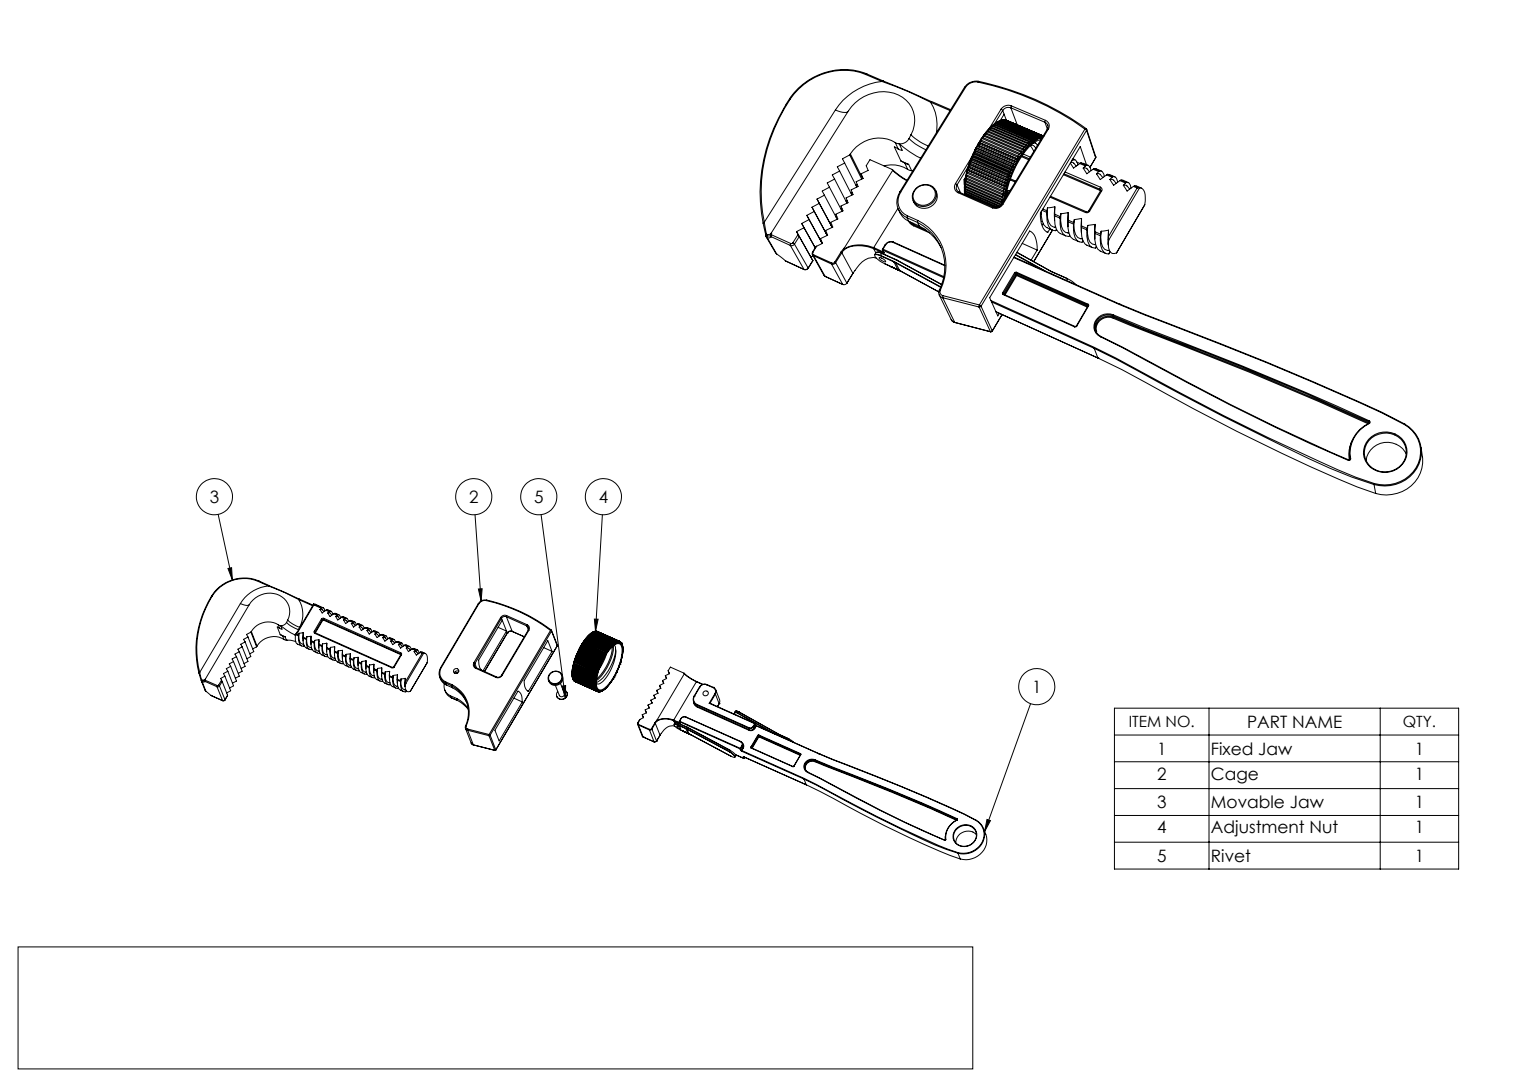
ISO-10303-21;
HEADER;
FILE_DESCRIPTION (('STEP AP214'),
    '1' );
FILE_NAME ('MAS-685',
    '2026-10-07T05:30:18',
    ( '' ),
    ( '' ),
    'SwSTEP 2.0',
    'SolidWorks 2021',
    '' );
FILE_SCHEMA (( 'AUTOMOTIVE_DESIGN' ));
ENDSEC;

DATA;
#1 = CARTESIAN_POINT ( 'NONE',  ( 7.084665262690076126, 22.02201867748817321, -10.88017736071110164 ) ) ;
#2 = CARTESIAN_POINT ( 'NONE',  ( 14.03351048042397231, -0.03417435944610275333, -2.474486531753715024 ) ) ;
#3 = CARTESIAN_POINT ( 'NONE',  ( 10.00000000000000000, 59.75893115100078745, -9.846743663894594434 ) ) ;
#4 = CARTESIAN_POINT ( 'NONE',  ( 14.71525861348289865, 0.5000000000000004441, -2.908807992686582633 ) ) ;
#5 = CARTESIAN_POINT ( 'NONE',  ( 14.92337183194729988, 29.34226448433411960, -8.527530157486177487 ) ) ;
#6 = CARTESIAN_POINT ( 'NONE',  ( -1.099225684535947600, 54.54030133659708923, 6.408140936763237150 ) ) ;
#7 = B_SPLINE_CURVE_WITH_KNOTS ( 'NONE', 3,
 ( #85792, #56757, #94261, #25787, #71286, #3780 ),
 .UNSPECIFIED., .F., .F.,
 ( 4, 2, 4 ),
 ( 0.0002800003243993068715, 0.0006862055569927260918, 0.001092410789586145421 ),
 .UNSPECIFIED. ) ;
#8 = CARTESIAN_POINT ( 'NONE',  ( 7.082119434687054849, -1.529584498419354954, 12.26659068614894288 ) ) ;
#9 = CARTESIAN_POINT ( 'NONE',  ( 4.559911319644449179, 47.23035201082150536, -9.422509992056141925 ) ) ;
#10 = CARTESIAN_POINT ( 'NONE',  ( 10.00000000000000000, 49.75893115100078745, -9.846743663894594434 ) ) ;
#11 = CARTESIAN_POINT ( 'NONE',  ( 6.204703633549690345, 40.76208216824731778, -14.16423886937410259 ) ) ;
#12 = ORIENTED_EDGE ( 'NONE', *, *, #89075, .F. ) ;
#13 = CARTESIAN_POINT ( 'NONE',  ( 17.08211943468705840, 5.137082168247300906, -12.26659068614894466 ) ) ;
#14 = CARTESIAN_POINT ( 'NONE',  ( 0.5774900079438590739, 67.64701867748817676, -5.440088680355550821 ) ) ;
#15 = CARTESIAN_POINT ( 'NONE',  ( 1.915564264621432589, 3.914659629196372862E-16, -14.37291249357990530 ) ) ;
#16 = CARTESIAN_POINT ( 'NONE',  ( 24.16423886937410614, 59.51208216824728936, -3.795296366450302550 ) ) ;
#17 = CARTESIAN_POINT ( 'NONE',  ( 13.43411237798106583, 7.665301336597086568, -12.81628187352647252 ) ) ;
#18 = CARTESIAN_POINT ( 'NONE',  ( 18.95386800104995473, 43.23810908735726599, -6.499999999999990230 ) ) ;
#19 = CARTESIAN_POINT ( 'NONE',  ( 0.5774900079438607392, 58.48035201082151247, 5.440088680355550821 ) ) ;
#20 = DIRECTION ( 'NONE',  ( -0.000000000000000000, 1.000000000000000000, -0.000000000000000000 ) ) ;
#21 = CARTESIAN_POINT ( 'NONE',  ( -46.94000000000001194, 100.5254250115999923, -8.865097534344174690 ) ) ;
#22 = CARTESIAN_POINT ( 'NONE',  ( 0.6178305044545818747, 33.49863466993042493, -9.382169495545419124 ) ) ;
#23 = CARTESIAN_POINT ( 'NONE',  ( -2.266590686148945544, 67.22041550158063217, 7.082119434687048631 ) ) ;
#24 = CARTESIAN_POINT ( 'NONE',  ( -10.88017736071110342, 33.06368534415485527, 3.903127820947815962E-15 ) ) ;
#25 = CARTESIAN_POINT ( 'NONE',  ( 20.88017736071110875, 15.77201867748817143, -2.915334737309920765 ) ) ;
#26 = CARTESIAN_POINT ( 'NONE',  ( 19.42250999205614193, 30.14701867748817321, 5.440088680355555262 ) ) ;
#27 = CARTESIAN_POINT ( 'NONE',  ( 7.361572987183169658, 49.96726448433410894, -9.846743663894592657 ) ) ;
#28 = CARTESIAN_POINT ( 'NONE',  ( 19.84674366389459266, 58.71726448433411605, -2.638427012816827677 ) ) ;
#29 = CARTESIAN_POINT ( 'NONE',  ( -2.816281873526473856, 49.12363466993042493, 9.499525473075851096E-16 ) ) ;
#31 = ORIENTED_EDGE ( 'NONE', *, *, #54443, .T. ) ;
#30 = AXIS2_PLACEMENT_3D ( 'NONE', #64343, #43811, #52312 ) ;
#32 = EDGE_CURVE ( 'NONE', #89546, #61124, #1756, .T. ) ;
#33 = VECTOR ( 'NONE', #15415, 1000.000000000000114 ) ;
#34 = CARTESIAN_POINT ( 'NONE',  ( 20.88017736071110875, 20.77201867748816611, -2.915334737309920765 ) ) ;
#35 = CARTESIAN_POINT ( 'NONE',  ( 6.565887622018943937, 23.08196800326375708, -12.81628187352647608 ) ) ;
#36 = CARTESIAN_POINT ( 'NONE',  ( 0.000000000000000000, 0.000000000000000000, 0.000000000000000000 ) ) ;
#37 = CARTESIAN_POINT ( 'NONE',  ( 10.00000000000000000, 54.75893115100078745, -9.846743663894594434 ) ) ;
#38 = CARTESIAN_POINT ( 'NONE',  ( 12.91533473730992121, 29.52201867748817321, 10.88017736071110164 ) ) ;
#39 = CARTESIAN_POINT ( 'NONE',  ( 3.591859063236763294, 18.29030133659708568, -11.09922568453595026 ) ) ;
#41 = DIRECTION ( 'NONE',  ( 1.000000000000000000, -5.818595309480553908E-17, 0.000000000000000000 ) ) ;
#40 = CARTESIAN_POINT ( 'NONE',  ( -0.8801773607111008646, 43.27201867748817676, 2.915334737309923430 ) ) ;
#42 = DIRECTION ( 'NONE',  ( -1.000000000000000000, 0.000000000000000000, 0.000000000000000000 ) ) ;
#43 = CARTESIAN_POINT ( 'NONE',  ( 21.09922568453594849, 56.20696800326375353, 6.408140936763242479 ) ) ;
#44 = ORIENTED_EDGE ( 'NONE', *, *, #85385, .F. ) ;
#45 = CARTESIAN_POINT ( 'NONE',  ( 12.63842701281683034, 62.46726448433410894, 9.846743663894596210 ) ) ;
#46 = CARTESIAN_POINT ( 'NONE',  ( -0.8801773607110991993, 42.85535201082150536, -2.915334737309923874 ) ) ;
#48 = CARTESIAN_POINT ( 'NONE',  ( -4.164238869374099039, 6.803748834913967869, 8.674139862899312516E-16 ) ) ;
#47 = CARTESIAN_POINT ( 'NONE',  ( 13.43411237798106583, 32.66530133659708213, -12.81628187352647252 ) ) ;
#49 = CARTESIAN_POINT ( 'NONE',  ( 10.00000000000000000, 9.758931151000785675, -9.846743663894594434 ) ) ;
#50 = CARTESIAN_POINT ( 'NONE',  ( 2.035157376598824452, 58.68868534415482685, 7.964842623401179544 ) ) ;
#51 = CARTESIAN_POINT ( 'NONE',  ( -4.164238869374099039, 46.80374883491397497, 8.674139862899312516E-16 ) ) ;
#52 = LINE ( 'NONE', #39009, #8257 ) ;
#53 = CARTESIAN_POINT ( 'NONE',  ( 0.1532563361054083140, 11.00893115100078568, 1.131784320476157264E-15 ) ) ;
#54 = CARTESIAN_POINT ( 'NONE',  ( 0.1532563361054082862, 6.217264484334118713, 2.638427012816831674 ) ) ;
#55 = CARTESIAN_POINT ( 'NONE',  ( 5.361923921558577000, 0.000000000000000000, -0.9937738586171993571 ) ) ;
#56 = CARTESIAN_POINT ( 'NONE',  ( 2.917880565312950480, 45.97041550158063927, -12.26659068614894821 ) ) ;
#57 = CARTESIAN_POINT ( 'NONE',  ( -14.09394518620607606, 3.895088541583166744E-16, -3.407449058785548157 ) ) ;
#58 = CARTESIAN_POINT ( 'NONE',  ( 0.5774900079438590739, 12.64701867748817143, -5.440088680355550821 ) ) ;
#59 = CARTESIAN_POINT ( 'NONE',  ( -14.35840480524194440, 15.00000000000000000, -4.340070442839038201 ) ) ;
#60 = ORIENTED_EDGE ( 'NONE', *, *, #26638, .T. ) ;
#61 = ORIENTED_EDGE ( 'NONE', *, *, #8376, .F. ) ;
#62 = CARTESIAN_POINT ( 'NONE',  ( 15.44008868035555793, 11.39701867748817143, -9.422509992056140149 ) ) ;
#64 = EDGE_CURVE ( 'NONE', #6847, #38896, #39743, .T. ) ;
#63 = CARTESIAN_POINT ( 'NONE',  ( 22.26659068614895176, 59.72041550158063927, -7.082119434687042414 ) ) ;
#65 = CARTESIAN_POINT ( 'NONE',  ( 17.20831665107776587, 42.88393115100077324, 7.208316651077764980 ) ) ;
#66 = CARTESIAN_POINT ( 'NONE',  ( -2.816281873526473856, 34.33196800326376064, 3.434112377981055619 ) ) ;
#67 = LINE ( 'NONE', #92990, #97116 ) ;
#69 = CARTESIAN_POINT ( 'NONE',  ( -2.266590686148945544, 11.38708216824730179, -7.082119434687050408 ) ) ;
#68 = FACE_OUTER_BOUND ( 'NONE', #36092, .T. ) ;
#70 = CARTESIAN_POINT ( 'NONE',  ( 12.91533473730992121, 29.52201867748817321, 10.88017736071110164 ) ) ;
#71 = CARTESIAN_POINT ( 'NONE',  ( -0.8801773607111009756, 8.063685344154837509, 1.068504757029289695E-15 ) ) ;
#72 = CARTESIAN_POINT ( 'NONE',  ( 19.84674366389459266, 48.71726448433413026, -2.638427012816827677 ) ) ;
#73 = ADVANCED_FACE ( 'NONE', ( #77721, #92241 ), #62222, .F. ) ;
#74 = SURFACE_SIDE_STYLE ('',( #68542 ) ) ;
#75 = CARTESIAN_POINT ( 'NONE',  ( 17.20831665107776587, 17.88393115100078745, 7.208316651077764980 ) ) ;
#76 = CARTESIAN_POINT ( 'NONE',  ( 1.274849032794231007, 33.57228050351031357, 6.499999999999895195 ) ) ;
#77 = CARTESIAN_POINT ( 'NONE',  ( 8.527530157486175710, 13.92559781766745886, -4.923371831947298993 ) ) ;
#78 = EDGE_LOOP ( 'NONE', ( #8782, #50817, #67592, #16515 ) ) ;
#79 = CARTESIAN_POINT ( 'NONE',  ( -6.715867195167276371, 15.00000000000000000, -12.85095824508335838 ) ) ;
#80 = ORIENTED_EDGE ( 'NONE', *, *, #34109, .F. ) ;
#81 = CARTESIAN_POINT ( 'NONE',  ( 12.63842701281683922, 59.55059781766744464, -9.846743663894590881 ) ) ;
#83 = CARTESIAN_POINT ( 'NONE',  ( 2.035157376598824452, 33.68868534415484106, 7.964842623401179544 ) ) ;
#82 = CARTESIAN_POINT ( 'NONE',  ( 20.88017736071110519, 30.56368534415484106, 2.639326808657452039E-16 ) ) ;
#85 = CARTESIAN_POINT ( 'NONE',  ( 16.40814093676323893, 25.79030133659708923, 11.09922568453595026 ) ) ;
#84 = CARTESIAN_POINT ( 'NONE',  ( 2.791683348922240793, 56.63393115100078035, 7.208316651077764092 ) ) ;
#86 = CARTESIAN_POINT ( 'NONE',  ( -2.266590686148945544, 21.38708216824730357, -7.082119434687050408 ) ) ;
#87 = CARTESIAN_POINT ( 'NONE',  ( -6.000000000000014211, 80.32179676972448590, -4.250000000000000000 ) ) ;
#88 =( GEOMETRIC_REPRESENTATION_CONTEXT ( 3 ) GLOBAL_UNCERTAINTY_ASSIGNED_CONTEXT ( ( #83266 ) ) GLOBAL_UNIT_ASSIGNED_CONTEXT ( ( #85236, #77227, #46251 ) ) REPRESENTATION_CONTEXT ( 'NONE', 'WORKASPACE' ) );
#89 = CARTESIAN_POINT ( 'NONE',  ( 19.38216949554541202, 40.99863466993042493, 9.382169495545424454 ) ) ;
#90 = EDGE_LOOP ( 'NONE', ( #14273, #19404, #8393, #55652 ) ) ;
#91 = CARTESIAN_POINT ( 'NONE',  ( 0.1532563361054083140, 51.00893115100078745, 1.131784320476157264E-15 ) ) ;
#92 = CARTESIAN_POINT ( 'NONE',  ( -0.8801773607110991993, 2.855352010821504471, -2.915334737309923874 ) ) ;
#93 = ORIENTED_EDGE ( 'NONE', *, *, #11884, .T. ) ;
#94 = CARTESIAN_POINT ( 'NONE',  ( 17.96484262340118221, 11.18868534415484106, -7.964842623401177768 ) ) ;
#95 = ORIENTED_EDGE ( 'NONE', *, *, #4795, .T. ) ;
#96 = CARTESIAN_POINT ( 'NONE',  ( 20.88017736071110164, 60.35535201082151957, 2.915334737309930979 ) ) ;
#97 = CARTESIAN_POINT ( 'NONE',  ( 15.44008868035555793, 61.39701867748817676, -9.422509992056140149 ) ) ;
#98 = CARTESIAN_POINT ( 'NONE',  ( 10.00000000000000178, 59.31368534415484106, 10.88017736071110342 ) ) ;
#99 = DIRECTION ( 'NONE',  ( -0.000000000000000000, -0.000000000000000000, -1.000000000000000000 ) ) ;
#100 = CARTESIAN_POINT ( 'NONE',  ( 0.5774900079438590739, 52.64701867748817676, -5.440088680355550821 ) ) ;
#101 = CIRCLE ( 'NONE', #95854, 15.00000000000000000 ) ;
#102 = DIRECTION ( 'NONE',  ( 0.000000000000000000, 0.000000000000000000, 1.000000000000000000 ) ) ;
#103 = CARTESIAN_POINT ( 'NONE',  ( -46.78604402846880106, 100.7423487049318140, 9.213902555517821114 ) ) ;
#105 = VERTEX_POINT ( 'NONE', #92727 ) ;
#104 = CARTESIAN_POINT ( 'NONE',  ( 11.15633734009358058, -69.21829398631774666, 4.000000000000000888 ) ) ;
#106 = CARTESIAN_POINT ( 'NONE',  ( 7.361572987183170547, 42.05059781766745886, 9.846743663894590881 ) ) ;
#107 = VERTEX_POINT ( 'NONE', #70238 ) ;
#108 = CARTESIAN_POINT ( 'NONE',  ( 1.472469842513823179, 65.59226448433412315, -4.923371831947296329 ) ) ;
#109 = FILL_AREA_STYLE_COLOUR ( '', #46180 ) ;
#110 = CARTESIAN_POINT ( 'NONE',  ( -4.164238869374098151, 16.59541550158063927, -3.795296366450310543 ) ) ;
#111 = DIRECTION ( 'NONE',  ( 1.000000000000000000, -0.000000000000000000, -0.000000000000000000 ) ) ;
#113 = CARTESIAN_POINT ( 'NONE',  ( 10.00000000000000178, 64.31368534415483396, 10.88017736071110342 ) ) ;
#112 = DIRECTION ( 'NONE',  ( 0.000000000000000000, 1.000000000000000000, 0.000000000000000000 ) ) ;
#114 = CARTESIAN_POINT ( 'NONE',  ( 7.084665262690076126, 12.02201867748817321, -10.88017736071110164 ) ) ;
#115 = CARTESIAN_POINT ( 'NONE',  ( 0.6081133539230425544, 48.33703382326399378, 6.499999999999948486 ) ) ;
#116 = CARTESIAN_POINT ( 'NONE',  ( 6.565887622018943937, 45.16530133659708923, 12.81628187352647430 ) ) ;
#117 = CARTESIAN_POINT ( 'NONE',  ( -10.32896413005679648, 5.104976035794177136, 5.963430220938290560 ) ) ;
#118 = CARTESIAN_POINT ( 'NONE',  ( 5.076628168052703671, 46.84226448433412315, 8.527530157486179263 ) ) ;
#119 = CARTESIAN_POINT ( 'NONE',  ( 12.63842701281683034, 2.467264484334118269, 9.846743663894596210 ) ) ;
#120 = CARTESIAN_POINT ( 'NONE',  ( 16.40814093676324603, 17.45696800326375353, -11.09922568453594671 ) ) ;
#121 = CARTESIAN_POINT ( 'NONE',  ( 14.92337183194729988, 19.34226448433411960, -8.527530157486177487 ) ) ;
#122 = CARTESIAN_POINT ( 'NONE',  ( 0.6178305044545818747, 13.49863466993041783, -9.382169495545419124 ) ) ;
#123 = FILL_AREA_STYLE ('',( #74603 ) ) ;
#124 = STYLED_ITEM ( 'NONE', ( #39195 ), #78361 ) ;
#125 = CARTESIAN_POINT ( 'NONE',  ( 12.63842701281683034, 12.46726448433411782, 9.846743663894596210 ) ) ;
#126 = EDGE_LOOP ( 'NONE', ( #78693, #55595, #4509, #60539 ) ) ;
#127 = ORIENTED_EDGE ( 'NONE', *, *, #93931, .T. ) ;
#128 = CARTESIAN_POINT ( 'NONE',  ( -0.8801773607110991993, 22.85535201082150181, -2.915334737309923874 ) ) ;
#129 = CARTESIAN_POINT ( 'NONE',  ( 24.16423886937410614, 19.30374883491397142, 8.672049930838204340E-16 ) ) ;
#130 = CARTESIAN_POINT ( 'NONE',  ( 0.1532563361054082862, 46.21726448433411605, 2.638427012816831674 ) ) ;
#131 = CARTESIAN_POINT ( 'NONE',  ( 1.472469842513823179, 5.592264484334118713, -4.923371831947296329 ) ) ;
#133 = CARTESIAN_POINT ( 'NONE',  ( -5.812563760649267941, -35.09659463721938977, -3.750000000000000000 ) ) ;
#132 = CARTESIAN_POINT ( 'NONE',  ( -2.816281873526473856, 44.33196800326375353, 3.434112377981055619 ) ) ;
#134 = CARTESIAN_POINT ( 'NONE',  ( -0.8801773607111008646, 18.27201867748817321, 2.915334737309923430 ) ) ;
#135 = DIRECTION ( 'NONE',  ( 0.000000000000000000, 0.000000000000000000, -1.000000000000000000 ) ) ;
#136 = CARTESIAN_POINT ( 'NONE',  ( 6.565887622018943937, 13.08196800326374998, -12.81628187352647608 ) ) ;
#137 = CARTESIAN_POINT ( 'NONE',  ( 3.591859063236761518, 4.956968003263753531, 11.09922568453594849 ) ) ;
#138 = CARTESIAN_POINT ( 'NONE',  ( 19.84674366389459266, 33.30059781766744464, 2.638427012816836559 ) ) ;
#139 = CARTESIAN_POINT ( 'NONE',  ( -10.88017736071110342, -6.936314655845155386, 3.903127820947815962E-15 ) ) ;
#140 = CARTESIAN_POINT ( 'NONE',  ( 19.38216949554541202, 30.99863466993042138, 9.382169495545424454 ) ) ;
#141 = CARTESIAN_POINT ( 'NONE',  ( 13.59972906620400401, 0.04962881387626714991, -5.718800721548577215 ) ) ;
#143 = CARTESIAN_POINT ( 'NONE',  ( 11.29222593019770393, 14.76930270348882068, 9.783848334571327854 ) ) ;
#142 = CARTESIAN_POINT ( 'NONE',  ( 2.035157376598822676, 42.43868534415483396, -7.964842623401177768 ) ) ;
#144 = ADVANCED_FACE ( 'NONE', ( #16249 ), #24174, .T. ) ;
#145 = CARTESIAN_POINT ( 'NONE',  ( 1.460619146402132233E-15, 35.00000000000000000, 11.92686044187656513 ) ) ;
#146 = CARTESIAN_POINT ( 'NONE',  ( 2.035157376598824452, 68.68868534415484817, 7.964842623401179544 ) ) ;
#147 = CARTESIAN_POINT ( 'NONE',  ( 2.035157376598822676, 42.43868534415483396, -7.964842623401177768 ) ) ;
#148 = CIRCLE ( 'NONE', #91104, 1.249999999999987121 ) ;
#149 = CARTESIAN_POINT ( 'NONE',  ( 2.035157376598824452, 48.68868534415483396, 7.964842623401179544 ) ) ;
#150 = CARTESIAN_POINT ( 'NONE',  ( 5.076628168052703671, 61.84226448433412315, 8.527530157486179263 ) ) ;
#151 = CARTESIAN_POINT ( 'NONE',  ( 19.42250999205614548, 65.98035201082151957, -5.440088680355545492 ) ) ;
#152 = CARTESIAN_POINT ( 'NONE',  ( 1.472469842513823179, 50.59226448433411605, -4.923371831947296329 ) ) ;
#153 = CARTESIAN_POINT ( 'NONE',  ( 15.44008868035555793, 6.397018677488170546, -9.422509992056140149 ) ) ;
#154 = AXIS2_PLACEMENT_3D ( 'NONE', #61355, #15392, #78324 ) ;
#155 = CARTESIAN_POINT ( 'NONE',  ( 3.591859063236763294, 8.290301336597087456, -11.09922568453595026 ) ) ;
#156 = VERTEX_POINT ( 'NONE', #67375 ) ;
#157 = CARTESIAN_POINT ( 'NONE',  ( -0.8801773607111009756, 38.06368534415484106, 1.068504757029289695E-15 ) ) ;
#159 = CARTESIAN_POINT ( 'NONE',  ( 0.9413316022086131163, 23.45508385108959004, 6.499999999999978684 ) ) ;
#158 = CARTESIAN_POINT ( 'NONE',  ( 19.84674366389459266, 63.71726448433412315, -2.638427012816827677 ) ) ;
#160 = CARTESIAN_POINT ( 'NONE',  ( 20.88017736071110164, 20.35535201082150891, 2.915334737309930979 ) ) ;
#161 = CARTESIAN_POINT ( 'NONE',  ( 4.559911319644449179, 23.89701867748817321, 9.422509992056141925 ) ) ;
#162 = CARTESIAN_POINT ( 'NONE',  ( 20.36894250292379738, 39.92874883491396787, -10.36894250292379027 ) ) ;
#163 = CARTESIAN_POINT ( 'NONE',  ( 18.52753015748618282, 23.92559781766745530, -4.923371831947291888 ) ) ;
#164 = CARTESIAN_POINT ( 'NONE',  ( 0.5774900079438590739, 42.64701867748816966, -5.440088680355550821 ) ) ;
#165 = CARTESIAN_POINT ( 'NONE',  ( 24.16423886937410614, 4.512082168247300906, -3.795296366450302550 ) ) ;
#166 = DIRECTION ( 'NONE',  ( 0.000000000000000000, 1.000000000000000000, 0.000000000000000000 ) ) ;
#167 = CARTESIAN_POINT ( 'NONE',  ( 7.361572987183170547, 57.05059781766744464, 9.846743663894590881 ) ) ;
#168 = EDGE_LOOP ( 'NONE', ( #11039, #37677, #32498, #88509 ) ) ;
#169 = ORIENTED_EDGE ( 'NONE', *, *, #60294, .T. ) ;
#170 = CARTESIAN_POINT ( 'NONE',  ( -2.266590686148945544, 32.22041550158063927, 7.082119434687048631 ) ) ;
#172 = ADVANCED_FACE ( 'NONE', ( #58883 ), #90560, .T. ) ;
#171 = CARTESIAN_POINT ( 'NONE',  ( 13.79529636645030344, 23.26208216824730002, 14.16423886937410614 ) ) ;
#173 = CARTESIAN_POINT ( 'NONE',  ( 0.1532563361054100626, 0.8005978176674514168, -2.638427012816831230 ) ) ;
#174 = CARTESIAN_POINT ( 'NONE',  ( 17.20831665107776587, 47.88393115100078745, 7.208316651077764980 ) ) ;
#175 = CARTESIAN_POINT ( 'NONE',  ( -11.62817260212919024, -77.84151128241038009, 3.750000000000000000 ) ) ;
#177 = CARTESIAN_POINT ( 'NONE',  ( 16.40814093676324603, 22.45696800326375353, -11.09922568453594671 ) ) ;
#176 = CARTESIAN_POINT ( 'NONE',  ( 4.559911319644449179, 52.23035201082151247, -9.422509992056141925 ) ) ;
#178 = CARTESIAN_POINT ( 'NONE',  ( 6.204703633549690345, 30.76208216824730357, -14.16423886937410259 ) ) ;
#179 = CARTESIAN_POINT ( 'NONE',  ( 0.5774900079438590739, 7.647018677488171434, -5.440088680355550821 ) ) ;
#180 = CARTESIAN_POINT ( 'NONE',  ( 20.88017736071110519, 25.56368534415483751, 2.639326808657452039E-16 ) ) ;
#181 = LINE ( 'NONE', #61621, #10834 ) ;
#182 = CARTESIAN_POINT ( 'NONE',  ( -0.8801773607110991993, 62.85535201082150536, -2.915334737309923874 ) ) ;
#183 = CARTESIAN_POINT ( 'NONE',  ( -1.099225684535947600, 44.54030133659708923, 6.408140936763237150 ) ) ;
#184 = CARTESIAN_POINT ( 'NONE',  ( -8.527530157486182816, -29.40773551566588040, -4.923371831947288335 ) ) ;
#185 = ORIENTED_EDGE ( 'NONE', *, *, #34928, .T. ) ;
#186 = CARTESIAN_POINT ( 'NONE',  ( 0.2074183518478781019, 14.95123636042159454, -14.75075219811622773 ) ) ;
#187 = CARTESIAN_POINT ( 'NONE',  ( 0.7375392941517235901, 0.5000000000000004441, 14.98185688723471110 ) ) ;
#188 = DIRECTION ( 'NONE',  ( 0.000000000000000000, 0.000000000000000000, -1.000000000000000000 ) ) ;
#189 = VERTEX_POINT ( 'NONE', #73386 ) ;
#190 = CARTESIAN_POINT ( 'NONE',  ( -0.8653096853335169314, -2.832054659144752395E-15, 14.59999144042650521 ) ) ;
#192 = CARTESIAN_POINT ( 'NONE',  ( 17.08211943468705840, 60.13708216824729647, -12.26659068614894466 ) ) ;
#191 = CARTESIAN_POINT ( 'NONE',  ( -0.3689425029237881626, 62.42874883491396787, 10.36894250292379027 ) ) ;
#194 = CARTESIAN_POINT ( 'NONE',  ( 2.791683348922237240, 60.38393115100078745, -7.208316651077763204 ) ) ;
#193 = CARTESIAN_POINT ( 'NONE',  ( 19.84674366389459621, 18.50893115100078745, 7.409399052514197653E-17 ) ) ;
#195 = DIRECTION ( 'NONE',  ( -1.483861936729427615E-16, 1.000000000000000000, -0.000000000000000000 ) ) ;
#196 = DIRECTION ( 'NONE',  ( 0.000000000000000000, 0.000000000000000000, 1.000000000000000000 ) ) ;
#197 = CARTESIAN_POINT ( 'NONE',  ( 21.09922568453595559, 2.040301336597086568, -6.408140936763230044 ) ) ;
#198 = CARTESIAN_POINT ( 'NONE',  ( 12.81628187352647608, 21.41530133659708923, 3.434112377981052511 ) ) ;
#199 = ORIENTED_EDGE ( 'NONE', *, *, #97123, .F. ) ;
#200 = CARTESIAN_POINT ( 'NONE',  ( 24.16423886937409904, 34.09541550158064638, 3.795296366450317205 ) ) ;
#201 = ORIENTED_EDGE ( 'NONE', *, *, #76299, .T. ) ;
#202 = CARTESIAN_POINT ( 'NONE',  ( 22.26659068614895176, 49.72041550158063927, -7.082119434687042414 ) ) ;
#203 = ORIENTED_EDGE ( 'NONE', *, *, #30154, .T. ) ;
#204 = CARTESIAN_POINT ( 'NONE',  ( 13.43411237798106583, 52.66530133659708213, -12.81628187352647252 ) ) ;
#205 = EDGE_CURVE ( 'NONE', #59600, #64703, #44234, .T. ) ;
#206 = CARTESIAN_POINT ( 'NONE',  ( -0.8801773607111008646, 28.27201867748817321, 2.915334737309923430 ) ) ;
#207 = CARTESIAN_POINT ( 'NONE',  ( 1.472469842513823179, 50.59226448433411605, -4.923371831947296329 ) ) ;
#208 = CARTESIAN_POINT ( 'NONE',  ( 19.42250999205614548, 25.98035201082150891, -5.440088680355545492 ) ) ;
#209 = CARTESIAN_POINT ( 'NONE',  ( 22.81628187352647785, 61.41530133659709634, 3.434112377981063169 ) ) ;
#210 = CARTESIAN_POINT ( 'NONE',  ( -6.874984555098656358, -78.81798443069058635, 2.499999999999998224 ) ) ;
#211 = CARTESIAN_POINT ( 'NONE',  ( 0.1532563361054083140, 51.00893115100078745, 1.131784320476157264E-15 ) ) ;
#212 = CARTESIAN_POINT ( 'NONE',  ( 7.361572987183169658, 54.96726448433413026, -9.846743663894592657 ) ) ;
#213 = EDGE_CURVE ( 'NONE', #70990, #82368, #80902, .T. ) ;
#216 = ORIENTED_EDGE ( 'NONE', *, *, #69949, .F. ) ;
#215 = VECTOR ( 'NONE', #1501, 1000.000000000000000 ) ;
#214 = CARTESIAN_POINT ( 'NONE',  ( -46.30928139467842897, 104.0823827281712255, -5.529860068218142466 ) ) ;
#217 = CARTESIAN_POINT ( 'NONE',  ( 0.7375392941518293943, 15.00000000000000000, -14.98185688723470932 ) ) ;
#218 = CARTESIAN_POINT ( 'NONE',  ( 18.52753015748617571, 3.092264484334118269, 4.923371831947298993 ) ) ;
#219 = CARTESIAN_POINT ( 'NONE',  ( -9.010802615327746068, 0.2301505768537817076, -11.91753657575794811 ) ) ;
#220 = ORIENTED_EDGE ( 'NONE', *, *, #48530, .T. ) ;
#221 = CARTESIAN_POINT ( 'NONE',  ( 0.9408516040111366552, 57.46693863883976405, -6.499999999999915623 ) ) ;
#222 = CARTESIAN_POINT ( 'NONE',  ( 12.63842701281683034, 37.46726448433411605, 9.846743663894596210 ) ) ;
#223 = DIRECTION ( 'NONE',  ( -1.000000000000000000, 0.000000000000000000, 0.000000000000000000 ) ) ;
#224 = CARTESIAN_POINT ( 'NONE',  ( 16.40814093676324603, 32.45696800326375353, -11.09922568453594671 ) ) ;
#225 = STYLED_ITEM ( 'NONE', ( #36779 ), #46100 ) ;
#226 = CARTESIAN_POINT ( 'NONE',  ( 0.000000000000000000, 15.00000000000000000, 0.000000000000000000 ) ) ;
#227 = CARTESIAN_POINT ( 'NONE',  ( -14.15281240980449873, -3.182726299308032341E-15, 3.688687068602606089 ) ) ;
#228 = ORIENTED_EDGE ( 'NONE', *, *, #21710, .F. ) ;
#229 = CARTESIAN_POINT ( 'NONE',  ( 18.52753015748618282, 63.92559781766745886, -4.923371831947291888 ) ) ;
#230 = DIRECTION ( 'NONE',  ( 0.000000000000000000, 1.000000000000000000, 0.000000000000000000 ) ) ;
#231 = CARTESIAN_POINT ( 'NONE',  ( 17.20831665107776587, 57.88393115100078745, 7.208316651077764980 ) ) ;
#232 = CARTESIAN_POINT ( 'NONE',  ( 2.917880565312948704, 37.63708216824731068, 12.26659068614894643 ) ) ;
#233 = CARTESIAN_POINT ( 'NONE',  ( 14.92337183194729633, 62.67559781766745886, 8.527530157486181039 ) ) ;
#234 = LINE ( 'NONE', #46200, #73516 ) ;
#235 = CARTESIAN_POINT ( 'NONE',  ( 14.92337183194729988, 9.342264484334119601, -8.527530157486177487 ) ) ;
#236 = CARTESIAN_POINT ( 'NONE',  ( 20.15039907845753220, 46.74884699246888431, 6.262539305110077947 ) ) ;
#237 = CARTESIAN_POINT ( 'NONE',  ( 10.00000000000000000, 44.75893115100078745, -9.846743663894594434 ) ) ;
#238 = CARTESIAN_POINT ( 'NONE',  ( 15.44008868035555260, 54.73035201082150536, 9.422509992056143702 ) ) ;
#239 = CARTESIAN_POINT ( 'NONE',  ( 10.00000000000000178, 47.25893115100078745, 9.846743663894594434 ) ) ;
#240 = APPLICATION_PROTOCOL_DEFINITION ( 'draft international standard', 'automotive_design', 1998, #25126 ) ;
#241 = DIRECTION ( 'NONE',  ( -0.2164396139381037087, 0.000000000000000000, 0.9762960071199331402 ) ) ;
#242 = CARTESIAN_POINT ( 'NONE',  ( 17.96484262340118221, 49.93868534415484106, 7.964842623401181321 ) ) ;
#243 = VERTEX_POINT ( 'NONE', #19901 ) ;
#244 = CARTESIAN_POINT ( 'NONE',  ( 17.35999999999999943, 37.99999999999997868, -7.000000000000000888 ) ) ;
#245 = CARTESIAN_POINT ( 'NONE',  ( 7.084665262690076126, 27.02201867748817676, -10.88017736071110164 ) ) ;
#247 = CARTESIAN_POINT ( 'NONE',  ( 19.42250999205614193, 60.14701867748817676, 5.440088680355555262 ) ) ;
#246 = CARTESIAN_POINT ( 'NONE',  ( -2.816281873526473856, -0.6680319967362464695, 3.434112377981055619 ) ) ;
#248 = LINE ( 'NONE', #13741, #50377 ) ;
#249 = LINE ( 'NONE', #54676, #20391 ) ;
#250 = SURFACE_STYLE_USAGE ( .BOTH. , #76223 ) ;
#252 = CARTESIAN_POINT ( 'NONE',  ( -35.44000000000001194, 93.50000000000000000, 9.500000000000000000 ) ) ;
#251 = CARTESIAN_POINT ( 'NONE',  ( 19.42250999205614193, 45.14701867748817676, 5.440088680355555262 ) ) ;
#253 = CARTESIAN_POINT ( 'NONE',  ( 19.84674366389459266, 8.300597817667451750, 2.638427012816836559 ) ) ;
#254 = CARTESIAN_POINT ( 'NONE',  ( 14.92337183194729633, 42.67559781766745886, 8.527530157486181039 ) ) ;
#255 = CARTESIAN_POINT ( 'NONE',  ( 14.16423886937410437, 14.09541550158063750, 3.795296366450304770 ) ) ;
#256 = CARTESIAN_POINT ( 'NONE',  ( 19.38216949554541202, 0.9986346699304200492, 9.382169495545424454 ) ) ;
#258 = FACE_OUTER_BOUND ( 'NONE', #51924, .T. ) ;
#257 = CARTESIAN_POINT ( 'NONE',  ( -4.164238869374098151, 61.59541550158063217, -3.795296366450310543 ) ) ;
#260 = AXIS2_PLACEMENT_3D ( 'NONE', #53452, #62422, #47430 ) ;
#259 = CARTESIAN_POINT ( 'NONE',  ( -10.17177286909477552, 0.2301502795151870728, 10.94336654633674399 ) ) ;
#261 = CARTESIAN_POINT ( 'NONE',  ( 24.16423886937410614, 24.30374883491396787, 8.672049930838204340E-16 ) ) ;
#262 = EDGE_CURVE ( 'NONE', #31207, #19224, #78615, .T. ) ;
#263 = CARTESIAN_POINT ( 'NONE',  ( -4.164238869374098151, 56.59541550158063927, -3.795296366450310543 ) ) ;
#264 = B_SPLINE_CURVE_WITH_KNOTS ( 'NONE', 3,
 ( #34760, #66749, #89251, #97273, #64755, #95267 ),
 .UNSPECIFIED., .F., .F.,
 ( 4, 2, 4 ),
 ( 3.409110551496085967E-05, 0.0004400426677367861379, 0.0008459942299586114840 ),
 .UNSPECIFIED. ) ;
#265 =( BOUNDED_CURVE ( )  B_SPLINE_CURVE ( 2, ( #5381, #12855, #20864, #27367, #66849, #65855, #27855, #66344, #19866 ),
 .UNSPECIFIED., .F., .F. ) 
 B_SPLINE_CURVE_WITH_KNOTS ( ( 3, 2, 2, 2, 3 ),
 ( 0.7962860886497512558, 0.7976190476190476719, 0.8035714285714286031, 0.8095238095238095344, 0.8108567684931060615 ),
 .UNSPECIFIED. ) 
 CURVE ( )  GEOMETRIC_REPRESENTATION_ITEM ( )  RATIONAL_B_SPLINE_CURVE ( ( 0.9881565478350734510, 0.9923695281211492025, 1.000000000000000000, 0.9659258262890683122, 1.000000000000000000, 0.9659258262890683122, 1.000000000000000000, 0.9923695281211484254, 0.9881565478350726739 ) ) 
 REPRESENTATION_ITEM ( '' )  );
#266 = CARTESIAN_POINT ( 'NONE',  ( 17.20831665107776587, 14.13393115100078568, -7.208316651077762316 ) ) ;
#267 = CARTESIAN_POINT ( 'NONE',  ( 19.88565890683626947, 32.71691075486303646, -6.480892540919838574 ) ) ;
#268 = AXIS2_PLACEMENT_3D ( 'NONE', #55440, #85944, #96401 ) ;
#269 = ORIENTED_EDGE ( 'NONE', *, *, #30362, .T. ) ;
#270 = CARTESIAN_POINT ( 'NONE',  ( 14.92337183194729633, 22.67559781766745175, 8.527530157486181039 ) ) ;
#271 = CARTESIAN_POINT ( 'NONE',  ( 7.084665262690076126, 24.10535201082150181, 10.88017736071109987 ) ) ;
#272 = CARTESIAN_POINT ( 'NONE',  ( -1.099225684535947600, -1.293031996736246469, -6.408140936763238038 ) ) ;
#274 = DIRECTION ( 'NONE',  ( -1.000000000000000000, -0.000000000000000000, -0.000000000000000000 ) ) ;
#273 = CARTESIAN_POINT ( 'NONE',  ( 6.204703633549690345, 12.84541550158063572, 14.16423886937410082 ) ) ;
#275 = CARTESIAN_POINT ( 'NONE',  ( -11.49658347684029813, 0.04962891477616592634, 9.245857368719700986 ) ) ;
#276 = CARTESIAN_POINT ( 'NONE',  ( 14.92337183194729633, 12.67559781766745353, 8.527530157486181039 ) ) ;
#277 = CARTESIAN_POINT ( 'NONE',  ( 13.43411237798105340, 40.58196800326375353, 12.81628187352647963 ) ) ;
#278 = CARTESIAN_POINT ( 'NONE',  ( 0.1532563361054083140, 46.00893115100079456, 1.131784320476157264E-15 ) ) ;
#279 = EDGE_LOOP ( 'NONE', ( #9235, #51853, #64977, #5678 ) ) ;
#280 = CARTESIAN_POINT ( 'NONE',  ( 1.472469842513823179, 16.42559781766745175, 4.923371831947296329 ) ) ;
#281 = CARTESIAN_POINT ( 'NONE',  ( 11.13643110622481203, -94.02619357113461263, -3.750000000000000000 ) ) ;
#282 = CARTESIAN_POINT ( 'NONE',  ( 5.795997163830076460, -0.03417435944610275333, 13.01802277140709663 ) ) ;
#283 = CARTESIAN_POINT ( 'NONE',  ( 24.16423886937410614, 59.30374883491397497, 8.672049930838204340E-16 ) ) ;
#284 = CARTESIAN_POINT ( 'NONE',  ( 2.035157376598822676, 57.43868534415484106, -7.964842623401177768 ) ) ;
#285 = DIRECTION ( 'NONE',  ( -0.9999619230641714207, 0.000000000000000000, 0.008726535498367550894 ) ) ;
#286 = LINE ( 'NONE', #30732, #94331 ) ;
#287 = CARTESIAN_POINT ( 'NONE',  ( 10.00000000000000000, 34.75893115100078745, -9.846743663894594434 ) ) ;
#288 = CARTESIAN_POINT ( 'NONE',  ( -0.8801773607111008646, 3.272018677488171434, 2.915334737309923430 ) ) ;
#289 = CARTESIAN_POINT ( 'NONE',  ( 10.00000000000000178, 42.25893115100078745, 9.846743663894594434 ) ) ;
#290 = CARTESIAN_POINT ( 'NONE',  ( 5.817157072110707539, 0.3640475087720986824, 13.82608706751091532 ) ) ;
#291 = CARTESIAN_POINT ( 'NONE',  ( 17.20831665107776587, 52.88393115100078035, 7.208316651077764980 ) ) ;
#292 = CARTESIAN_POINT ( 'NONE',  ( 7.084665262690076126, 49.10535201082149825, 10.88017736071109987 ) ) ;
#293 = UNCERTAINTY_MEASURE_WITH_UNIT (LENGTH_MEASURE( 1.000000000000000082E-05 ), #85346, 'distance_accuracy_value', 'NONE');
#294 = AXIS2_PLACEMENT_3D ( 'NONE', #67632, #98653, #53107 ) ;
#295 = VERTEX_POINT ( 'NONE', #12397 ) ;
#296 = ORIENTED_EDGE ( 'NONE', *, *, #42464, .F. ) ;
#297 = CARTESIAN_POINT ( 'NONE',  ( -14.73551000134586353, 0.04962893459885742153, 0.7225335126796733620 ) ) ;
#299 = ADVANCED_FACE ( 'NONE', ( #45868 ), #51618, .T. ) ;
#298 = DIRECTION ( 'NONE',  ( 0.000000000000000000, 0.000000000000000000, -1.000000000000000000 ) ) ;
#300 = CARTESIAN_POINT ( 'NONE',  ( 19.84674366389459621, 8.508931151000785675, 7.409399052514197653E-17 ) ) ;
#301 = CARTESIAN_POINT ( 'NONE',  ( 22.81628187352647785, 56.41530133659708213, 3.434112377981063169 ) ) ;
#303 = CARTESIAN_POINT ( 'NONE',  ( 2.791683348922237240, 55.38393115100078745, -7.208316651077763204 ) ) ;
#302 = CARTESIAN_POINT ( 'NONE',  ( 7.084665262690076126, 2.022018677488171434, -10.88017736071110164 ) ) ;
#304 = CARTESIAN_POINT ( 'NONE',  ( 20.00000000000000711, 81.00839193781131087, 4.500000000000000888 ) ) ;
#305 = CARTESIAN_POINT ( 'NONE',  ( 6.204703633549690345, 30.76208216824730357, -14.16423886937410259 ) ) ;
#306 = CARTESIAN_POINT ( 'NONE',  ( 2.917880565312948704, 52.63708216824730357, 12.26659068614894643 ) ) ;
#307 = CARTESIAN_POINT ( 'NONE',  ( 18.52753015748617571, 58.09226448433411605, 4.923371831947298993 ) ) ;
#308 = VECTOR ( 'NONE', #84981, 1000.000000000000000 ) ;
#309 =( NAMED_UNIT ( * ) SI_UNIT ( $, .STERADIAN. ) SOLID_ANGLE_UNIT ( ) );
#310 = CARTESIAN_POINT ( 'NONE',  ( 17.96484262340118221, 56.18868534415484817, -7.964842623401177768 ) ) ;
#311 = EDGE_CURVE ( 'NONE', #38139, #1776, #53773, .T. ) ;
#312 = CARTESIAN_POINT ( 'NONE',  ( 1.472469842513823179, 0.5922644843341181575, -4.923371831947296329 ) ) ;
#313 = ORIENTED_EDGE ( 'NONE', *, *, #41696, .F. ) ;
#314 = CARTESIAN_POINT ( 'NONE',  ( 13.43411237798106583, 62.66530133659708923, -12.81628187352647252 ) ) ;
#315 = AXIS2_PLACEMENT_3D ( 'NONE', #61065, #112, #24072 ) ;
#316 = ORIENTED_EDGE ( 'NONE', *, *, #50365, .T. ) ;
#317 = CARTESIAN_POINT ( 'NONE',  ( 10.00000000000000178, 7.258931151000785675, 9.846743663894594434 ) ) ;
#318 = ORIENTED_EDGE ( 'NONE', *, *, #77420, .F. ) ;
#319 = CARTESIAN_POINT ( 'NONE',  ( 10.00000000000000178, 23.05374883491397142, 14.16423886937410082 ) ) ;
#320 = CARTESIAN_POINT ( 'NONE',  ( 17.20831665107776587, 19.13393115100078035, -7.208316651077762316 ) ) ;
#321 = CARTESIAN_POINT ( 'NONE',  ( 15.44008868035555260, 34.73035201082151247, 9.422509992056143702 ) ) ;
#322 = CARTESIAN_POINT ( 'NONE',  ( 0.5600000000000076028, 107.5383484153110203, -5.000000000000000000 ) ) ;
#323 = ORIENTED_EDGE ( 'NONE', *, *, #6440, .F. ) ;
#324 = CARTESIAN_POINT ( 'NONE',  ( 12.91533473730993009, 21.60535201082150536, -10.88017736071109987 ) ) ;
#325 = VERTEX_POINT ( 'NONE', #97886 ) ;
#326 = CARTESIAN_POINT ( 'NONE',  ( 17.96484262340118221, 34.93868534415482685, 7.964842623401181321 ) ) ;
#327 = PRESENTATION_STYLE_ASSIGNMENT (( #76290 ) ) ;
#328 = ORIENTED_EDGE ( 'NONE', *, *, #58687, .T. ) ;
#329 = DIRECTION ( 'NONE',  ( 0.000000000000000000, 0.000000000000000000, 1.000000000000000000 ) ) ;
#330 = ORIENTED_EDGE ( 'NONE', *, *, #68148, .F. ) ;
#331 = CARTESIAN_POINT ( 'NONE',  ( 16.40814093676324603, 22.45696800326375353, -11.09922568453594671 ) ) ;
#332 = CARTESIAN_POINT ( 'NONE',  ( 2.603489959281199972, 21.58210964143324873, 6.499999999999559464 ) ) ;
#333 = CARTESIAN_POINT ( 'NONE',  ( 0.1532563361054082862, 6.217264484334118713, 2.638427012816831674 ) ) ;
#334 = DIRECTION ( 'NONE',  ( -0.000000000000000000, -1.000000000000000000, -0.000000000000000000 ) ) ;
#335 = CARTESIAN_POINT ( 'NONE',  ( -0.03932841506541424198, 58.12161441960502373, 6.397827110479012092 ) ) ;
#336 = CARTESIAN_POINT ( 'NONE',  ( 2.791683348922240793, 21.63393115100078745, 7.208316651077764092 ) ) ;
#337 = CARTESIAN_POINT ( 'NONE',  ( 7.084665262690076126, 29.10535201082150181, 10.88017736071109987 ) ) ;
#338 = ADVANCED_FACE ( 'NONE', ( #83350 ), #59848, .T. ) ;
#339 = VERTEX_POINT ( 'NONE', #7364 ) ;
#340 = VECTOR ( 'NONE', #77735, 1000.000000000000000 ) ;
#341 = ORIENTED_EDGE ( 'NONE', *, *, #63443, .F. ) ;
#342 = CARTESIAN_POINT ( 'NONE',  ( -0.1503990784575247319, 52.22266099184918176, -6.262539305110083276 ) ) ;
#343 = CARTESIAN_POINT ( 'NONE',  ( 10.00000000000000000, 56.81368534415484106, -10.88017736071110342 ) ) ;
#344 = CARTESIAN_POINT ( 'NONE',  ( 7.684764310694891520, 14.49999999999999112, -12.88194075009941564 ) ) ;
#345 = CARTESIAN_POINT ( 'NONE',  ( 21.09922568453594849, 61.20696800326376064, 6.408140936763242479 ) ) ;
#346 = CARTESIAN_POINT ( 'NONE',  ( 15.44008868035555260, 64.73035201082151957, 9.422509992056143702 ) ) ;
#347 = CARTESIAN_POINT ( 'NONE',  ( 7.361572987183170547, 67.05059781766746596, 9.846743663894590881 ) ) ;
#348 = EDGE_CURVE ( 'NONE', #78868, #92229, #98382, .T. ) ;
#349 = CARTESIAN_POINT ( 'NONE',  ( 5.076628168052704559, 30.17559781766745175, -8.527530157486179263 ) ) ;
#350 = CARTESIAN_POINT ( 'NONE',  ( 3.591859063236761518, 49.95696800326375353, 11.09922568453594849 ) ) ;
#351 = CARTESIAN_POINT ( 'NONE',  ( 6.574926501674518420, -50.89417846498341902, -3.750000000000001332 ) ) ;
#352 = CARTESIAN_POINT ( 'NONE',  ( 19.84674366389459266, 13.30059781766745353, 2.638427012816836559 ) ) ;
#353 = CARTESIAN_POINT ( 'NONE',  ( 0.6178305044545838731, 14.74863466993041783, 9.382169495545420901 ) ) ;
#354 = CYLINDRICAL_SURFACE ( 'NONE', #94314, 1.500000000000001332 ) ;
#355 = CARTESIAN_POINT ( 'NONE',  ( 19.42250999205614548, 30.98035201082150536, -5.440088680355545492 ) ) ;
#356 = CARTESIAN_POINT ( 'NONE',  ( 10.00000000000000000, 64.75893115100078035, -9.846743663894594434 ) ) ;
#357 = CARTESIAN_POINT ( 'NONE',  ( 12.21130863673200473, -3.098870037529856607E-15, 8.049375889233058246 ) ) ;
#358 = CARTESIAN_POINT ( 'NONE',  ( 5.076628168052704559, 20.17559781766745175, -8.527530157486179263 ) ) ;
#359 = CARTESIAN_POINT ( 'NONE',  ( 5.076628168052703671, 1.842264484334118047, 8.527530157486179263 ) ) ;
#360 = CARTESIAN_POINT ( 'NONE',  ( 0.5774900079438607392, 13.48035201082150358, 5.440088680355550821 ) ) ;
#361 = CARTESIAN_POINT ( 'NONE',  ( 0.6178305044545838731, 19.74863466993042138, 9.382169495545420901 ) ) ;
#362 = PRESENTATION_LAYER_ASSIGNMENT (  '', '', ( #43423 ) ) ;
#363 =( NAMED_UNIT ( * ) PLANE_ANGLE_UNIT ( ) SI_UNIT ( $, .RADIAN. ) );
#364 = CARTESIAN_POINT ( 'NONE',  ( -0.7575892234029697470, 0.2306972965111908358, -14.92193396517714099 ) ) ;
#365 = CARTESIAN_POINT ( 'NONE',  ( 4.864310448982641866, -17.52237222630224878, -2.499999999999999112 ) ) ;
#366 = CARTESIAN_POINT ( 'NONE',  ( -2.266590686148945544, 67.22041550158063217, 7.082119434687048631 ) ) ;
#367 = CARTESIAN_POINT ( 'NONE',  ( 7.361572987183169658, 49.96726448433410894, -9.846743663894592657 ) ) ;
#368 = EDGE_CURVE ( 'NONE', #36285, #1044, #68358, .T. ) ;
#369 = CIRCLE ( 'NONE', #57769, 0.2500000000000002220 ) ;
#370 = B_SPLINE_CURVE_WITH_KNOTS ( 'NONE', 3,
 ( #59553, #52060, #6070, #61027, #30031, #36570 ),
 .UNSPECIFIED., .F., .F.,
 ( 4, 2, 4 ),
 ( 0.0002800267093156125989, 0.0006862322000234134670, 0.001092437690731214335 ),
 .UNSPECIFIED. ) ;
#371 = CARTESIAN_POINT ( 'NONE',  ( 2.035157376598824452, 23.68868534415484461, 7.964842623401179544 ) ) ;
#372 = CARTESIAN_POINT ( 'NONE',  ( -0.8801773607111009756, 13.27201867748817321, 2.915334737309923874 ) ) ;
#373 = CIRCLE ( 'NONE', #80196, 14.49999999999999822 ) ;
#374 = CARTESIAN_POINT ( 'NONE',  ( 7.084665262690076126, 29.10535201082150181, 10.88017736071109987 ) ) ;
#376 = DIRECTION ( 'NONE',  ( 8.673617379884028570E-16, 1.000000000000000000, 0.000000000000000000 ) ) ;
#375 = CARTESIAN_POINT ( 'NONE',  ( 17.08211943468705840, 65.13708216824730357, -12.26659068614894466 ) ) ;
#377 =( LENGTH_UNIT ( ) NAMED_UNIT ( * ) SI_UNIT ( .MILLI., .METRE. ) );
#378 = CARTESIAN_POINT ( 'NONE',  ( 10.00000000000000000, 24.75893115100078745, -9.846743663894594434 ) ) ;
#379 = CARTESIAN_POINT ( 'NONE',  ( 0.6178305044545818747, 8.498634669930421381, -9.382169495545419124 ) ) ;
#380 = PLANE ( 'NONE',  #76873 ) ;
#381 = CARTESIAN_POINT ( 'NONE',  ( -2.816281873526473856, -0.8763653300695799508, 9.499525473075851096E-16 ) ) ;
#382 = DIRECTION ( 'NONE',  ( 0.000000000000000000, 0.000000000000000000, 1.000000000000000000 ) ) ;
#383 = ADVANCED_FACE ( 'NONE', ( #38841 ), #20965, .T. ) ;
#384 = CARTESIAN_POINT ( 'NONE',  ( -8.330963135173325540, -7.272696214946840598, -3.750000000000000000 ) ) ;
#385 = CARTESIAN_POINT ( 'NONE',  ( -0.3689425029237898834, 11.17874883491396787, -10.36894250292378850 ) ) ;
#386 = CARTESIAN_POINT ( 'NONE',  ( 5.076628168052703671, 31.84226448433412315, 8.527530157486179263 ) ) ;
#387 = EDGE_LOOP ( 'NONE', ( #36571, #85483, #95211, #2832, #77271 ) ) ;
#388 = CARTESIAN_POINT ( 'NONE',  ( 6.204703633549690345, 57.84541550158063927, 14.16423886937410082 ) ) ;
#389 = EDGE_CURVE ( 'NONE', #33071, #18961, #10309, .T. ) ;
#390 = CARTESIAN_POINT ( 'NONE',  ( 14.92337183194729633, 12.67559781766745353, 8.527530157486181039 ) ) ;
#392 = DIRECTION ( 'NONE',  ( -0.9170600743851266001, 0.000000000000000000, 0.3987490689252404796 ) ) ;
#391 = CARTESIAN_POINT ( 'NONE',  ( 9.050000000000002487, 99.99999999999998579, 8.000000000000000000 ) ) ;
#393 = CARTESIAN_POINT ( 'NONE',  ( 10.00000000000000178, 44.31368534415484106, 10.88017736071110342 ) ) ;
#394 = CARTESIAN_POINT ( 'NONE',  ( 22.81628187352647785, 46.41530133659708213, 3.434112377981063169 ) ) ;
#395 = CARTESIAN_POINT ( 'NONE',  ( 10.00000000000000000, 16.81368534415483751, -10.88017736071110342 ) ) ;
#396 = CARTESIAN_POINT ( 'NONE',  ( 19.38216949554541557, 47.24863466993041783, -9.382169495545420901 ) ) ;
#397 = CARTESIAN_POINT ( 'NONE',  ( 1.472469842513823179, 65.59226448433412315, -4.923371831947296329 ) ) ;
#398 = EDGE_LOOP ( 'NONE', ( #49399, #35064, #25132, #40932 ) ) ;
#399 = DIRECTION ( 'NONE',  ( 0.8870108331782213806, 0.000000000000000000, -0.4617486132350345773 ) ) ;
#400 = CARTESIAN_POINT ( 'NONE',  ( -8.081452932468565109, -7.288464344191233124, -3.999999999999999112 ) ) ;
#401 = CARTESIAN_POINT ( 'NONE',  ( -4.164238869374098151, 36.59541550158063217, -3.795296366450310543 ) ) ;
#402 = CARTESIAN_POINT ( 'NONE',  ( 13.79529636645030344, 13.26208216824729824, 14.16423886937410614 ) ) ;
#403 = CARTESIAN_POINT ( 'NONE',  ( 19.42250999205614193, 15.14701867748817143, 5.440088680355555262 ) ) ;
#404 = CARTESIAN_POINT ( 'NONE',  ( 15.44008868035555260, 34.73035201082151247, 9.422509992056143702 ) ) ;
#405 = LINE ( 'NONE', #8848, #3141 ) ;
#406 = CARTESIAN_POINT ( 'NONE',  ( -18.89999999999999147, 99.74999999999998579, 7.750000000000000000 ) ) ;
#407 = CARTESIAN_POINT ( 'NONE',  ( 19.84674366389459621, 3.508931151000785231, 7.409399052514197653E-17 ) ) ;
#408 = CARTESIAN_POINT ( 'NONE',  ( 0.5774900079438607392, 58.48035201082151247, 5.440088680355550821 ) ) ;
#409 = CARTESIAN_POINT ( 'NONE',  ( -2.816281873526473856, 24.33196800326375353, 3.434112377981055619 ) ) ;
#410 = DIRECTION ( 'NONE',  ( 1.000000000000000000, 0.000000000000000000, 0.000000000000000000 ) ) ;
#411 = DIRECTION ( 'NONE',  ( 0.9537169507482300412, 0.000000000000000000, -0.3007057995042635157 ) ) ;
#412 = CARTESIAN_POINT ( 'NONE',  ( 7.361572987183170547, 37.05059781766744464, 9.846743663894590881 ) ) ;
#413 = CARTESIAN_POINT ( 'NONE',  ( 19.42250999205614193, 20.14701867748817321, 5.440088680355555262 ) ) ;
#414 = AXIS2_PLACEMENT_3D ( 'NONE', #78877, #40404, #49357 ) ;
#416 = EDGE_CURVE ( 'NONE', #77981, #78868, #23450, .T. ) ;
#415 = CARTESIAN_POINT ( 'NONE',  ( 6.565887622018943937, 18.08196800326375708, -12.81628187352647608 ) ) ;
#417 = CARTESIAN_POINT ( 'NONE',  ( 10.00000000000000178, 12.25893115100078568, 9.846743663894594434 ) ) ;
#418 = CARTESIAN_POINT ( 'NONE',  ( 15.44008868035555260, 14.73035201082150536, 9.422509992056143702 ) ) ;
#419 = CARTESIAN_POINT ( 'NONE',  ( 5.076628168052704559, 35.17559781766745175, -8.527530157486179263 ) ) ;
#420 = CARTESIAN_POINT ( 'NONE',  ( -2.816281873526473856, 59.33196800326374643, 3.434112377981055619 ) ) ;
#422 = CARTESIAN_POINT ( 'NONE',  ( 17.08211943468705130, 3.470415501580634388, 12.26659068614894998 ) ) ;
#421 = CARTESIAN_POINT ( 'NONE',  ( 17.20831665107776587, 37.88393115100078745, 7.208316651077764980 ) ) ;
#423 = CARTESIAN_POINT ( 'NONE',  ( 22.26659068614894466, 13.88708216824730179, 7.082119434687054849 ) ) ;
#424 = CARTESIAN_POINT ( 'NONE',  ( 0.5774900079438607392, 33.48035201082150536, 5.440088680355550821 ) ) ;
#426 = CARTESIAN_POINT ( 'NONE',  ( 20.36894250292379382, 43.67874883491397497, 10.36894250292379205 ) ) ;
#425 = CARTESIAN_POINT ( 'NONE',  ( -0.8801773607111008646, 13.27201867748817143, 2.915334737309923430 ) ) ;
#427 = EDGE_CURVE ( 'NONE', #16059, #54251, #3743, .T. ) ;
#428 = CARTESIAN_POINT ( 'NONE',  ( 2.035157376598822676, 37.43868534415484106, -7.964842623401177768 ) ) ;
#429 = CARTESIAN_POINT ( 'NONE',  ( 15.44008868035555260, 14.73035201082150536, 9.422509992056143702 ) ) ;
#430 = ORIENTED_EDGE ( 'NONE', *, *, #84794, .F. ) ;
#431 = CARTESIAN_POINT ( 'NONE',  ( 10.00000000000000000, 36.81368534415484106, -10.88017736071110342 ) ) ;
#432 = CARTESIAN_POINT ( 'NONE',  ( 16.40814093676324603, 57.45696800326375353, -11.09922568453594671 ) ) ;
#433 = CARTESIAN_POINT ( 'NONE',  ( 7.084665262690076126, 44.10535201082151247, 10.88017736071109987 ) ) ;
#434 = CARTESIAN_POINT ( 'NONE',  ( 15.44008868035555260, 44.73035201082151247, 9.422509992056143702 ) ) ;
#435 = CIRCLE ( 'NONE', #56286, 0.5000000000000004441 ) ;
#436 = ORIENTED_EDGE ( 'NONE', *, *, #19518, .T. ) ;
#437 = CARTESIAN_POINT ( 'NONE',  ( 12.91533473730993009, 46.60535201082150536, -10.88017736071109987 ) ) ;
#438 = CARTESIAN_POINT ( 'NONE',  ( 4.096035146093440993, 4.852245006323173772E-16, 13.90943910019262120 ) ) ;
#439 = CARTESIAN_POINT ( 'NONE',  ( 20.36894250292379382, 48.67874883491396076, 10.36894250292379205 ) ) ;
#440 = CARTESIAN_POINT ( 'NONE',  ( 20.88017736071110875, 65.77201867748817676, -2.915334737309920765 ) ) ;
#441 = DIRECTION ( 'NONE',  ( -0.2503800040544453820, 0.000000000000000000, 0.9681476403781066331 ) ) ;
#442 = VECTOR ( 'NONE', #21341, 1000.000000000000000 ) ;
#443 = CARTESIAN_POINT ( 'NONE',  ( 0.000000000000000000, 0.000000000000000000, 0.000000000000000000 ) ) ;
#444 = CARTESIAN_POINT ( 'NONE',  ( 19.84674366389459621, 38.50893115100078745, 7.409399052514197653E-17 ) ) ;
#445 = ORIENTED_EDGE ( 'NONE', *, *, #14494, .F. ) ;
#446 = AXIS2_PLACEMENT_3D ( 'NONE', #98952, #30408, #60911 ) ;
#447 = CARTESIAN_POINT ( 'NONE',  ( 2.791683348922237240, 40.38393115100078035, -7.208316651077763204 ) ) ;
#448 = CARTESIAN_POINT ( 'NONE',  ( 17.96484262340118221, 39.93868534415484106, 7.964842623401181321 ) ) ;
#449 = CARTESIAN_POINT ( 'NONE',  ( 7.361572987183169658, 34.96726448433411605, -9.846743663894592657 ) ) ;
#450 = CARTESIAN_POINT ( 'NONE',  ( 6.565887622018943937, 20.16530133659708213, 12.81628187352647430 ) ) ;
#452 = CARTESIAN_POINT ( 'NONE',  ( 19.42250999205614548, 55.98035201082150536, -5.440088680355545492 ) ) ;
#451 = CARTESIAN_POINT ( 'NONE',  ( -6.000000000000014211, 79.82179676972448590, 6.500000000000000888 ) ) ;
#454 = CARTESIAN_POINT ( 'NONE',  ( 0.5774900079438607392, 3.480352010821504027, 5.440088680355550821 ) ) ;
#453 = CARTESIAN_POINT ( 'NONE',  ( 19.42250999205614193, 40.14701867748817676, 5.440088680355555262 ) ) ;
#455 = CARTESIAN_POINT ( 'NONE',  ( -4.164238869374099927, 52.01208216824729647, 3.795296366450308767 ) ) ;
#456 = EDGE_CURVE ( 'NONE', #94075, #88696, #79322, .T. ) ;
#457 =( GEOMETRIC_REPRESENTATION_CONTEXT ( 3 ) GLOBAL_UNCERTAINTY_ASSIGNED_CONTEXT ( ( #37162 ) ) GLOBAL_UNIT_ASSIGNED_CONTEXT ( ( #27747, #58230, #95771 ) ) REPRESENTATION_CONTEXT ( 'NONE', 'WORKASPACE' ) );
#458 = CARTESIAN_POINT ( 'NONE',  ( 10.00000000000000000, 22.87363466993042138, -12.81628187352647608 ) ) ;
#459 = CARTESIAN_POINT ( 'NONE',  ( 2.603489959281613420, 50.43575266056826933, -6.500000000000031086 ) ) ;
#460 = EDGE_LOOP ( 'NONE', ( #79001, #10921, #93802, #41323 ) ) ;
#461 = CARTESIAN_POINT ( 'NONE',  ( 22.81628187352647785, 21.62363466993041783, 6.195893100308588602E-16 ) ) ;
#462 = CARTESIAN_POINT ( 'NONE',  ( 4.559911319644449179, 22.23035201082150536, -9.422509992056141925 ) ) ;
#463 = CARTESIAN_POINT ( 'NONE',  ( 17.96484262340118221, 59.93868534415484106, 7.964842623401181321 ) ) ;
#464 = ORIENTED_EDGE ( 'NONE', *, *, #87707, .F. ) ;
#465 = ORIENTED_EDGE ( 'NONE', *, *, #55676, .T. ) ;
#466 = CARTESIAN_POINT ( 'NONE',  ( 7.361572987183170547, 2.050597817667451750, 9.846743663894590881 ) ) ;
#467 = CARTESIAN_POINT ( 'NONE',  ( 18.52753015748618282, 48.92559781766745886, -4.923371831947291888 ) ) ;
#468 = CARTESIAN_POINT ( 'NONE',  ( 1.472469842513823179, 40.59226448433411605, -4.923371831947296329 ) ) ;
#469 = CARTESIAN_POINT ( 'NONE',  ( 7.361572987183170547, 32.05059781766745175, 9.846743663894590881 ) ) ;
#470 = CARTESIAN_POINT ( 'NONE',  ( 0.2751277870542967463, 70.00000000000000000, 6.000000000000000000 ) ) ;
#472 = CARTESIAN_POINT ( 'NONE',  ( -2.816281873526473856, 39.12363466993041783, 9.499525473075851096E-16 ) ) ;
#471 = DIRECTION ( 'NONE',  ( 0.9537169507482238240, 0.000000000000000000, 0.3007057995042832221 ) ) ;
#474 = CARTESIAN_POINT ( 'NONE',  ( 19.89103541497710737, 50.66234555792570404, -6.479102184480820981 ) ) ;
#473 = CARTESIAN_POINT ( 'NONE',  ( 19.84674366389459621, 13.50893115100078568, 7.409399052514197653E-17 ) ) ;
#475 = CARTESIAN_POINT ( 'NONE',  ( -0.6999999999999975131, 99.99999999999998579, -8.000000000000000000 ) ) ;
#477 = EDGE_LOOP ( 'NONE', ( #2774, #88083, #69231, #10665 ) ) ;
#476 = CARTESIAN_POINT ( 'NONE',  ( 1.472469842513823179, 40.59226448433411605, -4.923371831947296329 ) ) ;
#478 = PRESENTATION_LAYER_ASSIGNMENT (  '', '', ( #16438 ) ) ;
#479 = CARTESIAN_POINT ( 'NONE',  ( 0.000000000000000000, 70.00000000000000000, 6.000000000000000000 ) ) ;
#480 = CARTESIAN_POINT ( 'NONE',  ( 0.6178305044545838731, 9.748634669930416052, 9.382169495545420901 ) ) ;
#481 = CARTESIAN_POINT ( 'NONE',  ( 4.559911319644449179, 48.89701867748817676, 9.422509992056141925 ) ) ;
#482 = CARTESIAN_POINT ( 'NONE',  ( -2.266590686148945544, 37.22041550158063217, 7.082119434687048631 ) ) ;
#483 = CARTESIAN_POINT ( 'NONE',  ( -10.96178847474192075, 12.64502661508361214, -3.125209426587095329 ) ) ;
#484 = CARTESIAN_POINT ( 'NONE',  ( 20.00000000000000711, 93.00652443313256867, 4.825407043044950051 ) ) ;
#485 = CARTESIAN_POINT ( 'NONE',  ( 24.16423886937409904, 29.09541550158063572, 3.795296366450317205 ) ) ;
#486 = CARTESIAN_POINT ( 'NONE',  ( 17.08211943468705840, 65.13708216824730357, -12.26659068614894466 ) ) ;
#487 = CARTESIAN_POINT ( 'NONE',  ( 24.16423886937410614, 14.30374883491396787, 8.672049930838204340E-16 ) ) ;
#489 = CARTESIAN_POINT ( 'NONE',  ( -9.705452947461466806, 12.49999999999999289, -5.689172442861226031 ) ) ;
#488 = CARTESIAN_POINT ( 'NONE',  ( -4.164238869374098151, 31.59541550158063927, -3.795296366450310543 ) ) ;
#490 = CARTESIAN_POINT ( 'NONE',  ( 7.084665262690076126, 59.10535201082150536, 10.88017736071109987 ) ) ;
#491 = CARTESIAN_POINT ( 'NONE',  ( 1.274849032794231007, 38.57228050351032067, 6.499999999999895195 ) ) ;
#492 = EDGE_CURVE ( 'NONE', #47923, #47609, #86304, .T. ) ;
#494 = CARTESIAN_POINT ( 'NONE',  ( 10.00000000000000000, 39.75893115100078745, -9.846743663894594434 ) ) ;
#493 = CARTESIAN_POINT ( 'NONE',  ( 6.033511671501928575, -36.04540650299031768, 2.750000000000000444 ) ) ;
#495 = CARTESIAN_POINT ( 'NONE',  ( 0.5774900079438607392, 23.48035201082150536, 5.440088680355550821 ) ) ;
#496 = CARTESIAN_POINT ( 'NONE',  ( 20.24186590665278018, 55.59014588040356841, -6.114288769123040090 ) ) ;
#497 = CARTESIAN_POINT ( 'NONE',  ( 1.472469842513823179, 66.42559781766745175, 4.923371831947296329 ) ) ;
#498 = CARTESIAN_POINT ( 'NONE',  ( 20.00000000000000711, 85.79222437201093499, -4.885465336748874066 ) ) ;
#499 = CARTESIAN_POINT ( 'NONE',  ( 7.361572987183169658, 34.96726448433411605, -9.846743663894592657 ) ) ;
#500 = CARTESIAN_POINT ( 'NONE',  ( 22.81628187352647785, 51.62363466993042493, 6.195893100308588602E-16 ) ) ;
#501 = CARTESIAN_POINT ( 'NONE',  ( 7.082119434687054849, -6.529584498419358951, 12.26659068614894288 ) ) ;
#502 = VECTOR ( 'NONE', #65777, 1000.000000000000114 ) ;
#503 = CARTESIAN_POINT ( 'NONE',  ( 0.1532563361054083140, 36.00893115100078745, 1.131784320476157264E-15 ) ) ;
#504 = CARTESIAN_POINT ( 'NONE',  ( 10.00000000000000000, 54.75893115100078745, -9.846743663894594434 ) ) ;
#505 = EDGE_CURVE ( 'NONE', #98966, #86629, #49108, .T. ) ;
#506 = CARTESIAN_POINT ( 'NONE',  ( -4.164238869374099927, 42.01208216824728936, 3.795296366450308767 ) ) ;
#507 = VERTEX_POINT ( 'NONE', #94282 ) ;
#508 = CARTESIAN_POINT ( 'NONE',  ( -2.266590686148945544, 7.220415501580634832, 7.082119434687048631 ) ) ;
#509 = VECTOR ( 'NONE', #13114, 1000.000000000000000 ) ;
#510 = EDGE_CURVE ( 'NONE', #54365, #74552, #66998, .T. ) ;
#511 = CARTESIAN_POINT ( 'NONE',  ( 19.42250999205614193, 60.14701867748817676, 5.440088680355555262 ) ) ;
#512 = CARTESIAN_POINT ( 'NONE',  ( 1.881645754503864953, -2.851112900457974152E-15, -14.50406564081096406 ) ) ;
#513 = CARTESIAN_POINT ( 'NONE',  ( 22.26659068614894466, 53.88708216824731068, 7.082119434687054849 ) ) ;
#514 = CARTESIAN_POINT ( 'NONE',  ( 16.40814093676323893, 10.79030133659708923, 11.09922568453595026 ) ) ;
#515 = AXIS2_PLACEMENT_3D ( 'NONE', #48897, #3417, #2454 ) ;
#516 = CARTESIAN_POINT ( 'NONE',  ( 19.84674366389459621, 3.508931151000785231, 7.409399052514197653E-17 ) ) ;
#517 = AXIS2_PLACEMENT_3D ( 'NONE', #48549, #24101, #1611 ) ;
#518 = CARTESIAN_POINT ( 'NONE',  ( -6.728956594450633766, -2.083701050245576615E-16, -12.98689685418151640 ) ) ;
#519 = CARTESIAN_POINT ( 'NONE',  ( 2.603489959281582777, 31.58210964143329136, 6.499999999999995559 ) ) ;
#520 = CARTESIAN_POINT ( 'NONE',  ( 2.917880565312948704, 57.63708216824731068, 12.26659068614894643 ) ) ;
#521 = LINE ( 'NONE', #78442, #17689 ) ;
#522 = CARTESIAN_POINT ( 'NONE',  ( 4.559911319644449179, 28.89701867748817321, 9.422509992056141925 ) ) ;
#524 = VECTOR ( 'NONE', #59815, 1000.000000000000000 ) ;
#523 = CARTESIAN_POINT ( 'NONE',  ( 20.88017736071110519, 30.56368534415484106, 2.639326808657452039E-16 ) ) ;
#525 = CARTESIAN_POINT ( 'NONE',  ( 10.00000000000000000, 54.75893115100078745, -9.846743663894594434 ) ) ;
#526 = CARTESIAN_POINT ( 'NONE',  ( 22.81628187352647785, 51.62363466993042493, 6.195893100308588602E-16 ) ) ;
#527 = CARTESIAN_POINT ( 'NONE',  ( 0.000000000000000000, 0.000000000000000000, 0.000000000000000000 ) ) ;
#528 = ORIENTED_EDGE ( 'NONE', *, *, #21195, .F. ) ;
#529 = CARTESIAN_POINT ( 'NONE',  ( 7.084665262690076126, 17.02201867748817676, -10.88017736071110164 ) ) ;
#530 = CARTESIAN_POINT ( 'NONE',  ( -2.816281873526473856, 14.33196800326375531, 3.434112377981055619 ) ) ;
#531 = CARTESIAN_POINT ( 'NONE',  ( -10.00000000000000000, 82.00000000000000000, 5.000000000000000000 ) ) ;
#532 = CARTESIAN_POINT ( 'NONE',  ( 17.20831665107776587, 42.88393115100077324, 7.208316651077764980 ) ) ;
#533 = CARTESIAN_POINT ( 'NONE',  ( -0.8801773607111009756, 48.06368534415484817, 1.068504757029289695E-15 ) ) ;
#534 = CARTESIAN_POINT ( 'NONE',  ( 10.00000000000000000, 27.87363466993042138, -12.81628187352647608 ) ) ;
#536 = CARTESIAN_POINT ( 'NONE',  ( 13.30119215211282047, 0.2301510699511992164, -6.804450086557198851 ) ) ;
#535 = CARTESIAN_POINT ( 'NONE',  ( 0.5774900079438590739, 52.64701867748817676, -5.440088680355550821 ) ) ;
#537 = CARTESIAN_POINT ( 'NONE',  ( 19.50000000000000000, 3.304235192336776005E-17, -4.500000000000001776 ) ) ;
#538 = VERTEX_POINT ( 'NONE', #32791 ) ;
#539 = LINE ( 'NONE', #73152, #10187 ) ;
#540 = LINE ( 'NONE', #46011, #12696 ) ;
#541 = CARTESIAN_POINT ( 'NONE',  ( 20.88017736071110164, 50.35535201082151247, 2.915334737309930979 ) ) ;
#542 = CARTESIAN_POINT ( 'NONE',  ( 22.81628187352647785, 41.62363466993042493, 6.195893100308588602E-16 ) ) ;
#543 = EDGE_CURVE ( 'NONE', #1556, #53389, #1840, .T. ) ;
#544 = AXIS2_PLACEMENT_3D ( 'NONE', #93741, #61758, #9760 ) ;
#545 = CARTESIAN_POINT ( 'NONE',  ( 18.52753015748618282, 63.92559781766745886, -4.923371831947291888 ) ) ;
#546 = CARTESIAN_POINT ( 'NONE',  ( 14.92337183194729633, 32.67559781766745175, 8.527530157486181039 ) ) ;
#547 = CARTESIAN_POINT ( 'NONE',  ( 1.472469842513823179, 10.59226448433411782, -4.923371831947296329 ) ) ;
#548 = PLANE ( 'NONE',  #17195 ) ;
#549 = CARTESIAN_POINT ( 'NONE',  ( 10.00000000000000178, 48.05374883491396787, 14.16423886937410082 ) ) ;
#550 =( BOUNDED_CURVE ( )  B_SPLINE_CURVE ( 2, ( #98605, #14593, #6092, #22091, #15581, #28586, #76549, #67588, #76059 ),
 .UNSPECIFIED., .F., .T. ) 
 B_SPLINE_CURVE_WITH_KNOTS ( ( 3, 2, 2, 2, 3 ),
 ( 0.5115695083688026612, 0.5119047619047618625, 0.5178571428571427937, 0.5238095238095238360, 0.5241447773454830372 ),
 .UNSPECIFIED. ) 
 CURVE ( )  GEOMETRIC_REPRESENTATION_ITEM ( )  RATIONAL_B_SPLINE_CURVE ( ( 0.9963778908391753841, 0.9980808541467917072, 1.000000000000000000, 0.9659258262890683122, 1.000000000000000000, 0.9659258262890683122, 1.000000000000000000, 0.9980808541467917072, 0.9963778908391753841 ) ) 
 REPRESENTATION_ITEM ( '' )  );
#551 = CARTESIAN_POINT ( 'NONE',  ( 0.5774900079438607392, 3.480352010821504027, 5.440088680355550821 ) ) ;
#552 = CARTESIAN_POINT ( 'NONE',  ( -0.8801773607111008646, 3.272018677488171434, 2.915334737309923430 ) ) ;
#553 = EDGE_CURVE ( 'NONE', #69641, #95502, #9313, .T. ) ;
#554 = CARTESIAN_POINT ( 'NONE',  ( -5.580560104534955101, -28.67655754327235584, -4.000000000000000000 ) ) ;
#555 = ORIENTED_EDGE ( 'NONE', *, *, #26429, .F. ) ;
#556 = ORIENTED_EDGE ( 'NONE', *, *, #48860, .F. ) ;
#557 = VECTOR ( 'NONE', #45943, 1000.000000000000000 ) ;
#558 = CARTESIAN_POINT ( 'NONE',  ( 2.035157376598824452, 3.688685344154837953, 7.964842623401179544 ) ) ;
#559 = CARTESIAN_POINT ( 'NONE',  ( -0.8801773607110991993, 12.85535201082150358, -2.915334737309923874 ) ) ;
#560 = CARTESIAN_POINT ( 'NONE',  ( 19.84674366389459266, 43.30059781766744464, 2.638427012816836559 ) ) ;
#561 = CARTESIAN_POINT ( 'NONE',  ( 10.00000000000000178, 35.37363466993042493, 12.81628187352647608 ) ) ;
#562 = CARTESIAN_POINT ( 'NONE',  ( -13.69000000000001549, 92.00000000000000000, -10.09898361729590199 ) ) ;
#564 = CARTESIAN_POINT ( 'NONE',  ( 2.917880565312948704, 12.63708216824730179, 12.26659068614894643 ) ) ;
#563 = DIRECTION ( 'NONE',  ( -8.881784197001252323E-16, 0.000000000000000000, 1.000000000000000000 ) ) ;
#565 = CARTESIAN_POINT ( 'NONE',  ( 15.44008868035555793, 26.39701867748817321, -9.422509992056140149 ) ) ;
#566 = CARTESIAN_POINT ( 'NONE',  ( 10.00000000000000178, 68.05374883491397497, 14.16423886937410082 ) ) ;
#567 = CARTESIAN_POINT ( 'NONE',  ( 19.84674366389459266, 38.30059781766745175, 2.638427012816836559 ) ) ;
#568 = LINE ( 'NONE', #15061, #79560 ) ;
#569 = CARTESIAN_POINT ( 'NONE',  ( 2.791683348922240793, 21.63393115100078745, 7.208316651077764092 ) ) ;
#570 = SURFACE_SIDE_STYLE ('',( #91028 ) ) ;
#571 = CARTESIAN_POINT ( 'NONE',  ( -3.434112377981067610, -41.91803199673623936, -12.81628187352647252 ) ) ;
#572 = ORIENTED_EDGE ( 'NONE', *, *, #57066, .F. ) ;
#573 = CARTESIAN_POINT ( 'NONE',  ( 2.035157376598822676, 2.438685344154837953, -7.964842623401177768 ) ) ;
#574 = ORIENTED_EDGE ( 'NONE', *, *, #38436, .F. ) ;
#575 = CARTESIAN_POINT ( 'NONE',  ( 0.1532563361054082862, 56.21726448433411605, 2.638427012816831674 ) ) ;
#577 = CARTESIAN_POINT ( 'NONE',  ( 20.88017736071110875, 40.77201867748818387, -2.915334737309920765 ) ) ;
#576 = CARTESIAN_POINT ( 'NONE',  ( 20.88017736071110875, 35.77201867748816966, -2.915334737309920765 ) ) ;
#579 = CARTESIAN_POINT ( 'NONE',  ( 16.40814093676324603, 32.45696800326375353, -11.09922568453594671 ) ) ;
#578 = CARTESIAN_POINT ( 'NONE',  ( 12.91533473730993009, 6.605352010821504471, -10.88017736071109987 ) ) ;
#580 = CARTESIAN_POINT ( 'NONE',  ( 13.79529636645031943, 15.34541550158063750, -14.16423886937409904 ) ) ;
#581 = AXIS2_PLACEMENT_3D ( 'NONE', #82369, #74368, #90856 ) ;
#582 = CARTESIAN_POINT ( 'NONE',  ( 22.81628187352648496, 51.83196800326376064, -3.434112377981050290 ) ) ;
#583 = ORIENTED_EDGE ( 'NONE', *, *, #80611, .T. ) ;
#584 = AXIS2_PLACEMENT_3D ( 'NONE', #70041, #3034, #55528 ) ;
#585 = CARTESIAN_POINT ( 'NONE',  ( 5.076628168052704559, 40.17559781766745175, -8.527530157486179263 ) ) ;
#586 = CARTESIAN_POINT ( 'NONE',  ( 2.035157376598824452, 23.68868534415484461, 7.964842623401179544 ) ) ;
#587 = VERTEX_POINT ( 'NONE', #25325 ) ;
#588 = AXIS2_PLACEMENT_3D ( 'NONE', #25960, #34918, #10951 ) ;
#589 = CARTESIAN_POINT ( 'NONE',  ( 20.88017736071110875, 15.77201867748817143, -2.915334737309920765 ) ) ;
#590 = ORIENTED_EDGE ( 'NONE', *, *, #95067, .T. ) ;
#591 = CARTESIAN_POINT ( 'NONE',  ( 17.96484262340118221, 54.93868534415484106, 7.964842623401181321 ) ) ;
#592 = CARTESIAN_POINT ( 'NONE',  ( -0.8801773607111008646, 68.27201867748817676, 2.915334737309923430 ) ) ;
#594 = ADVANCED_FACE ( 'NONE', ( #47799 ), #2628, .T. ) ;
#593 = CARTESIAN_POINT ( 'NONE',  ( 20.88017736071110164, 60.35535201082151957, 2.915334737309930979 ) ) ;
#595 =( GEOMETRIC_REPRESENTATION_CONTEXT ( 3 ) GLOBAL_UNCERTAINTY_ASSIGNED_CONTEXT ( ( #30226 ) ) GLOBAL_UNIT_ASSIGNED_CONTEXT ( ( #63751, #69807, #85295 ) ) REPRESENTATION_CONTEXT ( 'NONE', 'WORKASPACE' ) );
#596 = CARTESIAN_POINT ( 'NONE',  ( 2.791683348922237240, 15.38393115100078212, -7.208316651077763204 ) ) ;
#597 = CARTESIAN_POINT ( 'NONE',  ( 7.084665262690076126, 49.10535201082149825, 10.88017736071109987 ) ) ;
#598 = LINE ( 'NONE', #86029, #77826 ) ;
#599 = EDGE_CURVE ( 'NONE', #79717, #54884, #31804, .T. ) ;
#600 = CARTESIAN_POINT ( 'NONE',  ( -46.94000000000001194, 100.9546402834806713, 8.718409068399685324 ) ) ;
#602 = ORIENTED_EDGE ( 'NONE', *, *, #96478, .F. ) ;
#601 = CARTESIAN_POINT ( 'NONE',  ( 11.08989791451569396, -87.81815274841501662, 4.000000000000000888 ) ) ;
#603 = CARTESIAN_POINT ( 'NONE',  ( 5.076628168052704559, 40.17559781766745175, -8.527530157486179263 ) ) ;
#604 = ORIENTED_EDGE ( 'NONE', *, *, #21453, .F. ) ;
#605 = ORIENTED_EDGE ( 'NONE', *, *, #79248, .F. ) ;
#606 = CARTESIAN_POINT ( 'NONE',  ( -2.261421327065782805, 0.000000000000000000, 4.962236210031227834 ) ) ;
#607 = CARTESIAN_POINT ( 'NONE',  ( 15.99538290524656503, 15.00000000000000000, 0.1584996864329874799 ) ) ;
#608 = CARTESIAN_POINT ( 'NONE',  ( -0.3689425029237881626, 22.42874883491397142, 10.36894250292379027 ) ) ;
#609 = CARTESIAN_POINT ( 'NONE',  ( 20.15039907845753220, 29.72266099184918531, 6.262539305110077947 ) ) ;
#611 = CARTESIAN_POINT ( 'NONE',  ( 2.035157376598822676, 57.43868534415484106, -7.964842623401177768 ) ) ;
#610 = CARTESIAN_POINT ( 'NONE',  ( 19.39188664607694079, 10.83703382326400266, -6.499999999999999112 ) ) ;
#612 = CARTESIAN_POINT ( 'NONE',  ( -0.8801773607111008646, 3.272018677488171434, 2.915334737309923430 ) ) ;
#613 = CARTESIAN_POINT ( 'NONE',  ( 1.472469842513823179, 65.59226448433412315, -4.923371831947296329 ) ) ;
#614 = CARTESIAN_POINT ( 'NONE',  ( 5.076628168052703671, 1.842264484334118047, 8.527530157486179263 ) ) ;
#615 = CARTESIAN_POINT ( 'NONE',  ( 7.361572987183169658, 4.967264484334119601, -9.846743663894592657 ) ) ;
#616 = CARTESIAN_POINT ( 'NONE',  ( 10.00000000000000000, 37.87363466993041783, -12.81628187352647608 ) ) ;
#617 = CARTESIAN_POINT ( 'NONE',  ( 5.076628168052704559, 25.17559781766745175, -8.527530157486179263 ) ) ;
#618 = PLANE ( 'NONE',  #88836 ) ;
#619 = CARTESIAN_POINT ( 'NONE',  ( 22.81628187352647785, 21.41530133659708923, 3.434112377981063169 ) ) ;
#620 = EDGE_CURVE ( 'NONE', #27580, #78252, #34744, .T. ) ;
#621 = CARTESIAN_POINT ( 'NONE',  ( 7.361572987183169658, -0.03273551566588185635, -9.846743663894592657 ) ) ;
#622 = ORIENTED_EDGE ( 'NONE', *, *, #68148, .T. ) ;
#623 = ORIENTED_EDGE ( 'NONE', *, *, #11453, .T. ) ;
#624 = EDGE_CURVE ( 'NONE', #55254, #84180, #16333, .T. ) ;
#625 = CARTESIAN_POINT ( 'NONE',  ( 15.44008868035555260, 19.73035201082150536, 9.422509992056143702 ) ) ;
#626 = CARTESIAN_POINT ( 'NONE',  ( 20.36894250292379382, 18.67874883491397142, 10.36894250292379205 ) ) ;
#627 = CARTESIAN_POINT ( 'NONE',  ( 14.92337183194729633, 42.67559781766745886, 8.527530157486181039 ) ) ;
#628 = CARTESIAN_POINT ( 'NONE',  ( 12.91533473730993009, 66.60535201082150536, -10.88017736071109987 ) ) ;
#630 = DIRECTION ( 'NONE',  ( 0.000000000000000000, 1.000000000000000000, 0.000000000000000000 ) ) ;
#629 = CARTESIAN_POINT ( 'NONE',  ( 22.81628187352648496, 46.83196800326376064, -3.434112377981050290 ) ) ;
#631 = CARTESIAN_POINT ( 'NONE',  ( 7.084665262690076126, 22.02201867748817321, -10.88017736071110164 ) ) ;
#632 = CARTESIAN_POINT ( 'NONE',  ( 7.313705784284644906, 14.49999999999999112, -13.09617149020747817 ) ) ;
#633 = CARTESIAN_POINT ( 'NONE',  ( 16.40814093676323893, 10.79030133659708923, 11.09922568453595026 ) ) ;
#634 = CARTESIAN_POINT ( 'NONE',  ( 3.591859063236763294, 3.290301336597087012, -11.09922568453595026 ) ) ;
#635 = CARTESIAN_POINT ( 'NONE',  ( 1.472469842513823179, 31.42559781766745530, 4.923371831947296329 ) ) ;
#636 = CARTESIAN_POINT ( 'NONE',  ( 5.440088680355549045, -8.602981322511817908, -9.422509992056141925 ) ) ;
#637 = CARTESIAN_POINT ( 'NONE',  ( 22.81628187352648496, 46.83196800326376064, -3.434112377981050290 ) ) ;
#639 = DIRECTION ( 'NONE',  ( 0.000000000000000000, 0.000000000000000000, 1.000000000000000000 ) ) ;
#638 = CARTESIAN_POINT ( 'NONE',  ( 0.5774900079438607392, 48.48035201082150536, 5.440088680355550821 ) ) ;
#640 = CARTESIAN_POINT ( 'NONE',  ( -14.62617646268086524, 0.3639308321805994062, -3.327906561567071986 ) ) ;
#641 = CARTESIAN_POINT ( 'NONE',  ( 20.10421743870887212, 20.60736173766201773, -6.337391062633416894 ) ) ;
#642 = CARTESIAN_POINT ( 'NONE',  ( 19.42250999205614193, 45.14701867748817676, 5.440088680355555262 ) ) ;
#643 = CARTESIAN_POINT ( 'NONE',  ( 19.42250999205614193, 50.14701867748817676, 5.440088680355555262 ) ) ;
#644 = CARTESIAN_POINT ( 'NONE',  ( 18.52753015748618282, 63.92559781766745886, -4.923371831947291888 ) ) ;
#645 = CARTESIAN_POINT ( 'NONE',  ( 7.084665262690076126, 62.02201867748816966, -10.88017736071110164 ) ) ;
#646 = CIRCLE ( 'NONE', #50126, 0.5000000000000004441 ) ;
#647 = CARTESIAN_POINT ( 'NONE',  ( 10.00000000000000178, 52.25893115100078745, 9.846743663894594434 ) ) ;
#649 = DIRECTION ( 'NONE',  ( 0.000000000000000000, 1.000000000000000000, 0.000000000000000000 ) ) ;
#648 = CARTESIAN_POINT ( 'NONE',  ( 4.559911319644449179, 13.89701867748817143, 9.422509992056141925 ) ) ;
#650 = CARTESIAN_POINT ( 'NONE',  ( -2.816281873526471635, 13.91530133659708746, -3.434112377981056508 ) ) ;
#651 = VERTEX_POINT ( 'NONE', #85315 ) ;
#652 = CARTESIAN_POINT ( 'NONE',  ( -0.8801773607110991993, 37.85535201082151247, -2.915334737309923874 ) ) ;
#654 = CYLINDRICAL_SURFACE ( 'NONE', #4662, 2.999999999999999112 ) ;
#653 = CARTESIAN_POINT ( 'NONE',  ( 3.591859063236763294, 3.290301336597087012, -11.09922568453595026 ) ) ;
#655 = EDGE_CURVE ( 'NONE', #6373, #42611, #90428, .T. ) ;
#656 = CARTESIAN_POINT ( 'NONE',  ( 17.96484262340118221, 16.18868534415483396, -7.964842623401177768 ) ) ;
#657 = CARTESIAN_POINT ( 'NONE',  ( 0.5774900079438590739, 27.64701867748817676, -5.440088680355550821 ) ) ;
#658 = CARTESIAN_POINT ( 'NONE',  ( 24.16423886937410614, 34.51208216824731068, -3.795296366450302550 ) ) ;
#659 = CARTESIAN_POINT ( 'NONE',  ( 17.20831665107776587, 24.13393115100078035, -7.208316651077762316 ) ) ;
#660 = CARTESIAN_POINT ( 'NONE',  ( 2.035157376598822676, 57.43868534415484106, -7.964842623401177768 ) ) ;
#661 = FACE_OUTER_BOUND ( 'NONE', #43555, .T. ) ;
#662 = CARTESIAN_POINT ( 'NONE',  ( 19.84674366389459621, 63.50893115100078745, 7.409399052514197653E-17 ) ) ;
#663 = VERTEX_POINT ( 'NONE', #55810 ) ;
#664 = ORIENTED_EDGE ( 'NONE', *, *, #80208, .F. ) ;
#665 = CARTESIAN_POINT ( 'NONE',  ( 6.204703633549690345, 32.84541550158063927, 14.16423886937410082 ) ) ;
#666 = CARTESIAN_POINT ( 'NONE',  ( 24.16423886937410614, 39.51208216824731068, -3.795296366450302550 ) ) ;
#667 = CARTESIAN_POINT ( 'NONE',  ( 0.1532563361054082862, 1.217264484334117824, 2.638427012816831674 ) ) ;
#668 = CARTESIAN_POINT ( 'NONE',  ( 19.84674366389459266, 58.30059781766745886, 2.638427012816836559 ) ) ;
#669 = CARTESIAN_POINT ( 'NONE',  ( -11.60563658634833040, -81.99692803277896758, 4.000000000000001776 ) ) ;
#671 = CARTESIAN_POINT ( 'NONE',  ( 22.81628187352648496, 21.83196800326374643, -3.434112377981050290 ) ) ;
#670 = CARTESIAN_POINT ( 'NONE',  ( 19.42250999205614193, 60.14701867748817676, 5.440088680355555262 ) ) ;
#672 = CARTESIAN_POINT ( 'NONE',  ( 17.08211943468705840, 25.13708216824730357, -12.26659068614894466 ) ) ;
#673 = CARTESIAN_POINT ( 'NONE',  ( 10.00000000000000178, 19.31368534415484106, 10.88017736071110342 ) ) ;
#674 = CARTESIAN_POINT ( 'NONE',  ( 12.91533473730993009, 26.60535201082150536, -10.88017736071109987 ) ) ;
#675 = CARTESIAN_POINT ( 'NONE',  ( -8.606322355891443010, 15.00000000000000000, 11.66967075398801335 ) ) ;
#676 = CARTESIAN_POINT ( 'NONE',  ( 2.035157376598822676, 57.43868534415484106, -7.964842623401177768 ) ) ;
#677 = CARTESIAN_POINT ( 'NONE',  ( 10.00000000000000000, 52.87363466993041783, -12.81628187352647608 ) ) ;
#678 = CARTESIAN_POINT ( 'NONE',  ( -4.923371831947292776, -8.157735515665876846, 8.527530157486181039 ) ) ;
#679 = ORIENTED_EDGE ( 'NONE', *, *, #13478, .F. ) ;
#680 = SURFACE_SIDE_STYLE ('',( #69155 ) ) ;
#681 = ORIENTED_EDGE ( 'NONE', *, *, #51264, .T. ) ;
#682 = CARTESIAN_POINT ( 'NONE',  ( -0.1503990784575277295, 54.24884699246889852, -6.262539305110077947 ) ) ;
#683 = EDGE_LOOP ( 'NONE', ( #89286, #70772, #2079, #80343 ) ) ;
#685 = CARTESIAN_POINT ( 'NONE',  ( -0.8801773607111008646, 3.272018677488171434, 2.915334737309923430 ) ) ;
#684 = CARTESIAN_POINT ( 'NONE',  ( -4.164238869374099039, 56.80374883491397497, 8.674139862899312516E-16 ) ) ;
#687 = CARTESIAN_POINT ( 'NONE',  ( 1.472469842513823179, 56.42559781766745886, 4.923371831947296329 ) ) ;
#686 = CARTESIAN_POINT ( 'NONE',  ( 12.63842701281683922, 34.55059781766745886, -9.846743663894590881 ) ) ;
#688 = CARTESIAN_POINT ( 'NONE',  ( -3.999999999999994671, 43.00000000000000711, 6.500000000000000888 ) ) ;
#689 = CARTESIAN_POINT ( 'NONE',  ( 0.1532563361054100626, 10.80059781766745175, -2.638427012816831230 ) ) ;
#690 = CARTESIAN_POINT ( 'NONE',  ( 19.38216949554541557, 2.248634669930420049, -9.382169495545420901 ) ) ;
#691 = CARTESIAN_POINT ( 'NONE',  ( 12.81628187352647608, 26.62363466993042493, -2.602085213965210642E-15 ) ) ;
#692 = ORIENTED_EDGE ( 'NONE', *, *, #60606, .T. ) ;
#693 = CARTESIAN_POINT ( 'NONE',  ( 24.16423886937410614, 49.30374883491396787, 8.672049930838204340E-16 ) ) ;
#694 = ORIENTED_EDGE ( 'NONE', *, *, #84783, .T. ) ;
#695 = CARTESIAN_POINT ( 'NONE',  ( -0.3689425029237881626, 37.42874883491396787, 10.36894250292379027 ) ) ;
#696 = EDGE_LOOP ( 'NONE', ( #40227, #25908, #8282, #49239, #90855, #86389 ) ) ;
#697 = CARTESIAN_POINT ( 'NONE',  ( 6.565887622018943937, 58.08196800326376064, -12.81628187352647608 ) ) ;
#698 = CARTESIAN_POINT ( 'NONE',  ( 19.42250999205614193, 30.14701867748817321, 5.440088680355555262 ) ) ;
#699 = CARTESIAN_POINT ( 'NONE',  ( 18.52753015748618282, 43.92559781766745175, -4.923371831947291888 ) ) ;
#700 = CARTESIAN_POINT ( 'NONE',  ( 7.084665262690076126, 24.10535201082150181, 10.88017736071109987 ) ) ;
#701 = CARTESIAN_POINT ( 'NONE',  ( -1.926860441876563801, 64.89664270246085209, 3.195792623639529761 ) ) ;
#702 = CARTESIAN_POINT ( 'NONE',  ( 19.84674366389459266, 53.71726448433411605, -2.638427012816827677 ) ) ;
#703 = CARTESIAN_POINT ( 'NONE',  ( 19.84674366389459266, 48.30059781766745175, 2.638427012816836559 ) ) ;
#704 = EDGE_CURVE ( 'NONE', #20604, #37674, #29970, .T. ) ;
#705 = CARTESIAN_POINT ( 'NONE',  ( 0.000000000000000000, 14.49999999999999822, 0.000000000000000000 ) ) ;
#706 = CARTESIAN_POINT ( 'NONE',  ( -14.35840480524201190, 14.49999999999999112, -4.340070442839034648 ) ) ;
#707 = AXIS2_PLACEMENT_3D ( 'NONE', #2561, #55539, #79512 ) ;
#708 = CARTESIAN_POINT ( 'NONE',  ( 17.85158348494335812, 19.73726573380441351, -6.499999999999992895 ) ) ;
#709 = EDGE_LOOP ( 'NONE', ( #92265, #29499, #42364, #81425, #71041, #49947 ) ) ;
#710 = DIRECTION ( 'NONE',  ( 0.000000000000000000, -0.000000000000000000, -1.000000000000000000 ) ) ;
#711 = CARTESIAN_POINT ( 'NONE',  ( 2.791683348922237240, 35.38393115100079456, -7.208316651077763204 ) ) ;
#712 = CARTESIAN_POINT ( 'NONE',  ( -15.94536257719939698, 15.00000000000000000, -1.273895096820171657 ) ) ;
#713 = CARTESIAN_POINT ( 'NONE',  ( 13.43411237798106583, 32.66530133659708213, -12.81628187352647252 ) ) ;
#715 = DIRECTION ( 'NONE',  ( -0.000000000000000000, -0.000000000000000000, 1.000000000000000000 ) ) ;
#714 = AXIS2_PLACEMENT_3D ( 'NONE', #93061, #56067, #79045 ) ;
#716 = DIRECTION ( 'NONE',  ( 0.000000000000000000, 0.000000000000000000, 1.000000000000000000 ) ) ;
#717 = VERTEX_POINT ( 'NONE', #42770 ) ;
#718 = CARTESIAN_POINT ( 'NONE',  ( 10.00000000000000000, 64.75893115100078035, -9.846743663894594434 ) ) ;
#719 = CARTESIAN_POINT ( 'NONE',  ( -11.59580422753514384, 14.76984949557107640, -9.421229451860563486 ) ) ;
#720 = CARTESIAN_POINT ( 'NONE',  ( 10.00000000000000178, 57.25893115100078745, 9.846743663894594434 ) ) ;
#721 = CARTESIAN_POINT ( 'NONE',  ( 24.16423886937410614, 39.30374883491396787, 8.672049930838204340E-16 ) ) ;
#722 = CARTESIAN_POINT ( 'NONE',  ( 2.791683348922237240, 60.38393115100078745, -7.208316651077763204 ) ) ;
#723 = FACE_OUTER_BOUND ( 'NONE', #60066, .T. ) ;
#724 = CARTESIAN_POINT ( 'NONE',  ( 2.791683348922237240, 15.38393115100078212, -7.208316651077763204 ) ) ;
#725 = CARTESIAN_POINT ( 'NONE',  ( -2.816281873526471635, 53.91530133659709634, -3.434112377981056508 ) ) ;
#726 = CARTESIAN_POINT ( 'NONE',  ( 5.076628168052703671, 61.84226448433412315, 8.527530157486179263 ) ) ;
#727 = CARTESIAN_POINT ( 'NONE',  ( 7.084665262690076126, 49.10535201082149825, 10.88017736071109987 ) ) ;
#728 = CARTESIAN_POINT ( 'NONE',  ( 7.361572987183170547, 47.05059781766745175, 9.846743663894590881 ) ) ;
#729 = CONTEXT_DEPENDENT_SHAPE_REPRESENTATION ( #51961, #1989 ) ;
#730 = CARTESIAN_POINT ( 'NONE',  ( 6.034042420210333546, -36.05779855178114701, -2.750000000000001332 ) ) ;
#731 = EDGE_CURVE ( 'NONE', #11978, #70278, #61820, .T. ) ;
#732 = CARTESIAN_POINT ( 'NONE',  ( 0.5774900079438607392, 53.48035201082151247, 5.440088680355550821 ) ) ;
#733 = ORIENTED_EDGE ( 'NONE', *, *, #34970, .T. ) ;
#734 = EDGE_CURVE ( 'NONE', #717, #9323, #56198, .T. ) ;
#735 = CARTESIAN_POINT ( 'NONE',  ( 14.82269085861167390, 14.49999999999999822, 2.299529454047062327 ) ) ;
#736 = CARTESIAN_POINT ( 'NONE',  ( 4.559911319644449179, 32.23035201082150536, -9.422509992056141925 ) ) ;
#738 = CARTESIAN_POINT ( 'NONE',  ( 4.559911319644449179, 58.89701867748817676, 9.422509992056141925 ) ) ;
#737 = CARTESIAN_POINT ( 'NONE',  ( 10.00000000000000000, 2.873634669930420049, -12.81628187352647608 ) ) ;
#739 = DIRECTION ( 'NONE',  ( 0.000000000000000000, 0.000000000000000000, -1.000000000000000000 ) ) ;
#740 = CARTESIAN_POINT ( 'NONE',  ( 20.10421743870887568, 10.60736173766201773, -6.337391062633407124 ) ) ;
#741 = CARTESIAN_POINT ( 'NONE',  ( 3.195792623639593266, 4.120456701841152203, 11.92686044187653494 ) ) ;
#743 = DIRECTION ( 'NONE',  ( 0.000000000000000000, 1.000000000000000000, 0.000000000000000000 ) ) ;
#742 = CARTESIAN_POINT ( 'NONE',  ( 19.42250999205614548, 45.98035201082150536, -5.440088680355545492 ) ) ;
#744 = CARTESIAN_POINT ( 'NONE',  ( 7.361572987183169658, 34.96726448433411605, -9.846743663894592657 ) ) ;
#745 = DIRECTION ( 'NONE',  ( -0.8320502943378437211, 0.5547001962252290364, 0.000000000000000000 ) ) ;
#746 = CARTESIAN_POINT ( 'NONE',  ( 14.16423886937410082, 19.51208216824730712, -3.795296366450314096 ) ) ;
#747 = CARTESIAN_POINT ( 'NONE',  ( 7.361572987183170547, 62.05059781766745886, 9.846743663894590881 ) ) ;
#748 = CARTESIAN_POINT ( 'NONE',  ( -0.8801773607110991993, 7.855352010821506248, -2.915334737309923874 ) ) ;
#749 = CARTESIAN_POINT ( 'NONE',  ( 3.270351084886796933, 14.95037111082768000, -14.38617789677962655 ) ) ;
#750 = CIRCLE ( 'NONE', #66369, 0.1000000000000001166 ) ;
#751 = CARTESIAN_POINT ( 'NONE',  ( 2.917880565312948704, 27.63708216824730357, 12.26659068614894643 ) ) ;
#752 = CARTESIAN_POINT ( 'NONE',  ( 10.00000000000000178, 58.05374883491397497, 14.16423886937410082 ) ) ;
#753 = CARTESIAN_POINT ( 'NONE',  ( 12.63842701281683922, 34.55059781766745886, -9.846743663894590881 ) ) ;
#754 = CARTESIAN_POINT ( 'NONE',  ( 0.1532563361054082862, 21.21726448433412315, 2.638427012816831674 ) ) ;
#755 = DIRECTION ( 'NONE',  ( -0.000000000000000000, -1.000000000000000000, -0.000000000000000000 ) ) ;
#756 = ORIENTED_EDGE ( 'NONE', *, *, #56154, .F. ) ;
#757 = CARTESIAN_POINT ( 'NONE',  ( 18.52753015748618282, 28.92559781766745175, -4.923371831947291888 ) ) ;
#758 = CARTESIAN_POINT ( 'NONE',  ( 0.5774900079438590739, 27.64701867748817676, -5.440088680355550821 ) ) ;
#759 = CARTESIAN_POINT ( 'NONE',  ( 0.1532563361054100626, 55.80059781766745175, -2.638427012816831230 ) ) ;
#760 = CARTESIAN_POINT ( 'NONE',  ( 22.26659068614894466, 3.887082168247300906, 7.082119434687054849 ) ) ;
#761 = DIRECTION ( 'NONE',  ( 0.000000000000000000, 0.000000000000000000, -1.000000000000000000 ) ) ;
#762 = CARTESIAN_POINT ( 'NONE',  ( 0.1532563361054082862, 11.21726448433411605, 2.638427012816831674 ) ) ;
#763 = CARTESIAN_POINT ( 'NONE',  ( 21.09922568453595559, 32.04030133659708923, -6.408140936763230044 ) ) ;
#764 = CARTESIAN_POINT ( 'NONE',  ( 17.20831665107776587, 37.88393115100078745, 7.208316651077764980 ) ) ;
#765 = VERTEX_POINT ( 'NONE', #66241 ) ;
#766 = CARTESIAN_POINT ( 'NONE',  ( 0.1532563361054082862, 21.21726448433412315, 2.638427012816831674 ) ) ;
#767 = CARTESIAN_POINT ( 'NONE',  ( 10.68823582872827060, -97.11172657260387098, -4.000000000000000000 ) ) ;
#768 = CARTESIAN_POINT ( 'NONE',  ( -46.58960623550384383, 101.6399765164375850, -8.033401704989589831 ) ) ;
#769 = CARTESIAN_POINT ( 'NONE',  ( -4.164238869374099039, 51.80374883491396787, 8.674139862899312516E-16 ) ) ;
#770 = CARTESIAN_POINT ( 'NONE',  ( 10.00000000000000178, 54.31368534415484106, 10.88017736071110342 ) ) ;
#771 = CARTESIAN_POINT ( 'NONE',  ( 2.035157376598822676, 52.43868534415483396, -7.964842623401177768 ) ) ;
#772 = CARTESIAN_POINT ( 'NONE',  ( 2.791683348922240793, 31.63393115100078745, 7.208316651077764092 ) ) ;
#773 = CARTESIAN_POINT ( 'NONE',  ( 7.084665262690076126, 2.022018677488170990, -10.88017736071110164 ) ) ;
#774 = PRESENTATION_STYLE_ASSIGNMENT (( #85725 ) ) ;
#775 = CARTESIAN_POINT ( 'NONE',  ( 12.63842701281683922, 44.55059781766745175, -9.846743663894590881 ) ) ;
#776 = ADVANCED_FACE ( 'NONE', ( #13253 ), #4285, .T. ) ;
#777 = CARTESIAN_POINT ( 'NONE',  ( 4.559911319644449179, 53.89701867748817676, 9.422509992056141925 ) ) ;
#778 = CARTESIAN_POINT ( 'NONE',  ( 17.20831665107776587, 4.133931151000785675, -7.208316651077762316 ) ) ;
#779 = ORIENTED_EDGE ( 'NONE', *, *, #18509, .T. ) ;
#780 = ORIENTED_EDGE ( 'NONE', *, *, #20104, .T. ) ;
#781 = CARTESIAN_POINT ( 'NONE',  ( 14.03351048042397231, 0.000000000000000000, -2.474486531753715024 ) ) ;
#782 = DIRECTION ( 'NONE',  ( -0.000000000000000000, 1.000000000000000000, 0.000000000000000000 ) ) ;
#783 = CARTESIAN_POINT ( 'NONE',  ( 5.076628168052704559, 20.17559781766745175, -8.527530157486179263 ) ) ;
#784 = CARTESIAN_POINT ( 'NONE',  ( 10.00000000000000178, 55.37363466993042493, 12.81628187352647608 ) ) ;
#786 = CARTESIAN_POINT ( 'NONE',  ( 2.791683348922240793, 46.63393115100077324, 7.208316651077764092 ) ) ;
#785 = CARTESIAN_POINT ( 'NONE',  ( 4.559911319644449179, 13.89701867748817321, 9.422509992056141925 ) ) ;
#787 = LINE ( 'NONE', #31240, #15154 ) ;
#788 = CARTESIAN_POINT ( 'NONE',  ( 10.00000000000000178, 28.05374883491396787, 14.16423886937410082 ) ) ;
#789 = CARTESIAN_POINT ( 'NONE',  ( 20.36894250292379738, 59.92874883491397497, -10.36894250292379027 ) ) ;
#790 = CARTESIAN_POINT ( 'NONE',  ( 12.63842701281683922, 54.55059781766745175, -9.846743663894590881 ) ) ;
#791 = CARTESIAN_POINT ( 'NONE',  ( 15.44008868035555260, 49.73035201082150536, 9.422509992056143702 ) ) ;
#792 = AXIS2_PLACEMENT_3D ( 'NONE', #36008, #73504, #34024 ) ;
#793 = CARTESIAN_POINT ( 'NONE',  ( 1.472469842513823179, 15.59226448433411960, -4.923371831947296329 ) ) ;
#794 = CARTESIAN_POINT ( 'NONE',  ( -3.772059543480554389, -0.8421633283343330501, 3.999999999999999112 ) ) ;
#795 = EDGE_LOOP ( 'NONE', ( #13304, #46664, #87844, #53045 ) ) ;
#796 = B_SPLINE_CURVE_WITH_KNOTS ( 'NONE', 3,
 ( #44696, #708, #68688, #75192 ),
 .UNSPECIFIED., .F., .F.,
 ( 4, 4 ),
 ( 0.000000000000000000, 0.002392975128318422604 ),
 .UNSPECIFIED. ) ;
#797 = LINE ( 'NONE', #31249, #42721 ) ;
#798 = ORIENTED_EDGE ( 'NONE', *, *, #95058, .F. ) ;
#799 = CARTESIAN_POINT ( 'NONE',  ( 19.84674366389459621, 8.508931151000785675, 7.409399052514197653E-17 ) ) ;
#800 = VERTEX_POINT ( 'NONE', #21761 ) ;
#801 = CARTESIAN_POINT ( 'NONE',  ( -4.164238869374098151, 21.59541550158063217, -3.795296366450310543 ) ) ;
#802 = CARTESIAN_POINT ( 'NONE',  ( 19.84674366389459266, 18.71726448433411960, -2.638427012816827677 ) ) ;
#803 = CARTESIAN_POINT ( 'NONE',  ( 15.44008868035555793, 41.39701867748817676, -9.422509992056140149 ) ) ;
#804 = CARTESIAN_POINT ( 'NONE',  ( -5.803070148808146200, 15.00000000000000000, -13.28812917035395813 ) ) ;
#805 = ORIENTED_EDGE ( 'NONE', *, *, #45534, .F. ) ;
#806 = CARTESIAN_POINT ( 'NONE',  ( 2.035157376598824452, 23.68868534415484461, 7.964842623401179544 ) ) ;
#807 = CARTESIAN_POINT ( 'NONE',  ( 2.602060718268849104, 0.000000000000000000, -4.792399674598859072 ) ) ;
#808 = VECTOR ( 'NONE', #6367, 1000.000000000000000 ) ;
#809 = ORIENTED_EDGE ( 'NONE', *, *, #74543, .T. ) ;
#810 = CARTESIAN_POINT ( 'NONE',  ( 2.035157376598822676, 32.43868534415483396, -7.964842623401177768 ) ) ;
#811 = FACE_OUTER_BOUND ( 'NONE', #83164, .T. ) ;
#812 = EDGE_LOOP ( 'NONE', ( #36804, #71222, #33329, #97808 ) ) ;
#813 = CARTESIAN_POINT ( 'NONE',  ( 13.43411237798106583, 22.66530133659708923, -12.81628187352647252 ) ) ;
#814 =( LENGTH_UNIT ( ) NAMED_UNIT ( * ) SI_UNIT ( .MILLI., .METRE. ) );
#815 = CARTESIAN_POINT ( 'NONE',  ( 5.076628168052704559, 5.175597817667451750, -8.527530157486179263 ) ) ;
#816 = CARTESIAN_POINT ( 'NONE',  ( 19.84674366389459621, 18.50893115100078745, 7.409399052514197653E-17 ) ) ;
#817 = CARTESIAN_POINT ( 'NONE',  ( 2.035157376598824452, 33.68868534415484106, 7.964842623401179544 ) ) ;
#818 = ADVANCED_FACE ( 'NONE', ( #258 ), #67246, .F. ) ;
#819 = B_SPLINE_CURVE_WITH_KNOTS ( 'NONE', 3,
 ( #42826, #41374, #64319, #73311, #4834, #33813 ),
 .UNSPECIFIED., .F., .F.,
 ( 4, 2, 4 ),
 ( 0.0002800005319459006065, 0.0006862057665691816740, 0.001092411001192462741 ),
 .UNSPECIFIED. ) ;
#820 = ORIENTED_EDGE ( 'NONE', *, *, #72852, .F. ) ;
#821 = DIRECTION ( 'NONE',  ( 1.000000000000000000, 0.000000000000000000, 5.329070518200751394E-15 ) ) ;
#822 = CARTESIAN_POINT ( 'NONE',  ( 0.5774900079438607392, 63.48035201082149825, 5.440088680355550821 ) ) ;
#823 = CARTESIAN_POINT ( 'NONE',  ( -8.000000000000000000, 80.99999999999994316, -1.249999999999987121 ) ) ;
#824 = CARTESIAN_POINT ( 'NONE',  ( 10.00000000000000000, 66.81368534415484817, -10.88017736071110342 ) ) ;
#825 = CARTESIAN_POINT ( 'NONE',  ( 13.43411237798105340, 5.581968003263753531, 12.81628187352647963 ) ) ;
#826 = DIRECTION ( 'NONE',  ( 0.6246950475544238435, 0.7808688094430307203, 0.000000000000000000 ) ) ;
#827 = CARTESIAN_POINT ( 'NONE',  ( 12.63842701281683034, 32.46726448433412315, 9.846743663894596210 ) ) ;
#828 = CARTESIAN_POINT ( 'NONE',  ( -1.099225684535947600, 49.54030133659708923, 6.408140936763237150 ) ) ;
#829 = CARTESIAN_POINT ( 'NONE',  ( 2.153642693323476909, 36.13791097397317742, -6.500000000000079936 ) ) ;
#830 = CARTESIAN_POINT ( 'NONE',  ( 17.20831665107776587, 14.13393115100078568, -7.208316651077762316 ) ) ;
#831 = CARTESIAN_POINT ( 'NONE',  ( -2.816281873526471635, 13.91530133659708746, -3.434112377981056508 ) ) ;
#832 = CARTESIAN_POINT ( 'NONE',  ( -7.116236337400218659, -80.68324593764592123, -2.750000000000000000 ) ) ;
#833 = CARTESIAN_POINT ( 'NONE',  ( 20.88017736071110164, 35.35535201082150536, 2.915334737309930979 ) ) ;
#834 = CARTESIAN_POINT ( 'NONE',  ( 0.1532563361054083140, 61.00893115100078745, 1.131784320476157264E-15 ) ) ;
#835 =( NAMED_UNIT ( * ) SI_UNIT ( $, .STERADIAN. ) SOLID_ANGLE_UNIT ( ) );
#836 = CARTESIAN_POINT ( 'NONE',  ( 2.791683348922237240, 20.38393115100078745, -7.208316651077763204 ) ) ;
#837 = CARTESIAN_POINT ( 'NONE',  ( 18.52753015748618282, 3.925597817667451306, -4.923371831947291888 ) ) ;
#838 = CARTESIAN_POINT ( 'NONE',  ( 19.42250999205614548, 10.98035201082150358, -5.440088680355545492 ) ) ;
#839 = CARTESIAN_POINT ( 'NONE',  ( 19.38216949554541557, 12.24863466993041961, -9.382169495545420901 ) ) ;
#840 = CARTESIAN_POINT ( 'NONE',  ( 14.92337183194729988, 64.34226448433412315, -8.527530157486177487 ) ) ;
#841 = EDGE_CURVE ( 'NONE', #25175, #32896, #62196, .T. ) ;
#842 = PRODUCT_DEFINITION_FORMATION_WITH_SPECIFIED_SOURCE ( 'ANY', '', #6128, .NOT_KNOWN. ) ;
#843 = CARTESIAN_POINT ( 'NONE',  ( 6.685134130357478277, -80.57704203013921074, -2.500000000000000888 ) ) ;
#844 = CARTESIAN_POINT ( 'NONE',  ( 10.00000000000000178, 24.31368534415484106, 10.88017736071110342 ) ) ;
#845 = CARTESIAN_POINT ( 'NONE',  ( 1.472469842513823179, 46.42559781766745175, 4.923371831947296329 ) ) ;
#846 = COLOUR_RGB ( '', 0.40784314, 0.44705882, 0.49803922) ;
#847 = CARTESIAN_POINT ( 'NONE',  ( 4.471352795670365587, -3.620003340340034015, 2.750000000000000000 ) ) ;
#848 = ADVANCED_FACE ( 'NONE', ( #33166 ), #69709, .F. ) ;
#849 = CARTESIAN_POINT ( 'NONE',  ( -0.8801773607111008646, 18.27201867748817321, 2.915334737309923430 ) ) ;
#850 = DIRECTION ( 'NONE',  ( 0.5664062369248313855, 0.000000000000000000, -0.8241261886220165866 ) ) ;
#851 = CARTESIAN_POINT ( 'NONE',  ( -0.8801773607111009756, 28.06368534415484106, 1.068504757029289695E-15 ) ) ;
#853 = CARTESIAN_POINT ( 'NONE',  ( 14.29730467489532408, 4.491438197698105257E-16, 2.416004766803315995 ) ) ;
#852 = CARTESIAN_POINT ( 'NONE',  ( -4.164238869374099039, 66.80374883491396076, 8.674139862899312516E-16 ) ) ;
#854 = CARTESIAN_POINT ( 'NONE',  ( 1.472469842513823179, 0.5922644843341181575, -4.923371831947296329 ) ) ;
#855 = CARTESIAN_POINT ( 'NONE',  ( 18.52753015748617571, 23.09226448433411960, 4.923371831947298993 ) ) ;
#856 = CARTESIAN_POINT ( 'NONE',  ( 0.6178305044545838731, 9.748634669930416052, 9.382169495545420901 ) ) ;
#857 = DIRECTION ( 'NONE',  ( 0.000000000000000000, 0.000000000000000000, 1.000000000000000000 ) ) ;
#858 = CARTESIAN_POINT ( 'NONE',  ( 6.742022620658236320, 0.04962897188439623769, -13.12259272460504533 ) ) ;
#859 = CARTESIAN_POINT ( 'NONE',  ( 14.92337183194729988, 64.34226448433412315, -8.527530157486177487 ) ) ;
#860 = DIRECTION ( 'NONE',  ( -1.000000000000000000, 0.000000000000000000, 0.000000000000000000 ) ) ;
#861 = FILL_AREA_STYLE ('',( #14877 ) ) ;
#862 = CARTESIAN_POINT ( 'NONE',  ( 2.917880565312950480, 10.97041550158063572, -12.26659068614894821 ) ) ;
#863 = CARTESIAN_POINT ( 'NONE',  ( 1.472469842513823179, 35.59226448433412315, -4.923371831947296329 ) ) ;
#864 = DIRECTION ( 'NONE',  ( 0.000000000000000000, 1.000000000000000000, -0.000000000000000000 ) ) ;
#865 = STYLED_ITEM ( 'NONE', ( #71034 ), #8224 ) ;
#866 = CARTESIAN_POINT ( 'NONE',  ( 22.26659068614894466, 53.88708216824731068, 7.082119434687054849 ) ) ;
#867 = CARTESIAN_POINT ( 'NONE',  ( 2.791683348922240793, 16.63393115100078745, 7.208316651077764092 ) ) ;
#869 = DIRECTION ( 'NONE',  ( 0.000000000000000000, 0.000000000000000000, -1.000000000000000000 ) ) ;
#868 = CYLINDRICAL_SURFACE ( 'NONE', #65920, 0.2500000000000002220 ) ;
#870 = CARTESIAN_POINT ( 'NONE',  ( 4.559911319644449179, 43.89701867748816966, 9.422509992056141925 ) ) ;
#871 = CARTESIAN_POINT ( 'NONE',  ( 21.09922568453594849, 56.20696800326375353, 6.408140936763242479 ) ) ;
#872 = CARTESIAN_POINT ( 'NONE',  ( 4.559911319644449179, 23.89701867748817321, 9.422509992056141925 ) ) ;
#873 = CARTESIAN_POINT ( 'NONE',  ( 21.09922568453594849, 46.20696800326376064, 6.408140936763242479 ) ) ;
#874 = CARTESIAN_POINT ( 'NONE',  ( -1.099225684535947600, 3.706968003263753531, -6.408140936763238038 ) ) ;
#875 = VERTEX_POINT ( 'NONE', #9203 ) ;
#876 = SURFACE_STYLE_FILL_AREA ( #39838 ) ;
#877 = CARTESIAN_POINT ( 'NONE',  ( -14.93875075227008509, 0.2301502577613187550, -0.2365588874161651534 ) ) ;
#878 = CARTESIAN_POINT ( 'NONE',  ( 20.36894250292379382, 53.67874883491397497, 10.36894250292379205 ) ) ;
#879 = CARTESIAN_POINT ( 'NONE',  ( -0.3689425029237881626, 17.42874883491397142, 10.36894250292379027 ) ) ;
#880 = CARTESIAN_POINT ( 'NONE',  ( 10.00000000000000178, 14.31368534415483751, 10.88017736071110342 ) ) ;
#881 = CARTESIAN_POINT ( 'NONE',  ( 0.5774900079438607392, 33.48035201082150536, 5.440088680355550821 ) ) ;
#882 = CARTESIAN_POINT ( 'NONE',  ( 9.519554572442958218, 15.00000000000000178, -11.10344954678180329 ) ) ;
#883 = CARTESIAN_POINT ( 'NONE',  ( -46.76873188434316830, 100.6386073946591466, -9.384976975161267276 ) ) ;
#884 = CARTESIAN_POINT ( 'NONE',  ( 7.084665262690076126, 64.10535201082150536, 10.88017736071109987 ) ) ;
#885 = CARTESIAN_POINT ( 'NONE',  ( 17.96484262340118221, 66.18868534415483396, -7.964842623401177768 ) ) ;
#886 = CARTESIAN_POINT ( 'NONE',  ( -2.816281873526473856, 29.33196800326376064, 3.434112377981055619 ) ) ;
#887 = DIRECTION ( 'NONE',  ( 0.1650476058606741014, 0.000000000000000000, 0.9862856015372319929 ) ) ;
#888 = CARTESIAN_POINT ( 'NONE',  ( 17.20831665107776587, 14.13393115100078568, -7.208316651077762316 ) ) ;
#889 = CARTESIAN_POINT ( 'NONE',  ( 18.52753015748617571, 43.09226448433412315, 4.923371831947298993 ) ) ;
#890 = STYLED_ITEM ( 'NONE', ( #61535 ), #52669 ) ;
#891 = EDGE_CURVE ( 'NONE', #46987, #90157, #82265, .T. ) ;
#892 = CARTESIAN_POINT ( 'NONE',  ( 10.00000000000000178, 14.31368534415483751, 10.88017736071110342 ) ) ;
#893 = CARTESIAN_POINT ( 'NONE',  ( 16.40814093676323893, 35.79030133659708923, 11.09922568453595026 ) ) ;
#894 = AXIS2_PLACEMENT_3D ( 'NONE', #5161, #50153, #35647 ) ;
#895 = CARTESIAN_POINT ( 'NONE',  ( 0.1532563361054100626, 10.80059781766745175, -2.638427012816831230 ) ) ;
#896 = CARTESIAN_POINT ( 'NONE',  ( -3.750000000000000000, 37.00000000000000000, 2.500000000000000000 ) ) ;
#897 = CARTESIAN_POINT ( 'NONE',  ( 19.84674366389459621, 53.50893115100078745, 7.409399052514197653E-17 ) ) ;
#898 = CARTESIAN_POINT ( 'NONE',  ( 19.84674366389459266, 28.30059781766745886, 2.638427012816836559 ) ) ;
#899 = CARTESIAN_POINT ( 'NONE',  ( 2.917880565312948704, 17.63708216824730357, 12.26659068614894643 ) ) ;
#900 = CARTESIAN_POINT ( 'NONE',  ( 10.00000000000000000, 36.81368534415484106, -10.88017736071110342 ) ) ;
#901 = CARTESIAN_POINT ( 'NONE',  ( 19.42250999205614193, 5.147018677488171434, 5.440088680355555262 ) ) ;
#902 = EDGE_CURVE ( 'NONE', #80852, #61558, #58673, .T. ) ;
#903 = CARTESIAN_POINT ( 'NONE',  ( 20.88017736071110519, 35.56368534415484106, 2.639326808657452039E-16 ) ) ;
#904 = CARTESIAN_POINT ( 'NONE',  ( -0.8801773607111009756, 28.06368534415484106, 1.068504757029289695E-15 ) ) ;
#905 = ORIENTED_EDGE ( 'NONE', *, *, #91110, .F. ) ;
#906 = CARTESIAN_POINT ( 'NONE',  ( 20.88017736071110164, 35.35535201082150536, 2.915334737309930979 ) ) ;
#907 = ORIENTED_EDGE ( 'NONE', *, *, #41162, .F. ) ;
#908 = CARTESIAN_POINT ( 'NONE',  ( 0.6178305044545818747, 63.49863466993043204, -9.382169495545419124 ) ) ;
#909 = CARTESIAN_POINT ( 'NONE',  ( 7.084665262690076126, 54.10535201082151247, 10.88017736071109987 ) ) ;
#910 = VECTOR ( 'NONE', #54975, 1000.000000000000000 ) ;
#911 = ORIENTED_EDGE ( 'NONE', *, *, #98370, .F. ) ;
#912 = CARTESIAN_POINT ( 'NONE',  ( 17.96484262340118221, 44.93868534415483396, 7.964842623401181321 ) ) ;
#913 = CARTESIAN_POINT ( 'NONE',  ( 7.155633850256548634, -69.45312897839663435, 4.000000000000000000 ) ) ;
#914 = CARTESIAN_POINT ( 'NONE',  ( -0.1503990784575247319, 37.22266099184918176, -6.262539305110083276 ) ) ;
#915 = CARTESIAN_POINT ( 'NONE',  ( -0.3689425029237881626, 62.42874883491396787, 10.36894250292379027 ) ) ;
#916 = CARTESIAN_POINT ( 'NONE',  ( 7.084665262690076126, 64.10535201082150536, 10.88017736071109987 ) ) ;
#917 = DIRECTION ( 'NONE',  ( -1.000000000000000000, 0.000000000000000000, 0.000000000000000000 ) ) ;
#918 = CARTESIAN_POINT ( 'NONE',  ( -6.060849023604187202, -36.09672517615241816, -3.999999999999998224 ) ) ;
#919 = CARTESIAN_POINT ( 'NONE',  ( 2.035157376598822676, 2.438685344154837953, -7.964842623401177768 ) ) ;
#920 = CARTESIAN_POINT ( 'NONE',  ( 14.92337183194729988, 29.34226448433411960, -8.527530157486177487 ) ) ;
#921 = ORIENTED_EDGE ( 'NONE', *, *, #98148, .F. ) ;
#922 = CARTESIAN_POINT ( 'NONE',  ( 5.076628168052704559, 35.17559781766745175, -8.527530157486179263 ) ) ;
#923 = CARTESIAN_POINT ( 'NONE',  ( 2.035157376598822676, 37.43868534415484106, -7.964842623401177768 ) ) ;
#924 = CARTESIAN_POINT ( 'NONE',  ( 19.84674366389459266, 43.71726448433410894, -2.638427012816827677 ) ) ;
#925 = CARTESIAN_POINT ( 'NONE',  ( 10.00000000000000000, 17.87363466993041783, -12.81628187352647608 ) ) ;
#927 = CARTESIAN_POINT ( 'NONE',  ( 0.5774900079438607392, 68.48035201082150536, 5.440088680355550821 ) ) ;
#926 = CARTESIAN_POINT ( 'NONE',  ( -0.8801773607110991993, 67.85535201082151957, -2.915334737309923874 ) ) ;
#928 = CARTESIAN_POINT ( 'NONE',  ( 10.00000000000000000, 51.81368534415484106, -10.88017736071110342 ) ) ;
#929 = CARTESIAN_POINT ( 'NONE',  ( -0.3689425029237898834, 56.17874883491396076, -10.36894250292378850 ) ) ;
#930 = EDGE_CURVE ( 'NONE', #78202, #91469, #93678, .T. ) ;
#931 = AXIS2_PLACEMENT_3D ( 'NONE', #97642, #90596, #92936 ) ;
#932 = CARTESIAN_POINT ( 'NONE',  ( 3.591859063236761518, 19.95696800326375353, 11.09922568453594849 ) ) ;
#933 = CARTESIAN_POINT ( 'NONE',  ( -9.876730923139145801, 0.5000000000000004441, -11.28938378619076843 ) ) ;
#934 = EDGE_CURVE ( 'NONE', #70902, #7776, #71189, .T. ) ;
#935 = VERTEX_POINT ( 'NONE', #12147 ) ;
#936 = CARTESIAN_POINT ( 'NONE',  ( 22.81628187352648496, 21.83196800326374643, -3.434112377981050290 ) ) ;
#937 = CARTESIAN_POINT ( 'NONE',  ( 2.035157376598824452, 23.68868534415484461, 7.964842623401179544 ) ) ;
#938 = CARTESIAN_POINT ( 'NONE',  ( 4.559911319644449179, 62.23035201082150536, -9.422509992056141925 ) ) ;
#939 = EDGE_LOOP ( 'NONE', ( #2928, #68689, #25232, #41405 ) ) ;
#940 = CARTESIAN_POINT ( 'NONE',  ( 1.472469842513823179, 5.592264484334118713, -4.923371831947296329 ) ) ;
#941 = CARTESIAN_POINT ( 'NONE',  ( 2.791683348922237240, 50.38393115100078035, -7.208316651077763204 ) ) ;
#942 = EDGE_CURVE ( 'NONE', #49230, #87437, #86679, .T. ) ;
#943 = CARTESIAN_POINT ( 'NONE',  ( 17.20831665107776587, 37.88393115100078745, 7.208316651077764980 ) ) ;
#944 = SURFACE_STYLE_USAGE ( .BOTH. , #70415 ) ;
#945 = CARTESIAN_POINT ( 'NONE',  ( 17.20831665107776587, 22.88393115100078745, 7.208316651077764980 ) ) ;
#946 = AXIS2_PLACEMENT_3D ( 'NONE', #32170, #55169, #47682 ) ;
#947 = DIRECTION ( 'NONE',  ( 0.000000000000000000, 0.000000000000000000, -1.000000000000000000 ) ) ;
#949 = CARTESIAN_POINT ( 'NONE',  ( 12.25993886608599759, 0.3640475087720986269, 8.642563219313707634 ) ) ;
#948 = CARTESIAN_POINT ( 'NONE',  ( 1.472469842513823179, 15.59226448433411960, -4.923371831947296329 ) ) ;
#950 = CARTESIAN_POINT ( 'NONE',  ( 4.691427381388422191, -2.693150427207434028, -4.000000000000000000 ) ) ;
#952 = VERTEX_POINT ( 'NONE', #4168 ) ;
#951 = CARTESIAN_POINT ( 'NONE',  ( 10.00000000000000178, 47.25893115100078745, 9.846743663894594434 ) ) ;
#953 = CARTESIAN_POINT ( 'NONE',  ( 2.863771337576527021, 0.04962896698837649528, -14.47259902956229283 ) ) ;
#954 = CARTESIAN_POINT ( 'NONE',  ( 0.6178305044545838731, 14.74863466993041783, 9.382169495545420901 ) ) ;
#955 = AXIS2_PLACEMENT_3D ( 'NONE', #88798, #94817, #26320 ) ;
#956 = CARTESIAN_POINT ( 'NONE',  ( -0.8801773607110991993, 47.85535201082150536, -2.915334737309923874 ) ) ;
#957 = CARTESIAN_POINT ( 'NONE',  ( 17.08211943468705130, 43.47041550158063927, 12.26659068614894998 ) ) ;
#958 = CARTESIAN_POINT ( 'NONE',  ( 10.00000000000000178, 2.258931151000784787, 9.846743663894594434 ) ) ;
#959 = CARTESIAN_POINT ( 'NONE',  ( -46.94000000000001194, 100.4376529975699981, 9.000000000001183054 ) ) ;
#960 = ADVANCED_FACE ( 'NONE', ( #34637 ), #97527, .T. ) ;
#961 = CARTESIAN_POINT ( 'NONE',  ( 13.79529636645031943, 50.34541550158064638, -14.16423886937409904 ) ) ;
#962 = CARTESIAN_POINT ( 'NONE',  ( 10.00000000000000000, 65.55374883491396076, -14.16423886937410082 ) ) ;
#963 = CARTESIAN_POINT ( 'NONE',  ( 10.00000000000000000, 20.55374883491396787, -14.16423886937410082 ) ) ;
#965 = CARTESIAN_POINT ( 'NONE',  ( -13.22845221182699404, 91.00000000000001421, -8.000000000000001776 ) ) ;
#964 = CARTESIAN_POINT ( 'NONE',  ( 24.16423886937410614, 29.51208216824729647, -3.795296366450302550 ) ) ;
#966 = CARTESIAN_POINT ( 'NONE',  ( -8.235571585149862983, 10.74303362898264602, 8.235571585149875418 ) ) ;
#968 = CARTESIAN_POINT ( 'NONE',  ( 5.076628168052704559, 40.17559781766745175, -8.527530157486179263 ) ) ;
#967 = CARTESIAN_POINT ( 'NONE',  ( 4.572805492043258369, -6.390838093377243290, 2.750000000000000000 ) ) ;
#969 = CARTESIAN_POINT ( 'NONE',  ( 15.44008868035555793, 26.39701867748817321, -9.422509992056140149 ) ) ;
#970 = DIRECTION ( 'NONE',  ( 0.000000000000000000, 0.000000000000000000, -1.000000000000000000 ) ) ;
#971 = CARTESIAN_POINT ( 'NONE',  ( 1.472469842513823179, 65.59226448433412315, -4.923371831947296329 ) ) ;
#972 = CARTESIAN_POINT ( 'NONE',  ( 20.00000000000000711, 88.18949240714360371, -4.994480956907769276 ) ) ;
#973 = CARTESIAN_POINT ( 'NONE',  ( 17.20831665107776587, 42.88393115100077324, 7.208316651077764980 ) ) ;
#974 = CARTESIAN_POINT ( 'NONE',  ( 0.6178305044545838731, 59.74863466993041783, 9.382169495545420901 ) ) ;
#976 = AXIS2_PLACEMENT_3D ( 'NONE', #83405, #29399, #14927 ) ;
#975 = CARTESIAN_POINT ( 'NONE',  ( 14.16423886937410082, -5.487917831752695541, -3.795296366450314096 ) ) ;
#977 = CARTESIAN_POINT ( 'NONE',  ( 1.472469842513823179, 36.42559781766745175, 4.923371831947296329 ) ) ;
#978 = CARTESIAN_POINT ( 'NONE',  ( 17.20831665107776587, 57.88393115100078745, 7.208316651077764980 ) ) ;
#979 = VECTOR ( 'NONE', #94838, 1000.000000000000000 ) ;
#980 = CARTESIAN_POINT ( 'NONE',  ( 20.36894250292379382, 33.67874883491396076, 10.36894250292379205 ) ) ;
#981 = VERTEX_POINT ( 'NONE', #79166 ) ;
#982 = CARTESIAN_POINT ( 'NONE',  ( 13.79529636645030344, 13.26208216824729824, 14.16423886937410614 ) ) ;
#983 = PRESENTATION_LAYER_ASSIGNMENT (  '', '', ( #5748 ) ) ;
#984 = CARTESIAN_POINT ( 'NONE',  ( 0.000000000000000000, 15.00000000000000000, -11.25000000000000178 ) ) ;
#986 = CARTESIAN_POINT ( 'NONE',  ( 7.154372922009559765, -0.03417435944610275333, -14.30707323420376831 ) ) ;
#985 = CARTESIAN_POINT ( 'NONE',  ( 32.06412365047463453, 14.00000000000001066, 9.500000000000000000 ) ) ;
#987 = CARTESIAN_POINT ( 'NONE',  ( 2.035157376598824452, 8.688685344154839285, 7.964842623401179544 ) ) ;
#988 = CARTESIAN_POINT ( 'NONE',  ( 21.09922568453594849, 6.206968003263753531, 6.408140936763242479 ) ) ;
#989 = CARTESIAN_POINT ( 'NONE',  ( 18.00000000000000711, 77.36170532436575797, 4.193342410628620343 ) ) ;
#990 = CARTESIAN_POINT ( 'NONE',  ( 14.92337183194729988, 4.342264484334117824, -8.527530157486177487 ) ) ;
#991 = SURFACE_STYLE_FILL_AREA ( #92941 ) ;
#992 = CARTESIAN_POINT ( 'NONE',  ( -46.52365679472261206, 102.3054413859459828, -7.234551493516248932 ) ) ;
#993 = CARTESIAN_POINT ( 'NONE',  ( 2.917880565312950480, 65.97041550158063217, -12.26659068614894821 ) ) ;
#994 = LINE ( 'NONE', #30968, #8060 ) ;
#995 = CARTESIAN_POINT ( 'NONE',  ( 12.91533473730992121, 29.52201867748817321, 10.88017736071110164 ) ) ;
#996 = CARTESIAN_POINT ( 'NONE',  ( -0.8801773607111009756, 18.06368534415484106, 1.068504757029289695E-15 ) ) ;
#997 = CARTESIAN_POINT ( 'NONE',  ( 2.791683348922237240, 60.38393115100078745, -7.208316651077763204 ) ) ;
#998 = CARTESIAN_POINT ( 'NONE',  ( 0.1532563361054082862, 51.21726448433412315, 2.638427012816831674 ) ) ;
#999 = CARTESIAN_POINT ( 'NONE',  ( -44.79861740791880464, 105.6822567946284153, -4.824280223375575716 ) ) ;
#1000 = DIRECTION ( 'NONE',  ( -0.9426414910921759871, 0.000000000000000000, -0.3338068592337775642 ) ) ;
#1001 = ORIENTED_EDGE ( 'NONE', *, *, #82418, .F. ) ;
#1002 = CARTESIAN_POINT ( 'NONE',  ( 4.559911319644449179, 33.89701867748817676, 9.422509992056141925 ) ) ;
#1003 = EDGE_CURVE ( 'NONE', #3599, #65307, #65631, .T. ) ;
#1004 = CARTESIAN_POINT ( 'NONE',  ( 13.43411237798105340, 20.58196800326374643, 12.81628187352647963 ) ) ;
#1005 = CARTESIAN_POINT ( 'NONE',  ( 19.39235739573469530, 34.87576471608600315, 6.499999999999993783 ) ) ;
#1006 = CARTESIAN_POINT ( 'NONE',  ( 10.00000000000000178, 67.25893115100079456, 9.846743663894594434 ) ) ;
#1007 = CARTESIAN_POINT ( 'NONE',  ( 0.5774900079438590739, 52.64701867748817676, -5.440088680355550821 ) ) ;
#1008 = CARTESIAN_POINT ( 'NONE',  ( 0.6178305044545838731, 24.74863466993042493, 9.382169495545420901 ) ) ;
#1010 = CARTESIAN_POINT ( 'NONE',  ( 13.16767742306216604, 0.04962884061926501472, -6.653539137814636462 ) ) ;
#1009 = CARTESIAN_POINT ( 'NONE',  ( -0.8801773607110991993, 67.85535201082151957, -2.915334737309923874 ) ) ;
#1011 = CARTESIAN_POINT ( 'NONE',  ( 0.000000000000000000, 0.000000000000000000, 0.000000000000000000 ) ) ;
#1012 = CARTESIAN_POINT ( 'NONE',  ( -1.099225684535947600, 64.54030133659709634, 6.408140936763237150 ) ) ;
#1013 = ORIENTED_EDGE ( 'NONE', *, *, #57799, .T. ) ;
#1014 = CARTESIAN_POINT ( 'NONE',  ( -0.8801773607110990882, 47.85535201082150536, -2.915334737309924318 ) ) ;
#1015 = CARTESIAN_POINT ( 'NONE',  ( -46.94000000000001194, 103.0000000000000000, 5.997726559847112782 ) ) ;
#1016 = CARTESIAN_POINT ( 'NONE',  ( 12.91533473730992121, 49.52201867748817676, 10.88017736071110164 ) ) ;
#1018 = CARTESIAN_POINT ( 'NONE',  ( 10.00000000000000178, 13.05374883491396787, 14.16423886937410082 ) ) ;
#1017 = CARTESIAN_POINT ( 'NONE',  ( 3.591859063236763294, 53.29030133659708923, -11.09922568453595026 ) ) ;
#1019 = DIRECTION ( 'NONE',  ( 0.000000000000000000, 0.000000000000000000, 1.000000000000000000 ) ) ;
#1020 = CARTESIAN_POINT ( 'NONE',  ( 10.00000000000000000, 24.75893115100078745, -9.846743663894594434 ) ) ;
#1021 = DIRECTION ( 'NONE',  ( -0.02617694830787627158, 0.000000000000000000, 0.9996573249755572599 ) ) ;
#1022 = CARTESIAN_POINT ( 'NONE',  ( 13.79529636645031943, 55.34541550158062506, -14.16423886937409904 ) ) ;
#1023 = VERTEX_POINT ( 'NONE', #50645 ) ;
#1024 = CIRCLE ( 'NONE', #98383, 15.00000000000000000 ) ;
#1025 = CARTESIAN_POINT ( 'NONE',  ( 4.559911319644449179, 3.897018677488170990, 9.422509992056141925 ) ) ;
#1026 = CARTESIAN_POINT ( 'NONE',  ( 0.5774900079438607392, 3.480352010821504027, 5.440088680355550821 ) ) ;
#1027 = LINE ( 'NONE', #92490, #16884 ) ;
#1028 = ORIENTED_EDGE ( 'NONE', *, *, #35765, .F. ) ;
#1029 = CARTESIAN_POINT ( 'NONE',  ( 20.88017736071110875, 5.772018677488170546, -2.915334737309920765 ) ) ;
#1030 = CARTESIAN_POINT ( 'NONE',  ( 10.00000000000000000, 6.813685344154838397, -10.88017736071110342 ) ) ;
#1031 = CARTESIAN_POINT ( 'NONE',  ( 1.472469842513823179, 45.59226448433412315, -4.923371831947296329 ) ) ;
#1032 = CARTESIAN_POINT ( 'NONE',  ( 6.565887622018943937, 35.16530133659708923, 12.81628187352647430 ) ) ;
#1033 = CARTESIAN_POINT ( 'NONE',  ( 19.80832241502127999, 64.75868815902069286, 6.499999999999992006 ) ) ;
#1035 = CARTESIAN_POINT ( 'NONE',  ( -4.164238869374099927, 22.01208216824730357, 3.795296366450308767 ) ) ;
#1034 = CARTESIAN_POINT ( 'NONE',  ( 18.72515096720570327, 11.07228050351031712, -6.499999999999992006 ) ) ;
#1036 = CARTESIAN_POINT ( 'NONE',  ( 12.91533473730993009, 21.60535201082150536, -10.88017736071109987 ) ) ;
#1037 = CARTESIAN_POINT ( 'NONE',  ( 24.16423886937410614, 64.30374883491396076, 8.672049930838204340E-16 ) ) ;
#1038 = CARTESIAN_POINT ( 'NONE',  ( 5.076628168052704559, 45.17559781766745175, -8.527530157486179263 ) ) ;
#1039 = CARTESIAN_POINT ( 'NONE',  ( -45.94000000000000483, 92.50000000000000000, -9.000000000000000000 ) ) ;
#1040 = CARTESIAN_POINT ( 'NONE',  ( 10.00000000000000178, 22.25893115100078745, 9.846743663894594434 ) ) ;
#1041 = DIRECTION ( 'NONE',  ( 0.000000000000000000, -1.000000000000000000, 0.000000000000000000 ) ) ;
#1042 = CARTESIAN_POINT ( 'NONE',  ( -4.923371831947302546, 30.17559781766745886, -8.527530157486173934 ) ) ;
#1043 = EDGE_LOOP ( 'NONE', ( #66084, #36581, #93814, #49851, #67190, #80121 ) ) ;
#1044 = VERTEX_POINT ( 'NONE', #73627 ) ;
#1045 = CARTESIAN_POINT ( 'NONE',  ( 18.52753015748617571, 63.09226448433412315, 4.923371831947298993 ) ) ;
#1047 = CARTESIAN_POINT ( 'NONE',  ( 17.96484262340118221, 36.18868534415484106, -7.964842623401177768 ) ) ;
#1046 = CARTESIAN_POINT ( 'NONE',  ( 10.00000000000000000, 36.81368534415484106, -10.88017736071110342 ) ) ;
#1048 = CARTESIAN_POINT ( 'NONE',  ( 21.09922568453594849, 31.20696800326375353, 6.408140936763242479 ) ) ;
#1049 = CARTESIAN_POINT ( 'NONE',  ( -4.164238869374099927, 17.01208216824730357, 3.795296366450308767 ) ) ;
#1050 = STYLED_ITEM ( 'NONE', ( #3795 ), #35208 ) ;
#1051 = EDGE_CURVE ( 'NONE', #67870, #46091, #81134, .T. ) ;
#1052 = ORIENTED_EDGE ( 'NONE', *, *, #1534, .F. ) ;
#1053 = EDGE_CURVE ( 'NONE', #87334, #57215, #41639, .T. ) ;
#1055 = CARTESIAN_POINT ( 'NONE',  ( -1.099225684535947600, 38.70696800326375353, -6.408140936763238038 ) ) ;
#1054 = AXIS2_PLACEMENT_3D ( 'NONE', #1684, #85651, #92650 ) ;
#1056 = EDGE_CURVE ( 'NONE', #28374, #28519, #71675, .T. ) ;
#1057 = EDGE_LOOP ( 'NONE', ( #46401, #67806, #92729, #95178, #5184, #32431 ) ) ;
#1058 = CARTESIAN_POINT ( 'NONE',  ( 0.1532563361054082862, 46.21726448433411605, 2.638427012816831674 ) ) ;
#1059 = CARTESIAN_POINT ( 'NONE',  ( -0.8801773607110991993, 17.85535201082150536, -2.915334737309923874 ) ) ;
#1060 = ORIENTED_EDGE ( 'NONE', *, *, #71039, .T. ) ;
#1061 = CARTESIAN_POINT ( 'NONE',  ( 0.5774900079438590739, 12.64701867748817321, -5.440088680355550821 ) ) ;
#1062 = B_SPLINE_CURVE_WITH_KNOTS ( 'NONE', 3,
 ( #33138, #63633, #11628, #71651, #19621, #50115 ),
 .UNSPECIFIED., .F., .F.,
 ( 4, 2, 4 ),
 ( 0.0002800452451301727584, 0.0006862509172429725589, 0.001092456589355772414 ),
 .UNSPECIFIED. ) ;
#1063 = ORIENTED_EDGE ( 'NONE', *, *, #45515, .F. ) ;
#1064 = CARTESIAN_POINT ( 'NONE',  ( 15.44008868035555260, 59.73035201082151247, 9.422509992056143702 ) ) ;
#1065 = CARTESIAN_POINT ( 'NONE',  ( 2.035157376598822676, 67.43868534415484817, -7.964842623401177768 ) ) ;
#1066 = CARTESIAN_POINT ( 'NONE',  ( 8.629999999999995453, 40.74999999999999289, -3.750000000000000000 ) ) ;
#1067 = CARTESIAN_POINT ( 'NONE',  ( 5.076628168052704559, 5.175597817667451750, -8.527530157486179263 ) ) ;
#1068 = CARTESIAN_POINT ( 'NONE',  ( 4.559911319644449179, 63.89701867748817676, 9.422509992056141925 ) ) ;
#1069 = CARTESIAN_POINT ( 'NONE',  ( 4.879999999999991900, 76.07179676972444327, 6.250000000000000000 ) ) ;
#1071 = CARTESIAN_POINT ( 'NONE',  ( -46.67091953292581508, 101.1773697441846736, 8.660634561519810148 ) ) ;
#1070 =( GEOMETRIC_REPRESENTATION_CONTEXT ( 3 ) GLOBAL_UNCERTAINTY_ASSIGNED_CONTEXT ( ( #63324 ) ) GLOBAL_UNIT_ASSIGNED_CONTEXT ( ( #52443, #14458, #5965 ) ) REPRESENTATION_CONTEXT ( 'NONE', 'WORKASPACE' ) );
#1073 = ORIENTED_EDGE ( 'NONE', *, *, #35562, .F. ) ;
#1072 = CARTESIAN_POINT ( 'NONE',  ( 10.00000000000000000, 4.758931151000784787, -9.846743663894594434 ) ) ;
#1074 = AXIS2_PLACEMENT_3D ( 'NONE', #31900, #47402, #86886 ) ;
#1075 = VECTOR ( 'NONE', #35109, 1000.000000000000000 ) ;
#1076 = CARTESIAN_POINT ( 'NONE',  ( 7.361572987183170547, 47.05059781766745175, 9.846743663894590881 ) ) ;
#1077 = EDGE_LOOP ( 'NONE', ( #4944, #29200, #60589, #70264, #59437, #51331 ) ) ;
#1078 = VERTEX_POINT ( 'NONE', #64147 ) ;
#1079 = CARTESIAN_POINT ( 'NONE',  ( 5.500000000000000000, 11.50000000000000000, -6.000000000000000000 ) ) ;
#1080 = DIRECTION ( 'NONE',  ( 1.000000000000000000, 0.000000000000000000, 0.000000000000000000 ) ) ;
#1081 = LINE ( 'NONE', #65482, #88658 ) ;
#1082 = EDGE_CURVE ( 'NONE', #46208, #94458, #57424, .T. ) ;
#1083 = CARTESIAN_POINT ( 'NONE',  ( 13.79529636645030344, 8.262082168247300018, 14.16423886937410614 ) ) ;
#1084 = CARTESIAN_POINT ( 'NONE',  ( -2.266590686148945544, 21.38708216824730357, -7.082119434687050408 ) ) ;
#1085 = DIRECTION ( 'NONE',  ( 0.000000000000000000, 0.000000000000000000, 1.000000000000000000 ) ) ;
#1086 = DIRECTION ( 'NONE',  ( 1.000000000000000000, 0.000000000000000000, 0.000000000000000000 ) ) ;
#1087 = CARTESIAN_POINT ( 'NONE',  ( -0.8801773607110991993, 27.85535201082150181, -2.915334737309923874 ) ) ;
#1088 =( NAMED_UNIT ( * ) PLANE_ANGLE_UNIT ( ) SI_UNIT ( $, .RADIAN. ) );
#1089 = ORIENTED_EDGE ( 'NONE', *, *, #45048, .F. ) ;
#1090 = CARTESIAN_POINT ( 'NONE',  ( 1.472469842513823179, 6.425597817667451750, 4.923371831947296329 ) ) ;
#1091 = STYLED_ITEM ( 'NONE', ( #64075 ), #55484 ) ;
#1092 = CARTESIAN_POINT ( 'NONE',  ( 3.591859063236763294, 28.29030133659708568, -11.09922568453595026 ) ) ;
#1093 = CARTESIAN_POINT ( 'NONE',  ( 19.84674366389459266, 23.71726448433412315, -2.638427012816827677 ) ) ;
#1094 = CARTESIAN_POINT ( 'NONE',  ( 7.618485323809272458, 15.00000000000000888, -12.48587314215760458 ) ) ;
#1095 = CARTESIAN_POINT ( 'NONE',  ( 6.565887622018943937, 10.16530133659708746, 12.81628187352647430 ) ) ;
#1096 = DIRECTION ( 'NONE',  ( 0.000000000000000000, 0.000000000000000000, 1.000000000000000000 ) ) ;
#1097 = CARTESIAN_POINT ( 'NONE',  ( 14.92337183194729633, 2.675597817667451750, 8.527530157486181039 ) ) ;
#1098 = ORIENTED_EDGE ( 'NONE', *, *, #58474, .T. ) ;
#1099 = EDGE_LOOP ( 'NONE', ( #77070, #42549, #66446, #65909, #31655, #89303 ) ) ;
#1100 = CARTESIAN_POINT ( 'NONE',  ( 7.084665262690076126, 17.02201867748817676, -10.88017736071110164 ) ) ;
#1101 = CARTESIAN_POINT ( 'NONE',  ( -0.3689425029237898834, 36.17874883491396787, -10.36894250292378850 ) ) ;
#1102 = CARTESIAN_POINT ( 'NONE',  ( 17.20831665107776587, 37.88393115100078745, 7.208316651077764980 ) ) ;
#1103 = CARTESIAN_POINT ( 'NONE',  ( 0.1532563361054082862, 1.217264484334117824, 2.638427012816831674 ) ) ;
#1105 = LINE ( 'NONE', #77561, #75163 ) ;
#1104 = CARTESIAN_POINT ( 'NONE',  ( 10.00000000000000178, 50.37363466993042493, 12.81628187352647608 ) ) ;
#1106 = CARTESIAN_POINT ( 'NONE',  ( -0.8801773607111008646, 23.27201867748817676, 2.915334737309923430 ) ) ;
#1107 = CARTESIAN_POINT ( 'NONE',  ( -0.000000000000000000, 99.99999999999998579, -8.000000000000000000 ) ) ;
#1108 = CARTESIAN_POINT ( 'NONE',  ( -1.099225684535947600, 18.70696800326375353, -6.408140936763238038 ) ) ;
#1109 = CARTESIAN_POINT ( 'NONE',  ( 22.81628187352648496, 6.831968003263753531, -3.434112377981050290 ) ) ;
#1110 = CARTESIAN_POINT ( 'NONE',  ( 19.84674366389459266, 38.30059781766745175, 2.638427012816836559 ) ) ;
#1111 = CARTESIAN_POINT ( 'NONE',  ( 9.422509992056141925, 0.1470186774881754310, 5.440088680355547268 ) ) ;
#1112 = CARTESIAN_POINT ( 'NONE',  ( -1.099225684535947600, 44.54030133659708923, 6.408140936763237150 ) ) ;
#1113 =( BOUNDED_SURFACE ( )  B_SPLINE_SURFACE ( 3, 2, ( 
 ( #32802, #48792, #77812 ),
 ( #94787, #11290, #63297 ),
 ( #64765, #79787, #93807 ),
 ( #79300, #24835, #25337 ),
 ( #95277, #55821, #86315 ),
 ( #87283, #17819, #26287 ),
 ( #39830, #48301, #56788 ),
 ( #26780, #57278, #41327 ),
 ( #70336, #1852, #32310 ),
 ( #62815, #93313, #49774 ),
 ( #35263, #97782, #89746 ),
 ( #50260, #96285, #20276 ),
 ( #5774, #66252, #73265 ),
 ( #87772, #58247, #13760 ),
 ( #27764, #20772, #43262 ),
 ( #35763, #67258, #80281 ),
 ( #28755, #65760, #88766 ),
 ( #44247, #58757, #50773 ) ),
 .UNSPECIFIED., .F., .F., .T. ) 
 B_SPLINE_SURFACE_WITH_KNOTS ( ( 4, 2, 2, 2, 2, 2, 2, 2, 4 ),
 ( 3, 3 ),
 ( 0.000000000000000000, 0.001371970262341175176, 0.002743940524682350352, 0.004115910787023525745, 0.005487881049364700704, 0.006859851311705876531, 0.008231821574047051490, 0.009603791836388226449, 0.01097576209872940141 ),
 ( 0.000000000000000000, 1.000000000000000000 ),
 .UNSPECIFIED. ) 
 GEOMETRIC_REPRESENTATION_ITEM ( )  RATIONAL_B_SPLINE_SURFACE ( (
 ( 1.000000000000000000, 0.7071067811865475727, 1.000000000000000000),
 ( 1.000000000000000000, 0.7072982590433614103, 1.000000000000000000),
 ( 1.000000000000000000, 0.7113498972295660971, 1.000000000000000000),
 ( 1.000000000000000000, 0.7257703676791772418, 1.000000000000000000),
 ( 1.000000000000000000, 0.7362840324263598690, 1.000000000000000000),
 ( 1.000000000000000000, 0.7606319170830569965, 1.000000000000000000),
 ( 1.000000000000000000, 0.7745485803766045674, 1.000000000000000000),
 ( 1.000000000000000000, 0.8036690257212466548, 1.000000000000000000),
 ( 1.000000000000000000, 0.8185245023543151754, 1.000000000000000000),
 ( 1.000000000000000000, 0.8475516512717119477, 1.000000000000000000),
 ( 1.000000000000000000, 0.8617420886046736062, 1.000000000000000000),
 ( 1.000000000000000000, 0.8886174597629885596, 1.000000000000000000),
 ( 1.000000000000000000, 0.9010211234293969973, 1.000000000000000000),
 ( 1.000000000000000000, 0.9233336449993967410, 1.000000000000000000),
 ( 1.000000000000000000, 0.9332564696565026630, 1.000000000000000000),
 ( 1.000000000000000000, 0.9500370447730048795, 1.000000000000000000),
 ( 1.000000000000000000, 0.9567390024731449172, 1.000000000000000000),
 ( 1.000000000000000000, 0.9611621933234241189, 1.000000000000000000) ) ) 
 REPRESENTATION_ITEM ( '' )  SURFACE ( )  );
#1114 = CARTESIAN_POINT ( 'NONE',  ( 4.862001128006775197, 15.00000000000000000, -13.66056166602457367 ) ) ;
#1116 = DIRECTION ( 'NONE',  ( 0.000000000000000000, 1.000000000000000000, 0.000000000000000000 ) ) ;
#1115 = CARTESIAN_POINT ( 'NONE',  ( 10.00000000000000178, 59.31368534415484106, 10.88017736071110342 ) ) ;
#1117 = DIRECTION ( 'NONE',  ( 0.000000000000000000, 0.000000000000000000, -1.000000000000000000 ) ) ;
#1118 = SURFACE_SIDE_STYLE ('',( #69107 ) ) ;
#1119 =( BOUNDED_SURFACE ( )  B_SPLINE_SURFACE ( 3, 2, ( 
 ( #95548, #95038, #27036 ),
 ( #4558, #57535, #35527 ),
 ( #64531, #96046, #35022 ),
 ( #88032, #19544, #50040 ),
 ( #80543, #49535, #58021 ),
 ( #20031, #57043, #65523 ),
 ( #50533, #81028, #56562 ),
 ( #73515, #19057, #66021 ) ),
 .UNSPECIFIED., .F., .F., .F. ) 
 B_SPLINE_SURFACE_WITH_KNOTS ( ( 4, 2, 2, 4 ),
 ( 3, 3 ),
 ( 0.000000000000000000, 0.0004516266542298884193, 0.0009032533084597768385, 0.001806506616919553677 ),
 ( 0.000000000000000000, 1.000000000000000000 ),
 .UNSPECIFIED. ) 
 GEOMETRIC_REPRESENTATION_ITEM ( )  RATIONAL_B_SPLINE_SURFACE ( (
 ( 1.000000000000000000, 0.7071067811865523467, 1.000000000000000000),
 ( 1.000000000000000000, 0.7557133596825000854, 1.000000000000000000),
 ( 1.000000000000000000, 0.7976722695486582193, 1.000000000000000000),
 ( 1.000000000000000000, 0.8702934545465945693, 1.000000000000000000),
 ( 1.000000000000000000, 0.9009816261290091166, 1.000000000000000000),
 ( 1.000000000000000000, 0.9749059260395099846, 1.000000000000000000),
 ( 1.000000000000000000, 1.000014990204702858, 1.000000000000000000),
 ( 1.000000000000000000, 1.000000000000000000, 1.000000000000000000) ) ) 
 REPRESENTATION_ITEM ( '' )  SURFACE ( )  );
#1120 = CARTESIAN_POINT ( 'NONE',  ( 19.42250999205614193, 60.14701867748817676, 5.440088680355555262 ) ) ;
#1121 = CARTESIAN_POINT ( 'NONE',  ( 15.44008868035555260, 59.73035201082151247, 9.422509992056143702 ) ) ;
#1122 = CARTESIAN_POINT ( 'NONE',  ( 8.209432707284918251, 14.49999999999999112, -12.55409154915490255 ) ) ;
#1123 = FACE_OUTER_BOUND ( 'NONE', #83548, .T. ) ;
#1124 = CARTESIAN_POINT ( 'NONE',  ( 20.88017736071110875, 5.772018677488170546, -2.915334737309920765 ) ) ;
#1125 = CARTESIAN_POINT ( 'NONE',  ( 19.84674366389459266, 53.30059781766744464, 2.638427012816836559 ) ) ;
#1127 = DIRECTION ( 'NONE',  ( -0.000000000000000000, -0.000000000000000000, -1.000000000000000000 ) ) ;
#1126 = CARTESIAN_POINT ( 'NONE',  ( 10.00000000000000000, 21.81368534415484106, -10.88017736071110342 ) ) ;
#1128 = CARTESIAN_POINT ( 'NONE',  ( 10.00000000000000178, 30.37363466993042138, 12.81628187352647608 ) ) ;
#1129 = ORIENTED_EDGE ( 'NONE', *, *, #54416, .T. ) ;
#1130 = CARTESIAN_POINT ( 'NONE',  ( -0.8801773607111009756, 43.06368534415484106, 1.068504757029289695E-15 ) ) ;
#1132 = CARTESIAN_POINT ( 'NONE',  ( -12.58781651029209492, -3.178914651045387989E-15, 7.446837378630629445 ) ) ;
#1131 = CARTESIAN_POINT ( 'NONE',  ( 10.00000000000000178, 5.373634669930420493, 12.81628187352647608 ) ) ;
#1133 = CARTESIAN_POINT ( 'NONE',  ( 10.00000000000000178, 9.313685344154839285, 10.88017736071110342 ) ) ;
#1134 = CARTESIAN_POINT ( 'NONE',  ( -0.8801773607110991993, 42.85535201082150536, -2.915334737309923874 ) ) ;
#1135 = CARTESIAN_POINT ( 'NONE',  ( -0.3689425029237898834, 41.17874883491397497, -10.36894250292378850 ) ) ;
#1136 = CARTESIAN_POINT ( 'NONE',  ( 10.00000000000000178, 22.25893115100078745, 9.846743663894594434 ) ) ;
#1137 = CARTESIAN_POINT ( 'NONE',  ( 10.00000000000000178, 64.31368534415483396, 10.88017736071110342 ) ) ;
#1138 = CARTESIAN_POINT ( 'NONE',  ( 0.000000000000000000, 0.000000000000000000, 0.000000000000000000 ) ) ;
#1139 = CARTESIAN_POINT ( 'NONE',  ( 24.16423886937409904, 9.095415501580633943, 3.795296366450317205 ) ) ;
#1140 = VECTOR ( 'NONE', #36904, 1000.000000000000000 ) ;
#1141 = EDGE_CURVE ( 'NONE', #84500, #74647, #63450, .T. ) ;
#1142 = VECTOR ( 'NONE', #53062, 1000.000000000000000 ) ;
#1143 = CARTESIAN_POINT ( 'NONE',  ( 5.806616290881413178, -3.171291354520099286E-15, -13.42355087257362278 ) ) ;
#1144 = CARTESIAN_POINT ( 'NONE',  ( 1.472469842513823179, 55.59226448433412315, -4.923371831947296329 ) ) ;
#1145 = AXIS2_PLACEMENT_3D ( 'NONE', #11568, #56586, #78594 ) ;
#1146 = VERTEX_POINT ( 'NONE', #6136 ) ;
#1147 = CARTESIAN_POINT ( 'NONE',  ( -0.3689425029237898834, 36.17874883491396787, -10.36894250292378850 ) ) ;
#1149 = AXIS2_PLACEMENT_3D ( 'NONE', #2580, #34009, #40556 ) ;
#1148 = CARTESIAN_POINT ( 'NONE',  ( 20.36894250292379738, 34.92874883491396076, -10.36894250292379027 ) ) ;
#1150 = CARTESIAN_POINT ( 'NONE',  ( 19.84674366389459266, 3.300597817667451750, 2.638427012816836559 ) ) ;
#1151 = CARTESIAN_POINT ( 'NONE',  ( 19.38216949554541557, 7.248634669930421381, -9.382169495545420901 ) ) ;
#1152 = CARTESIAN_POINT ( 'NONE',  ( 10.00000000000000178, 57.25893115100078745, 9.846743663894594434 ) ) ;
#1153 = CARTESIAN_POINT ( 'NONE',  ( -8.218805110796523650, -9.361916056598095892, 4.000000000000000000 ) ) ;
#1155 = CARTESIAN_POINT ( 'NONE',  ( 22.81628187352648496, 16.83196800326374998, -3.434112377981050290 ) ) ;
#1154 = CARTESIAN_POINT ( 'NONE',  ( 19.42250999205614548, 65.98035201082151957, -5.440088680355545492 ) ) ;
#1156 = CARTESIAN_POINT ( 'NONE',  ( -4.164238869374099039, 31.80374883491396432, 8.674139862899312516E-16 ) ) ;
#1157 = CARTESIAN_POINT ( 'NONE',  ( -0.8801773607110991993, 32.85535201082151247, -2.915334737309923874 ) ) ;
#1158 = CARTESIAN_POINT ( 'NONE',  ( 15.44008868035555793, 26.39701867748817321, -9.422509992056140149 ) ) ;
#1159 = DIRECTION ( 'NONE',  ( -0.7604059656000340395, 0.000000000000000000, 0.6494480483301799945 ) ) ;
#1160 = CARTESIAN_POINT ( 'NONE',  ( 20.88017736071110519, 55.56368534415484817, 2.639326808657452039E-16 ) ) ;
#1161 = CARTESIAN_POINT ( 'NONE',  ( 3.469446951953614189E-15, -12.74106884899921255, 9.846743663894594434 ) ) ;
#1162 = VERTEX_POINT ( 'NONE', #38126 ) ;
#1163 = FACE_OUTER_BOUND ( 'NONE', #27124, .T. ) ;
#1164 = EDGE_LOOP ( 'NONE', ( #40551, #53847, #17244, #68763 ) ) ;
#1165 = AXIS2_PLACEMENT_3D ( 'NONE', #34895, #57889, #50892 ) ;
#1167 = EDGE_CURVE ( 'NONE', #65699, #33104, #6078, .T. ) ;
#1166 = FACE_OUTER_BOUND ( 'NONE', #61543, .T. ) ;
#1168 = VERTEX_POINT ( 'NONE', #82619 ) ;
#1170 = CARTESIAN_POINT ( 'NONE',  ( 2.035157376598824452, 3.688685344154837953, 7.964842623401179544 ) ) ;
#1169 = CARTESIAN_POINT ( 'NONE',  ( 13.79529636645031943, 60.34541550158063927, -14.16423886937409904 ) ) ;
#1172 = CARTESIAN_POINT ( 'NONE',  ( 1.472469842513823179, 66.42559781766745175, 4.923371831947296329 ) ) ;
#1171 = CARTESIAN_POINT ( 'NONE',  ( 14.92337183194729988, 39.34226448433412315, -8.527530157486177487 ) ) ;
#1173 = CYLINDRICAL_SURFACE ( 'NONE', #94987, 0.2500000000000002220 ) ;
#1174 = CARTESIAN_POINT ( 'NONE',  ( 20.10493008474205823, 49.71697413083879269, 6.336235997365754713 ) ) ;
#1175 = ADVANCED_FACE ( 'NONE', ( #75612 ), #52125, .F. ) ;
#1176 = B_SPLINE_CURVE_WITH_KNOTS ( 'NONE', 3,
 ( #51662, #22649, #81158, #20665, #74645, #43162 ),
 .UNSPECIFIED., .F., .F.,
 ( 4, 2, 4 ),
 ( 7.822990134193277425E-18, 0.0002626113303185972870, 0.0005252226606371867678 ),
 .UNSPECIFIED. ) ;
#1177 = CARTESIAN_POINT ( 'NONE',  ( 3.591859063236761518, 9.956968003263753531, 11.09922568453594849 ) ) ;
#1178 = ADVANCED_FACE ( 'NONE', ( #20644 ), #36125, .F. ) ;
#1179 = VERTEX_POINT ( 'NONE', #14643 ) ;
#1180 = CARTESIAN_POINT ( 'NONE',  ( 2.917880565312948704, 42.63708216824729647, 12.26659068614894643 ) ) ;
#1181 = CARTESIAN_POINT ( 'NONE',  ( 13.79529636645031943, 45.34541550158062506, -14.16423886937409904 ) ) ;
#1182 = EDGE_LOOP ( 'NONE', ( #21964, #53207, #68054, #84302 ) ) ;
#1183 = CARTESIAN_POINT ( 'NONE',  ( 7.084665262690076126, 22.02201867748817321, -10.88017736071110164 ) ) ;
#1184 = CARTESIAN_POINT ( 'NONE',  ( 19.38216949554541202, 55.99863466993041072, 9.382169495545424454 ) ) ;
#1185 = CARTESIAN_POINT ( 'NONE',  ( 15.44008868035555793, 26.39701867748817321, -9.422509992056140149 ) ) ;
#1186 = CARTESIAN_POINT ( 'NONE',  ( 19.84674366389459621, 53.50893115100078745, 7.409399052514197653E-17 ) ) ;
#1187 = CARTESIAN_POINT ( 'NONE',  ( 4.559911319644449179, 38.89701867748817676, 9.422509992056141925 ) ) ;
#1188 = CARTESIAN_POINT ( 'NONE',  ( -0.3289641300568005855, 65.10497603579418069, 5.963430220938281678 ) ) ;
#1189 = CARTESIAN_POINT ( 'NONE',  ( 19.84674366389459266, 58.71726448433411605, -2.638427012816827677 ) ) ;
#1190 = DIRECTION ( 'NONE',  ( -1.257402221000611116E-16, 1.000000000000000000, 0.000000000000000000 ) ) ;
#1191 = CARTESIAN_POINT ( 'NONE',  ( 2.035157376598822676, 27.43868534415483396, -7.964842623401177768 ) ) ;
#1194 = VERTEX_POINT ( 'NONE', #53106 ) ;
#1193 = VECTOR ( 'NONE', #97289, 1000.000000000000000 ) ;
#1192 = FACE_OUTER_BOUND ( 'NONE', #20968, .T. ) ;
#1195 = CARTESIAN_POINT ( 'NONE',  ( 9.065164099344512394, 14.49999999999999112, 11.95084933600776722 ) ) ;
#1196 = CARTESIAN_POINT ( 'NONE',  ( 5.076628168052704559, 0.1755978176674514724, -8.527530157486179263 ) ) ;
#1197 = FACE_OUTER_BOUND ( 'NONE', #80893, .T. ) ;
#1198 = ORIENTED_EDGE ( 'NONE', *, *, #54099, .T. ) ;
#1199 = EDGE_CURVE ( 'NONE', #67320, #77856, #28630, .T. ) ;
#1200 = CIRCLE ( 'NONE', #26713, 0.5000000000000004441 ) ;
#1201 = CARTESIAN_POINT ( 'NONE',  ( 8.955817848695199146, -3.107653060320455296, 3.750000000000000000 ) ) ;
#1202 = CARTESIAN_POINT ( 'NONE',  ( 0.1532563361054100626, 25.80059781766744820, -2.638427012816831230 ) ) ;
#1203 = CARTESIAN_POINT ( 'NONE',  ( 20.15039907845753575, 47.62777174578613426, -6.262539305110073506 ) ) ;
#1204 = CARTESIAN_POINT ( 'NONE',  ( -2.816281873526473856, 49.33196800326374643, 3.434112377981055619 ) ) ;
#1205 = EDGE_CURVE ( 'NONE', #2423, #23291, #59166, .T. ) ;
#1206 = CARTESIAN_POINT ( 'NONE',  ( -14.24131928502211863, 15.00000000000000000, 0.4973178280104966764 ) ) ;
#1207 = VECTOR ( 'NONE', #86265, 1000.000000000000000 ) ;
#1208 = VERTEX_POINT ( 'NONE', #30098 ) ;
#1209 = FACE_BOUND ( 'NONE', #56829, .T. ) ;
#1210 = FACE_OUTER_BOUND ( 'NONE', #79066, .T. ) ;
#1211 = CARTESIAN_POINT ( 'NONE',  ( 7.361572987183170547, 57.05059781766744464, 9.846743663894590881 ) ) ;
#1212 = CARTESIAN_POINT ( 'NONE',  ( -0.3689425029237881626, 52.42874883491396076, 10.36894250292379027 ) ) ;
#1213 = CARTESIAN_POINT ( 'NONE',  ( 12.63842701281683922, 64.55059781766745175, -9.846743663894590881 ) ) ;
#1214 = CARTESIAN_POINT ( 'NONE',  ( 19.80448550324509682, 41.82703681773342907, 6.500000000002703615 ) ) ;
#1215 = CARTESIAN_POINT ( 'NONE',  ( 0.1532563361054082862, 16.21726448433411960, 2.638427012816831674 ) ) ;
#1216 = CARTESIAN_POINT ( 'NONE',  ( -1.099225684535947600, 48.70696800326375353, -6.408140936763238038 ) ) ;
#1217 = CARTESIAN_POINT ( 'NONE',  ( 1.472469842513823179, 55.59226448433412315, -4.923371831947296329 ) ) ;
#1218 = CARTESIAN_POINT ( 'NONE',  ( 2.035157376598822676, 57.43868534415484106, -7.964842623401177768 ) ) ;
#1219 = VECTOR ( 'NONE', #42137, 1000.000000000000114 ) ;
#1220 = CARTESIAN_POINT ( 'NONE',  ( 10.00000000000000000, 49.75893115100078745, -9.846743663894594434 ) ) ;
#1221 = CIRCLE ( 'NONE', #85851, 2.500000000000002220 ) ;
#1222 = CARTESIAN_POINT ( 'NONE',  ( 4.441302488725088260, -2.692589364072287772, -2.750000000000000444 ) ) ;
#1223 = CARTESIAN_POINT ( 'NONE',  ( 7.084665262690076126, 54.10535201082151247, 10.88017736071109987 ) ) ;
#1224 = ORIENTED_EDGE ( 'NONE', *, *, #61317, .F. ) ;
#1225 = CARTESIAN_POINT ( 'NONE',  ( -8.375939845167600595, -0.03417435944610275333, -11.52849216984310310 ) ) ;
#1226 = CARTESIAN_POINT ( 'NONE',  ( 20.88017736071110164, 35.35535201082150536, 2.915334737309930979 ) ) ;
#1228 = CARTESIAN_POINT ( 'NONE',  ( 19.42250999205614548, 60.98035201082151247, -5.440088680355545492 ) ) ;
#1227 = CARTESIAN_POINT ( 'NONE',  ( 0.6178305044545838731, 9.748634669930416052, 9.382169495545420901 ) ) ;
#1229 = DIRECTION ( 'NONE',  ( 1.776356839400250780E-14, 0.000000000000000000, 1.000000000000000000 ) ) ;
#1230 = CARTESIAN_POINT ( 'NONE',  ( -7.684764310694971456, 0.5000000000000004441, 12.88194075009929840 ) ) ;
#1231 = CARTESIAN_POINT ( 'NONE',  ( 3.195792623639528873, 6.203790035174478135, -11.92686044187656513 ) ) ;
#1233 = CARTESIAN_POINT ( 'NONE',  ( -0.1503990784575277295, 54.24884699246889852, -6.262539305110077947 ) ) ;
#1232 = CARTESIAN_POINT ( 'NONE',  ( 2.035157376598822676, 42.43868534415483396, -7.964842623401177768 ) ) ;
#1234 = CARTESIAN_POINT ( 'NONE',  ( 7.361572987183170547, 42.05059781766745886, 9.846743663894590881 ) ) ;
#1235 = CARTESIAN_POINT ( 'NONE',  ( 7.361572987183169658, 4.967264484334119601, -9.846743663894592657 ) ) ;
#1236 = CARTESIAN_POINT ( 'NONE',  ( -10.36894250292378317, 32.42874883491396076, 10.36894250292379560 ) ) ;
#1237 = CARTESIAN_POINT ( 'NONE',  ( 3.591859063236763294, 13.29030133659708746, -11.09922568453595026 ) ) ;
#1238 = CARTESIAN_POINT ( 'NONE',  ( 0.5774900079438590739, 7.647018677488171434, -5.440088680355550821 ) ) ;
#1239 = DIRECTION ( 'NONE',  ( -1.000000000000000000, 0.000000000000000000, -0.000000000000000000 ) ) ;
#1240 = CARTESIAN_POINT ( 'NONE',  ( -4.164238869374098151, 26.59541550158063217, -3.795296366450310543 ) ) ;
#1241 = CARTESIAN_POINT ( 'NONE',  ( -2.266590686148945544, 66.38708216824730357, -7.082119434687050408 ) ) ;
#1242 = CARTESIAN_POINT ( 'NONE',  ( 2.791683348922237240, 35.38393115100079456, -7.208316651077763204 ) ) ;
#1243 = CARTESIAN_POINT ( 'NONE',  ( 10.00000000000000000, 19.75893115100078390, -9.846743663894594434 ) ) ;
#1244 = CARTESIAN_POINT ( 'NONE',  ( 0.5774900079438607392, 18.48035201082150536, 5.440088680355550821 ) ) ;
#1245 = ORIENTED_EDGE ( 'NONE', *, *, #9371, .T. ) ;
#1246 = CARTESIAN_POINT ( 'NONE',  ( 14.92337183194729633, 42.67559781766745886, 8.527530157486181039 ) ) ;
#1247 = CARTESIAN_POINT ( 'NONE',  ( 19.42250999205614548, 30.98035201082150536, -5.440088680355545492 ) ) ;
#1248 = CARTESIAN_POINT ( 'NONE',  ( 5.076628168052703671, 66.84226448433412315, 8.527530157486179263 ) ) ;
#1250 = DIRECTION ( 'NONE',  ( 0.000000000000000000, 0.000000000000000000, 1.000000000000000000 ) ) ;
#1249 = CARTESIAN_POINT ( 'NONE',  ( 17.08211943468705130, 13.47041550158063572, 12.26659068614894998 ) ) ;
#1251 = CARTESIAN_POINT ( 'NONE',  ( 0.000000000000000000, 15.00000000000000000, 0.000000000000000000 ) ) ;
#1252 = UNCERTAINTY_MEASURE_WITH_UNIT (LENGTH_MEASURE( 1.000000000000000082E-05 ), #79189, 'distance_accuracy_value', 'NONE');
#1253 = CARTESIAN_POINT ( 'NONE',  ( 2.791683348922237240, 5.383931151000785675, -7.208316651077763204 ) ) ;
#1254 = CARTESIAN_POINT ( 'NONE',  ( 3.591859063236763294, 38.29030133659708923, -11.09922568453595026 ) ) ;
#1255 = CARTESIAN_POINT ( 'NONE',  ( 0.1532563361054100626, 60.80059781766744464, -2.638427012816831230 ) ) ;
#1256 = ORIENTED_EDGE ( 'NONE', *, *, #69290, .F. ) ;
#1257 = CARTESIAN_POINT ( 'NONE',  ( 19.84674366389459266, 18.71726448433411960, -2.638427012816827677 ) ) ;
#1258 = FACE_OUTER_BOUND ( 'NONE', #92860, .T. ) ;
#1259 = CARTESIAN_POINT ( 'NONE',  ( 17.08211943468705840, 50.13708216824730357, -12.26659068614894466 ) ) ;
#1260 = CARTESIAN_POINT ( 'NONE',  ( 12.91533473730992121, 49.52201867748817676, 10.88017736071110164 ) ) ;
#1261 = CARTESIAN_POINT ( 'NONE',  ( 2.917880565312948704, 2.637082168247300906, 12.26659068614894643 ) ) ;
#1262 = AXIS2_PLACEMENT_3D ( 'NONE', #21741, #97750, #29215 ) ;
#1263 = CARTESIAN_POINT ( 'NONE',  ( 19.42250999205614548, 60.98035201082151247, -5.440088680355545492 ) ) ;
#1264 = CARTESIAN_POINT ( 'NONE',  ( 10.00000000000000000, 39.75893115100078745, -9.846743663894594434 ) ) ;
#1265 = CARTESIAN_POINT ( 'NONE',  ( 10.00000000000000178, 19.31368534415484106, 10.88017736071110342 ) ) ;
#1266 = CARTESIAN_POINT ( 'NONE',  ( 17.39651004071841101, 37.93575266056827644, 6.500000000000005329 ) ) ;
#1267 = CARTESIAN_POINT ( 'NONE',  ( 1.472469842513823179, 45.59226448433412315, -4.923371831947296329 ) ) ;
#1268 = EDGE_CURVE ( 'NONE', #62689, #78249, #21639, .T. ) ;
#1269 = CARTESIAN_POINT ( 'NONE',  ( 7.084665262690076126, 54.10535201082151247, 10.88017736071109987 ) ) ;
#1270 = ORIENTED_EDGE ( 'NONE', *, *, #68403, .F. ) ;
#1271 = CARTESIAN_POINT ( 'NONE',  ( -7.750000000000000000, 40.99999999999999289, 4.000000000000000000 ) ) ;
#1272 = UNCERTAINTY_MEASURE_WITH_UNIT (LENGTH_MEASURE( 1.000000000000000082E-05 ), #83156, 'distance_accuracy_value', 'NONE');
#1273 = VECTOR ( 'NONE', #52048, 1000.000000000000114 ) ;
#1274 = ORIENTED_EDGE ( 'NONE', *, *, #47851, .F. ) ;
#1275 = ORIENTED_EDGE ( 'NONE', *, *, #42360, .T. ) ;
#1276 = DIRECTION ( 'NONE',  ( 0.000000000000000000, 1.000000000000000000, 0.000000000000000000 ) ) ;
#1277 = CARTESIAN_POINT ( 'NONE',  ( 13.79529636645030344, 3.262082168247301350, 14.16423886937410614 ) ) ;
#1278 = CARTESIAN_POINT ( 'NONE',  ( 12.63842701281683922, 44.55059781766745175, -9.846743663894590881 ) ) ;
#1279 = CARTESIAN_POINT ( 'NONE',  ( 10.00000000000000178, 22.25893115100078745, 9.846743663894594434 ) ) ;
#1280 = CARTESIAN_POINT ( 'NONE',  ( -1.099225684535947600, 53.70696800326376064, -6.408140936763238038 ) ) ;
#1282 = CARTESIAN_POINT ( 'NONE',  ( 10.00000000000000000, 54.75893115100078745, -9.846743663894594434 ) ) ;
#1281 = CARTESIAN_POINT ( 'NONE',  ( 15.44008868035555793, 16.39701867748817321, -9.422509992056140149 ) ) ;
#1283 = DIRECTION ( 'NONE',  ( 0.000000000000000000, 0.000000000000000000, -1.000000000000000000 ) ) ;
#1284 = CARTESIAN_POINT ( 'NONE',  ( 20.36894250292379738, 44.92874883491396787, -10.36894250292379027 ) ) ;
#1285 = CARTESIAN_POINT ( 'NONE',  ( 17.08211943468705130, 53.47041550158063217, 12.26659068614894998 ) ) ;
#1286 = CARTESIAN_POINT ( 'NONE',  ( 14.92337183194729633, 57.67559781766745886, 8.527530157486181039 ) ) ;
#1287 = CARTESIAN_POINT ( 'NONE',  ( 17.87804611792045151, 78.26090218833458323, 4.039389165979513585 ) ) ;
#1288 = CARTESIAN_POINT ( 'NONE',  ( 0.5774900079438607392, 53.48035201082151247, 5.440088680355550821 ) ) ;
#1289 = CARTESIAN_POINT ( 'NONE',  ( 7.361572987183169658, 19.96726448433411960, -9.846743663894592657 ) ) ;
#1290 =( GEOMETRIC_REPRESENTATION_CONTEXT ( 3 ) GLOBAL_UNCERTAINTY_ASSIGNED_CONTEXT ( ( #20152 ) ) GLOBAL_UNIT_ASSIGNED_CONTEXT ( ( #19702, #95707, #27190 ) ) REPRESENTATION_CONTEXT ( 'NONE', 'WORKASPACE' ) );
#1291 = CARTESIAN_POINT ( 'NONE',  ( -5.811454672306898495, -36.11427488548738296, 3.750000000000806022 ) ) ;
#1292 = ORIENTED_EDGE ( 'NONE', *, *, #36512, .F. ) ;
#1293 = CARTESIAN_POINT ( 'NONE',  ( -14.47650479471830387, 14.49999999999999112, 3.928206833721953561 ) ) ;
#1294 = ORIENTED_EDGE ( 'NONE', *, *, #27831, .T. ) ;
#1295 = AXIS2_PLACEMENT_3D ( 'NONE', #58868, #65872, #97386 ) ;
#1296 = CARTESIAN_POINT ( 'NONE',  ( 2.791683348922237240, 10.38393115100078390, -7.208316651077763204 ) ) ;
#1297 = ORIENTED_EDGE ( 'NONE', *, *, #81961, .T. ) ;
#1298 = CARTESIAN_POINT ( 'NONE',  ( -0.3689425029237898834, 16.17874883491396076, -10.36894250292378850 ) ) ;
#1299 = CARTESIAN_POINT ( 'NONE',  ( 2.791683348922237240, 15.38393115100078212, -7.208316651077763204 ) ) ;
#1300 = CARTESIAN_POINT ( 'NONE',  ( 2.035157376598824452, 43.68868534415484106, 7.964842623401179544 ) ) ;
#1301 = AXIS2_PLACEMENT_3D ( 'NONE', #24699, #5022, #40184 ) ;
#1302 = VERTEX_POINT ( 'NONE', #29114 ) ;
#1303 = VECTOR ( 'NONE', #84637, 1000.000000000000114 ) ;
#1304 = CARTESIAN_POINT ( 'NONE',  ( 17.96484262340118221, 39.93868534415484106, 7.964842623401181321 ) ) ;
#1305 = EDGE_CURVE ( 'NONE', #76195, #10376, #22926, .T. ) ;
#1306 = CARTESIAN_POINT ( 'NONE',  ( -0.1042174387088607435, 43.10736173766202484, 6.337391062633419558 ) ) ;
#1307 = EDGE_CURVE ( 'NONE', #94129, #86936, #40796, .T. ) ;
#1308 = ORIENTED_EDGE ( 'NONE', *, *, #88059, .T. ) ;
#1309 = CARTESIAN_POINT ( 'NONE',  ( 10.00000000000000178, 3.053748834913967425, 14.16423886937410082 ) ) ;
#1310 = ORIENTED_EDGE ( 'NONE', *, *, #27596, .T. ) ;
#1311 = ORIENTED_EDGE ( 'NONE', *, *, #12166, .F. ) ;
#1312 = CARTESIAN_POINT ( 'NONE',  ( 3.591859063236763294, 23.29030133659708568, -11.09922568453595026 ) ) ;
#1313 = CARTESIAN_POINT ( 'NONE',  ( 2.791683348922240793, 16.63393115100078745, 7.208316651077764092 ) ) ;
#1314 = CARTESIAN_POINT ( 'NONE',  ( 14.16722289976681814, 0.5000000000000004441, 4.928467845925615265 ) ) ;
#1315 = CARTESIAN_POINT ( 'NONE',  ( 19.10478245763051319, 10.10160829253885950, 5.990408912944328534 ) ) ;
#1316 = CARTESIAN_POINT ( 'NONE',  ( 18.52753015748618282, 13.92559781766745175, -4.923371831947291888 ) ) ;
#1317 = CARTESIAN_POINT ( 'NONE',  ( 10.00000000000000000, 36.81368534415484106, -10.88017736071110342 ) ) ;
#1318 = ORIENTED_EDGE ( 'NONE', *, *, #78245, .F. ) ;
#1319 = ORIENTED_EDGE ( 'NONE', *, *, #41541, .F. ) ;
#1320 = CARTESIAN_POINT ( 'NONE',  ( 3.969999999999999751, 10.25000000000000000, 3.750000000000000000 ) ) ;
#1321 = CARTESIAN_POINT ( 'NONE',  ( -0.8801773607110991993, 57.85535201082149825, -2.915334737309923874 ) ) ;
#1322 = CARTESIAN_POINT ( 'NONE',  ( -1.354709868695727959, 0.3640475087720941305, 14.93870011653151231 ) ) ;
#1323 = CARTESIAN_POINT ( 'NONE',  ( 20.88017736071110519, 60.56368534415484106, 2.639326808657452039E-16 ) ) ;
#1324 = CARTESIAN_POINT ( 'NONE',  ( 11.75249112336553381, 0.04962895880866900755, 8.918310463590511716 ) ) ;
#1325 = CARTESIAN_POINT ( 'NONE',  ( 14.92337183194729633, 32.67559781766745175, 8.527530157486181039 ) ) ;
#1326 = CARTESIAN_POINT ( 'NONE',  ( 10.00000000000000000, 57.87363466993042493, -12.81628187352647608 ) ) ;
#1327 = CARTESIAN_POINT ( 'NONE',  ( 5.114684334861586024, -17.52319251364448505, -3.750000000000001332 ) ) ;
#1328 = CARTESIAN_POINT ( 'NONE',  ( 2.791683348922237240, 20.38393115100078745, -7.208316651077763204 ) ) ;
#1329 = CARTESIAN_POINT ( 'NONE',  ( 0.6178305044545818747, 18.49863466993041428, -9.382169495545419124 ) ) ;
#1331 = CARTESIAN_POINT ( 'NONE',  ( -3.888850692990851954, -8.270209051930519806, -2.750000000000000000 ) ) ;
#1330 = PLANE ( 'NONE',  #13321 ) ;
#1332 = CARTESIAN_POINT ( 'NONE',  ( 17.96484262340118221, 46.18868534415484106, -7.964842623401177768 ) ) ;
#1333 = CARTESIAN_POINT ( 'NONE',  ( 10.00000000000000178, 57.25893115100078745, 9.846743663894594434 ) ) ;
#1334 = DIRECTION ( 'NONE',  ( 0.1822355254921578516, 0.000000000000000000, -0.9832549075639526182 ) ) ;
#1335 = CARTESIAN_POINT ( 'NONE',  ( 19.84674366389459621, 33.50893115100078745, 7.409399052514197653E-17 ) ) ;
#1336 = CARTESIAN_POINT ( 'NONE',  ( 0.1532563361054100626, 20.80059781766744464, -2.638427012816831230 ) ) ;
#1337 = CARTESIAN_POINT ( 'NONE',  ( 17.96484262340118221, 14.93868534415483751, 7.964842623401181321 ) ) ;
#1338 = CARTESIAN_POINT ( 'NONE',  ( 22.81628187352647785, 11.41530133659708390, 3.434112377981063169 ) ) ;
#1339 = CIRCLE ( 'NONE', #14092, 2.000000000000000000 ) ;
#1340 = PRESENTATION_STYLE_ASSIGNMENT (( #34861 ) ) ;
#1341 = CARTESIAN_POINT ( 'NONE',  ( -7.982674952684395642, 85.82256618331770426, 4.181766378585055399 ) ) ;
#1342 = CARTESIAN_POINT ( 'NONE',  ( 17.96484262340118221, 19.93868534415484106, 7.964842623401181321 ) ) ;
#1343 = DIRECTION ( 'NONE',  ( 0.9975640502598257520, -0.06975647374410356982, 0.000000000000000000 ) ) ;
#1345 = CARTESIAN_POINT ( 'NONE',  ( 0.5774900079438607392, 13.48035201082150358, 5.440088680355550821 ) ) ;
#1344 = CARTESIAN_POINT ( 'NONE',  ( 18.52753015748617571, 33.09226448433411605, 4.923371831947298993 ) ) ;
#1346 = CARTESIAN_POINT ( 'NONE',  ( 0.000000000000000000, 0.5000000000000004441, 0.000000000000000000 ) ) ;
#1347 = CARTESIAN_POINT ( 'NONE',  ( 2.035157376598824452, 33.68868534415484106, 7.964842623401179544 ) ) ;
#1348 = CIRCLE ( 'NONE', #65182, 0.09999999999999982514 ) ;
#1350 =( NAMED_UNIT ( * ) PLANE_ANGLE_UNIT ( ) SI_UNIT ( $, .RADIAN. ) );
#1349 = CARTESIAN_POINT ( 'NONE',  ( 22.26659068614894466, 63.88708216824730357, 7.082119434687054849 ) ) ;
#1351 = CARTESIAN_POINT ( 'NONE',  ( 19.84674366389459266, 18.71726448433411960, -2.638427012816827677 ) ) ;
#1352 = CARTESIAN_POINT ( 'NONE',  ( 0.1532563361054100626, 40.80059781766745886, -2.638427012816831230 ) ) ;
#1353 = CARTESIAN_POINT ( 'NONE',  ( 56.78206182523731371, 11.99999999999999645, 0.000000000000000000 ) ) ;
#1354 = CARTESIAN_POINT ( 'NONE',  ( 19.84674366389459621, 63.50893115100078745, 7.409399052514197653E-17 ) ) ;
#1356 = CARTESIAN_POINT ( 'NONE',  ( -5.795997163829992083, -0.03417435944610275333, -13.01802277140713926 ) ) ;
#1355 = CIRCLE ( 'NONE', #90757, 15.00000000000000000 ) ;
#1357 = VECTOR ( 'NONE', #75041, 1000.000000000000114 ) ;
#1358 = CARTESIAN_POINT ( 'NONE',  ( -11.30180206635943030, -57.06075279892166208, -3.750000000000000000 ) ) ;
#1359 = CARTESIAN_POINT ( 'NONE',  ( -4.164238869374098151, 21.59541550158063217, -3.795296366450310543 ) ) ;
#1360 = CARTESIAN_POINT ( 'NONE',  ( 17.20831665107776587, 34.13393115100078745, -7.208316651077762316 ) ) ;
#1361 = DIRECTION ( 'NONE',  ( -1.000000000000000000, 0.000000000000000000, 0.000000000000000000 ) ) ;
#1362 = ORIENTED_EDGE ( 'NONE', *, *, #16997, .T. ) ;
#1363 = CARTESIAN_POINT ( 'NONE',  ( 2.917880565312950480, 50.97041550158064638, -12.26659068614894821 ) ) ;
#1364 = CARTESIAN_POINT ( 'NONE',  ( 1.472469842513823179, 25.59226448433412315, -4.923371831947296329 ) ) ;
#1366 = CARTESIAN_POINT ( 'NONE',  ( 4.431036607602471200, 14.63595249122791131, 14.33059365769914173 ) ) ;
#1365 =( LENGTH_UNIT ( ) NAMED_UNIT ( * ) SI_UNIT ( .MILLI., .METRE. ) );
#1367 = CARTESIAN_POINT ( 'NONE',  ( 12.91533473730993009, 51.60535201082149825, -10.88017736071109987 ) ) ;
#1368 = CARTESIAN_POINT ( 'NONE',  ( 19.38216949554541557, 52.24863466993041072, -9.382169495545420901 ) ) ;
#1369 = CARTESIAN_POINT ( 'NONE',  ( 20.88017736071110164, 20.35535201082150891, 2.915334737309930979 ) ) ;
#1370 = CARTESIAN_POINT ( 'NONE',  ( 0.6178305044545818747, 43.49863466993042493, -9.382169495545419124 ) ) ;
#1371 = CARTESIAN_POINT ( 'NONE',  ( 0.6178305044545838731, -0.2513653300695798953, 9.382169495545420901 ) ) ;
#1372 = VERTEX_POINT ( 'NONE', #7635 ) ;
#1373 = CARTESIAN_POINT ( 'NONE',  ( 0.7166339456633684657, 15.00000000000000000, -15.98010739087745868 ) ) ;
#1374 = CYLINDRICAL_SURFACE ( 'NONE', #18936, 0.09999999999999939493 ) ;
#1375 = CARTESIAN_POINT ( 'NONE',  ( 24.16423886937410614, 59.51208216824728936, -3.795296366450302550 ) ) ;
#1376 = CARTESIAN_POINT ( 'NONE',  ( 24.16423886937410614, 19.51208216824729647, -3.795296366450302550 ) ) ;
#1377 = CARTESIAN_POINT ( 'NONE',  ( 7.084665262690076126, 19.10535201082150181, 10.88017736071109987 ) ) ;
#1378 = CARTESIAN_POINT ( 'NONE',  ( 2.035157376598824452, 38.68868534415483396, 7.964842623401179544 ) ) ;
#1379 = CARTESIAN_POINT ( 'NONE',  ( 20.15039907845753930, 70.00000000000000000, -6.262539305110068177 ) ) ;
#1380 = CARTESIAN_POINT ( 'NONE',  ( 2.791683348922237240, 0.3839311510007847872, -7.208316651077763204 ) ) ;
#1381 = CYLINDRICAL_SURFACE ( 'NONE', #44974, 0.2500000000000002220 ) ;
#1382 = CARTESIAN_POINT ( 'NONE',  ( 2.791683348922237240, 15.38393115100078212, -7.208316651077763204 ) ) ;
#1383 = CARTESIAN_POINT ( 'NONE',  ( 2.603489959281614308, 61.58210964143329846, 6.500000000000031086 ) ) ;
#1384 =( LENGTH_UNIT ( ) NAMED_UNIT ( * ) SI_UNIT ( .MILLI., .METRE. ) );
#1385 = CARTESIAN_POINT ( 'NONE',  ( 19.84674366389459266, 13.71726448433411782, -2.638427012816827677 ) ) ;
#1386 = CARTESIAN_POINT ( 'NONE',  ( 1.472469842513823179, 35.59226448433412315, -4.923371831947296329 ) ) ;
#1387 = EDGE_CURVE ( 'NONE', #78530, #49977, #45607, .T. ) ;
#1388 = CARTESIAN_POINT ( 'NONE',  ( 15.44008868035555793, 16.39701867748817321, -9.422509992056140149 ) ) ;
#1389 = CARTESIAN_POINT ( 'NONE',  ( -1.099225684535947600, 34.54030133659708923, 6.408140936763237150 ) ) ;
#1390 = CARTESIAN_POINT ( 'NONE',  ( 18.52753015748618282, 3.925597817667451306, -4.923371831947291888 ) ) ;
#1391 = LINE ( 'NONE', #31846, #2543 ) ;
#1392 = CARTESIAN_POINT ( 'NONE',  ( 1.472469842513823179, 46.42559781766745175, 4.923371831947296329 ) ) ;
#1394 = CARTESIAN_POINT ( 'NONE',  ( 22.26659068614894466, 3.887082168247300906, 7.082119434687054849 ) ) ;
#1393 = CARTESIAN_POINT ( 'NONE',  ( 12.63842701281683922, 29.55059781766745175, -9.846743663894590881 ) ) ;
#1395 = CARTESIAN_POINT ( 'NONE',  ( -2.266590686148945544, 21.38708216824730357, -7.082119434687050408 ) ) ;
#1396 = CARTESIAN_POINT ( 'NONE',  ( 2.035157376598822676, 52.43868534415483396, -7.964842623401177768 ) ) ;
#1397 = CARTESIAN_POINT ( 'NONE',  ( 20.88017736071110164, 10.35535201082150714, 2.915334737309930979 ) ) ;
#1398 = CARTESIAN_POINT ( 'NONE',  ( 17.96484262340118221, 44.93868534415483396, 7.964842623401181321 ) ) ;
#1399 = CARTESIAN_POINT ( 'NONE',  ( 20.88017736071110519, 30.56368534415484106, 2.639326808657452039E-16 ) ) ;
#1400 = ORIENTED_EDGE ( 'NONE', *, *, #12642, .F. ) ;
#1401 = CARTESIAN_POINT ( 'NONE',  ( 10.00000000000000178, 30.37363466993042138, 12.81628187352647608 ) ) ;
#1402 = CARTESIAN_POINT ( 'NONE',  ( 7.084665262690076126, 42.02201867748816966, -10.88017736071110164 ) ) ;
#1403 = ORIENTED_EDGE ( 'NONE', *, *, #70327, .T. ) ;
#1404 = CARTESIAN_POINT ( 'NONE',  ( 21.09922568453594849, 56.20696800326375353, 6.408140936763242479 ) ) ;
#1405 = CARTESIAN_POINT ( 'NONE',  ( 0.5774900079438607392, 53.48035201082151247, 5.440088680355550821 ) ) ;
#1406 = VECTOR ( 'NONE', #82915, 999.9999999999998863 ) ;
#1407 = EDGE_LOOP ( 'NONE', ( #82520, #59091, #75364, #18143 ) ) ;
#1408 = CARTESIAN_POINT ( 'NONE',  ( 2.035157376598824452, 53.68868534415484817, 7.964842623401179544 ) ) ;
#1409 = CARTESIAN_POINT ( 'NONE',  ( 7.160361147697994255, -84.29732993326337009, 4.000000000000000000 ) ) ;
#1410 = EDGE_CURVE ( 'NONE', #51188, #59403, #75116, .T. ) ;
#1411 = CARTESIAN_POINT ( 'NONE',  ( 10.00000000000000178, 70.00000000000000000, 0.000000000000000000 ) ) ;
#1412 = CARTESIAN_POINT ( 'NONE',  ( 24.16423886937410614, 59.30374883491397497, 8.672049930838204340E-16 ) ) ;
#1413 = CARTESIAN_POINT ( 'NONE',  ( 10.00000000000000178, 64.31368534415483396, 10.88017736071110342 ) ) ;
#1414 = CARTESIAN_POINT ( 'NONE',  ( 2.917880565312950480, 10.97041550158063572, -12.26659068614894821 ) ) ;
#1415 = SURFACE_STYLE_USAGE ( .BOTH. , #69895 ) ;
#1416 = CARTESIAN_POINT ( 'NONE',  ( 4.559911319644449179, 12.23035201082150536, -9.422509992056141925 ) ) ;
#1417 = CARTESIAN_POINT ( 'NONE',  ( 0.1532563361054083140, 41.00893115100078745, 1.131784320476157264E-15 ) ) ;
#1418 = VERTEX_POINT ( 'NONE', #21138 ) ;
#1419 = CARTESIAN_POINT ( 'NONE',  ( 12.63842701281683922, 34.55059781766745886, -9.846743663894590881 ) ) ;
#1420 = VECTOR ( 'NONE', #20421, 1000.000000000000000 ) ;
#1421 = CARTESIAN_POINT ( 'NONE',  ( 7.084665262690076126, 39.10535201082150536, 10.88017736071109987 ) ) ;
#1422 = CARTESIAN_POINT ( 'NONE',  ( 17.20831665107776587, 44.13393115100078745, -7.208316651077762316 ) ) ;
#1423 = CARTESIAN_POINT ( 'NONE',  ( 16.40814093676323893, 20.79030133659708923, 11.09922568453595026 ) ) ;
#1425 = DIRECTION ( 'NONE',  ( -0.000000000000000000, -1.000000000000000000, -0.000000000000000000 ) ) ;
#1424 = SURFACE_STYLE_USAGE ( .BOTH. , #10872 ) ;
#1426 = CARTESIAN_POINT ( 'NONE',  ( 4.559911319644449179, 47.23035201082150536, -9.422509992056141925 ) ) ;
#1427 = CARTESIAN_POINT ( 'NONE',  ( 10.00000000000000178, 53.05374883491396787, 14.16423886937410082 ) ) ;
#1428 =( GEOMETRIC_REPRESENTATION_CONTEXT ( 3 ) GLOBAL_UNCERTAINTY_ASSIGNED_CONTEXT ( ( #50285 ) ) GLOBAL_UNIT_ASSIGNED_CONTEXT ( ( #76156, #96339, #37675 ) ) REPRESENTATION_CONTEXT ( 'NONE', 'WORKASPACE' ) );
#1429 = AXIS2_PLACEMENT_3D ( 'NONE', #13943, #37436, #81435 ) ;
#1430 = CARTESIAN_POINT ( 'NONE',  ( -1.099225684535947600, 19.54030133659708568, 6.408140936763237150 ) ) ;
#1431 = CARTESIAN_POINT ( 'NONE',  ( -9.641450013144313047, 0.04962892333243928977, -11.16690429682362407 ) ) ;
#1432 = ORIENTED_EDGE ( 'NONE', *, *, #18304, .F. ) ;
#1433 = CARTESIAN_POINT ( 'NONE',  ( 0.6178305044545818747, 23.49863466993041783, -9.382169495545419124 ) ) ;
#1434 = CARTESIAN_POINT ( 'NONE',  ( 20.88017736071110164, 15.35535201082150358, 2.915334737309930979 ) ) ;
#1435 = EDGE_LOOP ( 'NONE', ( #67910, #41636, #41848, #61382 ) ) ;
#1436 = VERTEX_POINT ( 'NONE', #60103 ) ;
#1437 = EDGE_CURVE ( 'NONE', #63858, #63123, #76557, .T. ) ;
#1438 = CARTESIAN_POINT ( 'NONE',  ( 19.42250999205614193, 65.14701867748817676, 5.440088680355555262 ) ) ;
#1439 = CARTESIAN_POINT ( 'NONE',  ( 19.84674366389459621, 48.50893115100078745, 7.409399052514197653E-17 ) ) ;
#1440 = CARTESIAN_POINT ( 'NONE',  ( 19.84674366389459266, 33.71726448433410894, -2.638427012816827677 ) ) ;
#1441 = CARTESIAN_POINT ( 'NONE',  ( 10.64017930668209466, 14.63606904708525747, -10.57291749337217368 ) ) ;
#1442 = CARTESIAN_POINT ( 'NONE',  ( -1.099225684535947600, 64.54030133659709634, 6.408140936763237150 ) ) ;
#1443 = CARTESIAN_POINT ( 'NONE',  ( 0.1532563361054083140, 31.00893115100078390, 1.131784320476157264E-15 ) ) ;
#1444 = FACE_OUTER_BOUND ( 'NONE', #61728, .T. ) ;
#1445 = ADVANCED_FACE ( 'NONE', ( #74115 ), #5649, .T. ) ;
#1446 = VECTOR ( 'NONE', #14096, 1000.000000000000114 ) ;
#1448 = CARTESIAN_POINT ( 'NONE',  ( 10.00000000000000178, 2.258931151000784787, 9.846743663894594434 ) ) ;
#1447 = CARTESIAN_POINT ( 'NONE',  ( 5.076628168052704559, 10.17559781766745175, -8.527530157486179263 ) ) ;
#1450 = VERTEX_POINT ( 'NONE', #71076 ) ;
#1449 = CARTESIAN_POINT ( 'NONE',  ( 0.1532563361054082862, 46.21726448433411605, 2.638427012816831674 ) ) ;
#1451 = CARTESIAN_POINT ( 'NONE',  ( 20.32896413005680003, 16.77164270246083788, 5.963430220938287007 ) ) ;
#1452 = CARTESIAN_POINT ( 'NONE',  ( 13.43411237798106583, 27.66530133659708568, -12.81628187352647252 ) ) ;
#1453 = CARTESIAN_POINT ( 'NONE',  ( 10.00000000000000000, 46.81368534415484106, -10.88017736071110342 ) ) ;
#1454 = CARTESIAN_POINT ( 'NONE',  ( 22.26659068614895176, 39.72041550158063217, -7.082119434687042414 ) ) ;
#1455 = CARTESIAN_POINT ( 'NONE',  ( 0.1532563361054100626, 0.8005978176674514168, -2.638427012816831230 ) ) ;
#1456 = CARTESIAN_POINT ( 'NONE',  ( -14.11874224319634763, 0.2301510088455466507, 4.887061453529934596 ) ) ;
#1457 = CARTESIAN_POINT ( 'NONE',  ( 24.16423886937410614, 39.30374883491396787, 8.672049930838204340E-16 ) ) ;
#1458 = EDGE_CURVE ( 'NONE', #17988, #12785, #62566, .T. ) ;
#1459 = CARTESIAN_POINT ( 'NONE',  ( 20.36894250292379738, 54.92874883491396076, -10.36894250292379027 ) ) ;
#1460 = CARTESIAN_POINT ( 'NONE',  ( 24.16423886937410614, 24.51208216824730002, -3.795296366450302550 ) ) ;
#1462 = CARTESIAN_POINT ( 'NONE',  ( 34.56412365047464874, 28.99999999999999645, -9.500000000000000000 ) ) ;
#1461 = CARTESIAN_POINT ( 'NONE',  ( -4.164238869374099039, 31.80374883491396432, 8.674139862899312516E-16 ) ) ;
#1463 = CARTESIAN_POINT ( 'NONE',  ( 4.722628015970558479, -9.822377395415374579, -2.750000000000000000 ) ) ;
#1465 = CARTESIAN_POINT ( 'NONE',  ( 5.076628168052703671, 46.84226448433412315, 8.527530157486179263 ) ) ;
#1464 = CARTESIAN_POINT ( 'NONE',  ( 6.574584770547601487, -50.88238473864188194, 2.499999999996780797 ) ) ;
#1466 = CARTESIAN_POINT ( 'NONE',  ( -0.8801773607111008646, 43.27201867748817676, 2.915334737309923430 ) ) ;
#1467 = CARTESIAN_POINT ( 'NONE',  ( 10.00000000000000178, 70.00000000000000000, 0.000000000000000000 ) ) ;
#1468 = CARTESIAN_POINT ( 'NONE',  ( 20.00000000000000711, 92.21878522475820716, -5.248003389973252553 ) ) ;
#1469 = CARTESIAN_POINT ( 'NONE',  ( 12.63842701281683922, 39.55059781766744464, -9.846743663894590881 ) ) ;
#1470 = CARTESIAN_POINT ( 'NONE',  ( 10.00000000000000178, 50.37363466993042493, 12.81628187352647608 ) ) ;
#1471 = CARTESIAN_POINT ( 'NONE',  ( 3.795296366450306547, -4.654584498419360727, -14.16423886937410259 ) ) ;
#1472 = CARTESIAN_POINT ( 'NONE',  ( 17.20831665107776587, 39.13393115100079456, -7.208316651077762316 ) ) ;
#1473 = CARTESIAN_POINT ( 'NONE',  ( 1.472469842513823179, 66.42559781766745175, 4.923371831947296329 ) ) ;
#1474 = CARTESIAN_POINT ( 'NONE',  ( 10.00000000000000178, 38.05374883491396787, 14.16423886937410082 ) ) ;
#1475 = VERTEX_POINT ( 'NONE', #31088 ) ;
#1476 = CARTESIAN_POINT ( 'NONE',  ( -2.266590686148945544, 16.38708216824730357, -7.082119434687050408 ) ) ;
#1477 = CARTESIAN_POINT ( 'NONE',  ( -4.792102989642738287, -0.03417435944610275333, -15.26149223938179134 ) ) ;
#1479 = DIRECTION ( 'NONE',  ( -0.000000000000000000, 0.000000000000000000, 1.000000000000000000 ) ) ;
#1478 = LINE ( 'NONE', #16961, #22770 ) ;
#1480 = CARTESIAN_POINT ( 'NONE',  ( 0.5774900079438590739, 2.647018677488171434, -5.440088680355550821 ) ) ;
#1481 = CARTESIAN_POINT ( 'NONE',  ( 6.565887622018943937, 8.081968003263751754, -12.81628187352647608 ) ) ;
#1482 = DIRECTION ( 'NONE',  ( 1.000000000000000000, 0.000000000000000000, 0.000000000000000000 ) ) ;
#1483 = CARTESIAN_POINT ( 'NONE',  ( 10.00000000000000000, -0.2410688489992152128, -9.846743663894594434 ) ) ;
#1484 = CARTESIAN_POINT ( 'NONE',  ( 4.441537491767904022, -2.700695904837609351, -3.750000000000000000 ) ) ;
#1485 = CARTESIAN_POINT ( 'NONE',  ( -0.03743638938523759230, 14.25197528031018557, -6.399506433553937335 ) ) ;
#1486 = DIRECTION ( 'NONE',  ( -0.000000000000000000, -1.000000000000000000, 0.000000000000000000 ) ) ;
#1487 = CARTESIAN_POINT ( 'NONE',  ( -2.266590686148945544, 62.22041550158063927, 7.082119434687048631 ) ) ;
#1488 = DIRECTION ( 'NONE',  ( -0.08715574274765139351, -0.9961946980917461003, 0.000000000000000000 ) ) ;
#1489 = CARTESIAN_POINT ( 'NONE',  ( 10.00000000000000178, 24.31368534415484106, 10.88017736071110342 ) ) ;
#1490 = CARTESIAN_POINT ( 'NONE',  ( 15.44008868035555260, 19.73035201082150536, 9.422509992056143702 ) ) ;
#1491 = CARTESIAN_POINT ( 'NONE',  ( 7.361572987183170547, 67.05059781766746596, 9.846743663894590881 ) ) ;
#1492 = CARTESIAN_POINT ( 'NONE',  ( 12.63842701281683922, 54.55059781766745175, -9.846743663894590881 ) ) ;
#1493 = CARTESIAN_POINT ( 'NONE',  ( 6.565887622018943937, 60.16530133659707502, 12.81628187352647430 ) ) ;
#1494 = B_SPLINE_CURVE_WITH_KNOTS ( 'NONE', 3,
 ( #6532, #84018, #74530, #29510 ),
 .UNSPECIFIED., .F., .F.,
 ( 4, 4 ),
 ( 5.421010862427522170E-20, 0.002657014572711347174 ),
 .UNSPECIFIED. ) ;
#1495 = CARTESIAN_POINT ( 'NONE',  ( -8.924603092375777535, 75.06466731010172566, 2.900000000000000355 ) ) ;
#1496 = ORIENTED_EDGE ( 'NONE', *, *, #26313, .F. ) ;
#1497 = CIRCLE ( 'NONE', #4696, 14.49999999999999822 ) ;
#1498 = CARTESIAN_POINT ( 'NONE',  ( 0.5774900079438590739, 32.64701867748816966, -5.440088680355550821 ) ) ;
#1499 = EDGE_CURVE ( 'NONE', #12193, #16898, #77086, .T. ) ;
#1500 = CARTESIAN_POINT ( 'NONE',  ( 3.591859063236761518, 34.95696800326375353, 11.09922568453594849 ) ) ;
#1501 = DIRECTION ( 'NONE',  ( -5.818595309480553908E-17, -1.000000000000000000, -0.000000000000000000 ) ) ;
#1502 = AXIS2_PLACEMENT_3D ( 'NONE', #92176, #32141, #40157 ) ;
#1503 = B_SPLINE_CURVE_WITH_KNOTS ( 'NONE', 3,
 ( #37866, #6860, #858, #15368, #76338, #23356 ),
 .UNSPECIFIED., .F., .F.,
 ( 4, 2, 4 ),
 ( 0.0002800011564896236595, 0.0006862063972211524237, 0.001092411637952681296 ),
 .UNSPECIFIED. ) ;
#1504 = CARTESIAN_POINT ( 'NONE',  ( 1.472469842513823179, 55.59226448433412315, -4.923371831947296329 ) ) ;
#1505 = ADVANCED_FACE ( 'NONE', ( #62072 ), #85088, .T. ) ;
#1506 = CARTESIAN_POINT ( 'NONE',  ( 7.084665262690076126, 52.02201867748816255, -10.88017736071110164 ) ) ;
#1507 = B_SPLINE_CURVE_WITH_KNOTS ( 'NONE', 3,
 ( #54219, #55204, #84735, #8248, #69247, #85718 ),
 .UNSPECIFIED., .F., .F.,
 ( 4, 2, 4 ),
 ( 0.0002800026249563192867, 0.0006862078800502534673, 0.001092413135144187485 ),
 .UNSPECIFIED. ) ;
#1508 = CARTESIAN_POINT ( 'NONE',  ( 2.791683348922240793, 11.63393115100078568, 7.208316651077764092 ) ) ;
#1509 = CARTESIAN_POINT ( 'NONE',  ( 6.565887622018943937, 25.16530133659708213, 12.81628187352647430 ) ) ;
#1511 = CARTESIAN_POINT ( 'NONE',  ( 19.72487221294571569, 17.80223176428831522, -6.499999999999990230 ) ) ;
#1510 = CARTESIAN_POINT ( 'NONE',  ( 10.00000000000000178, 64.31368534415483396, 10.88017736071110342 ) ) ;
#1512 =( BOUNDED_SURFACE ( )  B_SPLINE_SURFACE ( 3, 2, ( 
 ( #55462, #86934, #71457 ),
 ( #47941, #9463, #86457 ),
 ( #32453, #78447, #23989 ),
 ( #40469, #69481, #999 ),
 ( #17955, #31461, #48442 ),
 ( #78941, #10452, #2971 ),
 ( #33421, #94431, #18447 ),
 ( #54460, #16485, #57418 ) ),
 .UNSPECIFIED., .F., .F., .T. ) 
 B_SPLINE_SURFACE_WITH_KNOTS ( ( 4, 2, 2, 4 ),
 ( 3, 3 ),
 ( 8.673617379884035472E-19, 0.002726357873101972664, 0.004089536809652958779, 0.005452715746203944461 ),
 ( 0.000000000000000000, 1.000000000000000000 ),
 .UNSPECIFIED. ) 
 GEOMETRIC_REPRESENTATION_ITEM ( )  RATIONAL_B_SPLINE_SURFACE ( (
 ( 1.000000000000000000, 0.7071067811865475727, 1.000000000000000000),
 ( 1.000000000000000000, 0.7287458841150015187, 1.000000000000000000),
 ( 1.000000000000000000, 0.7487351283423555603, 1.000000000000000000),
 ( 1.000000000000000000, 0.7766004504404603326, 1.000000000000000000),
 ( 1.000000000000000000, 0.7855344611292480739, 1.000000000000000000),
 ( 1.000000000000000000, 0.8027290847944021923, 1.000000000000000000),
 ( 1.000000000000000000, 0.8110176777142721338, 1.000000000000000000),
 ( 1.000000000000000000, 0.8188293140827601624, 1.000000000000000000) ) ) 
 REPRESENTATION_ITEM ( '' )  SURFACE ( )  );
#1513 = CARTESIAN_POINT ( 'NONE',  ( 18.28836319691949797, 54.34492782695772917, 6.499999999999920952 ) ) ;
#1514 = CARTESIAN_POINT ( 'NONE',  ( 3.591859063236763294, 63.29030133659708923, -11.09922568453595026 ) ) ;
#1515 = EDGE_LOOP ( 'NONE', ( #41990, #18383, #25113, #84572 ) ) ;
#1516 = CARTESIAN_POINT ( 'NONE',  ( 3.866399090317181653, 0.04922511925147171619, 14.23717170745775107 ) ) ;
#1517 = CARTESIAN_POINT ( 'NONE',  ( 19.05914839598885280, 24.96693863883976050, 6.499999999999962697 ) ) ;
#1518 = CARTESIAN_POINT ( 'NONE',  ( 15.44008868035555260, 49.73035201082150536, 9.422509992056143702 ) ) ;
#1519 = CARTESIAN_POINT ( 'NONE',  ( 22.81628187352648496, 41.83196800326375353, -3.434112377981050290 ) ) ;
#1520 = CARTESIAN_POINT ( 'NONE',  ( 19.84674366389459266, 23.71726448433412315, -2.638427012816827677 ) ) ;
#1521 = CARTESIAN_POINT ( 'NONE',  ( 0.5774900079438590739, 2.647018677488170990, -5.440088680355550821 ) ) ;
#1522 = CARTESIAN_POINT ( 'NONE',  ( 0.1532563361054100626, 25.80059781766744820, -2.638427012816831230 ) ) ;
#1523 = DIRECTION ( 'NONE',  ( 0.1822355254921448342, -0.000000000000000000, 0.9832549075639550606 ) ) ;
#1524 = CARTESIAN_POINT ( 'NONE',  ( 20.36894250292379738, 59.92874883491397497, -10.36894250292379027 ) ) ;
#1525 = ORIENTED_EDGE ( 'NONE', *, *, #93455, .T. ) ;
#1526 = CARTESIAN_POINT ( 'NONE',  ( 0.000000000000000000, 15.00000000000000000, 0.000000000000000000 ) ) ;
#1527 = CARTESIAN_POINT ( 'NONE',  ( 12.91533473730993009, 11.60535201082150536, -10.88017736071109987 ) ) ;
#1528 = DIRECTION ( 'NONE',  ( 0.000000000000000000, -0.000000000000000000, 1.000000000000000000 ) ) ;
#1529 = VERTEX_POINT ( 'NONE', #54573 ) ;
#1530 = ORIENTED_EDGE ( 'NONE', *, *, #39660, .F. ) ;
#1531 = CARTESIAN_POINT ( 'NONE',  ( -0.8801773607110991993, 7.855352010821506248, -2.915334737309923874 ) ) ;
#1532 = CARTESIAN_POINT ( 'NONE',  ( 20.88017736071110875, 15.77201867748817143, -2.915334737309920765 ) ) ;
#1533 = CARTESIAN_POINT ( 'NONE',  ( 10.00000000000000000, 44.75893115100078745, -9.846743663894594434 ) ) ;
#1534 = EDGE_CURVE ( 'NONE', #10597, #8161, #55979, .T. ) ;
#1535 = CARTESIAN_POINT ( 'NONE',  ( 22.81628187352648496, 51.83196800326376064, -3.434112377981050290 ) ) ;
#1536 = CARTESIAN_POINT ( 'NONE',  ( -16.60833333333331652, 99.75000000000000000, -8.000000000000000000 ) ) ;
#1538 = CARTESIAN_POINT ( 'NONE',  ( -4.164238869374099039, 26.80374883491397142, 8.674139862899312516E-16 ) ) ;
#1537 = CARTESIAN_POINT ( 'NONE',  ( 19.84674366389459266, 63.71726448433412315, -2.638427012816827677 ) ) ;
#1539 = CARTESIAN_POINT ( 'NONE',  ( 20.88017736071110519, 25.56368534415483751, 2.639326808657452039E-16 ) ) ;
#1540 = CARTESIAN_POINT ( 'NONE',  ( 4.559911319644449179, 2.230352010821504916, -9.422509992056141925 ) ) ;
#1541 = CARTESIAN_POINT ( 'NONE',  ( 0.1532563361054082862, 36.21726448433410894, 2.638427012816831674 ) ) ;
#1542 = SPHERICAL_SURFACE ( 'NONE', #10897, 0.2500000000000000000 ) ;
#1543 = CARTESIAN_POINT ( 'NONE',  ( 19.84674366389459266, 33.30059781766744464, 2.638427012816836559 ) ) ;
#1544 = ADVANCED_FACE ( 'NONE', ( #2108 ), #93563, .F. ) ;
#1545 = CARTESIAN_POINT ( 'NONE',  ( -3.469446951953614189E-15, 29.75893115100078390, -9.846743663894594434 ) ) ;
#1546 = EDGE_LOOP ( 'NONE', ( #6604, #81096, #63230, #9148 ) ) ;
#1547 = CARTESIAN_POINT ( 'NONE',  ( 20.88017736071110875, 5.772018677488170546, -2.915334737309920765 ) ) ;
#1548 = CARTESIAN_POINT ( 'NONE',  ( 20.88017736071110519, 65.56368534415483396, 2.639326808657452039E-16 ) ) ;
#1549 = CARTESIAN_POINT ( 'NONE',  ( 17.20831665107776587, 59.13393115100078745, -7.208316651077762316 ) ) ;
#1550 = CARTESIAN_POINT ( 'NONE',  ( 17.96484262340118221, 41.18868534415484106, -7.964842623401177768 ) ) ;
#1552 = CARTESIAN_POINT ( 'NONE',  ( 0.6178305044545838731, 34.74863466993042493, 9.382169495545420901 ) ) ;
#1551 = CARTESIAN_POINT ( 'NONE',  ( 0.5774900079438590739, 7.647018677488171434, -5.440088680355550821 ) ) ;
#1553 = CARTESIAN_POINT ( 'NONE',  ( 24.16423886937410614, 24.30374883491396787, 8.672049930838204340E-16 ) ) ;
#1554 = TOROIDAL_SURFACE ( 'NONE', #49394, 14.49999999999999822, 0.5000000000000000000 ) ;
#1555 = CARTESIAN_POINT ( 'NONE',  ( 16.40814093676323893, 45.79030133659708923, 11.09922568453595026 ) ) ;
#1556 = VERTEX_POINT ( 'NONE', #77571 ) ;
#1557 = CARTESIAN_POINT ( 'NONE',  ( 18.52753015748617571, 53.09226448433412315, 4.923371831947298993 ) ) ;
#1558 = CARTESIAN_POINT ( 'NONE',  ( 10.00000000000000000, 16.81368534415483751, -10.88017736071110342 ) ) ;
#1559 = VERTEX_POINT ( 'NONE', #16596 ) ;
#1560 = CARTESIAN_POINT ( 'NONE',  ( 4.559911319644449179, 23.89701867748817321, 9.422509992056141925 ) ) ;
#1561 = VERTEX_POINT ( 'NONE', #39601 ) ;
#1562 = CARTESIAN_POINT ( 'NONE',  ( 20.88017736071110164, 65.35535201082150536, 2.915334737309930979 ) ) ;
#1563 = CARTESIAN_POINT ( 'NONE',  ( 20.15039907845753220, 31.74884699246888786, 6.262539305110077059 ) ) ;
#1564 = CARTESIAN_POINT ( 'NONE',  ( 18.52753015748617571, 3.092264484334118269, 4.923371831947298993 ) ) ;
#1565 = CARTESIAN_POINT ( 'NONE',  ( 10.00000000000000000, -0.2410688489992152128, -9.846743663894594434 ) ) ;
#1566 = CARTESIAN_POINT ( 'NONE',  ( -10.19513985507818177, 0.3640475087720994041, -11.00268709613231977 ) ) ;
#1567 = EDGE_CURVE ( 'NONE', #22543, #76539, #36838, .T. ) ;
#1568 = CARTESIAN_POINT ( 'NONE',  ( -46.58521628013341598, 101.6760492933278215, 7.987317478326372289 ) ) ;
#1570 = ORIENTED_EDGE ( 'NONE', *, *, #53671, .F. ) ;
#1569 = CARTESIAN_POINT ( 'NONE',  ( 14.92337183194729633, 12.67559781766745353, 8.527530157486181039 ) ) ;
#1571 = CARTESIAN_POINT ( 'NONE',  ( 14.92337183194729988, 44.34226448433412315, -8.527530157486177487 ) ) ;
#1572 = VERTEX_POINT ( 'NONE', #23124 ) ;
#1573 = ORIENTED_EDGE ( 'NONE', *, *, #56390, .F. ) ;
#1574 = CARTESIAN_POINT ( 'NONE',  ( 66.76470751278411342, 44.49999999999998579, -10.00000000000000000 ) ) ;
#1575 = CARTESIAN_POINT ( 'NONE',  ( -0.3689425029237881626, 12.42874883491396609, 10.36894250292379027 ) ) ;
#1576 = CARTESIAN_POINT ( 'NONE',  ( 6.565887622018943937, 63.08196800326376064, -12.81628187352647608 ) ) ;
#1577 = AXIS2_PLACEMENT_3D ( 'NONE', #56614, #86134, #18135 ) ;
#1578 = CARTESIAN_POINT ( 'NONE',  ( 24.16423886937410614, 14.51208216824730179, -3.795296366450302550 ) ) ;
#1579 = LINE ( 'NONE', #33027, #36213 ) ;
#1581 = CARTESIAN_POINT ( 'NONE',  ( -0.8801773607111008646, 63.27201867748817676, 2.915334737309923430 ) ) ;
#1580 = LINE ( 'NONE', #93040, #88114 ) ;
#1582 = CARTESIAN_POINT ( 'NONE',  ( 7.084665262690076126, 17.02201867748817676, -10.88017736071110164 ) ) ;
#1583 =( LENGTH_UNIT ( ) NAMED_UNIT ( * ) SI_UNIT ( .MILLI., .METRE. ) );
#1584 = ORIENTED_EDGE ( 'NONE', *, *, #76121, .F. ) ;
#1585 =( LENGTH_UNIT ( ) NAMED_UNIT ( * ) SI_UNIT ( .MILLI., .METRE. ) );
#1587 = VECTOR ( 'NONE', #22324, 1000.000000000000000 ) ;
#1586 = CARTESIAN_POINT ( 'NONE',  ( 18.52753015748618282, 8.925597817667451750, -4.923371831947291888 ) ) ;
#1588 = CARTESIAN_POINT ( 'NONE',  ( 22.81628187352648496, 36.83196800326376064, -3.434112377981050290 ) ) ;
#1589 = CARTESIAN_POINT ( 'NONE',  ( 18.52753015748617571, 28.09226448433411960, 4.923371831947298993 ) ) ;
#1590 = CARTESIAN_POINT ( 'NONE',  ( 7.640917710489005366, 14.95077488074853456, -12.61992379908754458 ) ) ;
#1591 = CARTESIAN_POINT ( 'NONE',  ( -2.816281873526473856, 19.12363466993042138, 9.499525473075851096E-16 ) ) ;
#1592 = CARTESIAN_POINT ( 'NONE',  ( -6.189644032515865035, 0.04922511925147087658, 13.39157970158793276 ) ) ;
#1593 = CARTESIAN_POINT ( 'NONE',  ( 1.472469842513823179, 11.42559781766745175, 4.923371831947296329 ) ) ;
#1594 = ORIENTED_EDGE ( 'NONE', *, *, #90193, .F. ) ;
#1595 = ORIENTED_EDGE ( 'NONE', *, *, #22327, .T. ) ;
#1596 = CARTESIAN_POINT ( 'NONE',  ( -0.8801773607111009756, 43.06368534415484106, 1.068504757029289695E-15 ) ) ;
#1597 = CARTESIAN_POINT ( 'NONE',  ( 24.16423886937409904, 29.09541550158063572, 3.795296366450317205 ) ) ;
#1598 = CARTESIAN_POINT ( 'NONE',  ( 19.84674366389459266, 43.30059781766744464, 2.638427012816836559 ) ) ;
#1599 = ADVANCED_FACE ( 'NONE', ( #9580 ), #1613, .T. ) ;
#1600 = CARTESIAN_POINT ( 'NONE',  ( 10.00000000000000178, 2.258931151000784787, 9.846743663894594434 ) ) ;
#1601 = B_SPLINE_CURVE_WITH_KNOTS ( 'NONE', 3,
 ( #20973, #97472, #89943, #21460 ),
 .UNSPECIFIED., .F., .F.,
 ( 4, 4 ),
 ( 3.469446951953614189E-18, 0.002392975128318428242 ),
 .UNSPECIFIED. ) ;
#1603 = CARTESIAN_POINT ( 'NONE',  ( 13.99999999999999822, 61.50000000000000711, -6.000000000000000000 ) ) ;
#1602 = CARTESIAN_POINT ( 'NONE',  ( 6.565887622018943937, 60.16530133659707502, 12.81628187352647430 ) ) ;
#1604 = CARTESIAN_POINT ( 'NONE',  ( 15.44008868035555260, 29.73035201082150891, 9.422509992056143702 ) ) ;
#1605 = DIRECTION ( 'NONE',  ( -0.000000000000000000, -1.000000000000000000, -0.000000000000000000 ) ) ;
#1606 = CIRCLE ( 'NONE', #6355, 14.49999999999999822 ) ;
#1607 = CARTESIAN_POINT ( 'NONE',  ( 19.38216949554541202, 25.99863466993042138, 9.382169495545424454 ) ) ;
#1608 = CARTESIAN_POINT ( 'NONE',  ( 0.1532563361054083140, 36.00893115100078745, 1.131784320476157264E-15 ) ) ;
#1609 = CARTESIAN_POINT ( 'NONE',  ( -9.422509992056136596, -1.519647989178487979, 5.440088680355559703 ) ) ;
#1610 = CARTESIAN_POINT ( 'NONE',  ( 0.6178305044545838731, 49.74863466993041072, 9.382169495545420901 ) ) ;
#1611 = DIRECTION ( 'NONE',  ( -0.8320502943378437211, 0.5547001962252290364, 0.000000000000000000 ) ) ;
#1613 = CYLINDRICAL_SURFACE ( 'NONE', #68754, 0.5000000000000000000 ) ;
#1612 = CARTESIAN_POINT ( 'NONE',  ( 4.559911319644449179, 47.23035201082150536, -9.422509992056141925 ) ) ;
#1614 = DIRECTION ( 'NONE',  ( -1.000000000000000000, -2.569960705150826877E-16, 0.000000000000000000 ) ) ;
#1615 = EDGE_CURVE ( 'NONE', #75199, #35183, #12837, .T. ) ;
#1616 = CARTESIAN_POINT ( 'NONE',  ( 1.042145700049407653, 14.74216108172003104, -6.499999999999879208 ) ) ;
#1617 = CARTESIAN_POINT ( 'NONE',  ( 0.5774900079438590739, 57.64701867748817676, -5.440088680355550821 ) ) ;
#1618 = CARTESIAN_POINT ( 'NONE',  ( 19.42250999205614548, 55.98035201082150536, -5.440088680355545492 ) ) ;
#1619 = DIRECTION ( 'NONE',  ( -0.000000000000000000, -1.000000000000000000, -0.000000000000000000 ) ) ;
#1620 = CARTESIAN_POINT ( 'NONE',  ( 11.92686044187655980, 12.39664270246084676, -3.195792623639533314 ) ) ;
#1621 = EDGE_CURVE ( 'NONE', #64078, #31259, #50151, .T. ) ;
#1622 = EDGE_CURVE ( 'NONE', #36305, #50106, #94278, .T. ) ;
#1623 = CARTESIAN_POINT ( 'NONE',  ( 17.96484262340118221, 11.18868534415484106, -7.964842623401177768 ) ) ;
#1624 = CARTESIAN_POINT ( 'NONE',  ( 0.1532563361054083140, 51.00893115100078745, 1.131784320476157264E-15 ) ) ;
#1626 = CARTESIAN_POINT ( 'NONE',  ( 9.383624259804085099, 0.2301501999354983174, -11.62625599701879509 ) ) ;
#1625 = CARTESIAN_POINT ( 'NONE',  ( 2.035157376598822676, 17.43868534415483751, -7.964842623401177768 ) ) ;
#1627 = CARTESIAN_POINT ( 'NONE',  ( 22.81628187352648496, 31.83196800326375353, -3.434112377981050290 ) ) ;
#1628 = ORIENTED_EDGE ( 'NONE', *, *, #70114, .F. ) ;
#1629 = CARTESIAN_POINT ( 'NONE',  ( 2.035157376598824452, 43.68868534415484106, 7.964842623401179544 ) ) ;
#1631 = CARTESIAN_POINT ( 'NONE',  ( -12.83294900548071205, 0.3639312116172442879, 7.766300266068302705 ) ) ;
#1630 = CARTESIAN_POINT ( 'NONE',  ( 13.43411237798105340, 0.5819680032637533085, 12.81628187352647963 ) ) ;
#1632 = CARTESIAN_POINT ( 'NONE',  ( -0.8801773607111008646, 18.27201867748817321, 2.915334737309923430 ) ) ;
#1633 = CARTESIAN_POINT ( 'NONE',  ( 10.00000000000000178, 44.31368534415484106, 10.88017736071110342 ) ) ;
#1634 = CARTESIAN_POINT ( 'NONE',  ( 2.917880565312948704, 57.63708216824731068, 12.26659068614894643 ) ) ;
#1635 = CARTESIAN_POINT ( 'NONE',  ( 12.63842701281683922, 29.55059781766745175, -9.846743663894590881 ) ) ;
#1636 = CARTESIAN_POINT ( 'NONE',  ( 19.42250999205614193, 65.14701867748817676, 5.440088680355555262 ) ) ;
#1637 = CARTESIAN_POINT ( 'NONE',  ( -8.399999999999998579, 98.49999999999998579, -8.000000000000000000 ) ) ;
#1638 = CARTESIAN_POINT ( 'NONE',  ( 24.16423886937410614, 19.51208216824729647, -3.795296366450302550 ) ) ;
#1639 = CARTESIAN_POINT ( 'NONE',  ( -0.5000000000000073275, 80.99999999999994316, 0.000000000000000000 ) ) ;
#1640 = ORIENTED_EDGE ( 'NONE', *, *, #78041, .T. ) ;
#1641 = EDGE_LOOP ( 'NONE', ( #14568, #34746, #43556, #39557 ) ) ;
#1642 = CARTESIAN_POINT ( 'NONE',  ( 2.917880565312950480, 40.97041550158063217, -12.26659068614894821 ) ) ;
#1643 = CARTESIAN_POINT ( 'NONE',  ( 13.79529636645031943, 30.34541550158063927, -14.16423886937409904 ) ) ;
#1644 = CARTESIAN_POINT ( 'NONE',  ( 19.84674366389459621, 3.508931151000785231, 7.409399052514197653E-17 ) ) ;
#1645 = CARTESIAN_POINT ( 'NONE',  ( 12.63842701281683034, 62.46726448433410894, 9.846743663894596210 ) ) ;
#1646 = CARTESIAN_POINT ( 'NONE',  ( 0.000000000000000000, 69.50000000000000000, -6.000000000000000000 ) ) ;
#1648 = CARTESIAN_POINT ( 'NONE',  ( 19.38216949554541557, 37.24863466993041783, -9.382169495545420901 ) ) ;
#1647 = CARTESIAN_POINT ( 'NONE',  ( 17.96484262340118221, 61.18868534415482685, -7.964842623401177768 ) ) ;
#1649 = CARTESIAN_POINT ( 'NONE',  ( 13.79529636645031943, 30.34541550158063927, -14.16423886937409904 ) ) ;
#1650 = B_SPLINE_CURVE_WITH_KNOTS ( 'NONE', 3,
 ( #92412, #93890, #85907, #25418, #40902, #2919 ),
 .UNSPECIFIED., .F., .F.,
 ( 4, 2, 4 ),
 ( 0.0002800075630785962052, 0.0006862128664728917634, 0.001092418169867187322 ),
 .UNSPECIFIED. ) ;
#1651 = CARTESIAN_POINT ( 'NONE',  ( 4.559911319644449179, 28.89701867748817321, 9.422509992056141925 ) ) ;
#1652 = CARTESIAN_POINT ( 'NONE',  ( 10.00000000000000178, 29.31368534415483751, 10.88017736071110342 ) ) ;
#1653 = FACE_OUTER_BOUND ( 'NONE', #20086, .T. ) ;
#1654 = CARTESIAN_POINT ( 'NONE',  ( 1.472469842513823179, 0.5922644843341181575, -4.923371831947296329 ) ) ;
#1655 = ADVANCED_FACE ( 'NONE', ( #38607 ), #78570, .T. ) ;
#1656 = CARTESIAN_POINT ( 'NONE',  ( 4.923371831947301658, -12.32440218233254292, 8.527530157486175710 ) ) ;
#1657 = ORIENTED_EDGE ( 'NONE', *, *, #930, .T. ) ;
#1658 = CYLINDRICAL_SURFACE ( 'NONE', #12376, 15.00000000000000000 ) ;
#1659 = ORIENTED_EDGE ( 'NONE', *, *, #52501, .T. ) ;
#1660 = FACE_OUTER_BOUND ( 'NONE', #3950, .T. ) ;
#1661 = VECTOR ( 'NONE', #96367, 1000.000000000000000 ) ;
#1662 = ORIENTED_EDGE ( 'NONE', *, *, #74034, .F. ) ;
#1663 = CARTESIAN_POINT ( 'NONE',  ( 24.16423886937409904, 4.095415501580634832, 3.795296366450317205 ) ) ;
#1665 = CARTESIAN_POINT ( 'NONE',  ( 20.88017736071110519, 15.56368534415483751, 2.639326808657452039E-16 ) ) ;
#1664 = CARTESIAN_POINT ( 'NONE',  ( 17.08211943468705130, 63.47041550158063927, 12.26659068614894998 ) ) ;
#1667 = CARTESIAN_POINT ( 'NONE',  ( 17.20831665107776587, 54.13393115100079456, -7.208316651077762316 ) ) ;
#1666 = CARTESIAN_POINT ( 'NONE',  ( 0.1532563361054100626, 30.80059781766744820, -2.638427012816831230 ) ) ;
#1668 = PRESENTATION_STYLE_ASSIGNMENT (( #38659 ) ) ;
#1669 = CARTESIAN_POINT ( 'NONE',  ( -1.099225684535947600, -0.4596986634029132657, 6.408140936763237150 ) ) ;
#1670 = VERTEX_POINT ( 'NONE', #53595 ) ;
#1671 = CARTESIAN_POINT ( 'NONE',  ( -0.3689425029237898834, 51.17874883491397497, -10.36894250292378850 ) ) ;
#1672 = ORIENTED_EDGE ( 'NONE', *, *, #41805, .F. ) ;
#1673 = CARTESIAN_POINT ( 'NONE',  ( 13.79529636645030344, 43.26208216824730357, 14.16423886937410614 ) ) ;
#1674 = ORIENTED_EDGE ( 'NONE', *, *, #63110, .F. ) ;
#1675 = CARTESIAN_POINT ( 'NONE',  ( 20.88017736071110164, 25.35535201082150891, 2.915334737309930979 ) ) ;
#1676 = AXIS2_PLACEMENT_3D ( 'NONE', #76704, #7236, #53220 ) ;
#1677 = CARTESIAN_POINT ( 'NONE',  ( 12.91533473730992121, 44.52201867748816966, 10.88017736071110164 ) ) ;
#1678 = CARTESIAN_POINT ( 'NONE',  ( 2.791683348922237240, 45.38393115100079456, -7.208316651077763204 ) ) ;
#1679 = CARTESIAN_POINT ( 'NONE',  ( 12.91533473730992121, 39.52201867748817676, 10.88017736071110164 ) ) ;
#1680 = CARTESIAN_POINT ( 'NONE',  ( 10.39655283154076848, 14.95077488074853456, 10.46698568711271093 ) ) ;
#1681 = CARTESIAN_POINT ( 'NONE',  ( 17.96484262340118221, 61.18868534415482685, -7.964842623401177768 ) ) ;
#1682 = CARTESIAN_POINT ( 'NONE',  ( 0.5774900079438607392, 33.48035201082150536, 5.440088680355550821 ) ) ;
#1683 = B_SPLINE_CURVE_WITH_KNOTS ( 'NONE', 3,
 ( #94947, #20440, #87450, #88930, #57928, #73423 ),
 .UNSPECIFIED., .F., .F.,
 ( 4, 2, 4 ),
 ( 3.409110551495869127E-05, 0.0004400426677367973052, 0.0008459942299586359869 ),
 .UNSPECIFIED. ) ;
#1684 = CARTESIAN_POINT ( 'NONE',  ( 0.4400000000000020006, 1.019547802438468986, -3.750000000000000000 ) ) ;
#1685 = CARTESIAN_POINT ( 'NONE',  ( 1.472469842513823179, 6.425597817667451750, 4.923371831947296329 ) ) ;
#1686 = CARTESIAN_POINT ( 'NONE',  ( -3.627483523208183680, -3.617667194774622619, 2.499999999999597655 ) ) ;
#1687 = ORIENTED_EDGE ( 'NONE', *, *, #24059, .T. ) ;
#1688 = CARTESIAN_POINT ( 'NONE',  ( 18.52753015748617571, 43.09226448433412315, 4.923371831947298993 ) ) ;
#1689 = CARTESIAN_POINT ( 'NONE',  ( 18.29284471827482150, 10.40189080397285437, -6.499999999999984901 ) ) ;
#1690 = DIRECTION ( 'NONE',  ( -0.000000000000000000, 0.000000000000000000, 1.000000000000000000 ) ) ;
#1691 = DIRECTION ( 'NONE',  ( 1.000000000000000000, 0.000000000000000000, -0.000000000000000000 ) ) ;
#1692 = CARTESIAN_POINT ( 'NONE',  ( 14.47650479471822216, 0.5000000000000004441, -3.928206833722012625 ) ) ;
#1693 = CARTESIAN_POINT ( 'NONE',  ( 0.8952175423695086787, 53.52576239577083328, 5.990408912944362285 ) ) ;
#1694 = CARTESIAN_POINT ( 'NONE',  ( 19.84674366389459266, 53.30059781766744464, 2.638427012816836559 ) ) ;
#1695 = CARTESIAN_POINT ( 'NONE',  ( 13.79529636645030344, 53.26208216824730357, 14.16423886937410614 ) ) ;
#1696 = CARTESIAN_POINT ( 'NONE',  ( 1.472469842513823179, 61.42559781766745175, 4.923371831947296329 ) ) ;
#1697 = ORIENTED_EDGE ( 'NONE', *, *, #73921, .T. ) ;
#1698 = DIRECTION ( 'NONE',  ( 1.000000000000000000, 0.000000000000000000, 0.000000000000000000 ) ) ;
#1699 = CARTESIAN_POINT ( 'NONE',  ( 14.92337183194729633, 22.67559781766745175, 8.527530157486181039 ) ) ;
#1700 = CARTESIAN_POINT ( 'NONE',  ( 13.43411237798105340, 55.58196800326374643, 12.81628187352647963 ) ) ;
#1701 = EDGE_CURVE ( 'NONE', #97107, #26202, #14406, .T. ) ;
#1702 = CARTESIAN_POINT ( 'NONE',  ( 14.92337183194729988, 64.34226448433412315, -8.527530157486177487 ) ) ;
#1703 = CARTESIAN_POINT ( 'NONE',  ( 20.88017736071110164, 55.35535201082149825, 2.915334737309930979 ) ) ;
#1704 = CARTESIAN_POINT ( 'NONE',  ( 4.656459206268571904, -8.255604869814334279, -2.750000000000000444 ) ) ;
#1705 = VERTEX_POINT ( 'NONE', #76594 ) ;
#1706 = CARTESIAN_POINT ( 'NONE',  ( 10.00000000000000178, 63.05374883491396076, 14.16423886937410082 ) ) ;
#1707 = DIRECTION ( 'NONE',  ( -0.9914448613738113814, 0.000000000000000000, 0.1305261922200445512 ) ) ;
#1708 = CARTESIAN_POINT ( 'NONE',  ( 2.035157376598822676, 32.43868534415483396, -7.964842623401177768 ) ) ;
#1709 = VECTOR ( 'NONE', #83376, 1000.000000000000114 ) ;
#1711 = CARTESIAN_POINT ( 'NONE',  ( 10.00000000000000000, 61.81368534415484106, -10.88017736071110342 ) ) ;
#1710 = CARTESIAN_POINT ( 'NONE',  ( 6.565887622018943937, 10.16530133659708746, 12.81628187352647430 ) ) ;
#1712 = CARTESIAN_POINT ( 'NONE',  ( 18.72515096720583827, 65.05509018479936856, 6.499999999999810818 ) ) ;
#1713 = SURFACE_SIDE_STYLE ('',( #70194 ) ) ;
#1715 = VECTOR ( 'NONE', #13530, 1000.000000000000000 ) ;
#1714 = CARTESIAN_POINT ( 'NONE',  ( -9.159723438033276821, 0.000000000000000000, 10.91613331444536250 ) ) ;
#1717 = FACE_OUTER_BOUND ( 'NONE', #48148, .T. ) ;
#1716 = CARTESIAN_POINT ( 'NONE',  ( 2.035157376598824452, 53.68868534415484817, 7.964842623401179544 ) ) ;
#1718 = CARTESIAN_POINT ( 'NONE',  ( 2.791683348922240793, 41.63393115100078745, 7.208316651077764092 ) ) ;
#1719 = CARTESIAN_POINT ( 'NONE',  ( 19.84674366389459266, 3.717264484334118713, -2.638427012816827677 ) ) ;
#1720 = CARTESIAN_POINT ( 'NONE',  ( 2.915334737309928315, -35.47798132251182324, 10.88017736071109987 ) ) ;
#1721 = CARTESIAN_POINT ( 'NONE',  ( 0.6178305044545838731, 14.74863466993041783, 9.382169495545420901 ) ) ;
#1722 = EDGE_CURVE ( 'NONE', #68545, #40747, #20847, .T. ) ;
#1723 = VECTOR ( 'NONE', #88199, 1000.000000000000000 ) ;
#1725 = CARTESIAN_POINT ( 'NONE',  ( 1.274849032794292736, 67.55509018479936856, -6.499999999999977796 ) ) ;
#1724 = CARTESIAN_POINT ( 'NONE',  ( -0.8801773607111008646, 18.27201867748817321, 2.915334737309923430 ) ) ;
#1726 = CARTESIAN_POINT ( 'NONE',  ( 6.204703633549690345, 40.76208216824731778, -14.16423886937410259 ) ) ;
#1727 = CARTESIAN_POINT ( 'NONE',  ( -2.266590686148945544, 26.38708216824730357, -7.082119434687050408 ) ) ;
#1728 = CARTESIAN_POINT ( 'NONE',  ( -0.3689425029237881626, 62.42874883491396787, 10.36894250292379027 ) ) ;
#1729 = CARTESIAN_POINT ( 'NONE',  ( 12.63842701281683922, 29.55059781766745175, -9.846743663894590881 ) ) ;
#1730 = CARTESIAN_POINT ( 'NONE',  ( 12.63842701281683922, 24.55059781766745175, -9.846743663894590881 ) ) ;
#1731 = CARTESIAN_POINT ( 'NONE',  ( 15.44008868035555793, 16.39701867748817321, -9.422509992056140149 ) ) ;
#1732 = EDGE_CURVE ( 'NONE', #49491, #1559, #46589, .T. ) ;
#1733 = ORIENTED_EDGE ( 'NONE', *, *, #95525, .T. ) ;
#1734 = CARTESIAN_POINT ( 'NONE',  ( 10.00000000000000178, 42.25893115100078745, 9.846743663894594434 ) ) ;
#1735 = CARTESIAN_POINT ( 'NONE',  ( 20.88017736071110519, 30.56368534415484106, 2.639326808657452039E-16 ) ) ;
#1736 = CARTESIAN_POINT ( 'NONE',  ( 10.00000000000000000, 59.75893115100078745, -9.846743663894594434 ) ) ;
#1738 = CARTESIAN_POINT ( 'NONE',  ( 1.959929470562282283, 61.50257860105349295, 5.767676674365853629 ) ) ;
#1737 = CARTESIAN_POINT ( 'NONE',  ( 13.79529636645030344, 18.26208216824730002, 14.16423886937410614 ) ) ;
#1739 = CARTESIAN_POINT ( 'NONE',  ( -5.149999999999996803, 98.49999999999998579, -8.525133428036873795 ) ) ;
#1740 = EDGE_CURVE ( 'NONE', #77207, #79612, #51888, .T. ) ;
#1741 = CARTESIAN_POINT ( 'NONE',  ( 12.63842701281683922, 9.550597817667449974, -9.846743663894590881 ) ) ;
#1742 = CARTESIAN_POINT ( 'NONE',  ( 16.40814093676323893, 45.79030133659708923, 11.09922568453595026 ) ) ;
#1743 = CARTESIAN_POINT ( 'NONE',  ( 5.076628168052704559, 55.17559781766745175, -8.527530157486179263 ) ) ;
#1744 = ORIENTED_EDGE ( 'NONE', *, *, #48499, .F. ) ;
#1745 = CARTESIAN_POINT ( 'NONE',  ( 12.83294900548063744, 0.5000000000000004441, -7.766300266068363101 ) ) ;
#1746 = CARTESIAN_POINT ( 'NONE',  ( 0.000000000000000000, 0.000000000000000000, 0.000000000000000000 ) ) ;
#1747 = CARTESIAN_POINT ( 'NONE',  ( 17.96484262340118221, 6.188685344154837509, -7.964842623401177768 ) ) ;
#1748 = CARTESIAN_POINT ( 'NONE',  ( 7.084665262690076126, 52.02201867748816255, -10.88017736071110164 ) ) ;
#1749 = CARTESIAN_POINT ( 'NONE',  ( 22.26659068614895176, 4.720415501580633943, -7.082119434687042414 ) ) ;
#1750 = CARTESIAN_POINT ( 'NONE',  ( 4.559911319644449179, 53.89701867748817676, 9.422509992056141925 ) ) ;
#1751 = CARTESIAN_POINT ( 'NONE',  ( 19.84674366389459266, 38.30059781766745175, 2.638427012816836559 ) ) ;
#1752 = CARTESIAN_POINT ( 'NONE',  ( -0.8801773607111009756, 23.06368534415484106, 1.068504757029289695E-15 ) ) ;
#1753 = DIRECTION ( 'NONE',  ( -0.000000000000000000, -0.000000000000000000, 1.000000000000000000 ) ) ;
#1754 = CARTESIAN_POINT ( 'NONE',  ( 1.472469842513823179, 65.59226448433412315, -4.923371831947296329 ) ) ;
#1755 = MECHANICAL_DESIGN_GEOMETRIC_PRESENTATION_REPRESENTATION (  '', ( #6507 ), #67247 ) ;
#1756 = LINE ( 'NONE', #53749, #85727 ) ;
#1757 = VERTEX_POINT ( 'NONE', #35887 ) ;
#1758 = ORIENTED_EDGE ( 'NONE', *, *, #63670, .F. ) ;
#1759 = AXIS2_PLACEMENT_3D ( 'NONE', #38100, #97133, #68094 ) ;
#1760 = DIRECTION ( 'NONE',  ( 1.000000000000000000, 0.000000000000000000, 0.000000000000000000 ) ) ;
#1761 = DIRECTION ( 'NONE',  ( -0.5224985647159612334, -0.000000000000000000, 0.8526401643540847397 ) ) ;
#1762 = CARTESIAN_POINT ( 'NONE',  ( 0.1532563361054100626, 40.80059781766745886, -2.638427012816831230 ) ) ;
#1763 = CARTESIAN_POINT ( 'NONE',  ( 1.472469842513823179, 16.42559781766745175, 4.923371831947296329 ) ) ;
#1764 = CARTESIAN_POINT ( 'NONE',  ( 0.6178305044545818747, 63.49863466993043204, -9.382169495545419124 ) ) ;
#1766 = CARTESIAN_POINT ( 'NONE',  ( 5.076628168052703671, 46.84226448433412315, 8.527530157486179263 ) ) ;
#1765 = CARTESIAN_POINT ( 'NONE',  ( 15.44008868035555260, 24.73035201082150891, 9.422509992056143702 ) ) ;
#1767 = CARTESIAN_POINT ( 'NONE',  ( 0.000000000000000000, 0.5000000000000004441, 0.000000000000000000 ) ) ;
#1768 = CARTESIAN_POINT ( 'NONE',  ( 2.917880565312948704, 37.63708216824731068, 12.26659068614894643 ) ) ;
#1769 = CARTESIAN_POINT ( 'NONE',  ( 22.26659068614894466, 53.88708216824731068, 7.082119434687054849 ) ) ;
#1770 = DIRECTION ( 'NONE',  ( 0.000000000000000000, 0.000000000000000000, 1.000000000000000000 ) ) ;
#1771 = CARTESIAN_POINT ( 'NONE',  ( 17.99999999999999645, 78.24875198621454331, 3.965855704038781404 ) ) ;
#1772 = CARTESIAN_POINT ( 'NONE',  ( 10.00000000000000000, 46.81368534415484106, -10.88017736071110342 ) ) ;
#1773 = EDGE_CURVE ( 'NONE', #35739, #94992, #27891, .T. ) ;
#1774 = CARTESIAN_POINT ( 'NONE',  ( 1.472469842513823179, 20.59226448433411960, -4.923371831947296329 ) ) ;
#1775 = LINE ( 'NONE', #9251, #65321 ) ;
#1776 = VERTEX_POINT ( 'NONE', #64034 ) ;
#1777 = DIRECTION ( 'NONE',  ( 1.000000000000000000, -5.818595309480552676E-17, 0.000000000000000000 ) ) ;
#1778 = VERTEX_POINT ( 'NONE', #71570 ) ;
#1779 = CARTESIAN_POINT ( 'NONE',  ( 7.361572987183170547, 7.050597817667451750, 9.846743663894590881 ) ) ;
#1780 = VERTEX_POINT ( 'NONE', #21394 ) ;
#1781 = CARTESIAN_POINT ( 'NONE',  ( 13.79529636645030344, 23.26208216824730002, 14.16423886937410614 ) ) ;
#1782 = CARTESIAN_POINT ( 'NONE',  ( 1.472469842513823179, 26.42559781766745175, 4.923371831947296329 ) ) ;
#1783 = CARTESIAN_POINT ( 'NONE',  ( 19.42250999205614548, 45.98035201082150536, -5.440088680355545492 ) ) ;
#1785 = EDGE_CURVE ( 'NONE', #54884, #35492, #44377, .T. ) ;
#1784 = ORIENTED_EDGE ( 'NONE', *, *, #75473, .F. ) ;
#1786 = STYLED_ITEM ( 'NONE', ( #71662 ), #61780 ) ;
#1787 = CARTESIAN_POINT ( 'NONE',  ( -0.8801773607110991993, 42.85535201082150536, -2.915334737309923874 ) ) ;
#1788 = CARTESIAN_POINT ( 'NONE',  ( 14.75001642003105395, 0.04962894700187066993, 0.3071237627330382636 ) ) ;
#1789 = CARTESIAN_POINT ( 'NONE',  ( -6.408140936763246032, -6.709698663402908991, -11.09922568453594316 ) ) ;
#1790 = ORIENTED_EDGE ( 'NONE', *, *, #67877, .F. ) ;
#1791 = CARTESIAN_POINT ( 'NONE',  ( 15.44008868035555793, 46.39701867748817676, -9.422509992056140149 ) ) ;
#1792 = VECTOR ( 'NONE', #20290, 1000.000000000000000 ) ;
#1793 = CARTESIAN_POINT ( 'NONE',  ( 10.00000000000000000, 10.55374883491396787, -14.16423886937410082 ) ) ;
#1794 = MECHANICAL_DESIGN_GEOMETRIC_PRESENTATION_REPRESENTATION (  '', ( #87976 ), #62411 ) ;
#1795 = VERTEX_POINT ( 'NONE', #12892 ) ;
#1796 = CARTESIAN_POINT ( 'NONE',  ( -1.099225684535947600, 28.70696800326375353, -6.408140936763238038 ) ) ;
#1797 = CARTESIAN_POINT ( 'NONE',  ( 10.00000000000000000, 4.758931151000784787, -9.846743663894594434 ) ) ;
#1798 = CARTESIAN_POINT ( 'NONE',  ( 19.42250999205614548, 5.980352010821504471, -5.440088680355545492 ) ) ;
#1799 = CARTESIAN_POINT ( 'NONE',  ( -0.5000000000000073275, 80.99999999999994316, 0.000000000000000000 ) ) ;
#1800 = CARTESIAN_POINT ( 'NONE',  ( 14.92337183194729988, 14.34226448433411782, -8.527530157486177487 ) ) ;
#1801 = CARTESIAN_POINT ( 'NONE',  ( 20.88017736071110164, 50.35535201082151247, 2.915334737309930979 ) ) ;
#1802 = ORIENTED_EDGE ( 'NONE', *, *, #84904, .T. ) ;
#1803 = CARTESIAN_POINT ( 'NONE',  ( 10.00000000000000000, 62.87363466993042493, -12.81628187352647608 ) ) ;
#1804 = CARTESIAN_POINT ( 'NONE',  ( 19.42250999205614193, 55.14701867748817676, 5.440088680355555262 ) ) ;
#1805 = CARTESIAN_POINT ( 'NONE',  ( -4.249999999999994671, 43.00000000000000000, -6.500000000000000888 ) ) ;
#1806 = DIRECTION ( 'NONE',  ( 1.000000000000000000, 0.000000000000000000, 0.000000000000000000 ) ) ;
#1807 = CARTESIAN_POINT ( 'NONE',  ( 10.00000000000000178, 59.31368534415484106, 10.88017736071110342 ) ) ;
#1808 = CARTESIAN_POINT ( 'NONE',  ( 0.6178305044545818747, 8.498634669930421381, -9.382169495545419124 ) ) ;
#1809 = DIRECTION ( 'NONE',  ( 0.000000000000000000, -1.000000000000000000, 0.000000000000000000 ) ) ;
#1810 = EDGE_CURVE ( 'NONE', #65059, #16083, #5417, .T. ) ;
#1811 = CARTESIAN_POINT ( 'NONE',  ( 5.076628168052704559, 25.17559781766745175, -8.527530157486179263 ) ) ;
#1812 = CARTESIAN_POINT ( 'NONE',  ( 18.72515096720568906, 36.07228050351032778, -6.500000000000007105 ) ) ;
#1813 = CARTESIAN_POINT ( 'NONE',  ( 6.204703633549690345, 5.762082168247301794, -14.16423886937410259 ) ) ;
#1814 = CARTESIAN_POINT ( 'NONE',  ( 2.791683348922240793, 16.63393115100078745, 7.208316651077764092 ) ) ;
#1815 = CARTESIAN_POINT ( 'NONE',  ( 19.38216949554541202, 20.99863466993042138, 9.382169495545424454 ) ) ;
#1816 = CARTESIAN_POINT ( 'NONE',  ( 10.00000000000000178, 70.00000000000000000, 0.000000000000000000 ) ) ;
#1817 = CARTESIAN_POINT ( 'NONE',  ( 20.88017736071110519, 55.56368534415484817, 2.639326808657452039E-16 ) ) ;
#1818 = CARTESIAN_POINT ( 'NONE',  ( 5.076628168052704559, 65.17559781766745175, -8.527530157486179263 ) ) ;
#1819 = AXIS2_PLACEMENT_3D ( 'NONE', #37872, #98390, #30336 ) ;
#1820 = STYLED_ITEM ( 'NONE', ( #65871 ), #39060 ) ;
#1821 = CARTESIAN_POINT ( 'NONE',  ( -8.000000000000000000, 41.24999999999999289, 6.250000000000000000 ) ) ;
#1822 = EDGE_CURVE ( 'NONE', #51220, #2779, #49053, .T. ) ;
#1823 = CARTESIAN_POINT ( 'NONE',  ( 10.00000000000000000, 34.75893115100078745, -9.846743663894594434 ) ) ;
#1824 = CARTESIAN_POINT ( 'NONE',  ( 19.84674366389459266, 28.30059781766745886, 2.638427012816836559 ) ) ;
#1825 = CARTESIAN_POINT ( 'NONE',  ( 12.91533473730992121, 14.52201867748817143, 10.88017736071110164 ) ) ;
#1826 = CARTESIAN_POINT ( 'NONE',  ( 16.40814093676323893, 15.79030133659708746, 11.09922568453595026 ) ) ;
#1827 = CARTESIAN_POINT ( 'NONE',  ( 18.52753015748618282, 18.92559781766745175, -4.923371831947291888 ) ) ;
#1828 = SHAPE_REPRESENTATION_RELATIONSHIP ( 'NONE' , 'NONE' ,  #19841, #54890 ) ;
#1829 = CARTESIAN_POINT ( 'NONE',  ( -10.00219152607943407, 88.91691738930971667, 5.623636179944063507 ) ) ;
#1830 = VECTOR ( 'NONE', #23097, 1000.000000000000000 ) ;
#1831 = CARTESIAN_POINT ( 'NONE',  ( 19.42250999205614548, 20.98035201082150891, -5.440088680355545492 ) ) ;
#1832 = CARTESIAN_POINT ( 'NONE',  ( 5.679566525943226196, -28.64346213806842556, 2.750000000000001332 ) ) ;
#1834 = CARTESIAN_POINT ( 'NONE',  ( 20.88017736071110875, 15.77201867748817143, -2.915334737309920765 ) ) ;
#1833 = CARTESIAN_POINT ( 'NONE',  ( 0.1532563361054083140, 46.00893115100079456, 1.131784320476157264E-15 ) ) ;
#1835 = CARTESIAN_POINT ( 'NONE',  ( 20.88017736071110875, 40.77201867748818387, -2.915334737309920765 ) ) ;
#1837 = CARTESIAN_POINT ( 'NONE',  ( -0.2418659066527494572, 19.26028685723174405, -6.114288769123083611 ) ) ;
#1836 = CARTESIAN_POINT ( 'NONE',  ( 0.5774900079438607392, 13.48035201082150358, 5.440088680355550821 ) ) ;
#1838 = CARTESIAN_POINT ( 'NONE',  ( 0.1532563361054100626, 20.80059781766744464, -2.638427012816831230 ) ) ;
#1839 = CARTESIAN_POINT ( 'NONE',  ( 1.472469842513823179, 35.59226448433412315, -4.923371831947296329 ) ) ;
#1840 = LINE ( 'NONE', #10798, #58539 ) ;
#1841 = CARTESIAN_POINT ( 'NONE',  ( 19.72487221294571569, 30.71833443783938122, -6.499999999999989342 ) ) ;
#1842 = CARTESIAN_POINT ( 'NONE',  ( 1.472469842513823179, 65.59226448433412315, -4.923371831947296329 ) ) ;
#1843 = CARTESIAN_POINT ( 'NONE',  ( 10.00000000000000000, 0.5537488349139675359, -14.16423886937410082 ) ) ;
#1844 = CARTESIAN_POINT ( 'NONE',  ( 13.79529636645031943, 30.34541550158063927, -14.16423886937409904 ) ) ;
#1845 =( GEOMETRIC_REPRESENTATION_CONTEXT ( 3 ) GLOBAL_UNCERTAINTY_ASSIGNED_CONTEXT ( ( #55344 ) ) GLOBAL_UNIT_ASSIGNED_CONTEXT ( ( #13017, #80038, #42063 ) ) REPRESENTATION_CONTEXT ( 'NONE', 'WORKASPACE' ) );
#1846 = CARTESIAN_POINT ( 'NONE',  ( 19.84674366389459266, 33.30059781766744464, 2.638427012816836559 ) ) ;
#1847 = ADVANCED_FACE ( 'NONE', ( #82370 ), #1554, .T. ) ;
#1848 = CARTESIAN_POINT ( 'NONE',  ( -15.41943733314634635, -0.03417435944610275333, 4.256565371896233962 ) ) ;
#1849 = CARTESIAN_POINT ( 'NONE',  ( 10.00000000000000178, 58.05374883491397497, 14.16423886937410082 ) ) ;
#1850 = CARTESIAN_POINT ( 'NONE',  ( 18.52753015748618282, 18.92559781766745175, -4.923371831947291888 ) ) ;
#1852 = CARTESIAN_POINT ( 'NONE',  ( -9.483770294663381506, 88.32858231846628883, -5.216041430090311515 ) ) ;
#1851 = DIRECTION ( 'NONE',  ( -0.4771587602596096822, 0.000000000000000000, 0.8788171126619647167 ) ) ;
#1853 = CARTESIAN_POINT ( 'NONE',  ( 20.88017736071110164, 45.35535201082149115, 2.915334737309930979 ) ) ;
#1854 = CARTESIAN_POINT ( 'NONE',  ( -8.564643372776448160, 0.5000000000000004441, -12.31449893000752205 ) ) ;
#1855 = EDGE_CURVE ( 'NONE', #77981, #81201, #86570, .T. ) ;
#1856 = CARTESIAN_POINT ( 'NONE',  ( 20.88017736071110519, 20.56368534415484106, 2.639326808657452039E-16 ) ) ;
#1857 = VECTOR ( 'NONE', #90994, 1000.000000000000000 ) ;
#1858 = CARTESIAN_POINT ( 'NONE',  ( 13.43411237798105340, 50.58196800326375353, 12.81628187352647963 ) ) ;
#1859 = CARTESIAN_POINT ( 'NONE',  ( 19.38216949554541202, 15.99863466993042138, 9.382169495545424454 ) ) ;
#1860 = CARTESIAN_POINT ( 'NONE',  ( 1.472469842513823179, 20.59226448433411960, -4.923371831947296329 ) ) ;
#1861 = ORIENTED_EDGE ( 'NONE', *, *, #32, .T. ) ;
#1862 = DIRECTION ( 'NONE',  ( -0.000000000000000000, -0.000000000000000000, -1.000000000000000000 ) ) ;
#1863 = CARTESIAN_POINT ( 'NONE',  ( 0.000000000000000000, 0.5000000000000004441, 0.000000000000000000 ) ) ;
#1864 = CARTESIAN_POINT ( 'NONE',  ( 13.79529636645031943, 50.34541550158064638, -14.16423886937409904 ) ) ;
#1865 = CARTESIAN_POINT ( 'NONE',  ( -2.266590686148945544, 21.38708216824730357, -7.082119434687050408 ) ) ;
#1866 = CARTESIAN_POINT ( 'NONE',  ( 19.42250999205614193, 20.14701867748817321, 5.440088680355555262 ) ) ;
#1867 = CARTESIAN_POINT ( 'NONE',  ( 12.91533473730993009, 31.60535201082150891, -10.88017736071109987 ) ) ;
#1868 = CARTESIAN_POINT ( 'NONE',  ( -0.9082943533635161604, 4.683954948888111413E-16, -14.47152380945586359 ) ) ;
#1869 = CARTESIAN_POINT ( 'NONE',  ( -1.983216688681034068, 15.00000000000000000, 14.11131997956736406 ) ) ;
#1870 = CARTESIAN_POINT ( 'NONE',  ( 2.791683348922240793, 1.633931151000784565, 7.208316651077764092 ) ) ;
#1871 = CARTESIAN_POINT ( 'NONE',  ( 1.274849032794231007, 33.57228050351031357, 6.499999999999895195 ) ) ;
#1872 = CARTESIAN_POINT ( 'NONE',  ( 14.92337183194729988, 19.34226448433411960, -8.527530157486177487 ) ) ;
#1873 = CARTESIAN_POINT ( 'NONE',  ( 5.419894505350487002, 0.5000000000000004441, 13.98659156302462314 ) ) ;
#1874 = AXIS2_PLACEMENT_3D ( 'NONE', #4581, #86104, #3112 ) ;
#1875 = CARTESIAN_POINT ( 'NONE',  ( 19.84674366389459621, 18.50893115100078745, 7.409399052514197653E-17 ) ) ;
#1876 = CARTESIAN_POINT ( 'NONE',  ( 7.361572987183169658, 34.96726448433411605, -9.846743663894592657 ) ) ;
#1877 = CARTESIAN_POINT ( 'NONE',  ( 2.035157376598824452, 8.688685344154839285, 7.964842623401179544 ) ) ;
#1878 = B_SPLINE_CURVE_WITH_KNOTS ( 'NONE', 3,
 ( #8995, #40988, #86487, #77985, #32481, #31974 ),
 .UNSPECIFIED., .F., .F.,
 ( 4, 2, 4 ),
 ( 0.000000000000000000, 0.0002626113303184896258, 0.0005252226606369792515 ),
 .UNSPECIFIED. ) ;
#1879 = CARTESIAN_POINT ( 'NONE',  ( 6.565887622018943937, 30.16530133659708568, 12.81628187352647430 ) ) ;
#1880 = CARTESIAN_POINT ( 'NONE',  ( 10.00000000000000178, 59.31368534415484106, 10.88017736071110342 ) ) ;
#1883 = EDGE_CURVE ( 'NONE', #35180, #37045, #27056, .T. ) ;
#1882 = CARTESIAN_POINT ( 'NONE',  ( 7.361572987183169658, 9.967264484334119601, -9.846743663894592657 ) ) ;
#1881 = CARTESIAN_POINT ( 'NONE',  ( -0.3689425029237881626, 52.42874883491396076, 10.36894250292379027 ) ) ;
#1884 = CARTESIAN_POINT ( 'NONE',  ( 0.000000000000000000, 15.00000000000000000, 0.000000000000000000 ) ) ;
#1885 = CARTESIAN_POINT ( 'NONE',  ( 5.076628168052704559, 50.17559781766745886, -8.527530157486179263 ) ) ;
#1887 = CARTESIAN_POINT ( 'NONE',  ( 24.16423886937410614, 14.51208216824730179, -3.795296366450302550 ) ) ;
#1886 = CARTESIAN_POINT ( 'NONE',  ( 12.63842701281683034, 37.46726448433411605, 9.846743663894596210 ) ) ;
#1888 = CARTESIAN_POINT ( 'NONE',  ( 20.36894250292379382, 13.67874883491396965, 10.36894250292379205 ) ) ;
#1889 = CARTESIAN_POINT ( 'NONE',  ( 7.084665262690076126, 44.10535201082151247, 10.88017736071109987 ) ) ;
#1890 = CARTESIAN_POINT ( 'NONE',  ( 20.88017736071110519, 15.56368534415483751, 2.639326808657452039E-16 ) ) ;
#1891 = EDGE_CURVE ( 'NONE', #46560, #16030, #51044, .T. ) ;
#1892 = CARTESIAN_POINT ( 'NONE',  ( 17.96484262340118221, 46.18868534415484106, -7.964842623401177768 ) ) ;
#1893 = CARTESIAN_POINT ( 'NONE',  ( 12.91533473730993009, 26.60535201082150536, -10.88017736071109987 ) ) ;
#1894 = ORIENTED_EDGE ( 'NONE', *, *, #66949, .F. ) ;
#1895 = CARTESIAN_POINT ( 'NONE',  ( 13.43411237798105340, 35.58196800326375353, 12.81628187352647963 ) ) ;
#1896 = CARTESIAN_POINT ( 'NONE',  ( 20.88017736071110875, 40.77201867748818387, -2.915334737309920765 ) ) ;
#1897 = AXIS2_PLACEMENT_3D ( 'NONE', #81738, #73253, #28746 ) ;
#1898 = VERTEX_POINT ( 'NONE', #63551 ) ;
#1899 = CARTESIAN_POINT ( 'NONE',  ( -2.816281873526473856, 64.33196800326376774, 3.434112377981055619 ) ) ;
#1900 = CARTESIAN_POINT ( 'NONE',  ( 12.91533473730992121, 54.52201867748816255, 10.88017736071110164 ) ) ;
#1901 = VERTEX_POINT ( 'NONE', #73886 ) ;
#1902 = CARTESIAN_POINT ( 'NONE',  ( 17.96484262340118221, 54.93868534415484106, 7.964842623401181321 ) ) ;
#1903 =( NAMED_UNIT ( * ) SI_UNIT ( $, .STERADIAN. ) SOLID_ANGLE_UNIT ( ) );
#1904 = CARTESIAN_POINT ( 'NONE',  ( 19.84674366389459266, 8.300597817667453526, 2.638427012816836559 ) ) ;
#1905 = DIRECTION ( 'NONE',  ( -0.9961946980917462113, 0.08715574274765114371, 0.000000000000000000 ) ) ;
#1906 = CARTESIAN_POINT ( 'NONE',  ( 20.36894250292379382, 58.67874883491396076, 10.36894250292379205 ) ) ;
#1907 = CARTESIAN_POINT ( 'NONE',  ( 19.42250999205614193, 60.14701867748817676, 5.440088680355555262 ) ) ;
#1908 = CARTESIAN_POINT ( 'NONE',  ( 0.1532563361054100626, 10.80059781766745175, -2.638427012816831230 ) ) ;
#1909 = CARTESIAN_POINT ( 'NONE',  ( 15.44008868035555793, 16.39701867748817321, -9.422509992056140149 ) ) ;
#1910 = CARTESIAN_POINT ( 'NONE',  ( 19.84674366389459621, 48.50893115100078745, 7.409399052514197653E-17 ) ) ;
#1911 = VERTEX_POINT ( 'NONE', #18561 ) ;
#1912 = CARTESIAN_POINT ( 'NONE',  ( 18.52753015748618282, 43.92559781766745175, -4.923371831947291888 ) ) ;
#1913 = CARTESIAN_POINT ( 'NONE',  ( 17.96484262340118221, 41.18868534415484106, -7.964842623401177768 ) ) ;
#1914 = CARTESIAN_POINT ( 'NONE',  ( 14.92337183194729633, 52.67559781766745175, 8.527530157486181039 ) ) ;
#1915 = CARTESIAN_POINT ( 'NONE',  ( 13.43411237798106583, 27.66530133659708568, -12.81628187352647252 ) ) ;
#1917 = CARTESIAN_POINT ( 'NONE',  ( 17.96484262340118221, 64.93868534415483396, 7.964842623401181321 ) ) ;
#1916 = SURFACE_SIDE_STYLE ('',( #70397 ) ) ;
#1918 = CARTESIAN_POINT ( 'NONE',  ( 20.88017736071110164, 50.35535201082151247, 2.915334737309930979 ) ) ;
#1919 = CARTESIAN_POINT ( 'NONE',  ( 17.08211943468705840, 55.13708216824731068, -12.26659068614894466 ) ) ;
#1920 = COLOUR_RGB ( '', 0.72549020, 0.75294118, 0.79215686) ;
#1921 = MECHANICAL_DESIGN_GEOMETRIC_PRESENTATION_REPRESENTATION (  '', ( #25810 ), #22686 ) ;
#1922 = CARTESIAN_POINT ( 'NONE',  ( 10.00000000000000000, 27.87363466993042138, -12.81628187352647608 ) ) ;
#1923 = DIRECTION ( 'NONE',  ( 1.000000000000000000, 0.000000000000000000, 0.000000000000000000 ) ) ;
#1924 = ORIENTED_EDGE ( 'NONE', *, *, #27259, .T. ) ;
#1925 = CARTESIAN_POINT ( 'NONE',  ( 13.43411237798106583, 32.66530133659708213, -12.81628187352647252 ) ) ;
#1926 = CARTESIAN_POINT ( 'NONE',  ( 2.035157376598822676, 27.43868534415483396, -7.964842623401177768 ) ) ;
#1927 = MECHANICAL_DESIGN_GEOMETRIC_PRESENTATION_REPRESENTATION (  '', ( #37028 ), #64114 ) ;
#1928 = ORIENTED_EDGE ( 'NONE', *, *, #82443, .T. ) ;
#1929 = CARTESIAN_POINT ( 'NONE',  ( 12.91533473730993009, 66.60535201082150536, -10.88017736071109987 ) ) ;
#1930 = COLOUR_RGB ( '', 0.31764706, 0.68627451, 0.89019608) ;
#1931 = CARTESIAN_POINT ( 'NONE',  ( 10.00000000000000000, 44.75893115100078745, -9.846743663894594434 ) ) ;
#1933 = CARTESIAN_POINT ( 'NONE',  ( 0.1532563361054100626, 35.80059781766745175, -2.638427012816831230 ) ) ;
#1932 = CARTESIAN_POINT ( 'NONE',  ( 14.92337183194729988, 9.342264484334119601, -8.527530157486177487 ) ) ;
#1934 = CARTESIAN_POINT ( 'NONE',  ( -8.000000000000003553, -0.02173251731167446035, 3.750000000000001776 ) ) ;
#1935 = CARTESIAN_POINT ( 'NONE',  ( -13.95692576442123034, 0.2301500530278518253, -5.331646315825927296 ) ) ;
#1936 = DIRECTION ( 'NONE',  ( -1.195561081071950118E-14, 8.738726411657103070E-15, 1.000000000000000000 ) ) ;
#1937 = LINE ( 'NONE', #47399, #8515 ) ;
#1938 = EDGE_CURVE ( 'NONE', #89108, #507, #93384, .T. ) ;
#1939 = CARTESIAN_POINT ( 'NONE',  ( 14.92337183194729633, 27.67559781766745530, 8.527530157486181039 ) ) ;
#1940 = DIRECTION ( 'NONE',  ( 0.000000000000000000, 1.000000000000000000, 0.000000000000000000 ) ) ;
#1942 = EDGE_LOOP ( 'NONE', ( #82166, #11641, #33187, #89350, #49488, #32510 ) ) ;
#1941 = CARTESIAN_POINT ( 'NONE',  ( 1.472469842513823179, 45.59226448433412315, -4.923371831947296329 ) ) ;
#1943 = DIRECTION ( 'NONE',  ( -0.9588197348681947174, 0.000000000000000000, 0.2840153447039170387 ) ) ;
#1944 = CARTESIAN_POINT ( 'NONE',  ( 22.81628187352648496, 26.83196800326374998, -3.434112377981050290 ) ) ;
#1945 = CARTESIAN_POINT ( 'NONE',  ( 7.850000000000003197, 98.49999999999998579, -8.525133428036873795 ) ) ;
#1946 = CARTESIAN_POINT ( 'NONE',  ( 2.917880565312950480, 50.97041550158064638, -12.26659068614894821 ) ) ;
#1947 = CARTESIAN_POINT ( 'NONE',  ( 7.361572987183169658, 24.96726448433412315, -9.846743663894592657 ) ) ;
#1948 = DIRECTION ( 'NONE',  ( 0.000000000000000000, 1.000000000000000000, 0.000000000000000000 ) ) ;
#1949 = CARTESIAN_POINT ( 'NONE',  ( 20.36894250292379382, 38.67874883491396076, 10.36894250292379205 ) ) ;
#1950 = CARTESIAN_POINT ( 'NONE',  ( 2.791683348922237240, 65.38393115100078035, -7.208316651077763204 ) ) ;
#1951 = CARTESIAN_POINT ( 'NONE',  ( 10.00000000000000000, 55.55374883491396787, -14.16423886937410082 ) ) ;
#1952 = CARTESIAN_POINT ( 'NONE',  ( 2.917880565312948704, 27.63708216824730357, 12.26659068614894643 ) ) ;
#1954 = CARTESIAN_POINT ( 'NONE',  ( -45.72064753280899652, 104.7206091210568957, -5.189487810365704057 ) ) ;
#1953 = CARTESIAN_POINT ( 'NONE',  ( -2.266590686148945544, 36.38708216824730357, -7.082119434687050408 ) ) ;
#1955 = CARTESIAN_POINT ( 'NONE',  ( 13.61912076658542325, 15.00000000000000888, 5.334594295380997053 ) ) ;
#1957 = CARTESIAN_POINT ( 'NONE',  ( 7.361572987183170547, 62.05059781766745886, 9.846743663894590881 ) ) ;
#1956 = CARTESIAN_POINT ( 'NONE',  ( 4.221206346830829403, -3.619822760651511651, 2.500000000000000000 ) ) ;
#1958 = CARTESIAN_POINT ( 'NONE',  ( -0.8801773607110991993, 42.85535201082150536, -2.915334737309923874 ) ) ;
#1959 = CARTESIAN_POINT ( 'NONE',  ( 0.2751277870542909176, 64.36607318730132477, -6.499999999999992006 ) ) ;
#1960 = CARTESIAN_POINT ( 'NONE',  ( 10.00000000000000000, 34.75893115100078745, -9.846743663894594434 ) ) ;
#1961 = CARTESIAN_POINT ( 'NONE',  ( 19.38216949554541557, 57.24863466993042493, -9.382169495545420901 ) ) ;
#1962 = CARTESIAN_POINT ( 'NONE',  ( -7.082119434687044190, -2.362917831752693765, 12.26659068614894998 ) ) ;
#1963 = CARTESIAN_POINT ( 'NONE',  ( 19.84674366389459266, 48.71726448433413026, -2.638427012816827677 ) ) ;
#1964 = PLANE ( 'NONE',  #68910 ) ;
#1965 = AXIS2_PLACEMENT_3D ( 'NONE', #90045, #52540, #82549 ) ;
#1966 = EDGE_CURVE ( 'NONE', #30537, #86221, #95700, .T. ) ;
#1967 = ORIENTED_EDGE ( 'NONE', *, *, #84025, .F. ) ;
#1968 = CARTESIAN_POINT ( 'NONE',  ( -0.3689425029237881626, 17.42874883491397142, 10.36894250292379027 ) ) ;
#1969 = DIRECTION ( 'NONE',  ( 0.04361938736534638067, 0.000000000000000000, -0.9990482215818573541 ) ) ;
#1971 = CARTESIAN_POINT ( 'NONE',  ( -5.991992585808429972, 15.00000000000000000, -13.20401548210301357 ) ) ;
#1970 = CARTESIAN_POINT ( 'NONE',  ( 1.780824192092501423, 0.5000000000000004441, -14.89391369643513485 ) ) ;
#1972 = CARTESIAN_POINT ( 'NONE',  ( 12.91533473730993009, 11.60535201082150714, -10.88017736071109987 ) ) ;
#1973 = CARTESIAN_POINT ( 'NONE',  ( 22.81628187352647785, 11.41530133659708390, 3.434112377981063169 ) ) ;
#1974 = EDGE_CURVE ( 'NONE', #13755, #54264, #90903, .T. ) ;
#1975 = CARTESIAN_POINT ( 'NONE',  ( 0.1957200283969096621, 55.25733960839544068, 6.499999999999992006 ) ) ;
#1976 = CARTESIAN_POINT ( 'NONE',  ( 7.084665262690076126, 69.10535201082151957, 10.88017736071109987 ) ) ;
#1977 = CARTESIAN_POINT ( 'NONE',  ( 20.15039907845753220, 26.74884699246889141, 6.262539305110078836 ) ) ;
#1978 = CARTESIAN_POINT ( 'NONE',  ( 8.629999999999995453, 41.24999999999999289, 4.000000000000000000 ) ) ;
#1979 = DIRECTION ( 'NONE',  ( 1.257568779154408793E-17, 1.000000000000000000, -0.000000000000000000 ) ) ;
#1980 = CARTESIAN_POINT ( 'NONE',  ( 24.16423886937409904, 59.09541550158063217, 3.795296366450317205 ) ) ;
#1981 = CARTESIAN_POINT ( 'NONE',  ( 17.39651004071838969, 44.08210964143329846, -6.500000000000027534 ) ) ;
#1982 = CARTESIAN_POINT ( 'NONE',  ( 9.050000000000002487, 99.99999999999998579, -8.525133428036873795 ) ) ;
#1983 = CARTESIAN_POINT ( 'NONE',  ( 7.084665262690076126, 24.10535201082150181, 10.88017736071109987 ) ) ;
#1984 = CARTESIAN_POINT ( 'NONE',  ( 7.084665262690076126, 39.10535201082150536, 10.88017736071109987 ) ) ;
#1985 = CARTESIAN_POINT ( 'NONE',  ( -1.099225684535947600, 3.706968003263753531, -6.408140936763238038 ) ) ;
#1986 = CARTESIAN_POINT ( 'NONE',  ( 10.00000000000000178, 52.25893115100078745, 9.846743663894594434 ) ) ;
#1987 = CARTESIAN_POINT ( 'NONE',  ( 0.6178305044545838731, 59.74863466993041783, 9.382169495545420901 ) ) ;
#1988 = ORIENTED_EDGE ( 'NONE', *, *, #46418, .F. ) ;
#1989 = PRODUCT_DEFINITION_SHAPE ( 'NONE', 'NONE',  #98992 ) ;
#1990 = CARTESIAN_POINT ( 'NONE',  ( 20.88017736071110875, 25.77201867748816966, -2.915334737309920765 ) ) ;
#1991 = CARTESIAN_POINT ( 'NONE',  ( 13.43411237798105340, 35.58196800326375353, 12.81628187352647963 ) ) ;
#1992 = CARTESIAN_POINT ( 'NONE',  ( -1.319618665598680717E-31, 72.38931350946023713, 5.123507015312970481 ) ) ;
#1993 = VECTOR ( 'NONE', #29194, 1000.000000000000000 ) ;
#1994 = CARTESIAN_POINT ( 'NONE',  ( 1.472469842513823179, 66.42559781766745175, 4.923371831947296329 ) ) ;
#1995 = CARTESIAN_POINT ( 'NONE',  ( 0.5774900079438607392, 48.48035201082150536, 5.440088680355550821 ) ) ;
#1996 = CARTESIAN_POINT ( 'NONE',  ( 7.361572987183170547, 12.05059781766744997, 9.846743663894590881 ) ) ;
#1997 = CARTESIAN_POINT ( 'NONE',  ( 0.6178305044545818747, 33.49863466993042493, -9.382169495545419124 ) ) ;
#1998 = AXIS2_PLACEMENT_3D ( 'NONE', #63257, #93765, #25292 ) ;
#2000 = CARTESIAN_POINT ( 'NONE',  ( -19.89999999999999858, 92.00000000000000000, 8.000000000000000000 ) ) ;
#1999 = CARTESIAN_POINT ( 'NONE',  ( 4.559911319644449179, 57.23035201082150536, -9.422509992056141925 ) ) ;
#2001 = PRESENTATION_STYLE_ASSIGNMENT (( #23520 ) ) ;
#2002 = CARTESIAN_POINT ( 'NONE',  ( -2.816281873526473856, 59.33196800326374643, 3.434112377981055619 ) ) ;
#2003 = ORIENTED_EDGE ( 'NONE', *, *, #2547, .F. ) ;
#2004 = DIRECTION ( 'NONE',  ( 1.000000000000000000, 0.000000000000000000, 0.000000000000000000 ) ) ;
#2005 = CARTESIAN_POINT ( 'NONE',  ( 1.602071938427501063, 17.02224192338641373, -6.499999999999984901 ) ) ;
#2006 = CARTESIAN_POINT ( 'NONE',  ( 7.084665262690076126, 7.022018677488169658, -10.88017736071110164 ) ) ;
#2008 = CARTESIAN_POINT ( 'NONE',  ( -4.164238869374099039, 16.80374883491396787, 8.674139862899312516E-16 ) ) ;
#2007 = CARTESIAN_POINT ( 'NONE',  ( 10.00000000000000000, 42.87363466993042493, -12.81628187352647608 ) ) ;
#2009 = CARTESIAN_POINT ( 'NONE',  ( 0.1532563361054082862, 16.21726448433411960, 2.638427012816831674 ) ) ;
#2010 = CARTESIAN_POINT ( 'NONE',  ( 12.91533473730992121, 4.522018677488169658, 10.88017736071110164 ) ) ;
#2011 = CARTESIAN_POINT ( 'NONE',  ( 17.20831665107776587, 22.88393115100078745, 7.208316651077764980 ) ) ;
#2012 = CARTESIAN_POINT ( 'NONE',  ( 10.00000000000000178, 53.05374883491396787, 14.16423886937410082 ) ) ;
#2013 = ORIENTED_EDGE ( 'NONE', *, *, #91431, .T. ) ;
#2014 = MECHANICAL_DESIGN_GEOMETRIC_PRESENTATION_REPRESENTATION (  '', ( #72206 ), #89765 ) ;
#2015 = CARTESIAN_POINT ( 'NONE',  ( 12.00809552683958614, 0.5000000000000004441, -8.989195838243546177 ) ) ;
#2016 = EDGE_CURVE ( 'NONE', #38851, #45156, #79036, .T. ) ;
#2017 = CARTESIAN_POINT ( 'NONE',  ( 4.559911319644449179, 22.23035201082150536, -9.422509992056141925 ) ) ;
#2018 = CARTESIAN_POINT ( 'NONE',  ( 1.492507162822237499, 32.19955587570479594, -6.499999999999986677 ) ) ;
#2019 = VECTOR ( 'NONE', #11768, 999.9999999999998863 ) ;
#2020 = ORIENTED_EDGE ( 'NONE', *, *, #74478, .T. ) ;
#2021 = VERTEX_POINT ( 'NONE', #29367 ) ;
#2022 = CARTESIAN_POINT ( 'NONE',  ( 0.5774900079438590739, 17.64701867748817321, -5.440088680355550821 ) ) ;
#2023 = CARTESIAN_POINT ( 'NONE',  ( 19.42250999205614193, 15.14701867748817143, 5.440088680355555262 ) ) ;
#2024 = CARTESIAN_POINT ( 'NONE',  ( 1.472469842513823179, 51.42559781766745886, 4.923371831947296329 ) ) ;
#2025 = CARTESIAN_POINT ( 'NONE',  ( -2.816281873526473856, 54.33196800326376064, 3.434112377981055619 ) ) ;
#2026 = CARTESIAN_POINT ( 'NONE',  ( 20.10493008474205823, 64.71697413083879269, 6.336235997365761818 ) ) ;
#2028 = CARTESIAN_POINT ( 'NONE',  ( 22.26659068614894466, 13.88708216824730179, 7.082119434687054849 ) ) ;
#2027 = CARTESIAN_POINT ( 'NONE',  ( -9.402796353260987061, 14.49999999999999112, -11.68706210897776465 ) ) ;
#2029 = CARTESIAN_POINT ( 'NONE',  ( 4.559911319644449179, 22.23035201082150536, -9.422509992056141925 ) ) ;
#2030 = CARTESIAN_POINT ( 'NONE',  ( 12.91533473730992121, 4.522018677488170546, 10.88017736071110164 ) ) ;
#2031 = CARTESIAN_POINT ( 'NONE',  ( 5.076628168052703671, 56.84226448433412315, 8.527530157486179263 ) ) ;
#2032 = DIRECTION ( 'NONE',  ( 1.000000000000000000, 0.000000000000000000, 0.000000000000000000 ) ) ;
#2033 = CARTESIAN_POINT ( 'NONE',  ( 17.20831665107776587, 37.88393115100078745, 7.208316651077764980 ) ) ;
#2034 = AXIS2_PLACEMENT_3D ( 'NONE', #76436, #7952, #38447 ) ;
#2035 = CARTESIAN_POINT ( 'NONE',  ( 19.84674366389459621, 3.508931151000785231, 7.409399052514197653E-17 ) ) ;
#2036 = CARTESIAN_POINT ( 'NONE',  ( -4.923371831947302546, 25.17559781766745530, -8.527530157486173934 ) ) ;
#2037 = EDGE_LOOP ( 'NONE', ( #97126, #36813, #40941, #13080 ) ) ;
#2038 = CARTESIAN_POINT ( 'NONE',  ( 17.96484262340118221, 6.188685344154836621, -7.964842623401177768 ) ) ;
#2039 = CARTESIAN_POINT ( 'NONE',  ( 10.00000000000000178, 2.258931151000784787, 9.846743663894594434 ) ) ;
#2040 = CARTESIAN_POINT ( 'NONE',  ( 3.591859063236763294, 3.290301336597087012, -11.09922568453595026 ) ) ;
#2042 = CARTESIAN_POINT ( 'NONE',  ( 7.084665262690076126, 47.02201867748818387, -10.88017736071110164 ) ) ;
#2041 = CARTESIAN_POINT ( 'NONE',  ( 19.42250999205614193, 40.14701867748817676, 5.440088680355555262 ) ) ;
#2044 = CARTESIAN_POINT ( 'NONE',  ( 3.591859063236761518, 44.95696800326376064, 11.09922568453594849 ) ) ;
#2043 = CARTESIAN_POINT ( 'NONE',  ( -0.8801773607110991993, 12.85535201082150358, -2.915334737309923874 ) ) ;
#2045 = CARTESIAN_POINT ( 'NONE',  ( 24.16423886937409904, 19.09541550158063927, 3.795296366450317205 ) ) ;
#2046 = CIRCLE ( 'NONE', #96235, 14.49999999999999822 ) ;
#2047 = CARTESIAN_POINT ( 'NONE',  ( 22.81628187352647785, 46.41530133659708213, 3.434112377981063169 ) ) ;
#2048 = ORIENTED_EDGE ( 'NONE', *, *, #64961, .T. ) ;
#2049 = CARTESIAN_POINT ( 'NONE',  ( 0.1532563361054100626, 55.80059781766745175, -2.638427012816831230 ) ) ;
#2050 = CARTESIAN_POINT ( 'NONE',  ( 19.42250999205614548, 20.98035201082150891, -5.440088680355545492 ) ) ;
#2051 = CARTESIAN_POINT ( 'NONE',  ( 17.96484262340118221, 26.18868534415483396, -7.964842623401177768 ) ) ;
#2052 = ORIENTED_EDGE ( 'NONE', *, *, #45045, .T. ) ;
#2053 = CARTESIAN_POINT ( 'NONE',  ( -0.8801773607111008646, 68.27201867748817676, 2.915334737309923430 ) ) ;
#2054 =( NAMED_UNIT ( * ) PLANE_ANGLE_UNIT ( ) SI_UNIT ( $, .RADIAN. ) );
#2055 = CARTESIAN_POINT ( 'NONE',  ( 20.15039907845753930, 70.00000000000000000, 6.262539305110068177 ) ) ;
#2056 = CARTESIAN_POINT ( 'NONE',  ( 2.791683348922237240, 10.38393115100078390, -7.208316651077763204 ) ) ;
#2057 = CARTESIAN_POINT ( 'NONE',  ( 2.791683348922237240, 0.3839311510007847872, -7.208316651077763204 ) ) ;
#2058 = EDGE_CURVE ( 'NONE', #58154, #8981, #69489, .T. ) ;
#2060 = CARTESIAN_POINT ( 'NONE',  ( 10.58840669699852199, -98.14374106289703548, -4.000000000000000000 ) ) ;
#2059 = CARTESIAN_POINT ( 'NONE',  ( 10.00000000000000178, 54.31368534415484106, 10.88017736071110342 ) ) ;
#2061 = CARTESIAN_POINT ( 'NONE',  ( 7.084665262690076126, 69.10535201082151957, 10.88017736071109987 ) ) ;
#2064 = ORIENTED_EDGE ( 'NONE', *, *, #89439, .F. ) ;
#2063 = VECTOR ( 'NONE', #88908, 1000.000000000000000 ) ;
#2062 = CARTESIAN_POINT ( 'NONE',  ( 7.361572987183170547, 7.050597817667451750, 9.846743663894590881 ) ) ;
#2065 = LINE ( 'NONE', #63025, #37451 ) ;
#2066 = CARTESIAN_POINT ( 'NONE',  ( 2.791683348922240793, 61.63393115100079456, 7.208316651077764092 ) ) ;
#2067 = ORIENTED_EDGE ( 'NONE', *, *, #18669, .T. ) ;
#2068 = ORIENTED_EDGE ( 'NONE', *, *, #24511, .F. ) ;
#2069 = DIRECTION ( 'NONE',  ( -0.02177529129993028070, -0.9997628902338809853, 0.000000000000000000 ) ) ;
#2070 = CARTESIAN_POINT ( 'NONE',  ( 10.00000000000000000, 10.55374883491396787, -14.16423886937410082 ) ) ;
#2071 = VECTOR ( 'NONE', #29687, 1000.000000000000000 ) ;
#2072 = CARTESIAN_POINT ( 'NONE',  ( 13.43411237798106583, 57.66530133659708923, -12.81628187352647252 ) ) ;
#2073 =( GEOMETRIC_REPRESENTATION_CONTEXT ( 3 ) GLOBAL_UNCERTAINTY_ASSIGNED_CONTEXT ( ( #64491 ) ) GLOBAL_UNIT_ASSIGNED_CONTEXT ( ( #85888, #78872, #74305 ) ) REPRESENTATION_CONTEXT ( 'NONE', 'WORKASPACE' ) );
#2074 = CARTESIAN_POINT ( 'NONE',  ( 20.36894250292379382, 3.678748834913967869, 10.36894250292379205 ) ) ;
#2075 = CARTESIAN_POINT ( 'NONE',  ( 17.08211943468705840, 20.13708216824730357, -12.26659068614894466 ) ) ;
#2076 = CARTESIAN_POINT ( 'NONE',  ( 19.72487221294570858, 56.86607318730075633, 6.500000000000000888 ) ) ;
#2077 = CARTESIAN_POINT ( 'NONE',  ( 13.82671409943293739, -0.03417435944610275333, 3.447387012295318076 ) ) ;
#2078 = CARTESIAN_POINT ( 'NONE',  ( -0.8801773607111009756, 23.06368534415484106, 1.068504757029289695E-15 ) ) ;
#2079 = ORIENTED_EDGE ( 'NONE', *, *, #57225, .T. ) ;
#2081 = STYLED_ITEM ( 'NONE', ( #69841 ), #76215 ) ;
#2080 = CARTESIAN_POINT ( 'NONE',  ( 0.1532563361054083140, 1.008931151000784787, 1.131784320476157264E-15 ) ) ;
#2082 = CARTESIAN_POINT ( 'NONE',  ( 22.81628187352647785, 26.62363466993042138, 6.195893100308588602E-16 ) ) ;
#2083 = CARTESIAN_POINT ( 'NONE',  ( 10.00000000000000000, 34.75893115100078745, -9.846743663894594434 ) ) ;
#2084 = CYLINDRICAL_SURFACE ( 'NONE', #21834, 0.2500000000000002220 ) ;
#2085 = CARTESIAN_POINT ( 'NONE',  ( 10.00000000000000000, 12.87363466993042138, -12.81628187352647608 ) ) ;
#2086 = CARTESIAN_POINT ( 'NONE',  ( -18.89999999999999147, 91.25000000000000000, -7.750000000000000000 ) ) ;
#2087 = CARTESIAN_POINT ( 'NONE',  ( 19.84674366389459621, 23.50893115100078390, 7.409399052514197653E-17 ) ) ;
#2088 = CARTESIAN_POINT ( 'NONE',  ( 10.00000000000000178, 12.25893115100078568, 9.846743663894594434 ) ) ;
#2089 = EDGE_CURVE ( 'NONE', #62241, #76019, #83370, .T. ) ;
#2090 = EDGE_LOOP ( 'NONE', ( #32914, #87501, #15357, #45766, #28426, #93141 ) ) ;
#2091 = ORIENTED_EDGE ( 'NONE', *, *, #77384, .F. ) ;
#2092 = CARTESIAN_POINT ( 'NONE',  ( 0.5774900079438607392, 38.48035201082150536, 5.440088680355550821 ) ) ;
#2093 = CARTESIAN_POINT ( 'NONE',  ( -4.164238869374099039, 26.80374883491397142, 8.674139862899312516E-16 ) ) ;
#2094 = CARTESIAN_POINT ( 'NONE',  ( 7.361572987183169658, 34.96726448433411605, -9.846743663894592657 ) ) ;
#2095 = CARTESIAN_POINT ( 'NONE',  ( 1.472469842513823179, 15.59226448433411960, -4.923371831947296329 ) ) ;
#2097 = CARTESIAN_POINT ( 'NONE',  ( -11.12340613366069419, 89.95527085539235657, 6.571742733942877557 ) ) ;
#2096 = CARTESIAN_POINT ( 'NONE',  ( -1.099225684535947600, 53.70696800326376064, -6.408140936763238038 ) ) ;
#2098 = CARTESIAN_POINT ( 'NONE',  ( 2.035157376598824452, 33.68868534415484106, 7.964842623401179544 ) ) ;
#2099 = EDGE_CURVE ( 'NONE', #84532, #89907, #23376, .T. ) ;
#2100 = CARTESIAN_POINT ( 'NONE',  ( -0.1503990784575328643, 70.00000000000000000, 6.262539305110068177 ) ) ;
#2101 = CARTESIAN_POINT ( 'NONE',  ( 16.40814093676323893, 20.79030133659708923, 11.09922568453595026 ) ) ;
#2102 = CARTESIAN_POINT ( 'NONE',  ( 22.81628187352647785, 16.41530133659708923, 3.434112377981063169 ) ) ;
#2103 = CARTESIAN_POINT ( 'NONE',  ( 12.63842701281683922, 34.55059781766745886, -9.846743663894590881 ) ) ;
#2104 = CARTESIAN_POINT ( 'NONE',  ( 10.88017736071110164, 0.3553520108215071915, 2.915334737309921209 ) ) ;
#2105 = CARTESIAN_POINT ( 'NONE',  ( 10.00000000000000178, 45.37363466993041783, 12.81628187352647608 ) ) ;
#2106 = FILL_AREA_STYLE ('',( #17588 ) ) ;
#2108 = FACE_OUTER_BOUND ( 'NONE', #53525, .T. ) ;
#2107 = CARTESIAN_POINT ( 'NONE',  ( 10.00000000000000000, 56.81368534415484106, -10.88017736071110342 ) ) ;
#2109 = CARTESIAN_POINT ( 'NONE',  ( -10.82635109560346898, -96.00292546281778527, 4.000000000000000000 ) ) ;
#2110 = DIRECTION ( 'NONE',  ( 3.375077994860475883E-14, 0.000000000000000000, 1.000000000000000000 ) ) ;
#2111 = CARTESIAN_POINT ( 'NONE',  ( 15.44008868035555793, 51.39701867748816966, -9.422509992056140149 ) ) ;
#2113 = CARTESIAN_POINT ( 'NONE',  ( 20.88017736071110875, 55.77201867748816966, -2.915334737309920765 ) ) ;
#2112 = VECTOR ( 'NONE', #8669, 1000.000000000000000 ) ;
#2114 = CARTESIAN_POINT ( 'NONE',  ( -11.62719953690074881, 14.49999999999999112, 9.476720473301769587 ) ) ;
#2115 = CARTESIAN_POINT ( 'NONE',  ( 5.963430220938279902, 13.02164270246083966, -10.32896413005680181 ) ) ;
#2116 = CARTESIAN_POINT ( 'NONE',  ( 7.084665262690076126, 14.10535201082150358, 10.88017736071109987 ) ) ;
#2117 = CARTESIAN_POINT ( 'NONE',  ( 5.076628168052704559, 60.17559781766745175, -8.527530157486179263 ) ) ;
#2119 = CARTESIAN_POINT ( 'NONE',  ( -10.29278075765157041, 44.03034551814236153, 0.000000000000000000 ) ) ;
#2118 = CARTESIAN_POINT ( 'NONE',  ( 4.559911319644449179, 18.89701867748817321, 9.422509992056141925 ) ) ;
#2120 = PRESENTATION_STYLE_ASSIGNMENT (( #63075 ) ) ;
#2121 = CARTESIAN_POINT ( 'NONE',  ( 22.81628187352648496, 21.83196800326374643, -3.434112377981050290 ) ) ;
#2122 = VERTEX_POINT ( 'NONE', #45871 ) ;
#2123 = CARTESIAN_POINT ( 'NONE',  ( 17.96484262340118221, 54.93868534415484106, 7.964842623401181321 ) ) ;
#2124 = CARTESIAN_POINT ( 'NONE',  ( 5.076628168052704559, 40.17559781766745175, -8.527530157486179263 ) ) ;
#2126 = CARTESIAN_POINT ( 'NONE',  ( 19.80427997160309062, 47.75733960839543357, -6.499999999999980460 ) ) ;
#2125 = CARTESIAN_POINT ( 'NONE',  ( 22.81628187352648496, 1.831968003263753753, -3.434112377981050290 ) ) ;
#2127 = CARTESIAN_POINT ( 'NONE',  ( 19.42250999205614548, 15.98035201082150714, -5.440088680355545492 ) ) ;
#2128 = CARTESIAN_POINT ( 'NONE',  ( 19.42250999205614548, 40.98035201082150536, -5.440088680355545492 ) ) ;
#2129 = CARTESIAN_POINT ( 'NONE',  ( 17.08211943468705840, 55.13708216824731068, -12.26659068614894466 ) ) ;
#2130 = CARTESIAN_POINT ( 'NONE',  ( 10.00000000000000178, 37.25893115100078745, 9.846743663894594434 ) ) ;
#2131 = CARTESIAN_POINT ( 'NONE',  ( 15.44008868035555793, 56.39701867748817676, -9.422509992056140149 ) ) ;
#2132 = DIRECTION ( 'NONE',  ( 0.000000000000000000, -1.000000000000000000, 0.000000000000000000 ) ) ;
#2133 = CARTESIAN_POINT ( 'NONE',  ( -4.164238869374098151, 11.59541550158063217, -3.795296366450310543 ) ) ;
#2134 = EDGE_CURVE ( 'NONE', #92052, #81238, #82877, .T. ) ;
#2135 = CARTESIAN_POINT ( 'NONE',  ( 5.803070148808322948, 4.011383936018713867E-16, -13.28812917035388175 ) ) ;
#2136 = DIRECTION ( 'NONE',  ( 0.000000000000000000, 1.000000000000000000, 0.000000000000000000 ) ) ;
#2137 = VERTEX_POINT ( 'NONE', #75867 ) ;
#2138 = ORIENTED_EDGE ( 'NONE', *, *, #4766, .T. ) ;
#2139 = CARTESIAN_POINT ( 'NONE',  ( -2.266590686148945544, 31.38708216824730002, -7.082119434687050408 ) ) ;
#2140 = CARTESIAN_POINT ( 'NONE',  ( -0.3689425029237881626, 37.42874883491396787, 10.36894250292379027 ) ) ;
#2141 = CARTESIAN_POINT ( 'NONE',  ( 1.472469842513823179, 5.592264484334118713, -4.923371831947296329 ) ) ;
#2142 = CARTESIAN_POINT ( 'NONE',  ( 5.076628168052703671, 66.84226448433412315, 8.527530157486179263 ) ) ;
#2143 = CARTESIAN_POINT ( 'NONE',  ( 19.72487221294570858, 70.00000000000000000, -6.000000000000000000 ) ) ;
#2145 = CARTESIAN_POINT ( 'NONE',  ( -2.816281873526471635, 38.91530133659708213, -3.434112377981056508 ) ) ;
#2144 = CARTESIAN_POINT ( 'NONE',  ( 0.5774900079438590739, 62.64701867748817676, -5.440088680355550821 ) ) ;
#2146 = CARTESIAN_POINT ( 'NONE',  ( 20.36894250292379382, 28.67874883491396787, 10.36894250292379205 ) ) ;
#2147 = CARTESIAN_POINT ( 'NONE',  ( -0.8801773607111009756, 28.06368534415484106, 1.068504757029289695E-15 ) ) ;
#2148 = CIRCLE ( 'NONE', #34070, 2.000000000000001776 ) ;
#2149 = CARTESIAN_POINT ( 'NONE',  ( 0.000000000000000000, 15.00000000000000000, 0.000000000000000000 ) ) ;
#2150 = CARTESIAN_POINT ( 'NONE',  ( 10.00000000000000178, 2.258931151000784787, 9.846743663894594434 ) ) ;
#2151 = AXIS2_PLACEMENT_3D ( 'NONE', #93067, #16594, #33053 ) ;
#2152 = EDGE_CURVE ( 'NONE', #46415, #92145, #11040, .T. ) ;
#2153 = CARTESIAN_POINT ( 'NONE',  ( -2.638427012816824124, -7.949402182332544697, 9.846743663894596210 ) ) ;
#2154 = CARTESIAN_POINT ( 'NONE',  ( 19.84674366389459266, 8.300597817667451750, 2.638427012816836559 ) ) ;
#2155 = ORIENTED_EDGE ( 'NONE', *, *, #40456, .T. ) ;
#2156 = DIRECTION ( 'NONE',  ( -1.000000000000000000, 0.000000000000000000, 0.000000000000000000 ) ) ;
#2157 = CIRCLE ( 'NONE', #43652, 0.2500000000000002220 ) ;
#2158 = EDGE_LOOP ( 'NONE', ( #70563, #51808, #69008, #45306, #49863, #97582 ) ) ;
#2159 = DIRECTION ( 'NONE',  ( 0.000000000000000000, 0.000000000000000000, 1.000000000000000000 ) ) ;
#2160 = ORIENTED_EDGE ( 'NONE', *, *, #16954, .T. ) ;
#2162 = CARTESIAN_POINT ( 'NONE',  ( 7.084665262690076126, 17.02201867748817676, -10.88017736071110164 ) ) ;
#2161 = CARTESIAN_POINT ( 'NONE',  ( 10.00000000000000178, 68.05374883491397497, 14.16423886937410082 ) ) ;
#2164 = CARTESIAN_POINT ( 'NONE',  ( -1.099225684535947600, 9.540301336597087456, 6.408140936763237150 ) ) ;
#2163 = CARTESIAN_POINT ( 'NONE',  ( 14.92337183194729633, 42.67559781766745886, 8.527530157486181039 ) ) ;
#2165 = DIRECTION ( 'NONE',  ( -0.09584575252021386438, 0.000000000000000000, -0.9953961983671798519 ) ) ;
#2166 = CARTESIAN_POINT ( 'NONE',  ( 8.439016546559898302, 4.734672723634894724E-16, -11.79122553964973541 ) ) ;
#2167 = CARTESIAN_POINT ( 'NONE',  ( 22.81628187352647785, 1.415301336597087012, 3.434112377981063169 ) ) ;
#2168 = ORIENTED_EDGE ( 'NONE', *, *, #97101, .T. ) ;
#2169 = CARTESIAN_POINT ( 'NONE',  ( 10.00000000000000000, 45.55374883491397497, -14.16423886937410082 ) ) ;
#2170 = ORIENTED_EDGE ( 'NONE', *, *, #68560, .F. ) ;
#2171 = CARTESIAN_POINT ( 'NONE',  ( 13.79529636645030344, 58.26208216824728936, 14.16423886937410614 ) ) ;
#2172 = ORIENTED_EDGE ( 'NONE', *, *, #90944, .T. ) ;
#2173 = CARTESIAN_POINT ( 'NONE',  ( 19.42250999205614548, 30.98035201082150536, -5.440088680355545492 ) ) ;
#2174 = CARTESIAN_POINT ( 'NONE',  ( 12.91533473730993009, 41.60535201082149825, -10.88017736071109987 ) ) ;
#2175 = CARTESIAN_POINT ( 'NONE',  ( 10.00000000000000000, 64.75893115100078035, -9.846743663894594434 ) ) ;
#2176 = CARTESIAN_POINT ( 'NONE',  ( 0.5774900079438607392, 38.48035201082150536, 5.440088680355550821 ) ) ;
#2177 = CARTESIAN_POINT ( 'NONE',  ( 10.00000000000000000, 61.81368534415484106, -10.88017736071110342 ) ) ;
#2178 = CARTESIAN_POINT ( 'NONE',  ( -0.8801773607111009756, 23.06368534415484106, 1.068504757029289695E-15 ) ) ;
#2179 = EDGE_CURVE ( 'NONE', #80524, #56195, #29858, .T. ) ;
#2180 = AXIS2_PLACEMENT_3D ( 'NONE', #30426, #471, #30918 ) ;
#2181 = CARTESIAN_POINT ( 'NONE',  ( 0.1532563361054082862, 16.21726448433411960, 2.638427012816831674 ) ) ;
#2182 = DIRECTION ( 'NONE',  ( 1.000000000000000000, 0.000000000000000000, 0.000000000000000000 ) ) ;
#2183 = VERTEX_POINT ( 'NONE', #61837 ) ;
#2184 = PRESENTATION_STYLE_ASSIGNMENT (( #40654 ) ) ;
#2185 = CARTESIAN_POINT ( 'NONE',  ( 5.076628168052704559, 40.17559781766745175, -8.527530157486179263 ) ) ;
#2186 = ADVANCED_FACE ( 'NONE', ( #16355 ), #98403, .T. ) ;
#2187 = FACE_OUTER_BOUND ( 'NONE', #9592, .T. ) ;
#2188 = DIRECTION ( 'NONE',  ( -0.2503800040544453820, 0.000000000000000000, 0.9681476403781066331 ) ) ;
#2189 = DIRECTION ( 'NONE',  ( -0.000000000000000000, 1.000000000000000000, -0.000000000000000000 ) ) ;
#2190 = CARTESIAN_POINT ( 'NONE',  ( 0.2751277870542913062, 49.36607318730131055, -6.499999999999992006 ) ) ;
#2191 = CARTESIAN_POINT ( 'NONE',  ( 18.52753015748618282, 48.92559781766745886, -4.923371831947291888 ) ) ;
#2192 = CARTESIAN_POINT ( 'NONE',  ( 17.08211943468705840, 45.13708216824730357, -12.26659068614894466 ) ) ;
#2193 = CARTESIAN_POINT ( 'NONE',  ( 2.791683348922240793, 61.63393115100079456, 7.208316651077764092 ) ) ;
#2194 = ORIENTED_EDGE ( 'NONE', *, *, #27099, .F. ) ;
#2195 = DIRECTION ( 'NONE',  ( -0.000000000000000000, -0.000000000000000000, -1.000000000000000000 ) ) ;
#2196 = CARTESIAN_POINT ( 'NONE',  ( 19.84674366389459621, 23.50893115100078390, 7.409399052514197653E-17 ) ) ;
#2197 = EDGE_CURVE ( 'NONE', #39981, #14329, #74238, .T. ) ;
#2198 = CARTESIAN_POINT ( 'NONE',  ( 6.565887622018943937, 50.16530133659708213, 12.81628187352647430 ) ) ;
#2199 = CARTESIAN_POINT ( 'NONE',  ( 7.361572987183170547, 67.05059781766746596, 9.846743663894590881 ) ) ;
#2200 = CARTESIAN_POINT ( 'NONE',  ( 7.084665262690076126, 69.10535201082151957, 10.88017736071109987 ) ) ;
#2201 = CARTESIAN_POINT ( 'NONE',  ( 12.83294900548060724, 14.63606878838274206, 7.766300266068485669 ) ) ;
#2202 = VECTOR ( 'NONE', #88898, 1000.000000000000000 ) ;
#2203 = VERTEX_POINT ( 'NONE', #90356 ) ;
#2204 = CARTESIAN_POINT ( 'NONE',  ( 13.79529636645031943, 60.34541550158063927, -14.16423886937409904 ) ) ;
#2205 = CARTESIAN_POINT ( 'NONE',  ( 4.559911319644449179, 38.89701867748817676, 9.422509992056141925 ) ) ;
#2207 = CARTESIAN_POINT ( 'NONE',  ( 19.42250999205614548, 55.98035201082150536, -5.440088680355545492 ) ) ;
#2206 = CARTESIAN_POINT ( 'NONE',  ( -2.816281873526473856, 9.331968003263753531, 3.434112377981055619 ) ) ;
#2208 = EDGE_CURVE ( 'NONE', #85540, #47721, #21894, .T. ) ;
#2209 = TOROIDAL_SURFACE ( 'NONE', #46864, 14.49999999999999822, 0.5000000000000000000 ) ;
#2210 =( NAMED_UNIT ( * ) SI_UNIT ( $, .STERADIAN. ) SOLID_ANGLE_UNIT ( ) );
#2211 = DIRECTION ( 'NONE',  ( 0.000000000000000000, 1.000000000000000000, 0.000000000000000000 ) ) ;
#2212 = DIRECTION ( 'NONE',  ( 0.000000000000000000, 1.000000000000000000, 0.000000000000000000 ) ) ;
#2213 = CARTESIAN_POINT ( 'NONE',  ( 18.52753015748618282, 53.92559781766745175, -4.923371831947291888 ) ) ;
#2214 = CARTESIAN_POINT ( 'NONE',  ( 18.52753015748617571, 3.092264484334118269, 4.923371831947298993 ) ) ;
#2215 = CARTESIAN_POINT ( 'NONE',  ( -3.795296366450300773, 27.84541550158064283, 14.16423886937410437 ) ) ;
#2216 = CARTESIAN_POINT ( 'NONE',  ( 10.00000000000000000, 2.873634669930420049, -12.81628187352647608 ) ) ;
#2217 = B_SPLINE_CURVE_WITH_KNOTS ( 'NONE', 3,
 ( #34173, #49193, #72665, #64663, #64178, #4199 ),
 .UNSPECIFIED., .F., .F.,
 ( 4, 2, 4 ),
 ( 3.409110551496104941E-05, 0.0004400426677367861921, 0.0008459942299586112671 ),
 .UNSPECIFIED. ) ;
#2218 = CARTESIAN_POINT ( 'NONE',  ( 12.91533473730992121, 9.522018677488171434, 10.88017736071110164 ) ) ;
#2219 =( NAMED_UNIT ( * ) SI_UNIT ( $, .STERADIAN. ) SOLID_ANGLE_UNIT ( ) );
#2220 = CARTESIAN_POINT ( 'NONE',  ( 10.00000000000000000, 30.55374883491397142, -14.16423886937410082 ) ) ;
#2221 = CARTESIAN_POINT ( 'NONE',  ( 6.204703633549690345, 32.84541550158063927, 14.16423886937410082 ) ) ;
#2222 = CARTESIAN_POINT ( 'NONE',  ( 13.79529636645031943, 65.34541550158063217, -14.16423886937409904 ) ) ;
#2223 = CARTESIAN_POINT ( 'NONE',  ( 1.472469842513823179, 20.59226448433411960, -4.923371831947296329 ) ) ;
#2224 = CARTESIAN_POINT ( 'NONE',  ( 12.91533473730992121, 9.522018677488171434, 10.88017736071110164 ) ) ;
#2225 = B_SPLINE_CURVE_WITH_KNOTS ( 'NONE', 3,
 ( #42817, #4825, #20312, #72310 ),
 .UNSPECIFIED., .F., .F.,
 ( 4, 4 ),
 ( 5.421010862427522170E-20, 0.0003153491572467390460 ),
 .UNSPECIFIED. ) ;
#2226 = ORIENTED_EDGE ( 'NONE', *, *, #49530, .F. ) ;
#2227 = CARTESIAN_POINT ( 'NONE',  ( 14.92337183194729633, 32.67559781766745175, 8.527530157486181039 ) ) ;
#2228 = CARTESIAN_POINT ( 'NONE',  ( 12.91533473730992121, 34.52201867748817676, 10.88017736071110164 ) ) ;
#2229 = CARTESIAN_POINT ( 'NONE',  ( 10.00000000000000178, 62.25893115100078745, 9.846743663894594434 ) ) ;
#2231 = CARTESIAN_POINT ( 'NONE',  ( -0.1503990784575407469, 17.22266099184918531, -6.262539305110056631 ) ) ;
#2230 = CARTESIAN_POINT ( 'NONE',  ( -4.164238869374098151, 21.59541550158063217, -3.795296366450310543 ) ) ;
#2232 = CARTESIAN_POINT ( 'NONE',  ( 0.000000000000000000, 0.5000000000000004441, 0.000000000000000000 ) ) ;
#2233 = UNCERTAINTY_MEASURE_WITH_UNIT (LENGTH_MEASURE( 1.000000000000000082E-05 ), #61801, 'distance_accuracy_value', 'NONE');
#2234 = CARTESIAN_POINT ( 'NONE',  ( 0.1532563361054083140, 31.00893115100078390, 1.131784320476157264E-15 ) ) ;
#2235 = CARTESIAN_POINT ( 'NONE',  ( 19.38216949554541557, 47.24863466993041783, -9.382169495545420901 ) ) ;
#2236 = CARTESIAN_POINT ( 'NONE',  ( 19.84674366389459266, 53.30059781766744464, 2.638427012816836559 ) ) ;
#2237 = ORIENTED_EDGE ( 'NONE', *, *, #87940, .T. ) ;
#2238 = DIRECTION ( 'NONE',  ( 0.9238795325112876267, 0.000000000000000000, -0.3826834323650877279 ) ) ;
#2239 = FACE_OUTER_BOUND ( 'NONE', #44031, .T. ) ;
#2240 = CARTESIAN_POINT ( 'NONE',  ( 2.917880565312950480, 60.97041550158063927, -12.26659068614894821 ) ) ;
#2241 = CARTESIAN_POINT ( 'NONE',  ( 4.559911319644449179, 57.23035201082150536, -9.422509992056141925 ) ) ;
#2242 = CARTESIAN_POINT ( 'NONE',  ( 6.204703633549690345, 10.76208216824729824, -14.16423886937410259 ) ) ;
#2243 = CARTESIAN_POINT ( 'NONE',  ( 18.52753015748617571, 3.092264484334118269, 4.923371831947298993 ) ) ;
#2244 = CARTESIAN_POINT ( 'NONE',  ( 0.1532563361054100626, 55.80059781766745175, -2.638427012816831230 ) ) ;
#2245 = CARTESIAN_POINT ( 'NONE',  ( 20.88017736071110875, 20.77201867748816611, -2.915334737309920765 ) ) ;
#2246 = CARTESIAN_POINT ( 'NONE',  ( 18.28836319691944112, 39.34492782695771496, 6.500000000000040856 ) ) ;
#2247 = CARTESIAN_POINT ( 'NONE',  ( 19.84674366389459266, 63.30059781766745886, 2.638427012816836559 ) ) ;
#2248 = EDGE_CURVE ( 'NONE', #61223, #42327, #18320, .T. ) ;
#2249 = DIRECTION ( 'NONE',  ( 0.000000000000000000, 0.000000000000000000, -1.000000000000000000 ) ) ;
#2250 = UNCERTAINTY_MEASURE_WITH_UNIT (LENGTH_MEASURE( 1.000000000000000082E-05 ), #55656, 'distance_accuracy_value', 'NONE');
#2251 = DIRECTION ( 'NONE',  ( -0.000000000000000000, -0.000000000000000000, 1.000000000000000000 ) ) ;
#2252 = ORIENTED_EDGE ( 'NONE', *, *, #16102, .F. ) ;
#2253 = ORIENTED_EDGE ( 'NONE', *, *, #72228, .F. ) ;
#2254 = LINE ( 'NONE', #32711, #64468 ) ;
#2255 = DIRECTION ( 'NONE',  ( 0.000000000000000000, 0.000000000000000000, 1.000000000000000000 ) ) ;
#2256 = SURFACE_STYLE_USAGE ( .BOTH. , #71710 ) ;
#2257 = CARTESIAN_POINT ( 'NONE',  ( 13.79529636645031943, 45.34541550158062506, -14.16423886937409904 ) ) ;
#2258 = CARTESIAN_POINT ( 'NONE',  ( 14.92337183194729633, 62.67559781766745886, 8.527530157486181039 ) ) ;
#2259 = CARTESIAN_POINT ( 'NONE',  ( 17.20831665107776587, 24.13393115100078035, -7.208316651077762316 ) ) ;
#2260 = CARTESIAN_POINT ( 'NONE',  ( 17.39651004071838614, 52.93575266056826933, 6.500000000000032863 ) ) ;
#2262 = CARTESIAN_POINT ( 'NONE',  ( 10.00000000000000000, -2.126365330069579951, -12.81628187352647608 ) ) ;
#2261 = CARTESIAN_POINT ( 'NONE',  ( -0.8801773607111009756, 13.06368534415483929, 1.068504757029289695E-15 ) ) ;
#2263 = CARTESIAN_POINT ( 'NONE',  ( -0.1503990784575242878, 34.24884699246889141, -6.262539305110083276 ) ) ;
#2264 = CARTESIAN_POINT ( 'NONE',  ( 17.08211943468705840, 40.13708216824731068, -12.26659068614894466 ) ) ;
#2265 = CARTESIAN_POINT ( 'NONE',  ( -4.164238869374099039, 61.80374883491397497, 8.674139862899312516E-16 ) ) ;
#2266 = CARTESIAN_POINT ( 'NONE',  ( 6.000000000000000000, 11.50000000000000000, 6.500000000000000888 ) ) ;
#2267 = CARTESIAN_POINT ( 'NONE',  ( 2.603489959281590771, 66.58210964143327715, 6.500000000000003553 ) ) ;
#2268 = CARTESIAN_POINT ( 'NONE',  ( 2.035157376598824452, 68.68868534415484817, 7.964842623401179544 ) ) ;
#2269 = CARTESIAN_POINT ( 'NONE',  ( 18.52753015748618282, 13.92559781766745175, -4.923371831947291888 ) ) ;
#2270 = CARTESIAN_POINT ( 'NONE',  ( -7.322357042924514836, -84.41015717759208314, 4.000000000000000000 ) ) ;
#2271 = ORIENTED_EDGE ( 'NONE', *, *, #89095, .F. ) ;
#2272 = CARTESIAN_POINT ( 'NONE',  ( 20.15039907845753220, 29.72266099184918531, 6.262539305110077947 ) ) ;
#2273 = ORIENTED_EDGE ( 'NONE', *, *, #21380, .F. ) ;
#2274 = CARTESIAN_POINT ( 'NONE',  ( 10.00000000000000000, 24.75893115100078745, -9.846743663894594434 ) ) ;
#2275 = ORIENTED_EDGE ( 'NONE', *, *, #34522, .F. ) ;
#2276 = CARTESIAN_POINT ( 'NONE',  ( 24.16423886937409904, 34.09541550158064638, 3.795296366450317205 ) ) ;
#2277 = CARTESIAN_POINT ( 'NONE',  ( 7.361572987183169658, 39.96726448433411605, -9.846743663894592657 ) ) ;
#2278 = CARTESIAN_POINT ( 'NONE',  ( 2.035157376598824452, 48.68868534415483396, 7.964842623401179544 ) ) ;
#2279 = CARTESIAN_POINT ( 'NONE',  ( -2.849309504156504413, 0.000000000000000000, 4.649650521509808954 ) ) ;
#2280 = ORIENTED_EDGE ( 'NONE', *, *, #80937, .F. ) ;
#2281 = CARTESIAN_POINT ( 'NONE',  ( 7.084665262690076126, 42.02201867748816966, -10.88017736071110164 ) ) ;
#2282 = CARTESIAN_POINT ( 'NONE',  ( 12.54397927573563365, 14.76930270348881180, 8.117058495689102315 ) ) ;
#2283 = VECTOR ( 'NONE', #25246, 1000.000000000000000 ) ;
#2284 = CARTESIAN_POINT ( 'NONE',  ( 6.408140936763243367, -4.209698663402907215, 11.09922568453594494 ) ) ;
#2285 = ORIENTED_EDGE ( 'NONE', *, *, #5834, .T. ) ;
#2286 = CARTESIAN_POINT ( 'NONE',  ( 20.36894250292379738, 9.928748834913966093, -10.36894250292379027 ) ) ;
#2287 = TOROIDAL_SURFACE ( 'NONE', #83696, 1.750000000000000888, 0.2500000000000000000 ) ;
#2288 = VERTEX_POINT ( 'NONE', #63306 ) ;
#2289 =( LENGTH_UNIT ( ) NAMED_UNIT ( * ) SI_UNIT ( .MILLI., .METRE. ) );
#2290 = CARTESIAN_POINT ( 'NONE',  ( 3.591859063236763294, 28.29030133659708568, -11.09922568453595026 ) ) ;
#2291 = CARTESIAN_POINT ( 'NONE',  ( -7.750000000000000000, 41.24999999999999289, 6.500000000000000888 ) ) ;
#2292 = CARTESIAN_POINT ( 'NONE',  ( 10.00000000000000000, 19.75893115100078390, -9.846743663894594434 ) ) ;
#2293 = CARTESIAN_POINT ( 'NONE',  ( 7.084665262690076126, 2.022018677488170990, -10.88017736071110164 ) ) ;
#2294 = EDGE_CURVE ( 'NONE', #83598, #13947, #39853, .T. ) ;
#2295 = CARTESIAN_POINT ( 'NONE',  ( 14.92337183194729633, 27.67559781766745530, 8.527530157486181039 ) ) ;
#2296 = ADVANCED_FACE ( 'NONE', ( #40339 ), #95730, .T. ) ;
#2297 = ORIENTED_EDGE ( 'NONE', *, *, #87825, .F. ) ;
#2298 = CARTESIAN_POINT ( 'NONE',  ( 1.326515405096126976, 0.2306972965111660223, -14.88215077106012529 ) ) ;
#2299 = CARTESIAN_POINT ( 'NONE',  ( 10.00000000000000000, 51.81368534415484106, -10.88017736071110342 ) ) ;
#2300 = CARTESIAN_POINT ( 'NONE',  ( -4.000000000000000000, 9.750000000000000000, 4.000000000000000000 ) ) ;
#2301 = EDGE_CURVE ( 'NONE', #15515, #34926, #64283, .T. ) ;
#2302 = CARTESIAN_POINT ( 'NONE',  ( 3.591859063236763294, 63.29030133659708923, -11.09922568453595026 ) ) ;
#2303 = CARTESIAN_POINT ( 'NONE',  ( 5.076628168052704559, 10.17559781766745175, -8.527530157486179263 ) ) ;
#2304 = EDGE_CURVE ( 'NONE', #91405, #41669, #8746, .T. ) ;
#2305 = CARTESIAN_POINT ( 'NONE',  ( 22.81628187352647785, 11.41530133659708390, 3.434112377981063169 ) ) ;
#2306 = CARTESIAN_POINT ( 'NONE',  ( 4.999999999999999112, 60.50000000000000711, 6.000000000000000000 ) ) ;
#2307 = B_SPLINE_CURVE_WITH_KNOTS ( 'NONE', 3,
 ( #22595, #53072, #115, #77058 ),
 .UNSPECIFIED., .F., .F.,
 ( 4, 4 ),
 ( 2.168404344971008868E-18, 0.001060528352561995475 ),
 .UNSPECIFIED. ) ;
#2308 = CARTESIAN_POINT ( 'NONE',  ( 0.1532563361054100626, 25.80059781766744820, -2.638427012816831230 ) ) ;
#2309 = DIRECTION ( 'NONE',  ( 1.000000000000000000, -0.000000000000000000, 0.000000000000000000 ) ) ;
#2310 = CARTESIAN_POINT ( 'NONE',  ( 6.204703633549690345, 7.845415501580634832, 14.16423886937410082 ) ) ;
#2311 = CARTESIAN_POINT ( 'NONE',  ( 14.92337183194729633, 22.67559781766745175, 8.527530157486181039 ) ) ;
#2312 = CARTESIAN_POINT ( 'NONE',  ( 3.591859063236763294, 33.29030133659708213, -11.09922568453595026 ) ) ;
#2314 = CARTESIAN_POINT ( 'NONE',  ( -3.628035103970717934, -3.629433155896151675, -2.750000000000000000 ) ) ;
#2313 = FACE_OUTER_BOUND ( 'NONE', #27274, .T. ) ;
#2315 = CARTESIAN_POINT ( 'NONE',  ( -0.8801773607110991993, 52.85535201082151247, -2.915334737309923874 ) ) ;
#2316 = CARTESIAN_POINT ( 'NONE',  ( 19.38216949554541202, 5.998634669930420493, 9.382169495545424454 ) ) ;
#2317 = EDGE_CURVE ( 'NONE', #39241, #14667, #25347, .T. ) ;
#2318 = DIRECTION ( 'NONE',  ( -0.000000000000000000, -0.000000000000000000, -1.000000000000000000 ) ) ;
#2319 = CARTESIAN_POINT ( 'NONE',  ( 2.791683348922237240, 30.38393115100078390, -7.208316651077763204 ) ) ;
#2320 = CARTESIAN_POINT ( 'NONE',  ( 14.92337183194729988, 24.34226448433411960, -8.527530157486177487 ) ) ;
#2321 = CARTESIAN_POINT ( 'NONE',  ( 7.084665262690076126, 32.02201867748816966, -10.88017736071110164 ) ) ;
#2322 = CARTESIAN_POINT ( 'NONE',  ( 6.565887622018943937, 23.08196800326375708, -12.81628187352647608 ) ) ;
#2323 = CARTESIAN_POINT ( 'NONE',  ( 1.472469842513823179, 25.59226448433412315, -4.923371831947296329 ) ) ;
#2324 = CARTESIAN_POINT ( 'NONE',  ( -8.211425130294045971, 85.75922772022539675, 4.168580035010579721 ) ) ;
#2325 = CARTESIAN_POINT ( 'NONE',  ( -0.8801773607111008646, 13.27201867748817321, 2.915334737309923430 ) ) ;
#2326 = CARTESIAN_POINT ( 'NONE',  ( 0.5774900079438590739, 62.64701867748817676, -5.440088680355550821 ) ) ;
#2327 =( LENGTH_UNIT ( ) NAMED_UNIT ( * ) SI_UNIT ( .MILLI., .METRE. ) );
#2329 = CARTESIAN_POINT ( 'NONE',  ( 7.084665262690076126, 22.02201867748817321, -10.88017736071110164 ) ) ;
#2328 = CARTESIAN_POINT ( 'NONE',  ( 19.84674366389459621, 48.50893115100078745, 7.409399052514197653E-17 ) ) ;
#2330 = DIRECTION ( 'NONE',  ( 0.000000000000000000, 0.000000000000000000, 1.000000000000000000 ) ) ;
#2331 = ADVANCED_FACE ( 'NONE', ( #94301 ), #32810, .F. ) ;
#2332 = CARTESIAN_POINT ( 'NONE',  ( 20.88017736071110519, 45.56368534415484106, 2.639326808657452039E-16 ) ) ;
#2333 = CARTESIAN_POINT ( 'NONE',  ( 0.5774900079438590739, 7.647018677488171434, -5.440088680355550821 ) ) ;
#2334 = CARTESIAN_POINT ( 'NONE',  ( 17.20831665107776587, 14.13393115100078568, -7.208316651077762316 ) ) ;
#2335 = CARTESIAN_POINT ( 'NONE',  ( 18.52753015748618282, 33.92559781766745886, -4.923371831947291888 ) ) ;
#2336 = CARTESIAN_POINT ( 'NONE',  ( -16.94999999999999929, 100.0000000000000000, -7.896446609406727823 ) ) ;
#2337 = CARTESIAN_POINT ( 'NONE',  ( -0.1558200433086290304, 15.00000000000000178, -14.62618286184525829 ) ) ;
#2338 = CARTESIAN_POINT ( 'NONE',  ( -4.164238869374098151, 1.595415501580634388, -3.795296366450310543 ) ) ;
#2339 = CARTESIAN_POINT ( 'NONE',  ( 17.08211943468705130, 23.47041550158063572, 12.26659068614894998 ) ) ;
#2340 = CARTESIAN_POINT ( 'NONE',  ( 17.20831665107776587, 32.88393115100078745, 7.208316651077764980 ) ) ;
#2341 = DIRECTION ( 'NONE',  ( 1.257568779154408793E-17, 1.000000000000000000, -0.000000000000000000 ) ) ;
#2342 = VERTEX_POINT ( 'NONE', #87294 ) ;
#2343 = CARTESIAN_POINT ( 'NONE',  ( 12.91533473730993009, 6.605352010821504471, -10.88017736071109987 ) ) ;
#2344 = CARTESIAN_POINT ( 'NONE',  ( 2.791683348922237240, 20.38393115100078745, -7.208316651077763204 ) ) ;
#2345 = DIRECTION ( 'NONE',  ( -2.107602052970794797E-16, 1.000000000000000000, -0.000000000000000000 ) ) ;
#2346 = CARTESIAN_POINT ( 'NONE',  ( 4.559911319644449179, 47.23035201082150536, -9.422509992056141925 ) ) ;
#2347 = CARTESIAN_POINT ( 'NONE',  ( -6.000000000000014211, 80.07179676972448590, 4.250000000000000000 ) ) ;
#2348 = MECHANICAL_DESIGN_GEOMETRIC_PRESENTATION_REPRESENTATION (  '', ( #80616 ), #15114 ) ;
#2349 = CARTESIAN_POINT ( 'NONE',  ( 15.44008868035555793, 21.39701867748817321, -9.422509992056140149 ) ) ;
#2350 = CARTESIAN_POINT ( 'NONE',  ( 10.00000000000000000, 47.87363466993042493, -12.81628187352647608 ) ) ;
#2351 = CARTESIAN_POINT ( 'NONE',  ( -2.816281873526473856, 14.12363466993041961, 9.499525473075851096E-16 ) ) ;
#2352 = CARTESIAN_POINT ( 'NONE',  ( 19.84674366389459266, 18.71726448433411960, -2.638427012816827677 ) ) ;
#2353 = EDGE_LOOP ( 'NONE', ( #32746, #47116, #81353, #98167 ) ) ;
#2354 = DIRECTION ( 'NONE',  ( -1.000000000000000000, -6.938893903907221278E-15, 6.938893903907221278E-15 ) ) ;
#2355 = DIRECTION ( 'NONE',  ( 0.000000000000000000, 1.000000000000000000, 0.000000000000000000 ) ) ;
#2356 = CARTESIAN_POINT ( 'NONE',  ( 22.26659068614895176, 54.72041550158063217, -7.082119434687042414 ) ) ;
#2357 = CARTESIAN_POINT ( 'NONE',  ( 24.16423886937410614, 24.51208216824730002, -3.795296366450302550 ) ) ;
#2358 = CARTESIAN_POINT ( 'NONE',  ( 17.96484262340118221, 19.93868534415484106, 7.964842623401181321 ) ) ;
#2359 = CARTESIAN_POINT ( 'NONE',  ( -0.8801773607111009756, 53.06368534415484106, 1.068504757029289695E-15 ) ) ;
#2360 = FACE_OUTER_BOUND ( 'NONE', #47057, .T. ) ;
#2361 = DIRECTION ( 'NONE',  ( -0.000000000000000000, -1.000000000000000000, -0.000000000000000000 ) ) ;
#2362 = CARTESIAN_POINT ( 'NONE',  ( 7.084665262690076126, 67.02201867748817676, -10.88017736071110164 ) ) ;
#2363 = DIRECTION ( 'NONE',  ( -0.8320502943378437211, 0.5547001962252290364, 0.000000000000000000 ) ) ;
#2364 = CARTESIAN_POINT ( 'NONE',  ( 12.63842701281683922, 19.55059781766745175, -9.846743663894590881 ) ) ;
#2365 = CARTESIAN_POINT ( 'NONE',  ( 17.20831665107776587, 17.88393115100078745, 7.208316651077764980 ) ) ;
#2366 = CARTESIAN_POINT ( 'NONE',  ( 2.791683348922240793, 56.63393115100078035, 7.208316651077764092 ) ) ;
#2367 = CARTESIAN_POINT ( 'NONE',  ( 4.559911319644449179, 8.897018677488171434, 9.422509992056141925 ) ) ;
#2368 = UNCERTAINTY_MEASURE_WITH_UNIT (LENGTH_MEASURE( 1.000000000000000082E-05 ), #13505, 'distance_accuracy_value', 'NONE');
#2369 =( BOUNDED_CURVE ( )  B_SPLINE_CURVE ( 2, ( #47773, #71759, #57235, #63747, #71279, #78271, #40779, #87733, #1812 ),
 .UNSPECIFIED., .F., .F. ) 
 B_SPLINE_CURVE_WITH_KNOTS ( ( 3, 2, 2, 2, 3 ),
 ( 0.4748575172211798034, 0.4761904761904761640, 0.4821428571428571508, 0.4880952380952380820, 0.4894281970645347202 ),
 .UNSPECIFIED. ) 
 CURVE ( )  GEOMETRIC_REPRESENTATION_ITEM ( )  RATIONAL_B_SPLINE_CURVE ( ( 0.9881565478350737841, 0.9923695281211494246, 1.000000000000000000, 0.9659258262890683122, 1.000000000000000000, 0.9659258262890683122, 1.000000000000000000, 0.9923695281211478703, 0.9881565478350720078 ) ) 
 REPRESENTATION_ITEM ( '' )  );
#2370 = CARTESIAN_POINT ( 'NONE',  ( 13.43411237798105340, 25.58196800326374998, 12.81628187352647963 ) ) ;
#2371 = VECTOR ( 'NONE', #55317, 1000.000000000000000 ) ;
#2372 = CARTESIAN_POINT ( 'NONE',  ( -0.8801773607110991993, 52.85535201082151247, -2.915334737309923874 ) ) ;
#2373 = CARTESIAN_POINT ( 'NONE',  ( 12.63842701281683922, 34.55059781766745886, -9.846743663894590881 ) ) ;
#2375 = CARTESIAN_POINT ( 'NONE',  ( 14.92337183194729633, 27.67559781766745530, 8.527530157486181039 ) ) ;
#2374 = CARTESIAN_POINT ( 'NONE',  ( 24.16423886937410614, 44.51208216824730357, -3.795296366450302550 ) ) ;
#2376 = DIRECTION ( 'NONE',  ( -0.3007057995042766718, 0.000000000000000000, 0.9537169507482258224 ) ) ;
#2377 = CARTESIAN_POINT ( 'NONE',  ( 0.1532563361054100626, 55.80059781766745175, -2.638427012816831230 ) ) ;
#2379 = CARTESIAN_POINT ( 'NONE',  ( 17.08211943468705840, 15.13708216824730179, -12.26659068614894466 ) ) ;
#2378 = CARTESIAN_POINT ( 'NONE',  ( 1.472469842513823179, 35.59226448433412315, -4.923371831947296329 ) ) ;
#2380 =( BOUNDED_SURFACE ( )  B_SPLINE_SURFACE ( 1, 2, ( 
 ( #32034, #18046, #25556, #70552, #77060, #63039, #2080, #92066, #62538, #9550, #614, #56048, #16074, #31059, #8085, #71052, #48524, #38581, #78542, #61559, #23595, #16572, #85556, #10052, #62048, #2575, #86052, #17563, #40552, #54059, #78048, #77543, #8572, #84573, #46561, #33031, #9061, #39076, #69570, #17068, #92548, #24077, #54544, #85060, #47551, #39574, #70063, #32540, #93537, #57989, #42035, #57503, #65988, #49021, #20502, #87513, #71546, #79025, #49503, #11028, #19998, #33510, #56530, #72994, #42510, #96515, #18531, #64007, #64500, #35493, #94520, #64986, #72500, #4524, #4032, #87019, #27006, #27987, #34987, #11512, #34495, #95513, #50007, #65491, #41547, #72011, #73482, #87999, #42999, #3056, #80512, #19512, #95006, #12011, #27496, #79528, #96011, #80008, #26514, #88495, #26038, #50500, #57010, #3542, #58483, #80997, #34002, #12500, #5009, #19026, #88996, #10538, #41048, #44472, #31796, #8815, #14490, #20997, #6981, #44962, #35984, #74972, #52468, #12986, #39327, #58984, #43482, #50988, #14987, #81482, #28491, #21992, #59963, #67975, #89487, #13491, #43970, #6477, #52955, #69822, #36491, #21490, #36981, #67480, #75465, #62294, #98001, #29455, #51485, #13995, #92802, #73983, #81979, #74472, #5996, #66983, #83466, #82971, #97504, #90455, #1344, #98500, #5508, #29955, #37486, #51987, #66485, #97013, #28969, #77300, #59472, #60461, #90950, #22480, #46808, #89972, #82475, #9304, #33271, #79279, #11268, #79769, #72260, #24329, #25316, #39813, #10789, #55803, #86296, #32784, #56770, #47792, #63281, #70316, #94272, #3789, #18787, #85308, #25795, #93787, #16816, #78793, #41788, #34244, #24818, #85805, #56294, #17803, #87266, #71300, #55294, #86789, #18290, #41306, #64744, #10301, #62794, #33753, #40799, #93294, #48281, #54792, #1833, #78290, #2821, #63765, #48773, #71779, #3288, #64255, #94770, #32289, #9806, #77794, #2328, #47293, #17317, #26269, #49269, #40307, #70813, #27247, #74726, #36241, #21243, #27741, #28731, #95763, #19265, #66737, #89240, #35240, #36742, #81241, #35742, #13239, #57745, #4768, #58223, #50241, #97262, #51741, #65238, #11763, #88744, #87751, #26762, #50755, #65738, #28240, #12740, #88248, #19756, #59222, #43733, #74219, #89726, #57254, #66230, #96267, #80756, #49749, #13739, #5752, #20254, #4275, #42271, #43239, #95256, #12251, #42758, #82225, #73734, #44222, #73240, #80259, #6240, #72742, #5264, #96765, #34749, #58735, #20748, #51239, #81725, #67233, #37737, #98253, #8218, #21748, #44721, #61204, #30694, #84701, #6730, #52229, #52715, #23725, #82721, #53214, #60706, #91710, #30203, #75218, #15236 ),
 ( #37246, #22238, #91203, #22731, #38228, #23229, #68715, #246, #46211, #14240, #83222, #67735, #45219, #90215, #29711, #76698, #75716, #60219, #90713, #14745, #46689, #38712, #92201, #98753, #737, #7230, #68236, #69211, #53701, #83716, #8694, #45717, #7732, #84222, #76219, #15731, #31190, #61684, #54188, #16206, #77186, #97756, #29222, #59721, #69697, #93668, #78174, #71178, #25202, #9190, #33155, #18665, #55680, #32667, #39704, #2206, #49153, #1227, #70191, #1710, #62669, #16699, #71664, #40678, #47172, #63160, #10184, #63649, #2704, #94157, #18173, #54673, #93170, #92681, #17203, #62172, #77677, #48655, #47680, #24206, #85192, #32168, #79654, #79155, #64135, #70688, #3174, #24695, #55167, #10669, #25683, #9685, #39210, #86179, #78675, #56176, #85682, #40181, #17690, #48161, #41183, #94653, #86669, #33639, #26161, #31680, #56656, #87142, #50133, #43126, #65619, #80137, #5138, #89616, #96144, #4658, #11647, #73117, #21128, #72141, #42160, #72625, #34625, #87636, #43617, #12624, #19150, #27627, #59106, #58620, #51627, #89121, #58112, #12136, #41673, #3668, #34131, #36115, #49628, #88621, #50632, #73615, #81123, #35629, #57140, #95132, #20128, #66114, #97148, #66621, #11152, #64623, #42639, #26644, #96643, #35119, #28120, #19640, #74104, #65124, #80640, #4158, #20632, #95643, #5637, #27129, #51121, #81613, #57632, #13121, #28619, #88128, #82606, #44608, #83605, #52599, #46097, #30087, #14124, #15119, #76093, #38115, #92084, #37617, #21629, #91596, #68111, #52114, #14630, #13618, #59605, #37123, #45095, #75103, #97638, #75601, #74610, #44099, #98636, #22119, #45595, #60594, #6610, #7623, #61573, #91089, #7113, #67619, #22617, #23610, #6123, #98127, #29588, #60090, #90101, #15613, #68604, #90592, #53093, #31075, #30582, #82107, #61086, #132, #83102, #36629, #67113, #29103, #8101, #23112, #53584, #84098, #76581, #38597, #69095, #629, #39093, #63056, #10069, #41065, #10554, #3074, #54075, #55054, #69584, #40568, #85573, #17087, #62554, #86559, #77560, #93058, #1104, #25086, #33530, #48542, #16090, #55569, #24591, #46577, #9568, #71562, #64025, #54561, #16586, #86068, #47567, #18063, #2096, #85077, #17579, #48045, #71066, #94538, #40070, #92566, #63541, #70571, #24092, #78065, #84590, #31567, #9076, #32555, #93553, #78559, #2591, #33046, #94051, #25572, #62063, #39589, #8587, #32051, #77075, #47062, #56064, #79041, #70080, #1602, #57029, #5526, #66005, #51006, #57523, #58504, #26533, #49042, #96533, #20018, #65007, #66509, #12029, #65509, #43019, #87530, #34514, #88019, #80029, #28008, #81501, #19532, #26056, #19044, #49520 ) ),
 .UNSPECIFIED., .F., .F., .F. ) 
 B_SPLINE_SURFACE_WITH_KNOTS ( ( 2, 2 ),
 ( 3, 2, 2, 2, 2, 2, 2, 2, 2, 2, 2, 2, 2, 2, 2, 2, 2, 2, 2, 2, 2, 2, 2, 2, 2, 2, 2, 2, 2, 2, 2, 2, 2, 2, 2, 2, 2, 2, 2, 2, 2, 2, 2, 2, 2, 2, 2, 2, 2, 2, 2, 2, 2, 2, 2, 2, 2, 2, 2, 2, 2, 2, 2, 2, 2, 2, 2, 2, 2, 2, 2, 2, 2, 2, 2, 2, 2, 2, 2, 2, 2, 2, 2, 2, 2, 2, 2, 2, 2, 2, 2, 2, 2, 2, 2, 2, 2, 2, 2, 2, 2, 2, 2, 2, 2, 2, 2, 2, 2, 2, 2, 2, 2, 2, 2, 2, 2, 2, 2, 2, 2, 2, 2, 2, 2, 2, 2, 2, 2, 2, 2, 2, 2, 2, 2, 2, 2, 2, 2, 2, 2, 2, 2, 2, 2, 2, 2, 2, 2, 2, 2, 2, 2, 2, 2, 2, 2, 2, 2, 2, 2, 2, 3 ),
 ( 0.000000000000000000, 1.000000000000000000 ),
 ( 0.000000000000000000, 0.005952380952380952051, 0.01190476190476190410, 0.01785714285714285615, 0.02380952380952380820, 0.02976190476190476025, 0.03571428571428571230, 0.04166666666666666435, 0.04761904761904761640, 0.05357142857142856845, 0.05952380952380952051, 0.06547619047619047949, 0.07142857142857142461, 0.07738095238095238360, 0.08333333333333332871, 0.08928571428571428770, 0.09523809523809523281, 0.1011904761904761918, 0.1071428571428571369, 0.1130952380952380959, 0.1190476190476190410, 0.1250000000000000000, 0.1309523809523809590, 0.1369047619047619180, 0.1428571428571428492, 0.1488095238095238082, 0.1547619047619047672, 0.1607142857142857262, 0.1666666666666666574, 0.1726190476190476164, 0.1785714285714285754, 0.1845238095238095344, 0.1904761904761904656, 0.1964285714285714246, 0.2023809523809523836, 0.2083333333333333426, 0.2142857142857142738, 0.2202380952380952328, 0.2261904761904761918, 0.2321428571428571508, 0.2380952380952380820, 0.2440476190476190410, 0.2500000000000000000, 0.2559523809523809312, 0.2619047619047619180, 0.2678571428571428492, 0.2738095238095238360, 0.2797619047619047672, 0.2857142857142856984, 0.2916666666666666852, 0.2976190476190476164, 0.3035714285714285476, 0.3095238095238095344, 0.3154761904761904656, 0.3214285714285714524, 0.3273809523809523836, 0.3333333333333333148, 0.3392857142857143016, 0.3452380952380952328, 0.3511904761904761640, 0.3571428571428571508, 0.3630952380952380820, 0.3690476190476190688, 0.3750000000000000000, 0.3809523809523809312, 0.3869047619047619180, 0.3928571428571428492, 0.3988095238095238360, 0.4047619047619047672, 0.4107142857142856984, 0.4166666666666666852, 0.4226190476190476164, 0.4285714285714285476, 0.4345238095238095344, 0.4404761904761904656, 0.4464285714285714524, 0.4523809523809523836, 0.4583333333333333148, 0.4642857142857143016, 0.4702380952380952328, 0.4761904761904761640, 0.4821428571428571508, 0.4880952380952380820, 0.4940476190476190688, 0.5000000000000000000, 0.5059523809523809312, 0.5119047619047618625, 0.5178571428571429047, 0.5238095238095238360, 0.5297619047619047672, 0.5357142857142856984, 0.5416666666666666297, 0.5476190476190476719, 0.5535714285714286031, 0.5595238095238095344, 0.5654761904761904656, 0.5714285714285713969, 0.5773809523809523281, 0.5833333333333333703, 0.5892857142857143016, 0.5952380952380952328, 0.6011904761904761640, 0.6071428571428570953, 0.6130952380952381375, 0.6190476190476190688, 0.6250000000000000000, 0.6309523809523809312, 0.6369047619047618625, 0.6428571428571429047, 0.6488095238095238360, 0.6547619047619047672, 0.6607142857142856984, 0.6666666666666666297, 0.6726190476190476719, 0.6785714285714286031, 0.6845238095238095344, 0.6904761904761904656, 0.6964285714285713969, 0.7023809523809523281, 0.7083333333333333703, 0.7142857142857143016, 0.7202380952380952328, 0.7261904761904761640, 0.7321428571428570953, 0.7380952380952381375, 0.7440476190476190688, 0.7500000000000000000, 0.7559523809523809312, 0.7619047619047618625, 0.7678571428571429047, 0.7738095238095238360, 0.7797619047619047672, 0.7857142857142856984, 0.7916666666666666297, 0.7976190476190476719, 0.8035714285714286031, 0.8095238095238095344, 0.8154761904761904656, 0.8214285714285713969, 0.8273809523809523281, 0.8333333333333333703, 0.8392857142857143016, 0.8452380952380952328, 0.8511904761904761640, 0.8571428571428570953, 0.8630952380952381375, 0.8690476190476190688, 0.8750000000000000000, 0.8809523809523809312, 0.8869047619047618625, 0.8928571428571429047, 0.8988095238095238360, 0.9047619047619047672, 0.9107142857142856984, 0.9166666666666666297, 0.9226190476190476719, 0.9285714285714286031, 0.9345238095238095344, 0.9404761904761904656, 0.9464285714285713969, 0.9523809523809523281, 0.9583333333333333703, 0.9642857142857143016 ),
 .UNSPECIFIED. ) 
 GEOMETRIC_REPRESENTATION_ITEM ( )  RATIONAL_B_SPLINE_SURFACE ( (
 ( 1.000000000000000000, 0.9659258262890683122, 1.000000000000000000, 0.9659258262890683122, 1.000000000000000000, 0.9659258262890683122, 1.000000000000000000, 0.9659258262890683122, 1.000000000000000000, 0.9659258262890683122, 1.000000000000000000, 0.9659258262890683122, 1.000000000000000000, 0.9659258262890683122, 1.000000000000000000, 0.9659258262890683122, 1.000000000000000000, 0.9659258262890683122, 1.000000000000000000, 0.9659258262890683122, 1.000000000000000000, 0.9659258262890683122, 1.000000000000000000, 0.9659258262890683122, 1.000000000000000000, 0.9659258262890683122, 1.000000000000000000, 0.9659258262890683122, 1.000000000000000000, 0.9659258262890683122, 1.000000000000000000, 0.9659258262890683122, 1.000000000000000000, 0.9659258262890683122, 1.000000000000000000, 0.9659258262890683122, 1.000000000000000000, 0.9659258262890683122, 1.000000000000000000, 0.9659258262890683122, 1.000000000000000000, 0.9659258262890683122, 1.000000000000000000, 0.9659258262890683122, 1.000000000000000000, 0.9659258262890683122, 1.000000000000000000, 0.9659258262890683122, 1.000000000000000000, 0.9659258262890683122, 1.000000000000000000, 0.9659258262890683122, 1.000000000000000000, 0.9659258262890683122, 1.000000000000000000, 0.9659258262890683122, 1.000000000000000000, 0.9659258262890683122, 1.000000000000000000, 0.9659258262890683122, 1.000000000000000000, 0.9659258262890683122, 1.000000000000000000, 0.9659258262890683122, 1.000000000000000000, 0.9659258262890683122, 1.000000000000000000, 0.9659258262890683122, 1.000000000000000000, 0.9659258262890683122, 1.000000000000000000, 0.9659258262890683122, 1.000000000000000000, 0.9659258262890683122, 1.000000000000000000, 0.9659258262890683122, 1.000000000000000000, 0.9659258262890683122, 1.000000000000000000, 0.9659258262890683122, 1.000000000000000000, 0.9659258262890683122, 1.000000000000000000, 0.9659258262890683122, 1.000000000000000000, 0.9659258262890683122, 1.000000000000000000, 0.9659258262890683122, 1.000000000000000000, 0.9659258262890683122, 1.000000000000000000, 0.9659258262890683122, 1.000000000000000000, 0.9659258262890683122, 1.000000000000000000, 0.9659258262890683122, 1.000000000000000000, 0.9659258262890683122, 1.000000000000000000, 0.9659258262890683122, 1.000000000000000000, 0.9659258262890683122, 1.000000000000000000, 0.9659258262890683122, 1.000000000000000000, 0.9659258262890683122, 1.000000000000000000, 0.9659258262890683122, 1.000000000000000000, 0.9659258262890683122, 1.000000000000000000, 0.9659258262890683122, 1.000000000000000000, 0.9659258262890683122, 1.000000000000000000, 0.9659258262890683122, 1.000000000000000000, 0.9659258262890683122, 1.000000000000000000, 0.9659258262890683122, 1.000000000000000000, 0.9659258262890683122, 1.000000000000000000, 0.9659258262890683122, 1.000000000000000000, 0.9659258262890683122, 1.000000000000000000, 0.9659258262890683122, 1.000000000000000000, 0.9659258262890683122, 1.000000000000000000, 0.9659258262890683122, 1.000000000000000000, 0.9659258262890683122, 1.000000000000000000, 0.9659258262890683122, 1.000000000000000000, 0.9659258262890683122, 1.000000000000000000, 0.9659258262890683122, 1.000000000000000000, 0.9659258262890683122, 1.000000000000000000, 0.9659258262890683122, 1.000000000000000000, 0.9659258262890683122, 1.000000000000000000, 0.9659258262890683122, 1.000000000000000000, 0.9659258262890683122, 1.000000000000000000, 0.9659258262890683122, 1.000000000000000000, 0.9659258262890683122, 1.000000000000000000, 0.9659258262890683122, 1.000000000000000000, 0.9659258262890683122, 1.000000000000000000, 0.9659258262890683122, 1.000000000000000000, 0.9659258262890683122, 1.000000000000000000, 0.9659258262890683122, 1.000000000000000000, 0.9659258262890683122, 1.000000000000000000, 0.9659258262890683122, 1.000000000000000000, 0.9659258262890683122, 1.000000000000000000, 0.9659258262890683122, 1.000000000000000000, 0.9659258262890683122, 1.000000000000000000, 0.9659258262890683122, 1.000000000000000000, 0.9659258262890683122, 1.000000000000000000, 0.9659258262890683122, 1.000000000000000000, 0.9659258262890683122, 1.000000000000000000, 0.9659258262890683122, 1.000000000000000000, 0.9659258262890683122, 1.000000000000000000, 0.9659258262890683122, 1.000000000000000000, 0.9659258262890683122, 1.000000000000000000, 0.9659258262890683122, 1.000000000000000000, 0.9659258262890683122, 1.000000000000000000, 0.9659258262890683122, 1.000000000000000000, 0.9659258262890683122, 1.000000000000000000, 0.9659258262890683122, 1.000000000000000000, 0.9659258262890683122, 1.000000000000000000, 0.9659258262890683122, 1.000000000000000000, 0.9659258262890683122, 1.000000000000000000, 0.9659258262890683122, 1.000000000000000000, 0.9659258262890683122, 1.000000000000000000, 0.9659258262890683122, 1.000000000000000000, 0.9659258262890683122, 1.000000000000000000, 0.9659258262890683122, 1.000000000000000000, 0.9659258262890683122, 1.000000000000000000, 0.9659258262890683122, 1.000000000000000000, 0.9659258262890683122, 1.000000000000000000, 0.9659258262890683122, 1.000000000000000000, 0.9659258262890683122, 1.000000000000000000, 0.9659258262890683122, 1.000000000000000000, 0.9659258262890683122, 1.000000000000000000, 0.9659258262890683122, 1.000000000000000000, 0.9659258262890683122, 1.000000000000000000, 0.9659258262890683122, 1.000000000000000000, 0.9659258262890683122, 1.000000000000000000, 0.9659258262890683122, 1.000000000000000000, 0.9659258262890683122, 1.000000000000000000, 0.9659258262890683122, 1.000000000000000000, 0.9659258262890683122, 1.000000000000000000, 0.9659258262890683122, 1.000000000000000000, 0.9659258262890683122, 1.000000000000000000, 0.9659258262890683122, 1.000000000000000000, 0.9659258262890683122, 1.000000000000000000, 0.9659258262890683122, 1.000000000000000000, 0.9659258262890683122, 1.000000000000000000, 0.9659258262890683122, 1.000000000000000000, 0.9659258262890683122, 1.000000000000000000, 0.9659258262890683122, 1.000000000000000000, 0.9659258262890683122, 1.000000000000000000, 0.9659258262890683122, 1.000000000000000000, 0.9659258262890683122, 1.000000000000000000, 0.9659258262890683122, 1.000000000000000000, 0.9659258262890683122, 1.000000000000000000, 0.9659258262890683122, 1.000000000000000000, 0.9659258262890683122, 1.000000000000000000, 0.9659258262890683122, 1.000000000000000000, 0.9659258262890683122, 1.000000000000000000, 0.9659258262890683122, 1.000000000000000000, 0.9659258262890683122, 1.000000000000000000, 0.9659258262890683122, 1.000000000000000000, 0.9659258262890683122, 1.000000000000000000, 0.9659258262890683122, 1.000000000000000000, 0.9659258262890683122, 1.000000000000000000, 0.9659258262890683122, 1.000000000000000000, 0.9659258262890683122, 1.000000000000000000, 0.9659258262890683122, 1.000000000000000000, 0.9659258262890683122, 1.000000000000000000, 0.9659258262890683122, 1.000000000000000000, 0.9659258262890683122, 1.000000000000000000, 0.9659258262890683122, 1.000000000000000000, 0.9659258262890683122, 1.000000000000000000, 0.9659258262890683122, 1.000000000000000000, 0.9659258262890683122, 1.000000000000000000, 0.9659258262890683122, 1.000000000000000000, 0.9659258262890683122, 1.000000000000000000, 0.9659258262890683122, 1.000000000000000000, 0.9659258262890683122, 1.000000000000000000, 0.9659258262890683122, 1.000000000000000000),
 ( 1.000000000000000000, 0.9659258262890683122, 1.000000000000000000, 0.9659258262890683122, 1.000000000000000000, 0.9659258262890683122, 1.000000000000000000, 0.9659258262890683122, 1.000000000000000000, 0.9659258262890683122, 1.000000000000000000, 0.9659258262890683122, 1.000000000000000000, 0.9659258262890683122, 1.000000000000000000, 0.9659258262890683122, 1.000000000000000000, 0.9659258262890683122, 1.000000000000000000, 0.9659258262890683122, 1.000000000000000000, 0.9659258262890683122, 1.000000000000000000, 0.9659258262890683122, 1.000000000000000000, 0.9659258262890683122, 1.000000000000000000, 0.9659258262890683122, 1.000000000000000000, 0.9659258262890683122, 1.000000000000000000, 0.9659258262890683122, 1.000000000000000000, 0.9659258262890683122, 1.000000000000000000, 0.9659258262890683122, 1.000000000000000000, 0.9659258262890683122, 1.000000000000000000, 0.9659258262890683122, 1.000000000000000000, 0.9659258262890683122, 1.000000000000000000, 0.9659258262890683122, 1.000000000000000000, 0.9659258262890683122, 1.000000000000000000, 0.9659258262890683122, 1.000000000000000000, 0.9659258262890683122, 1.000000000000000000, 0.9659258262890683122, 1.000000000000000000, 0.9659258262890683122, 1.000000000000000000, 0.9659258262890683122, 1.000000000000000000, 0.9659258262890683122, 1.000000000000000000, 0.9659258262890683122, 1.000000000000000000, 0.9659258262890683122, 1.000000000000000000, 0.9659258262890683122, 1.000000000000000000, 0.9659258262890683122, 1.000000000000000000, 0.9659258262890683122, 1.000000000000000000, 0.9659258262890683122, 1.000000000000000000, 0.9659258262890683122, 1.000000000000000000, 0.9659258262890683122, 1.000000000000000000, 0.9659258262890683122, 1.000000000000000000, 0.9659258262890683122, 1.000000000000000000, 0.9659258262890683122, 1.000000000000000000, 0.9659258262890683122, 1.000000000000000000, 0.9659258262890683122, 1.000000000000000000, 0.9659258262890683122, 1.000000000000000000, 0.9659258262890683122, 1.000000000000000000, 0.9659258262890683122, 1.000000000000000000, 0.9659258262890683122, 1.000000000000000000, 0.9659258262890683122, 1.000000000000000000, 0.9659258262890683122, 1.000000000000000000, 0.9659258262890683122, 1.000000000000000000, 0.9659258262890683122, 1.000000000000000000, 0.9659258262890683122, 1.000000000000000000, 0.9659258262890683122, 1.000000000000000000, 0.9659258262890683122, 1.000000000000000000, 0.9659258262890683122, 1.000000000000000000, 0.9659258262890683122, 1.000000000000000000, 0.9659258262890683122, 1.000000000000000000, 0.9659258262890683122, 1.000000000000000000, 0.9659258262890683122, 1.000000000000000000, 0.9659258262890683122, 1.000000000000000000, 0.9659258262890683122, 1.000000000000000000, 0.9659258262890683122, 1.000000000000000000, 0.9659258262890683122, 1.000000000000000000, 0.9659258262890683122, 1.000000000000000000, 0.9659258262890683122, 1.000000000000000000, 0.9659258262890683122, 1.000000000000000000, 0.9659258262890683122, 1.000000000000000000, 0.9659258262890683122, 1.000000000000000000, 0.9659258262890683122, 1.000000000000000000, 0.9659258262890683122, 1.000000000000000000, 0.9659258262890683122, 1.000000000000000000, 0.9659258262890683122, 1.000000000000000000, 0.9659258262890683122, 1.000000000000000000, 0.9659258262890683122, 1.000000000000000000, 0.9659258262890683122, 1.000000000000000000, 0.9659258262890683122, 1.000000000000000000, 0.9659258262890683122, 1.000000000000000000, 0.9659258262890683122, 1.000000000000000000, 0.9659258262890683122, 1.000000000000000000, 0.9659258262890683122, 1.000000000000000000, 0.9659258262890683122, 1.000000000000000000, 0.9659258262890683122, 1.000000000000000000, 0.9659258262890683122, 1.000000000000000000, 0.9659258262890683122, 1.000000000000000000, 0.9659258262890683122, 1.000000000000000000, 0.9659258262890683122, 1.000000000000000000, 0.9659258262890683122, 1.000000000000000000, 0.9659258262890683122, 1.000000000000000000, 0.9659258262890683122, 1.000000000000000000, 0.9659258262890683122, 1.000000000000000000, 0.9659258262890683122, 1.000000000000000000, 0.9659258262890683122, 1.000000000000000000, 0.9659258262890683122, 1.000000000000000000, 0.9659258262890683122, 1.000000000000000000, 0.9659258262890683122, 1.000000000000000000, 0.9659258262890683122, 1.000000000000000000, 0.9659258262890683122, 1.000000000000000000, 0.9659258262890683122, 1.000000000000000000, 0.9659258262890683122, 1.000000000000000000, 0.9659258262890683122, 1.000000000000000000, 0.9659258262890683122, 1.000000000000000000, 0.9659258262890683122, 1.000000000000000000, 0.9659258262890683122, 1.000000000000000000, 0.9659258262890683122, 1.000000000000000000, 0.9659258262890683122, 1.000000000000000000, 0.9659258262890683122, 1.000000000000000000, 0.9659258262890683122, 1.000000000000000000, 0.9659258262890683122, 1.000000000000000000, 0.9659258262890683122, 1.000000000000000000, 0.9659258262890683122, 1.000000000000000000, 0.9659258262890683122, 1.000000000000000000, 0.9659258262890683122, 1.000000000000000000, 0.9659258262890683122, 1.000000000000000000, 0.9659258262890683122, 1.000000000000000000, 0.9659258262890683122, 1.000000000000000000, 0.9659258262890683122, 1.000000000000000000, 0.9659258262890683122, 1.000000000000000000, 0.9659258262890683122, 1.000000000000000000, 0.9659258262890683122, 1.000000000000000000, 0.9659258262890683122, 1.000000000000000000, 0.9659258262890683122, 1.000000000000000000, 0.9659258262890683122, 1.000000000000000000, 0.9659258262890683122, 1.000000000000000000, 0.9659258262890683122, 1.000000000000000000, 0.9659258262890683122, 1.000000000000000000, 0.9659258262890683122, 1.000000000000000000, 0.9659258262890683122, 1.000000000000000000, 0.9659258262890683122, 1.000000000000000000, 0.9659258262890683122, 1.000000000000000000, 0.9659258262890683122, 1.000000000000000000, 0.9659258262890683122, 1.000000000000000000, 0.9659258262890683122, 1.000000000000000000, 0.9659258262890683122, 1.000000000000000000, 0.9659258262890683122, 1.000000000000000000, 0.9659258262890683122, 1.000000000000000000, 0.9659258262890683122, 1.000000000000000000, 0.9659258262890683122, 1.000000000000000000, 0.9659258262890683122, 1.000000000000000000, 0.9659258262890683122, 1.000000000000000000, 0.9659258262890683122, 1.000000000000000000, 0.9659258262890683122, 1.000000000000000000, 0.9659258262890683122, 1.000000000000000000, 0.9659258262890683122, 1.000000000000000000, 0.9659258262890683122, 1.000000000000000000, 0.9659258262890683122, 1.000000000000000000, 0.9659258262890683122, 1.000000000000000000, 0.9659258262890683122, 1.000000000000000000, 0.9659258262890683122, 1.000000000000000000, 0.9659258262890683122, 1.000000000000000000, 0.9659258262890683122, 1.000000000000000000, 0.9659258262890683122, 1.000000000000000000, 0.9659258262890683122, 1.000000000000000000, 0.9659258262890683122, 1.000000000000000000, 0.9659258262890683122, 1.000000000000000000, 0.9659258262890683122, 1.000000000000000000, 0.9659258262890683122, 1.000000000000000000, 0.9659258262890683122, 1.000000000000000000, 0.9659258262890683122, 1.000000000000000000, 0.9659258262890683122, 1.000000000000000000, 0.9659258262890683122, 1.000000000000000000, 0.9659258262890683122, 1.000000000000000000, 0.9659258262890683122, 1.000000000000000000, 0.9659258262890683122, 1.000000000000000000) ) ) 
 REPRESENTATION_ITEM ( '' )  SURFACE ( )  );
#2381 = CARTESIAN_POINT ( 'NONE',  ( 17.08211943468705840, 15.13708216824730179, -12.26659068614894466 ) ) ;
#2382 = CARTESIAN_POINT ( 'NONE',  ( 5.076628168052703671, 26.84226448433411960, 8.527530157486179263 ) ) ;
#2383 = CARTESIAN_POINT ( 'NONE',  ( 12.91533473730993009, 41.60535201082149825, -10.88017736071109987 ) ) ;
#2384 = CARTESIAN_POINT ( 'NONE',  ( 2.035157376598824452, 18.68868534415484106, 7.964842623401179544 ) ) ;
#2385 = CARTESIAN_POINT ( 'NONE',  ( 10.00000000000000178, 44.31368534415484106, 10.88017736071110342 ) ) ;
#2386 = EDGE_CURVE ( 'NONE', #63123, #89545, #48801, .T. ) ;
#2387 = CARTESIAN_POINT ( 'NONE',  ( 17.96484262340118221, 29.93868534415484106, 7.964842623401181321 ) ) ;
#2388 = VERTEX_POINT ( 'NONE', #48309 ) ;
#2389 = CARTESIAN_POINT ( 'NONE',  ( 10.00000000000000000, 37.87363466993041783, -12.81628187352647608 ) ) ;
#2390 = CARTESIAN_POINT ( 'NONE',  ( 7.084665262690076126, 44.10535201082151247, 10.88017736071109987 ) ) ;
#2391 = VERTEX_POINT ( 'NONE', #62824 ) ;
#2392 = EDGE_CURVE ( 'NONE', #70551, #70990, #85834, .T. ) ;
#2393 = CARTESIAN_POINT ( 'NONE',  ( -2.816281873526473856, 59.33196800326374643, 3.434112377981055619 ) ) ;
#2394 = CARTESIAN_POINT ( 'NONE',  ( 2.035157376598824452, 63.68868534415484106, 7.964842623401179544 ) ) ;
#2395 = ORIENTED_EDGE ( 'NONE', *, *, #42890, .F. ) ;
#2396 = CARTESIAN_POINT ( 'NONE',  ( 20.88017736071110164, 65.35535201082150536, 2.915334737309930979 ) ) ;
#2397 = CARTESIAN_POINT ( 'NONE',  ( 2.603489959281614308, 61.58210964143329846, 6.500000000000031086 ) ) ;
#2398 = FACE_OUTER_BOUND ( 'NONE', #84995, .T. ) ;
#2399 = CARTESIAN_POINT ( 'NONE',  ( -2.266590686148945544, 56.38708216824731068, -7.082119434687050408 ) ) ;
#2401 = VERTEX_POINT ( 'NONE', #47818 ) ;
#2400 = CARTESIAN_POINT ( 'NONE',  ( 7.361572987183169658, 9.967264484334119601, -9.846743663894592657 ) ) ;
#2402 =( NAMED_UNIT ( * ) PLANE_ANGLE_UNIT ( ) SI_UNIT ( $, .RADIAN. ) );
#2403 = CARTESIAN_POINT ( 'NONE',  ( 0.1532563361054083140, 6.008931151000784787, 1.131784320476157264E-15 ) ) ;
#2404 = CARTESIAN_POINT ( 'NONE',  ( 12.91533473730992121, 4.522018677488169658, 10.88017736071110164 ) ) ;
#2405 = CARTESIAN_POINT ( 'NONE',  ( 10.00000000000000000, 39.75893115100078745, -9.846743663894594434 ) ) ;
#2406 = EDGE_LOOP ( 'NONE', ( #38789, #68564, #35096, #78633 ) ) ;
#2407 = CARTESIAN_POINT ( 'NONE',  ( 17.20831665107776587, 49.13393115100078745, -7.208316651077762316 ) ) ;
#2408 = CARTESIAN_POINT ( 'NONE',  ( 17.96484262340118221, 46.18868534415484106, -7.964842623401177768 ) ) ;
#2409 = CARTESIAN_POINT ( 'NONE',  ( 18.52753015748617571, 48.09226448433412315, 4.923371831947298993 ) ) ;
#2411 = CARTESIAN_POINT ( 'NONE',  ( 0.000000000000000000, 15.00000000000000000, 0.000000000000000000 ) ) ;
#2410 = DIRECTION ( 'NONE',  ( -0.000000000000000000, -0.000000000000000000, 1.000000000000000000 ) ) ;
#2412 = CARTESIAN_POINT ( 'NONE',  ( 10.00000000000000178, 54.31368534415484106, 10.88017736071110342 ) ) ;
#2413 = CARTESIAN_POINT ( 'NONE',  ( 19.42250999205614193, 10.14701867748816966, 5.440088680355555262 ) ) ;
#2414 = EDGE_CURVE ( 'NONE', #37014, #48374, #2847, .T. ) ;
#2415 = B_SPLINE_CURVE_WITH_KNOTS ( 'NONE', 3,
 ( #47096, #84620, #16124, #31600 ),
 .UNSPECIFIED., .F., .F.,
 ( 4, 4 ),
 ( 0.000000000000000000, 0.001036303429213394781 ),
 .UNSPECIFIED. ) ;
#2416 = PRESENTATION_LAYER_ASSIGNMENT (  '', '', ( #48622 ) ) ;
#2417 = CARTESIAN_POINT ( 'NONE',  ( 13.43411237798105340, 40.58196800326375353, 12.81628187352647963 ) ) ;
#2418 = VERTEX_POINT ( 'NONE', #40827 ) ;
#2419 = VECTOR ( 'NONE', #1334, 1000.000000000000114 ) ;
#2420 = CARTESIAN_POINT ( 'NONE',  ( -2.816281873526473856, 34.12363466993042493, 9.499525473075851096E-16 ) ) ;
#2421 = CARTESIAN_POINT ( 'NONE',  ( -0.8801773607111009756, 28.06368534415484106, 1.068504757029289695E-15 ) ) ;
#2422 = EDGE_CURVE ( 'NONE', #19080, #91846, #96963, .T. ) ;
#2423 = VERTEX_POINT ( 'NONE', #39357 ) ;
#2424 = ORIENTED_EDGE ( 'NONE', *, *, #97101, .F. ) ;
#2425 = CARTESIAN_POINT ( 'NONE',  ( 10.00000000000000000, -0.2410688489992152128, -9.846743663894594434 ) ) ;
#2426 = CARTESIAN_POINT ( 'NONE',  ( 12.63842701281683922, 44.55059781766745175, -9.846743663894590881 ) ) ;
#2428 = CARTESIAN_POINT ( 'NONE',  ( 12.63842701281683034, 42.46726448433412315, 9.846743663894596210 ) ) ;
#2427 = CARTESIAN_POINT ( 'NONE',  ( 18.52753015748618282, 13.92559781766745175, -4.923371831947291888 ) ) ;
#2429 = DIRECTION ( 'NONE',  ( -0.000000000000000000, -1.000000000000000000, -0.000000000000000000 ) ) ;
#2430 = DIRECTION ( 'NONE',  ( -0.000000000000000000, -1.000000000000000000, -0.000000000000000000 ) ) ;
#2431 = CARTESIAN_POINT ( 'NONE',  ( 7.361572987183169658, 29.96726448433411960, -9.846743663894592657 ) ) ;
#2432 = DIRECTION ( 'NONE',  ( 0.000000000000000000, 1.000000000000000000, 0.000000000000000000 ) ) ;
#2433 = CARTESIAN_POINT ( 'NONE',  ( 2.603489959281614308, 61.58210964143329846, 6.500000000000031086 ) ) ;
#2435 = CARTESIAN_POINT ( 'NONE',  ( 0.2751277870542967463, 70.00000000000000000, -6.000000000000000000 ) ) ;
#2434 = CARTESIAN_POINT ( 'NONE',  ( 14.92337183194729633, 32.67559781766745175, 8.527530157486181039 ) ) ;
#2436 = DIRECTION ( 'NONE',  ( 0.000000000000000000, 1.000000000000000000, 0.000000000000000000 ) ) ;
#2438 = ORIENTED_EDGE ( 'NONE', *, *, #33837, .T. ) ;
#2437 = CARTESIAN_POINT ( 'NONE',  ( 10.00000000000000000, 39.75893115100078745, -9.846743663894594434 ) ) ;
#2439 = CARTESIAN_POINT ( 'NONE',  ( -14.47650479471817242, 0.5000000000000004441, -3.928206833722204028 ) ) ;
#2440 = CARTESIAN_POINT ( 'NONE',  ( 6.565887622018943937, 23.08196800326375708, -12.81628187352647608 ) ) ;
#2441 = VECTOR ( 'NONE', #86202, 1000.000000000000000 ) ;
#2442 = ADVANCED_FACE ( 'NONE', ( #69851 ), #1374, .T. ) ;
#2443 = CARTESIAN_POINT ( 'NONE',  ( -7.860426697680325425, 15.00000000000000000, -13.93165778241942832 ) ) ;
#2444 = CARTESIAN_POINT ( 'NONE',  ( -0.3689425029237881626, 42.42874883491396787, 10.36894250292379027 ) ) ;
#2445 = CARTESIAN_POINT ( 'NONE',  ( 5.076628168052703671, 21.84226448433411960, 8.527530157486179263 ) ) ;
#2446 = CARTESIAN_POINT ( 'NONE',  ( 14.92337183194729633, 2.675597817667451750, 8.527530157486181039 ) ) ;
#2447 = DIRECTION ( 'NONE',  ( -0.000000000000000000, -0.000000000000000000, 1.000000000000000000 ) ) ;
#2448 = CARTESIAN_POINT ( 'NONE',  ( -0.3689425029237898834, 46.17874883491397497, -10.36894250292378850 ) ) ;
#2449 = CARTESIAN_POINT ( 'NONE',  ( 19.84674366389459266, 58.30059781766745886, 2.638427012816836559 ) ) ;
#2450 = EDGE_CURVE ( 'NONE', #84403, #23604, #32460, .T. ) ;
#2451 = CARTESIAN_POINT ( 'NONE',  ( 0.5774900079438607392, 8.480352010821505360, 5.440088680355550821 ) ) ;
#2452 = CARTESIAN_POINT ( 'NONE',  ( 20.36894250292379382, 23.67874883491397142, 10.36894250292379205 ) ) ;
#2453 = CARTESIAN_POINT ( 'NONE',  ( 10.00000000000000000, 35.55374883491396787, -14.16423886937410082 ) ) ;
#2454 = DIRECTION ( 'NONE',  ( -1.000000000000000000, 0.000000000000000000, 0.000000000000000000 ) ) ;
#2456 = CARTESIAN_POINT ( 'NONE',  ( 0.1532563361054100626, 50.80059781766745175, -2.638427012816831230 ) ) ;
#2455 = FACE_OUTER_BOUND ( 'NONE', #69497, .T. ) ;
#2457 = ORIENTED_EDGE ( 'NONE', *, *, #89519, .T. ) ;
#2458 = CARTESIAN_POINT ( 'NONE',  ( 7.084665262690076126, 32.02201867748816966, -10.88017736071110164 ) ) ;
#2459 = CYLINDRICAL_SURFACE ( 'NONE', #92120, 0.2500000000000002220 ) ;
#2460 = COLOUR_RGB ( '', 0.66274510, 0.83137255, 0.94901961) ;
#2461 = CARTESIAN_POINT ( 'NONE',  ( -14.49440716394873085, 4.311470567659570904E-16, -0.4026921475168178111 ) ) ;
#2462 = CARTESIAN_POINT ( 'NONE',  ( 14.92337183194729988, 39.34226448433412315, -8.527530157486177487 ) ) ;
#2463 = DIRECTION ( 'NONE',  ( -1.000000000000000000, 0.000000000000000000, 0.000000000000000000 ) ) ;
#2464 = CARTESIAN_POINT ( 'NONE',  ( 10.36894250292379027, 8.678748834913974974, 10.36894250292378672 ) ) ;
#2465 = CARTESIAN_POINT ( 'NONE',  ( 0.1532563361054100626, 55.80059781766745175, -2.638427012816831230 ) ) ;
#2466 = CARTESIAN_POINT ( 'NONE',  ( 12.63842701281683922, 64.55059781766745175, -9.846743663894590881 ) ) ;
#2467 = ORIENTED_EDGE ( 'NONE', *, *, #82546, .F. ) ;
#2468 = AXIS2_PLACEMENT_3D ( 'NONE', #2232, #32691, #26186 ) ;
#2469 = CARTESIAN_POINT ( 'NONE',  ( 17.08211943468705130, 18.47041550158063572, 12.26659068614894998 ) ) ;
#2470 = CARTESIAN_POINT ( 'NONE',  ( -6.090257717040430840, -2.687212025164267037E-15, -13.29726560978576799 ) ) ;
#2472 = CARTESIAN_POINT ( 'NONE',  ( -6.336512077239706109, 14.76930270348881180, -13.53095227201393413 ) ) ;
#2471 = CARTESIAN_POINT ( 'NONE',  ( -3.250000000000000444, 1.019547802438453887, -2.500000000000000000 ) ) ;
#2473 = CARTESIAN_POINT ( 'NONE',  ( 0.5774900079438590739, 7.647018677488171434, -5.440088680355550821 ) ) ;
#2474 = CARTESIAN_POINT ( 'NONE',  ( 13.43411237798106583, 22.66530133659708923, -12.81628187352647252 ) ) ;
#2475 = CARTESIAN_POINT ( 'NONE',  ( -0.1503990784575328643, 55.12777174578612716, 6.262539305110068177 ) ) ;
#2476 = CARTESIAN_POINT ( 'NONE',  ( 7.084665262690076126, 64.10535201082150536, 10.88017736071109987 ) ) ;
#2477 = CARTESIAN_POINT ( 'NONE',  ( 21.92686044187656691, 42.18830936912751639, 4.562052436263911564E-16 ) ) ;
#2478 = FACE_OUTER_BOUND ( 'NONE', #29779, .T. ) ;
#2479 = CARTESIAN_POINT ( 'NONE',  ( 7.084665262690076126, 14.10535201082150358, 10.88017736071109987 ) ) ;
#2480 = AXIS2_PLACEMENT_3D ( 'NONE', #27488, #19503, #42990 ) ;
#2481 = CARTESIAN_POINT ( 'NONE',  ( 0.9413316022086114510, 3.455083851089586489, 6.499999999999963585 ) ) ;
#2482 = CARTESIAN_POINT ( 'NONE',  ( 17.96484262340118221, 29.93868534415484106, 7.964842623401181321 ) ) ;
#2483 = CARTESIAN_POINT ( 'NONE',  ( 20.88017736071110519, 40.56368534415484106, 2.639326808657452039E-16 ) ) ;
#2484 = AXIS2_PLACEMENT_3D ( 'NONE', #92075, #85069, #39580 ) ;
#2485 = CARTESIAN_POINT ( 'NONE',  ( 3.591859063236763294, -1.709698663402913210, -11.09922568453595026 ) ) ;
#2486 = DIRECTION ( 'NONE',  ( 0.000000000000000000, -1.000000000000000000, -0.000000000000000000 ) ) ;
#2487 = CARTESIAN_POINT ( 'NONE',  ( 0.6178305044545838731, 64.74863466993043914, 9.382169495545420901 ) ) ;
#2488 = CARTESIAN_POINT ( 'NONE',  ( 18.52753015748618282, 13.92559781766745175, -4.923371831947291888 ) ) ;
#2489 = VERTEX_POINT ( 'NONE', #92832 ) ;
#2490 = CARTESIAN_POINT ( 'NONE',  ( 12.91533473730992121, 24.52201867748816966, 10.88017736071110164 ) ) ;
#2491 = CARTESIAN_POINT ( 'NONE',  ( 22.81628187352648496, 26.83196800326374998, -3.434112377981050290 ) ) ;
#2492 = LINE ( 'NONE', #40474, #9821 ) ;
#2493 = CARTESIAN_POINT ( 'NONE',  ( 19.84674366389459266, 63.71726448433412315, -2.638427012816827677 ) ) ;
#2494 = CARTESIAN_POINT ( 'NONE',  ( 17.96484262340118221, 46.18868534415484106, -7.964842623401177768 ) ) ;
#2495 = TOROIDAL_SURFACE ( 'NONE', #71133, 14.49999999999999822, 0.5000000000000000000 ) ;
#2496 = CARTESIAN_POINT ( 'NONE',  ( 2.791683348922237240, 15.38393115100078212, -7.208316651077763204 ) ) ;
#2497 = CARTESIAN_POINT ( 'NONE',  ( 22.81628187352647785, 41.62363466993042493, 6.195893100308588602E-16 ) ) ;
#2499 = CARTESIAN_POINT ( 'NONE',  ( -4.862001128006866679, 15.00000000000000000, 13.66056166602454347 ) ) ;
#2498 = CARTESIAN_POINT ( 'NONE',  ( -0.8801773607111008646, 68.27201867748817676, 2.915334737309923430 ) ) ;
#2500 = CARTESIAN_POINT ( 'NONE',  ( 10.76493118081685019, 1.524659305057740610E-16, 9.902252441915806003 ) ) ;
#2501 = CARTESIAN_POINT ( 'NONE',  ( -2.816281873526473856, 64.12363466993042493, 9.499525473075851096E-16 ) ) ;
#2502 = VERTEX_POINT ( 'NONE', #93324 ) ;
#2503 = DIRECTION ( 'NONE',  ( -1.000000000000000000, 3.469446951953623261E-15, 0.000000000000000000 ) ) ;
#2504 =( LENGTH_UNIT ( ) NAMED_UNIT ( * ) SI_UNIT ( .MILLI., .METRE. ) );
#2505 =( NAMED_UNIT ( * ) SI_UNIT ( $, .STERADIAN. ) SOLID_ANGLE_UNIT ( ) );
#2507 = CARTESIAN_POINT ( 'NONE',  ( -0.3689425029237881626, 17.42874883491397142, 10.36894250292379027 ) ) ;
#2506 = CARTESIAN_POINT ( 'NONE',  ( 13.43411237798106583, 52.66530133659708213, -12.81628187352647252 ) ) ;
#2508 = CARTESIAN_POINT ( 'NONE',  ( 0.1532563361054100626, 10.80059781766745175, -2.638427012816831230 ) ) ;
#2509 = CARTESIAN_POINT ( 'NONE',  ( 2.035157376598822676, 7.438685344154837509, -7.964842623401177768 ) ) ;
#2510 = CARTESIAN_POINT ( 'NONE',  ( 19.84674366389459621, 13.50893115100078568, 7.409399052514197653E-17 ) ) ;
#2511 = CARTESIAN_POINT ( 'NONE',  ( 13.79529636645031943, 60.34541550158063927, -14.16423886937409904 ) ) ;
#2512 = ORIENTED_EDGE ( 'NONE', *, *, #65266, .T. ) ;
#2513 = CARTESIAN_POINT ( 'NONE',  ( 20.88017736071110875, 5.772018677488170546, -2.915334737309920765 ) ) ;
#2514 = EDGE_CURVE ( 'NONE', #98693, #52439, #24845, .T. ) ;
#2515 = CARTESIAN_POINT ( 'NONE',  ( 7.084665262690076126, 24.10535201082150181, 10.88017736071109987 ) ) ;
#2516 = DIRECTION ( 'NONE',  ( 0.000000000000000000, 0.000000000000000000, 1.000000000000000000 ) ) ;
#2517 = ORIENTED_EDGE ( 'NONE', *, *, #4236, .T. ) ;
#2518 = CARTESIAN_POINT ( 'NONE',  ( 4.559911319644449179, 13.89701867748817321, 9.422509992056141925 ) ) ;
#2519 = CARTESIAN_POINT ( 'NONE',  ( 7.361572987183170547, 57.05059781766744464, 9.846743663894590881 ) ) ;
#2520 = PRESENTATION_LAYER_ASSIGNMENT (  '', '', ( #10482 ) ) ;
#2521 = CARTESIAN_POINT ( 'NONE',  ( 21.09922568453594849, 56.20696800326375353, 6.408140936763242479 ) ) ;
#2522 = DIRECTION ( 'NONE',  ( 0.000000000000000000, 0.000000000000000000, -1.000000000000000000 ) ) ;
#2524 = CARTESIAN_POINT ( 'NONE',  ( -4.164238869374098151, 21.59541550158063217, -3.795296366450310543 ) ) ;
#2523 = CARTESIAN_POINT ( 'NONE',  ( -4.000000000000000000, 36.75000000000000000, -3.750000000000000000 ) ) ;
#2525 = CARTESIAN_POINT ( 'NONE',  ( 2.035157376598822676, 42.43868534415483396, -7.964842623401177768 ) ) ;
#2526 = CARTESIAN_POINT ( 'NONE',  ( -0.8801773607111009756, 23.06368534415484106, 1.068504757029289695E-15 ) ) ;
#2527 = CARTESIAN_POINT ( 'NONE',  ( 1.472469842513823179, 56.42559781766745886, 4.923371831947296329 ) ) ;
#2528 = B_SPLINE_CURVE_WITH_KNOTS ( 'NONE', 3,
 ( #81225, #81706, #5246, #96244, #97245, #59701 ),
 .UNSPECIFIED., .F., .F.,
 ( 4, 2, 4 ),
 ( 3.409110551496071059E-05, 0.0004400426677367861921, 0.0008459942299586115924 ),
 .UNSPECIFIED. ) ;
#2529 = CARTESIAN_POINT ( 'NONE',  ( 19.72487221294570858, 31.86607318730074567, 6.500000000000000888 ) ) ;
#2530 = CARTESIAN_POINT ( 'NONE',  ( 14.92337183194729988, 34.34226448433411605, -8.527530157486177487 ) ) ;
#2531 = CARTESIAN_POINT ( 'NONE',  ( 2.791683348922237240, 5.383931151000785675, -7.208316651077763204 ) ) ;
#2532 = CARTESIAN_POINT ( 'NONE',  ( 9.846743663894590881, 28.71726448433412671, -2.638427012816833894 ) ) ;
#2533 = ORIENTED_EDGE ( 'NONE', *, *, #11199, .F. ) ;
#2534 = CARTESIAN_POINT ( 'NONE',  ( 17.96484262340118221, 4.938685344154837509, 7.964842623401181321 ) ) ;
#2535 = CARTESIAN_POINT ( 'NONE',  ( 14.92337183194729633, 17.67559781766745175, 8.527530157486181039 ) ) ;
#2536 = CARTESIAN_POINT ( 'NONE',  ( 13.43411237798105340, 5.581968003263753531, 12.81628187352647963 ) ) ;
#2537 = CARTESIAN_POINT ( 'NONE',  ( 2.035157376598824452, 43.68868534415484106, 7.964842623401179544 ) ) ;
#2539 = CARTESIAN_POINT ( 'NONE',  ( 6.565887622018943937, 43.08196800326374643, -12.81628187352647608 ) ) ;
#2538 = CARTESIAN_POINT ( 'NONE',  ( 15.44008868035555793, 6.397018677488170546, -9.422509992056140149 ) ) ;
#2540 = CARTESIAN_POINT ( 'NONE',  ( 6.204703633549690345, 25.76208216824730712, -14.16423886937410259 ) ) ;
#2541 = AXIS2_PLACEMENT_3D ( 'NONE', #67737, #14747, #67235 ) ;
#2542 = ADVANCED_FACE ( 'NONE', ( #50268, #80785 ), #49783, .F. ) ;
#2543 = VECTOR ( 'NONE', #8861, 1000.000000000000227 ) ;
#2544 = CARTESIAN_POINT ( 'NONE',  ( 3.591859063236763294, 63.29030133659708923, -11.09922568453595026 ) ) ;
#2545 = ORIENTED_EDGE ( 'NONE', *, *, #97325, .F. ) ;
#2546 = CARTESIAN_POINT ( 'NONE',  ( 19.84674366389459266, 58.71726448433411605, -2.638427012816827677 ) ) ;
#2547 = EDGE_CURVE ( 'NONE', #23291, #42121, #26615, .T. ) ;
#2548 = CARTESIAN_POINT ( 'NONE',  ( 12.91533473730992121, 24.52201867748816966, 10.88017736071110164 ) ) ;
#2549 = ORIENTED_EDGE ( 'NONE', *, *, #98491, .T. ) ;
#2550 = CARTESIAN_POINT ( 'NONE',  ( 12.63842701281683034, 2.467264484334118269, 9.846743663894596210 ) ) ;
#2551 = DIRECTION ( 'NONE',  ( 1.224646799147353454E-16, -1.540077580099091832E-33, 1.000000000000000000 ) ) ;
#2552 = CARTESIAN_POINT ( 'NONE',  ( 5.076628168052703671, 11.84226448433411960, 8.527530157486179263 ) ) ;
#2553 = CARTESIAN_POINT ( 'NONE',  ( 14.92337183194729633, 2.675597817667451750, 8.527530157486181039 ) ) ;
#2555 = CARTESIAN_POINT ( 'NONE',  ( -5.376821459229932820, 0.2301511342434834628, -13.93958558162645112 ) ) ;
#2554 = CARTESIAN_POINT ( 'NONE',  ( 20.88017736071110164, 60.35535201082151957, 2.915334737309930979 ) ) ;
#2556 = CARTESIAN_POINT ( 'NONE',  ( -0.8801773607111008646, 68.27201867748817676, 2.915334737309923430 ) ) ;
#2557 = COLOUR_RGB ( '', 0.31764706, 0.68627451, 0.89019608) ;
#2559 = ORIENTED_EDGE ( 'NONE', *, *, #96342, .T. ) ;
#2558 = CARTESIAN_POINT ( 'NONE',  ( 19.84674366389459266, 3.300597817667451750, 2.638427012816836559 ) ) ;
#2560 = CIRCLE ( 'NONE', #58395, 15.00000000000000000 ) ;
#2561 = CARTESIAN_POINT ( 'NONE',  ( 3.969999999999999751, 10.25000000000000000, -2.750000000000000000 ) ) ;
#2562 = CARTESIAN_POINT ( 'NONE',  ( 0.1532563361054100626, 50.80059781766745175, -2.638427012816831230 ) ) ;
#2563 = ORIENTED_EDGE ( 'NONE', *, *, #97772, .T. ) ;
#2564 = ORIENTED_EDGE ( 'NONE', *, *, #16836, .T. ) ;
#2565 = FACE_OUTER_BOUND ( 'NONE', #78621, .T. ) ;
#2566 = CIRCLE ( 'NONE', #7408, 0.2500000000000002220 ) ;
#2567 = CARTESIAN_POINT ( 'NONE',  ( -0.3689425029237898834, 6.178748834913968757, -10.36894250292378850 ) ) ;
#2568 = CARTESIAN_POINT ( 'NONE',  ( -2.816281873526473856, 59.12363466993042493, 9.499525473075851096E-16 ) ) ;
#2569 = CARTESIAN_POINT ( 'NONE',  ( -0.3689425029237898834, 6.178748834913968757, -10.36894250292378850 ) ) ;
#2570 = CARTESIAN_POINT ( 'NONE',  ( 22.26659068614895176, 29.72041550158063572, -7.082119434687042414 ) ) ;
#2571 = CARTESIAN_POINT ( 'NONE',  ( 0.1957200283969079413, 45.25733960839543357, 6.499999999999982236 ) ) ;
#2572 = CARTESIAN_POINT ( 'NONE',  ( 19.42250999205614548, 25.98035201082150891, -5.440088680355545492 ) ) ;
#2573 = DIRECTION ( 'NONE',  ( -0.4461978131098131573, 0.000000000000000000, 0.8949343616020228875 ) ) ;
#2574 = ORIENTED_EDGE ( 'NONE', *, *, #72852, .T. ) ;
#2575 = CARTESIAN_POINT ( 'NONE',  ( 7.361572987183169658, 4.967264484334119601, -9.846743663894592657 ) ) ;
#2576 = CARTESIAN_POINT ( 'NONE',  ( 19.84674366389459266, 13.30059781766745353, 2.638427012816836559 ) ) ;
#2577 = CARTESIAN_POINT ( 'NONE',  ( -1.099225684535947600, 28.70696800326375353, -6.408140936763238038 ) ) ;
#2579 = EDGE_CURVE ( 'NONE', #91901, #78236, #2756, .T. ) ;
#2578 = CARTESIAN_POINT ( 'NONE',  ( 18.52753015748618282, 43.92559781766745175, -4.923371831947291888 ) ) ;
#2580 = CARTESIAN_POINT ( 'NONE',  ( 5.500000000000000000, 11.00000000000000000, -6.500000000000000888 ) ) ;
#2581 = CARTESIAN_POINT ( 'NONE',  ( 16.40814093676324603, 32.45696800326375353, -11.09922568453594671 ) ) ;
#2582 = CARTESIAN_POINT ( 'NONE',  ( 19.72487221294571569, 40.71833443783938122, -6.499999999999989342 ) ) ;
#2583 = CARTESIAN_POINT ( 'NONE',  ( 12.63842701281683034, 32.46726448433412315, 9.846743663894596210 ) ) ;
#2584 = AXIS2_PLACEMENT_3D ( 'NONE', #55942, #40945, #72394 ) ;
#2585 = CARTESIAN_POINT ( 'NONE',  ( -2.266590686148945544, 12.22041550158063394, 7.082119434687048631 ) ) ;
#2586 = ORIENTED_EDGE ( 'NONE', *, *, #2422, .T. ) ;
#2587 = CARTESIAN_POINT ( 'NONE',  ( 20.88017736071110519, 30.56368534415484106, 2.639326808657452039E-16 ) ) ;
#2588 = CARTESIAN_POINT ( 'NONE',  ( -4.164238869374098151, 31.59541550158063927, -3.795296366450310543 ) ) ;
#2589 = CARTESIAN_POINT ( 'NONE',  ( 14.92337183194729988, 54.34226448433412315, -8.527530157486177487 ) ) ;
#2590 = CARTESIAN_POINT ( 'NONE',  ( 0.1532563361054082862, 11.21726448433411605, 2.638427012816831674 ) ) ;
#2592 = LINE ( 'NONE', #10555, #38498 ) ;
#2591 = CARTESIAN_POINT ( 'NONE',  ( 16.40814093676324603, 57.45696800326375353, -11.09922568453594671 ) ) ;
#2593 = CARTESIAN_POINT ( 'NONE',  ( 10.00000000000000178, 34.31368534415484106, 10.88017736071110342 ) ) ;
#2594 = LINE ( 'NONE', #48545, #11887 ) ;
#2595 = CARTESIAN_POINT ( 'NONE',  ( 16.40814093676324603, 17.45696800326375353, -11.09922568453594671 ) ) ;
#2596 = CARTESIAN_POINT ( 'NONE',  ( 22.81628187352647785, 21.62363466993041783, 6.195893100308588602E-16 ) ) ;
#2597 = CARTESIAN_POINT ( 'NONE',  ( 2.791683348922237240, 45.38393115100079456, -7.208316651077763204 ) ) ;
#2598 = CARTESIAN_POINT ( 'NONE',  ( -2.915334737309934532, -2.977981322511826789, -10.88017736071109987 ) ) ;
#2599 = CARTESIAN_POINT ( 'NONE',  ( -2.816281873526471635, 43.91530133659708923, -3.434112377981056508 ) ) ;
#2601 = CARTESIAN_POINT ( 'NONE',  ( 64.56412365047461321, 11.49999999999999289, -9.500000000000000000 ) ) ;
#2600 = CARTESIAN_POINT ( 'NONE',  ( 7.084665262690076126, 57.02201867748817676, -10.88017736071110164 ) ) ;
#2602 = VECTOR ( 'NONE', #71219, 1000.000000000000000 ) ;
#2603 = VECTOR ( 'NONE', #71659, 1000.000000000000000 ) ;
#2604 = CARTESIAN_POINT ( 'NONE',  ( -7.778993153962144191, -1.060766117554759580, 4.000000000000000000 ) ) ;
#2605 = PLANE ( 'NONE',  #62401 ) ;
#2606 = CARTESIAN_POINT ( 'NONE',  ( -0.8801773607111008646, 48.27201867748816966, 2.915334737309923430 ) ) ;
#2607 = CARTESIAN_POINT ( 'NONE',  ( 10.00000000000000178, 54.31368534415484106, 10.88017736071110342 ) ) ;
#2608 = LINE ( 'NONE', #24109, #48873 ) ;
#2609 = DIRECTION ( 'NONE',  ( 0.8070303256584299145, -0.5905099943842175847, 0.000000000000000000 ) ) ;
#2610 = CARTESIAN_POINT ( 'NONE',  ( -0.8801773607110991993, 2.855352010821504471, -2.915334737309923874 ) ) ;
#2611 = CARTESIAN_POINT ( 'NONE',  ( 17.20831665107776587, 59.13393115100078745, -7.208316651077762316 ) ) ;
#2613 = DIRECTION ( 'NONE',  ( 1.000000000000000000, 0.000000000000000000, 0.000000000000000000 ) ) ;
#2612 = CARTESIAN_POINT ( 'NONE',  ( -0.8801773607110991993, 22.85535201082150181, -2.915334737309923874 ) ) ;
#2614 = CARTESIAN_POINT ( 'NONE',  ( 20.32896413005680003, 51.77164270246084499, 5.963430220938287007 ) ) ;
#2615 = CARTESIAN_POINT ( 'NONE',  ( -2.816281873526471635, 23.91530133659708568, -3.434112377981056508 ) ) ;
#2616 = ORIENTED_EDGE ( 'NONE', *, *, #83073, .F. ) ;
#2617 = CARTESIAN_POINT ( 'NONE',  ( 17.96484262340118221, 46.18868534415484106, -7.964842623401177768 ) ) ;
#2618 = CARTESIAN_POINT ( 'NONE',  ( 17.20831665107776587, 39.13393115100079456, -7.208316651077762316 ) ) ;
#2620 = CARTESIAN_POINT ( 'NONE',  ( 14.94699059465108171, 14.49999999999999112, -1.259949270174796965 ) ) ;
#2619 = CARTESIAN_POINT ( 'NONE',  ( -2.816281873526471635, 8.915301336597083903, -3.434112377981056508 ) ) ;
#2621 = CARTESIAN_POINT ( 'NONE',  ( 12.91533473730993009, 31.60535201082150891, -10.88017736071109987 ) ) ;
#2622 = CARTESIAN_POINT ( 'NONE',  ( 15.44008868035555260, 34.73035201082151247, 9.422509992056143702 ) ) ;
#2623 = CARTESIAN_POINT ( 'NONE',  ( 13.79529636645030344, 48.26208216824728936, 14.16423886937410614 ) ) ;
#2624 = CARTESIAN_POINT ( 'NONE',  ( 0.1532563361054083140, 41.00893115100078745, 1.131784320476157264E-15 ) ) ;
#2625 = CARTESIAN_POINT ( 'NONE',  ( 15.44008868035555260, 59.73035201082151247, 9.422509992056143702 ) ) ;
#2626 = PRESENTATION_STYLE_ASSIGNMENT (( #71598 ) ) ;
#2627 = CARTESIAN_POINT ( 'NONE',  ( 10.00000000000000178, 18.05374883491396787, 14.16423886937410082 ) ) ;
#2628 = TOROIDAL_SURFACE ( 'NONE', #18587, 14.49999999999999822, 0.5000000000000000000 ) ;
#2629 = EDGE_CURVE ( 'NONE', #59148, #50110, #58257, .T. ) ;
#2630 = SPHERICAL_SURFACE ( 'NONE', #35375, 0.2500000000000000000 ) ;
#2631 = CARTESIAN_POINT ( 'NONE',  ( -6.599999999999995204, -97.00000000000000000, -4.000000000000000000 ) ) ;
#2632 = VECTOR ( 'NONE', #83832, 1000.000000000000000 ) ;
#2633 = TOROIDAL_SURFACE ( 'NONE', #15403, 2.750000000000000888, 0.2500000000000000000 ) ;
#2634 = ORIENTED_EDGE ( 'NONE', *, *, #82984, .T. ) ;
#2635 = CARTESIAN_POINT ( 'NONE',  ( 20.36894250292379382, 43.67874883491397497, 10.36894250292379205 ) ) ;
#2636 = CARTESIAN_POINT ( 'NONE',  ( -0.3689425029237881626, 42.42874883491396787, 10.36894250292379027 ) ) ;
#2637 = CARTESIAN_POINT ( 'NONE',  ( 19.84674366389459621, 23.50893115100078390, 7.409399052514197653E-17 ) ) ;
#2638 = CARTESIAN_POINT ( 'NONE',  ( 19.38216949554541202, 20.99863466993042138, 9.382169495545424454 ) ) ;
#2639 = CARTESIAN_POINT ( 'NONE',  ( 5.076628168052703671, 61.84226448433412315, 8.527530157486179263 ) ) ;
#2640 = CARTESIAN_POINT ( 'NONE',  ( 18.72515096720568906, 36.07228050351032778, -6.500000000000007105 ) ) ;
#2642 = CARTESIAN_POINT ( 'NONE',  ( 21.09922568453594849, 31.20696800326375353, 6.408140936763242479 ) ) ;
#2641 = CARTESIAN_POINT ( 'NONE',  ( 4.559911319644449179, 53.89701867748817676, 9.422509992056141925 ) ) ;
#2643 = CARTESIAN_POINT ( 'NONE',  ( 17.08211943468705840, 40.13708216824731068, -12.26659068614894466 ) ) ;
#2644 = VECTOR ( 'NONE', #2309, 1000.000000000000000 ) ;
#2645 = CARTESIAN_POINT ( 'NONE',  ( 9.997910040112605756, 4.102332422533249404E-16, -10.50199004140717562 ) ) ;
#2646 = CARTESIAN_POINT ( 'NONE',  ( 10.00000000000000000, 66.81368534415484817, -10.88017736071110342 ) ) ;
#2647 = CARTESIAN_POINT ( 'NONE',  ( 9.846743663894590881, -6.699402182332541145, 2.638427012816828565 ) ) ;
#2648 = ORIENTED_EDGE ( 'NONE', *, *, #71276, .F. ) ;
#2649 = CARTESIAN_POINT ( 'NONE',  ( -0.1503990784575403861, 9.248846992468887862, -6.262539305110056631 ) ) ;
#2650 = ORIENTED_EDGE ( 'NONE', *, *, #57319, .T. ) ;
#2651 = CARTESIAN_POINT ( 'NONE',  ( -8.000000000000000000, 40.99999999999999289, -4.250000000000000000 ) ) ;
#2652 = ORIENTED_EDGE ( 'NONE', *, *, #42565, .F. ) ;
#2653 = CARTESIAN_POINT ( 'NONE',  ( 10.00000000000000178, 3.053748834913967425, 14.16423886937410082 ) ) ;
#2655 = CARTESIAN_POINT ( 'NONE',  ( 15.44008868035555793, 6.397018677488171434, -9.422509992056140149 ) ) ;
#2654 = CARTESIAN_POINT ( 'NONE',  ( 20.88017736071110519, 10.56368534415483929, 2.639326808657452039E-16 ) ) ;
#2657 = CARTESIAN_POINT ( 'NONE',  ( -2.816281873526471635, 8.915301336597083903, -3.434112377981056508 ) ) ;
#2656 = CARTESIAN_POINT ( 'NONE',  ( 14.92337183194729633, 32.67559781766745175, 8.527530157486181039 ) ) ;
#2658 = CARTESIAN_POINT ( 'NONE',  ( 17.75000000000001776, 4.561680251642721935E-15, 3.750000000000000000 ) ) ;
#2659 = STYLED_ITEM ( 'NONE', ( #90423 ), #60882 ) ;
#2660 = VECTOR ( 'NONE', #61914, 1000.000000000000000 ) ;
#2661 = EDGE_CURVE ( 'NONE', #59353, #94118, #44470, .T. ) ;
#2662 = CARTESIAN_POINT ( 'NONE',  ( 21.09922568453595559, 17.04030133659708923, -6.408140936763230044 ) ) ;
#2663 = ORIENTED_EDGE ( 'NONE', *, *, #69776, .T. ) ;
#2664 = CARTESIAN_POINT ( 'NONE',  ( -2.266590686148945544, 47.22041550158063927, 7.082119434687048631 ) ) ;
#2665 = ORIENTED_EDGE ( 'NONE', *, *, #18588, .T. ) ;
#2666 = CARTESIAN_POINT ( 'NONE',  ( -4.164238869374099039, 56.80374883491397497, 8.674139862899312516E-16 ) ) ;
#2667 = ORIENTED_EDGE ( 'NONE', *, *, #23207, .T. ) ;
#2668 = CARTESIAN_POINT ( 'NONE',  ( 12.91533473730993009, 36.60535201082151247, -10.88017736071109987 ) ) ;
#2669 = CARTESIAN_POINT ( 'NONE',  ( 15.44008868035555260, 34.73035201082151247, 9.422509992056143702 ) ) ;
#2670 = CARTESIAN_POINT ( 'NONE',  ( 19.42250999205614193, 40.14701867748817676, 5.440088680355555262 ) ) ;
#2671 = CARTESIAN_POINT ( 'NONE',  ( 20.88017736071110164, 60.35535201082151957, 2.915334737309930979 ) ) ;
#2672 = CARTESIAN_POINT ( 'NONE',  ( 19.42250999205614548, 30.98035201082150536, -5.440088680355545492 ) ) ;
#2673 = CIRCLE ( 'NONE', #64922, 0.2500000000000002220 ) ;
#2674 = LINE ( 'NONE', #48620, #45796 ) ;
#2675 = VECTOR ( 'NONE', #43581, 1000.000000000000000 ) ;
#2676 = CARTESIAN_POINT ( 'NONE',  ( 12.63842701281683922, 14.55059781766744997, -9.846743663894590881 ) ) ;
#2677 = LINE ( 'NONE', #80977, #85163 ) ;
#2678 = EDGE_LOOP ( 'NONE', ( #59455, #84303, #7010, #32845 ) ) ;
#2679 = CARTESIAN_POINT ( 'NONE',  ( 14.92337183194729988, 39.34226448433412315, -8.527530157486177487 ) ) ;
#2680 = CARTESIAN_POINT ( 'NONE',  ( 18.95386800104995828, 53.23810908735728020, -6.499999999999990230 ) ) ;
#2681 = LINE ( 'NONE', #40163, #5977 ) ;
#2682 = EDGE_CURVE ( 'NONE', #16289, #14317, #96295, .T. ) ;
#2683 = DIRECTION ( 'NONE',  ( 0.000000000000000000, 0.000000000000000000, -1.000000000000000000 ) ) ;
#2684 = CARTESIAN_POINT ( 'NONE',  ( -8.209432707285007069, 14.49999999999999112, 12.55409154915484393 ) ) ;
#2685 = CARTESIAN_POINT ( 'NONE',  ( 1.472469842513823179, 61.42559781766745175, 4.923371831947296329 ) ) ;
#2686 = CARTESIAN_POINT ( 'NONE',  ( 13.79529636645031943, 50.34541550158064638, -14.16423886937409904 ) ) ;
#2687 = CARTESIAN_POINT ( 'NONE',  ( 69.60148758828984228, 0.4999999999999982792, -9.500000000000000000 ) ) ;
#2688 = ORIENTED_EDGE ( 'NONE', *, *, #38184, .T. ) ;
#2689 = CARTESIAN_POINT ( 'NONE',  ( 14.04391541078763161, 15.00000000000000000, 3.608107528142933340 ) ) ;
#2690 = CARTESIAN_POINT ( 'NONE',  ( 10.00000000000000000, 24.75893115100078745, -9.846743663894594434 ) ) ;
#2691 = FACE_OUTER_BOUND ( 'NONE', #12878, .T. ) ;
#2692 = CARTESIAN_POINT ( 'NONE',  ( 14.92337183194729988, 59.34226448433412315, -8.527530157486177487 ) ) ;
#2694 = EDGE_CURVE ( 'NONE', #7312, #11472, #19363, .T. ) ;
#2693 = CARTESIAN_POINT ( 'NONE',  ( 2.791683348922240793, 1.633931151000784565, 7.208316651077764092 ) ) ;
#2695 = FILL_AREA_STYLE_COLOUR ( '', #96755 ) ;
#2696 = CARTESIAN_POINT ( 'NONE',  ( 7.361572987183170547, 57.05059781766744464, 9.846743663894590881 ) ) ;
#2697 = DIRECTION ( 'NONE',  ( -1.154631945610162802E-14, 0.000000000000000000, 1.000000000000000000 ) ) ;
#2698 = AXIS2_PLACEMENT_3D ( 'NONE', #72238, #18272, #9785 ) ;
#2699 = ORIENTED_EDGE ( 'NONE', *, *, #38085, .F. ) ;
#2700 =( BOUNDED_CURVE ( )  B_SPLINE_CURVE ( 2, ( #6769, #35777, #13774, #66266, #58264, #81279, #28277, #82759, #88780 ),
 .UNSPECIFIED., .F., .F. ) 
 B_SPLINE_CURVE_WITH_KNOTS ( ( 3, 2, 2, 2, 3 ),
 ( 0.4044266512259456214, 0.4047619047619047672, 0.4107142857142856984, 0.4166666666666666297, 0.4170019202026257754 ),
 .UNSPECIFIED. ) 
 CURVE ( )  GEOMETRIC_REPRESENTATION_ITEM ( )  RATIONAL_B_SPLINE_CURVE ( ( 0.9963778908391760503, 0.9980808541467920403, 1.000000000000000000, 0.9659258262890682012, 1.000000000000000000, 0.9659258262890682012, 1.000000000000000000, 0.9980808541467920403, 0.9963778908391760503 ) ) 
 REPRESENTATION_ITEM ( '' )  );
#2701 = CARTESIAN_POINT ( 'NONE',  ( 22.26659068614894466, 63.88708216824730357, 7.082119434687054849 ) ) ;
#2702 = CARTESIAN_POINT ( 'NONE',  ( -14.03351048042393856, 0.000000000000000000, -2.474486531753901541 ) ) ;
#2703 = CARTESIAN_POINT ( 'NONE',  ( -0.8801773607111008646, 38.27201867748816255, 2.915334737309923430 ) ) ;
#2705 = CARTESIAN_POINT ( 'NONE',  ( 19.42250999205614548, 65.98035201082151957, -5.440088680355545492 ) ) ;
#2704 = CARTESIAN_POINT ( 'NONE',  ( 21.09922568453595559, 12.04030133659708746, -6.408140936763230044 ) ) ;
#2706 = CARTESIAN_POINT ( 'NONE',  ( 10.91036564011041676, 0.2301503799940547990, -10.20716212663437261 ) ) ;
#2707 = CARTESIAN_POINT ( 'NONE',  ( 20.03932841506541962, 45.62161441960500241, -6.397827110479002322 ) ) ;
#2708 = DIRECTION ( 'NONE',  ( -0.000000000000000000, -0.000000000000000000, 1.000000000000000000 ) ) ;
#2709 = CARTESIAN_POINT ( 'NONE',  ( 17.20831665107776587, 47.88393115100078745, 7.208316651077764980 ) ) ;
#2710 = CARTESIAN_POINT ( 'NONE',  ( 5.076628168052703671, 6.842264484334118713, 8.527530157486179263 ) ) ;
#2711 = CARTESIAN_POINT ( 'NONE',  ( 3.469446951953614189E-15, 33.05374883491396787, 14.16423886937410259 ) ) ;
#2712 = CARTESIAN_POINT ( 'NONE',  ( -2.816281873526471635, 3.915301336597087456, -3.434112377981056508 ) ) ;
#2713 = CARTESIAN_POINT ( 'NONE',  ( -0.8801773607111008646, 13.27201867748817321, 2.915334737309923430 ) ) ;
#2714 = CARTESIAN_POINT ( 'NONE',  ( 17.08211943468705130, 33.47041550158063927, 12.26659068614894998 ) ) ;
#2715 = VECTOR ( 'NONE', #9049, 1000.000000000000000 ) ;
#2716 = CARTESIAN_POINT ( 'NONE',  ( 17.08211943468705130, 33.47041550158063927, 12.26659068614894998 ) ) ;
#2717 = CARTESIAN_POINT ( 'NONE',  ( -4.164238869374099927, 62.01208216824728936, 3.795296366450308767 ) ) ;
#2718 = CARTESIAN_POINT ( 'NONE',  ( 0.1532563361054082862, 31.21726448433412315, 2.638427012816831674 ) ) ;
#2719 = TOROIDAL_SURFACE ( 'NONE', #58571, 14.49999999999999822, 0.5000000000000000000 ) ;
#2720 = CARTESIAN_POINT ( 'NONE',  ( 22.81628187352647785, 36.41530133659707502, 3.434112377981063169 ) ) ;
#2721 = CARTESIAN_POINT ( 'NONE',  ( 7.084665262690076126, 12.02201867748817143, -10.88017736071110164 ) ) ;
#2722 = VERTEX_POINT ( 'NONE', #4306 ) ;
#2723 = CARTESIAN_POINT ( 'NONE',  ( 7.361572987183170547, 32.05059781766745175, 9.846743663894590881 ) ) ;
#2724 = CARTESIAN_POINT ( 'NONE',  ( 20.88017736071110875, 40.77201867748818387, -2.915334737309920765 ) ) ;
#2725 = CARTESIAN_POINT ( 'NONE',  ( 0.6178305044545818747, 3.498634669930420049, -9.382169495545419124 ) ) ;
#2727 = CARTESIAN_POINT ( 'NONE',  ( 1.042145700049402990, 44.74216108172000617, -6.499999999999941380 ) ) ;
#2726 = CARTESIAN_POINT ( 'NONE',  ( 6.204703633549690345, 27.84541550158063217, 14.16423886937410082 ) ) ;
#2728 = DIRECTION ( 'NONE',  ( 0.000000000000000000, 1.000000000000000000, 0.000000000000000000 ) ) ;
#2729 = CARTESIAN_POINT ( 'NONE',  ( 12.63842701281683034, 22.46726448433411605, 9.846743663894596210 ) ) ;
#2730 = CARTESIAN_POINT ( 'NONE',  ( 21.09922568453595559, 52.04030133659708923, -6.408140936763230044 ) ) ;
#2731 = CARTESIAN_POINT ( 'NONE',  ( 7.361572987183170547, 52.05059781766745175, 9.846743663894590881 ) ) ;
#2732 = EDGE_LOOP ( 'NONE', ( #59068, #59314, #36568, #45789 ) ) ;
#2733 = CARTESIAN_POINT ( 'NONE',  ( 8.742108547319491052, -4.148811688989288982, -4.000000000000000000 ) ) ;
#2734 = CARTESIAN_POINT ( 'NONE',  ( 17.08211943468705130, 63.47041550158063927, 12.26659068614894998 ) ) ;
#2735 = CARTESIAN_POINT ( 'NONE',  ( 24.16423886937409904, 9.095415501580633943, 3.795296366450317205 ) ) ;
#2736 = CARTESIAN_POINT ( 'NONE',  ( 18.52753015748618282, 3.925597817667451306, -4.923371831947291888 ) ) ;
#2737 = CARTESIAN_POINT ( 'NONE',  ( 10.00000000000000000, 54.75893115100078745, -9.846743663894594434 ) ) ;
#2738 = CARTESIAN_POINT ( 'NONE',  ( 0.5774900079438590739, 17.64701867748817321, -5.440088680355550821 ) ) ;
#2739 = DIRECTION ( 'NONE',  ( -0.000000000000000000, -1.000000000000000000, -0.000000000000000000 ) ) ;
#2740 = DIRECTION ( 'NONE',  ( 0.000000000000000000, 1.000000000000000000, 0.000000000000000000 ) ) ;
#2741 = ADVANCED_FACE ( 'NONE', ( #5781 ), #20283, .F. ) ;
#2742 = CARTESIAN_POINT ( 'NONE',  ( 0.000000000000000000, 0.000000000000000000, 0.000000000000000000 ) ) ;
#2743 = B_SPLINE_CURVE_WITH_KNOTS ( 'NONE', 3,
 ( #67360, #29348, #73371, #12384 ),
 .UNSPECIFIED., .F., .F.,
 ( 4, 4 ),
 ( 4.336808689942017736E-19, 0.002562518741975335079 ),
 .UNSPECIFIED. ) ;
#2744 = FACE_OUTER_BOUND ( 'NONE', #54008, .T. ) ;
#2745 = EDGE_LOOP ( 'NONE', ( #38210, #90387, #43418, #77232 ) ) ;
#2746 = ORIENTED_EDGE ( 'NONE', *, *, #3662, .F. ) ;
#2747 = DIRECTION ( 'NONE',  ( 0.000000000000000000, 1.000000000000000000, 0.000000000000000000 ) ) ;
#2748 = CARTESIAN_POINT ( 'NONE',  ( 22.26659068614895176, 14.72041550158063572, -7.082119434687042414 ) ) ;
#2749 = CARTESIAN_POINT ( 'NONE',  ( 6.204703633549690345, 0.7620821682473009062, -14.16423886937410259 ) ) ;
#2750 = CARTESIAN_POINT ( 'NONE',  ( 0.1532563361054082862, 51.21726448433412315, 2.638427012816831674 ) ) ;
#2751 = CARTESIAN_POINT ( 'NONE',  ( 7.361572987183170547, 27.05059781766745175, 9.846743663894590881 ) ) ;
#2752 = CARTESIAN_POINT ( 'NONE',  ( -2.816281873526471635, 63.91530133659708923, -3.434112377981056508 ) ) ;
#2754 = CARTESIAN_POINT ( 'NONE',  ( 10.00000000000000178, 62.25893115100078745, 9.846743663894594434 ) ) ;
#2753 = CARTESIAN_POINT ( 'NONE',  ( 17.96484262340118221, 14.93868534415484106, 7.964842623401181321 ) ) ;
#2755 = FACE_OUTER_BOUND ( 'NONE', #4071, .T. ) ;
#2757 = ADVANCED_FACE ( 'NONE', ( #13268 ), #12772, .T. ) ;
#2756 = B_SPLINE_CURVE_WITH_KNOTS ( 'NONE', 3,
 ( #65267, #72769, #81756, #43760, #19297, #4796, #88280, #59254, #49295, #87781 ),
 .UNSPECIFIED., .F., .F.,
 ( 4, 3, 3, 4 ),
 ( 1.474514954580286030E-17, 0.0006253016069560837905, 0.001250604074564929313, 0.002501455912506545670 ),
 .UNSPECIFIED. ) ;
#2758 = CARTESIAN_POINT ( 'NONE',  ( 6.204703633549690345, 40.76208216824731778, -14.16423886937410259 ) ) ;
#2759 = CARTESIAN_POINT ( 'NONE',  ( 12.91533473730992121, 9.522018677488171434, 10.88017736071110164 ) ) ;
#2760 = CARTESIAN_POINT ( 'NONE',  ( 11.39601241150452182, -0.03417435944610275333, 11.22534175661874301 ) ) ;
#2761 = CARTESIAN_POINT ( 'NONE',  ( 4.999999999999999112, 60.50000000000000000, -6.000000000000000000 ) ) ;
#2762 = CARTESIAN_POINT ( 'NONE',  ( 17.96484262340118221, 61.18868534415482685, -7.964842623401177768 ) ) ;
#2763 = CARTESIAN_POINT ( 'NONE',  ( 2.791683348922240793, 16.63393115100078745, 7.208316651077764092 ) ) ;
#2764 = CARTESIAN_POINT ( 'NONE',  ( -5.070949216137130122, -24.98410106516922013, 3.999999999995160316 ) ) ;
#2765 = ORIENTED_EDGE ( 'NONE', *, *, #69274, .F. ) ;
#2766 = CYLINDRICAL_SURFACE ( 'NONE', #37890, 0.5000000000000004441 ) ;
#2767 = ORIENTED_EDGE ( 'NONE', *, *, #73708, .F. ) ;
#2768 = CARTESIAN_POINT ( 'NONE',  ( 10.00000000000000178, 27.25893115100078390, 9.846743663894594434 ) ) ;
#2769 = ORIENTED_EDGE ( 'NONE', *, *, #81676, .T. ) ;
#2770 = CARTESIAN_POINT ( 'NONE',  ( 10.00000000000000000, 35.55374883491396787, -14.16423886937410082 ) ) ;
#2771 = CARTESIAN_POINT ( 'NONE',  ( 19.84674366389459621, 28.50893115100078745, 7.409399052514197653E-17 ) ) ;
#2772 = CARTESIAN_POINT ( 'NONE',  ( 2.035157376598822676, 47.43868534415484817, -7.964842623401177768 ) ) ;
#2773 = CARTESIAN_POINT ( 'NONE',  ( -15.00000000000000000, 83.99999999999998579, -8.000000000000000000 ) ) ;
#2774 = ORIENTED_EDGE ( 'NONE', *, *, #75792, .F. ) ;
#2775 = CARTESIAN_POINT ( 'NONE',  ( 0.5774900079438590739, 42.64701867748816966, -5.440088680355550821 ) ) ;
#2776 = ADVANCED_FACE ( 'NONE', ( #42297 ), #92491, .T. ) ;
#2777 = AXIS2_PLACEMENT_3D ( 'NONE', #29083, #61553, #15591 ) ;
#2778 = CARTESIAN_POINT ( 'NONE',  ( -12.81628187352647252, -5.668031996736239364, 3.434112377981066722 ) ) ;
#2779 = VERTEX_POINT ( 'NONE', #1745 ) ;
#2780 = CARTESIAN_POINT ( 'NONE',  ( -4.164238869374098151, 1.595415501580634388, -3.795296366450310543 ) ) ;
#2781 = ORIENTED_EDGE ( 'NONE', *, *, #92714, .T. ) ;
#2782 = EDGE_CURVE ( 'NONE', #60677, #50878, #54707, .T. ) ;
#2783 = ORIENTED_EDGE ( 'NONE', *, *, #80156, .F. ) ;
#2784 = CARTESIAN_POINT ( 'NONE',  ( 13.43411237798106583, 27.66530133659708568, -12.81628187352647252 ) ) ;
#2785 = AXIS2_PLACEMENT_3D ( 'NONE', #79007, #94012, #16555 ) ;
#2786 = CARTESIAN_POINT ( 'NONE',  ( 17.20831665107776587, 22.88393115100078745, 7.208316651077764980 ) ) ;
#2787 = CARTESIAN_POINT ( 'NONE',  ( 0.5774900079438607392, 3.480352010821504027, 5.440088680355550821 ) ) ;
#2788 = CARTESIAN_POINT ( 'NONE',  ( 0.000000000000000000, -97.00000000000000000, -3.750000000000000000 ) ) ;
#2789 = CARTESIAN_POINT ( 'NONE',  ( 12.63842701281683922, 34.55059781766745886, -9.846743663894590881 ) ) ;
#2790 = STYLED_ITEM ( 'NONE', ( #32997 ), #31045 ) ;
#2791 = VECTOR ( 'NONE', #20359, 1000.000000000000000 ) ;
#2792 = CIRCLE ( 'NONE', #5982, 2.250000000000001332 ) ;
#2793 = CARTESIAN_POINT ( 'NONE',  ( 20.88017736071110164, 55.35535201082149825, 2.915334737309930979 ) ) ;
#2794 = DIRECTION ( 'NONE',  ( 0.000000000000000000, -0.000000000000000000, -1.000000000000000000 ) ) ;
#2795 = CARTESIAN_POINT ( 'NONE',  ( 19.42250999205614193, 65.14701867748817676, 5.440088680355555262 ) ) ;
#2796 = CARTESIAN_POINT ( 'NONE',  ( 9.402796353261049234, 0.3640475087720986824, 11.68706210897764031 ) ) ;
#2797 = CARTESIAN_POINT ( 'NONE',  ( 17.20831665107776587, 9.133931151000787452, -7.208316651077762316 ) ) ;
#2798 = CARTESIAN_POINT ( 'NONE',  ( 6.565887622018943937, 13.08196800326374998, -12.81628187352647608 ) ) ;
#2799 = DIRECTION ( 'NONE',  ( -0.6038238647436497963, 0.7971177707001910751, 1.214306433183775537E-14 ) ) ;
#2800 = CARTESIAN_POINT ( 'NONE',  ( 0.1532563361054082862, 41.21726448433411605, 2.638427012816831674 ) ) ;
#2801 = CARTESIAN_POINT ( 'NONE',  ( -1.099225684535947600, 64.54030133659709634, 6.408140936763237150 ) ) ;
#2802 = CARTESIAN_POINT ( 'NONE',  ( 2.917880565312950480, 10.97041550158063572, -12.26659068614894821 ) ) ;
#2803 = CARTESIAN_POINT ( 'NONE',  ( 10.00000000000000178, 32.25893115100078745, 9.846743663894594434 ) ) ;
#2804 = CARTESIAN_POINT ( 'NONE',  ( 0.6178305044545818747, 28.49863466993041783, -9.382169495545419124 ) ) ;
#2806 = PRESENTATION_STYLE_ASSIGNMENT (( #71283 ) ) ;
#2805 = CARTESIAN_POINT ( 'NONE',  ( 2.603489959281115151, 16.58210964143323807, 6.499999999999462652 ) ) ;
#2807 = CARTESIAN_POINT ( 'NONE',  ( 17.96484262340118221, 44.93868534415483396, 7.964842623401181321 ) ) ;
#2808 = CARTESIAN_POINT ( 'NONE',  ( 10.00000000000000178, 5.373634669930420493, 12.81628187352647608 ) ) ;
#2809 = PRODUCT_DEFINITION_SHAPE ( 'NONE', 'NONE',  #98994 ) ;
#2810 = CARTESIAN_POINT ( 'NONE',  ( 13.75543905097946151, 14.95037102630295500, -5.333404663735534790 ) ) ;
#2811 = CARTESIAN_POINT ( 'NONE',  ( 14.92337183194729633, 27.67559781766745530, 8.527530157486181039 ) ) ;
#2813 = EDGE_CURVE ( 'NONE', #50944, #76767, #55120, .T. ) ;
#2812 = CARTESIAN_POINT ( 'NONE',  ( 4.559911319644449179, 23.89701867748817321, 9.422509992056141925 ) ) ;
#2814 = CARTESIAN_POINT ( 'NONE',  ( 3.591859063236761518, 29.95696800326375708, 11.09922568453594849 ) ) ;
#2815 = PRESENTATION_STYLE_ASSIGNMENT (( #41300 ) ) ;
#2816 = CARTESIAN_POINT ( 'NONE',  ( 4.559911319644449179, 17.23035201082150536, -9.422509992056141925 ) ) ;
#2817 = AXIS2_PLACEMENT_3D ( 'NONE', #13902, #44387, #20418 ) ;
#2818 = ORIENTED_EDGE ( 'NONE', *, *, #9036, .F. ) ;
#2819 = CARTESIAN_POINT ( 'NONE',  ( 20.88017736071110164, 55.35535201082149825, 2.915334737309930979 ) ) ;
#2820 = CARTESIAN_POINT ( 'NONE',  ( 0.5774900079438590739, 2.647018677488170990, -5.440088680355550821 ) ) ;
#2822 = CARTESIAN_POINT ( 'NONE',  ( 20.88017736071110875, 30.77201867748816966, -2.915334737309920765 ) ) ;
#2821 = CARTESIAN_POINT ( 'NONE',  ( 1.472469842513823179, 46.42559781766745175, 4.923371831947296329 ) ) ;
#2823 = CARTESIAN_POINT ( 'NONE',  ( 17.96484262340118221, 41.18868534415484106, -7.964842623401177768 ) ) ;
#2824 = CARTESIAN_POINT ( 'NONE',  ( 2.035157376598824452, 13.68868534415483751, 7.964842623401179544 ) ) ;
#2825 = CARTESIAN_POINT ( 'NONE',  ( 64.56412365047461321, 11.99999999999999467, 9.500000000000000000 ) ) ;
#2826 = CARTESIAN_POINT ( 'NONE',  ( 14.92337183194729988, 34.34226448433411605, -8.527530157486177487 ) ) ;
#2827 = CARTESIAN_POINT ( 'NONE',  ( 1.274849032794280523, 48.57228050351032067, 6.499999999999960032 ) ) ;
#2828 = CARTESIAN_POINT ( 'NONE',  ( 19.50000000000000711, 79.40087001978915282, -4.500000000000000888 ) ) ;
#2829 = CARTESIAN_POINT ( 'NONE',  ( 0.000000000000000000, 14.49999999999999822, 0.000000000000000000 ) ) ;
#2830 = CARTESIAN_POINT ( 'NONE',  ( 13.79529636645030344, 23.26208216824730002, 14.16423886937410614 ) ) ;
#2831 = CARTESIAN_POINT ( 'NONE',  ( -3.999999999999999112, 1.639999999999999014, 0.000000000000000000 ) ) ;
#2832 = ORIENTED_EDGE ( 'NONE', *, *, #61604, .F. ) ;
#2833 = CARTESIAN_POINT ( 'NONE',  ( -4.164238869374098151, 61.59541550158063217, -3.795296366450310543 ) ) ;
#2834 = CARTESIAN_POINT ( 'NONE',  ( 19.84674366389459621, 28.50893115100078745, 7.409399052514197653E-17 ) ) ;
#2836 =( NAMED_UNIT ( * ) PLANE_ANGLE_UNIT ( ) SI_UNIT ( $, .RADIAN. ) );
#2835 = CARTESIAN_POINT ( 'NONE',  ( -9.000000000000001776, 80.99999999999994316, 2.900000000000000355 ) ) ;
#2837 = CARTESIAN_POINT ( 'NONE',  ( 7.084665262690076126, 54.10535201082151247, 10.88017736071109987 ) ) ;
#2838 = CARTESIAN_POINT ( 'NONE',  ( 19.38216949554541557, 62.24863466993041072, -9.382169495545420901 ) ) ;
#2839 = ORIENTED_EDGE ( 'NONE', *, *, #66128, .F. ) ;
#2840 = CARTESIAN_POINT ( 'NONE',  ( 7.084665262690076126, 37.02201867748817676, -10.88017736071110164 ) ) ;
#2841 = DIRECTION ( 'NONE',  ( 0.2672383760782636175, 0.000000000000000000, -0.9636304532086211738 ) ) ;
#2842 = CARTESIAN_POINT ( 'NONE',  ( -1.099225684535947600, 8.706968003263753531, -6.408140936763238038 ) ) ;
#2843 = B_SPLINE_CURVE_WITH_KNOTS ( 'NONE', 3,
 ( #83444, #37960, #46425, #98476, #61908, #46907 ),
 .UNSPECIFIED., .F., .F.,
 ( 4, 2, 4 ),
 ( 0.0002800098399050243367, 0.0006862151655664761127, 0.001092420491227927889 ),
 .UNSPECIFIED. ) ;
#2844 = CARTESIAN_POINT ( 'NONE',  ( 0.1532563361054083140, 11.00893115100078568, 1.131784320476157264E-15 ) ) ;
#2845 = ORIENTED_EDGE ( 'NONE', *, *, #14494, .T. ) ;
#2846 = CARTESIAN_POINT ( 'NONE',  ( 5.076628168052704559, 0.1755978176674514724, -8.527530157486179263 ) ) ;
#2847 = LINE ( 'NONE', #10328, #31688 ) ;
#2848 = CARTESIAN_POINT ( 'NONE',  ( 10.00000000000000178, 53.05374883491396787, 14.16423886937410082 ) ) ;
#2849 = CARTESIAN_POINT ( 'NONE',  ( -0.3689425029237881626, 22.42874883491397142, 10.36894250292379027 ) ) ;
#2850 = AXIS2_PLACEMENT_3D ( 'NONE', #93611, #55110, #25148 ) ;
#2851 = CARTESIAN_POINT ( 'NONE',  ( 19.42250999205614548, 45.98035201082150536, -5.440088680355545492 ) ) ;
#2852 = CARTESIAN_POINT ( 'NONE',  ( -12.74414838903283531, 7.504711912673099032E-16, 7.178093659841884744 ) ) ;
#2853 = DIRECTION ( 'NONE',  ( -0.000000000000000000, -1.000000000000000000, -0.000000000000000000 ) ) ;
#2854 = CARTESIAN_POINT ( 'NONE',  ( 0.1532563361054083140, 6.008931151000784787, 1.131784320476157264E-15 ) ) ;
#2855 = SURFACE_STYLE_USAGE ( .BOTH. , #48318 ) ;
#2856 = CARTESIAN_POINT ( 'NONE',  ( 0.1532563361054083140, 21.00893115100078745, 1.131784320476157264E-15 ) ) ;
#2857 = CARTESIAN_POINT ( 'NONE',  ( 10.00000000000000178, 22.25893115100078745, 9.846743663894594434 ) ) ;
#2858 = CARTESIAN_POINT ( 'NONE',  ( 0.1532563361054082862, 46.21726448433411605, 2.638427012816831674 ) ) ;
#2859 = AXIS2_PLACEMENT_3D ( 'NONE', #20883, #73870, #34882 ) ;
#2860 = CARTESIAN_POINT ( 'NONE',  ( 2.035157376598824452, 28.68868534415484106, 7.964842623401179544 ) ) ;
#2861 = CIRCLE ( 'NONE', #97072, 15.00000000000000000 ) ;
#2862 = VECTOR ( 'NONE', #79215, 1000.000000000000000 ) ;
#2863 = CARTESIAN_POINT ( 'NONE',  ( 10.00000000000000178, 35.37363466993042493, 12.81628187352647608 ) ) ;
#2864 = CARTESIAN_POINT ( 'NONE',  ( 4.559911319644449179, 53.89701867748817676, 9.422509992056141925 ) ) ;
#2865 = CARTESIAN_POINT ( 'NONE',  ( 14.92337183194729633, 22.67559781766745175, 8.527530157486181039 ) ) ;
#2867 = CARTESIAN_POINT ( 'NONE',  ( 17.20831665107776587, 17.88393115100078745, 7.208316651077764980 ) ) ;
#2866 = CARTESIAN_POINT ( 'NONE',  ( 24.16423886937409904, 44.09541550158063927, 3.795296366450317205 ) ) ;
#2869 = EDGE_CURVE ( 'NONE', #16281, #17551, #93201, .T. ) ;
#2868 = LINE ( 'NONE', #39860, #28051 ) ;
#2870 = ADVANCED_FACE ( 'NONE', ( #78203 ), #33188, .F. ) ;
#2871 = CARTESIAN_POINT ( 'NONE',  ( 17.20831665107776587, 52.88393115100078035, 7.208316651077764980 ) ) ;
#2873 = CARTESIAN_POINT ( 'NONE',  ( -4.164238869374099927, 7.012082168247302683, 3.795296366450308767 ) ) ;
#2872 = CARTESIAN_POINT ( 'NONE',  ( 18.52753015748618282, 48.92559781766745886, -4.923371831947291888 ) ) ;
#2874 = CARTESIAN_POINT ( 'NONE',  ( 10.00000000000000178, 38.05374883491396787, 14.16423886937410082 ) ) ;
#2875 = CARTESIAN_POINT ( 'NONE',  ( 0.1532563361054082862, 26.21726448433411605, 2.638427012816831674 ) ) ;
#2876 = CARTESIAN_POINT ( 'NONE',  ( 20.88017736071110164, 25.35535201082150891, 2.915334737309930979 ) ) ;
#2877 = CARTESIAN_POINT ( 'NONE',  ( 20.88017736071110164, 45.35535201082149115, 2.915334737309930979 ) ) ;
#2878 = CARTESIAN_POINT ( 'NONE',  ( 12.91533473730993009, 31.60535201082150891, -10.88017736071109987 ) ) ;
#2879 = ORIENTED_EDGE ( 'NONE', *, *, #62271, .F. ) ;
#2880 = CARTESIAN_POINT ( 'NONE',  ( 21.09922568453595559, 32.04030133659708923, -6.408140936763230044 ) ) ;
#2881 = CARTESIAN_POINT ( 'NONE',  ( 20.88017736071110875, 55.77201867748816966, -2.915334737309920765 ) ) ;
#2882 = ORIENTED_EDGE ( 'NONE', *, *, #91334, .T. ) ;
#2883 = CARTESIAN_POINT ( 'NONE',  ( -0.8801773607110991993, 62.85535201082150536, -2.915334737309923874 ) ) ;
#2884 = ORIENTED_EDGE ( 'NONE', *, *, #5462, .T. ) ;
#2885 = CARTESIAN_POINT ( 'NONE',  ( 15.44008868035555260, 59.73035201082151247, 9.422509992056143702 ) ) ;
#2886 = CARTESIAN_POINT ( 'NONE',  ( 0.5774900079438590739, 2.647018677488170990, -5.440088680355550821 ) ) ;
#2887 = CARTESIAN_POINT ( 'NONE',  ( 13.07751017357379730, 4.171195230237741069E-16, 6.263284095430596388 ) ) ;
#2888 = DIRECTION ( 'NONE',  ( -5.151434834260726979E-14, 0.000000000000000000, 1.000000000000000000 ) ) ;
#2889 = CARTESIAN_POINT ( 'NONE',  ( 10.00000000000000000, 65.55374883491396076, -14.16423886937410082 ) ) ;
#2890 = CARTESIAN_POINT ( 'NONE',  ( 1.472469842513823179, 15.59226448433411960, -4.923371831947296329 ) ) ;
#2891 = EDGE_CURVE ( 'NONE', #49181, #13782, #9431, .T. ) ;
#2892 = CARTESIAN_POINT ( 'NONE',  ( 20.36894250292379382, 3.678748834913967869, 10.36894250292379205 ) ) ;
#2893 = CARTESIAN_POINT ( 'NONE',  ( 1.472469842513823179, 0.5922644843341181575, -4.923371831947296329 ) ) ;
#2894 = CARTESIAN_POINT ( 'NONE',  ( 10.00000000000000000, 6.813685344154838397, -10.88017736071110342 ) ) ;
#2895 = CARTESIAN_POINT ( 'NONE',  ( 18.52753015748617571, 48.09226448433412315, 4.923371831947298993 ) ) ;
#2896 = ORIENTED_EDGE ( 'NONE', *, *, #42226, .T. ) ;
#2897 = ADVANCED_FACE ( 'NONE', ( #61715 ), #32200, .T. ) ;
#2898 = CARTESIAN_POINT ( 'NONE',  ( 19.84674366389459266, 53.30059781766744464, 2.638427012816836559 ) ) ;
#2899 = EDGE_LOOP ( 'NONE', ( #31606, #88580, #57841, #77361 ) ) ;
#2900 = CARTESIAN_POINT ( 'NONE',  ( 12.91533473730992121, 59.52201867748816966, 10.88017736071110164 ) ) ;
#2901 = CARTESIAN_POINT ( 'NONE',  ( 12.63842701281683034, 57.46726448433411605, 9.846743663894596210 ) ) ;
#2902 = DIRECTION ( 'NONE',  ( 0.000000000000000000, 0.000000000000000000, 1.000000000000000000 ) ) ;
#2903 = CARTESIAN_POINT ( 'NONE',  ( -0.8801773607111008646, 53.27201867748816966, 2.915334737309923430 ) ) ;
#2904 = CARTESIAN_POINT ( 'NONE',  ( 17.96484262340118221, 9.938685344154839285, 7.964842623401181321 ) ) ;
#2905 = AXIS2_PLACEMENT_3D ( 'NONE', #26099, #87086, #58050 ) ;
#2906 = CARTESIAN_POINT ( 'NONE',  ( 13.43411237798106583, 42.66530133659707502, -12.81628187352647252 ) ) ;
#2907 = CARTESIAN_POINT ( 'NONE',  ( 0.000000000000000000, 14.49999999999999822, 0.000000000000000000 ) ) ;
#2908 = EDGE_LOOP ( 'NONE', ( #82923, #13926, #7024, #19525 ) ) ;
#2909 = CARTESIAN_POINT ( 'NONE',  ( 3.591859063236761518, 34.95696800326375353, 11.09922568453594849 ) ) ;
#2910 = CARTESIAN_POINT ( 'NONE',  ( -0.8801773607111008646, 33.27201867748817676, 2.915334737309923430 ) ) ;
#2911 = ORIENTED_EDGE ( 'NONE', *, *, #30927, .T. ) ;
#2912 = CARTESIAN_POINT ( 'NONE',  ( -2.614810775378867191, 35.00346125376525919, -9.500000000000000000 ) ) ;
#2913 = AXIS2_PLACEMENT_3D ( 'NONE', #54169, #93154, #31664 ) ;
#2914 = CARTESIAN_POINT ( 'NONE',  ( 2.791683348922237240, 10.38393115100078390, -7.208316651077763204 ) ) ;
#2915 = CARTESIAN_POINT ( 'NONE',  ( -1.099225684535947600, -0.4596986634029132657, 6.408140936763237150 ) ) ;
#2917 = CARTESIAN_POINT ( 'NONE',  ( 19.84674366389459266, 48.30059781766745175, 2.638427012816836559 ) ) ;
#2916 = CARTESIAN_POINT ( 'NONE',  ( 10.00000000000000000, 9.758931151000785675, -9.846743663894594434 ) ) ;
#2918 = CARTESIAN_POINT ( 'NONE',  ( -10.57641974390271322, -40.47698476369465936, 3.750000000000000000 ) ) ;
#2919 = CARTESIAN_POINT ( 'NONE',  ( -1.780824192092605562, 0.5000000000000004441, 14.89391369643512064 ) ) ;
#2920 = CARTESIAN_POINT ( 'NONE',  ( 19.84674366389459266, 43.30059781766744464, 2.638427012816836559 ) ) ;
#2921 = CARTESIAN_POINT ( 'NONE',  ( 10.58840669699852199, -98.14374106289703548, 3.750000000000000000 ) ) ;
#2922 = LINE ( 'NONE', #56872, #56403 ) ;
#2925 = CARTESIAN_POINT ( 'NONE',  ( 0.7575892234030736638, 0.2306972965111896423, 14.92193396517714454 ) ) ;
#2924 = TOROIDAL_SURFACE ( 'NONE', #6113, 14.49999999999999822, 0.5000000000000000000 ) ;
#2923 = CARTESIAN_POINT ( 'NONE',  ( 5.076628168052704559, 25.17559781766745175, -8.527530157486179263 ) ) ;
#2926 = FACE_OUTER_BOUND ( 'NONE', #51310, .T. ) ;
#2928 = ORIENTED_EDGE ( 'NONE', *, *, #29948, .T. ) ;
#2927 = CARTESIAN_POINT ( 'NONE',  ( 10.00000000000000000, 64.75893115100078035, -9.846743663894594434 ) ) ;
#2929 = CIRCLE ( 'NONE', #60423, 14.49999999999999822 ) ;
#2930 = CARTESIAN_POINT ( 'NONE',  ( 0.8952175423694859191, 7.601608292538859502, -5.990408912944324094 ) ) ;
#2931 = CARTESIAN_POINT ( 'NONE',  ( 13.43411237798106583, 22.66530133659708923, -12.81628187352647252 ) ) ;
#2932 = CARTESIAN_POINT ( 'NONE',  ( 18.52753015748617571, 38.09226448433412315, 4.923371831947298993 ) ) ;
#2933 = CARTESIAN_POINT ( 'NONE',  ( 13.99999999999999822, 61.50000000000000711, -6.500000000000000888 ) ) ;
#2934 = CARTESIAN_POINT ( 'NONE',  ( -4.164238869374098151, 41.59541550158061796, -3.795296366450310543 ) ) ;
#2935 = CARTESIAN_POINT ( 'NONE',  ( 19.84674366389459621, 18.50893115100078745, 7.409399052514197653E-17 ) ) ;
#2936 = CARTESIAN_POINT ( 'NONE',  ( -0.1503990784575328643, 40.12777174578613426, 6.262539305110068177 ) ) ;
#2937 = CARTESIAN_POINT ( 'NONE',  ( 6.204703633549690345, 45.76208216824729647, -14.16423886937410259 ) ) ;
#2938 = CARTESIAN_POINT ( 'NONE',  ( 1.472469842513823179, 60.59226448433412315, -4.923371831947296329 ) ) ;
#2939 = CARTESIAN_POINT ( 'NONE',  ( 10.00000000000000178, 68.05374883491397497, 14.16423886937410082 ) ) ;
#2940 = CARTESIAN_POINT ( 'NONE',  ( 17.08211943468705840, 20.13708216824730357, -12.26659068614894466 ) ) ;
#2941 = CARTESIAN_POINT ( 'NONE',  ( 13.79529636645031943, 40.34541550158063217, -14.16423886937409904 ) ) ;
#2942 = FILL_AREA_STYLE ('',( #40929 ) ) ;
#2944 = CARTESIAN_POINT ( 'NONE',  ( 19.84674366389459266, 53.71726448433411605, -2.638427012816827677 ) ) ;
#2943 = CARTESIAN_POINT ( 'NONE',  ( 1.274849032794317383, 27.55509018479935790, -6.500000000000010658 ) ) ;
#2945 = CARTESIAN_POINT ( 'NONE',  ( 20.88017736071110519, 30.56368534415484106, 2.639326808657452039E-16 ) ) ;
#2946 = CARTESIAN_POINT ( 'NONE',  ( 3.881909499400429286, -2.725328507790710552E-15, -14.10103859407594840 ) ) ;
#2947 = ADVANCED_FACE ( 'NONE', ( #70724 ), #63680, .F. ) ;
#2948 = CARTESIAN_POINT ( 'NONE',  ( 9.210000967481738243, -9.315410972688546565, 3.750000000000001776 ) ) ;
#2949 = CARTESIAN_POINT ( 'NONE',  ( 16.40814093676324603, 62.45696800326376064, -11.09922568453594671 ) ) ;
#2950 = CARTESIAN_POINT ( 'NONE',  ( -3.795296366450322534, 5.762082168247310676, -14.16423886937409904 ) ) ;
#2951 = CARTESIAN_POINT ( 'NONE',  ( 7.361572987183169658, 54.96726448433413026, -9.846743663894592657 ) ) ;
#2952 = CARTESIAN_POINT ( 'NONE',  ( 5.076628168052703671, 61.84226448433412315, 8.527530157486179263 ) ) ;
#2953 = VERTEX_POINT ( 'NONE', #77220 ) ;
#2954 = CARTESIAN_POINT ( 'NONE',  ( -2.266590686148945544, 21.38708216824730357, -7.082119434687050408 ) ) ;
#2955 = LINE ( 'NONE', #77940, #13527 ) ;
#2957 = CARTESIAN_POINT ( 'NONE',  ( 0.000000000000000000, 0.000000000000000000, 0.000000000000000000 ) ) ;
#2956 = CARTESIAN_POINT ( 'NONE',  ( -5.780406540405962801, -39.80436905996668884, -2.500000000000000000 ) ) ;
#2958 = CARTESIAN_POINT ( 'NONE',  ( 12.91533473730992121, 9.522018677488171434, 10.88017736071110164 ) ) ;
#2959 = CARTESIAN_POINT ( 'NONE',  ( 22.81628187352647785, 31.41530133659709279, 3.434112377981063169 ) ) ;
#2960 = DIRECTION ( 'NONE',  ( 1.000000000000000000, 0.000000000000000000, 0.000000000000000000 ) ) ;
#2961 = CARTESIAN_POINT ( 'NONE',  ( 10.00000000000000178, 17.25893115100078745, 9.846743663894594434 ) ) ;
#2962 = CARTESIAN_POINT ( 'NONE',  ( 4.380000000000000782, 1.019547802438464545, -3.750000000000000000 ) ) ;
#2963 = CARTESIAN_POINT ( 'NONE',  ( -0.1503990784575403861, 9.248846992468887862, -6.262539305110056631 ) ) ;
#2964 = CYLINDRICAL_SURFACE ( 'NONE', #23170, 3.000000000000000000 ) ;
#2965 = CARTESIAN_POINT ( 'NONE',  ( 19.42250999205614548, 15.98035201082150714, -5.440088680355545492 ) ) ;
#2966 = CARTESIAN_POINT ( 'NONE',  ( 12.83294900548063744, 0.5000000000000004441, -7.766300266068363101 ) ) ;
#2967 = CARTESIAN_POINT ( 'NONE',  ( 2.035157376598822676, 42.43868534415483396, -7.964842623401177768 ) ) ;
#2968 = CARTESIAN_POINT ( 'NONE',  ( 0.5774900079438590739, 32.64701867748816966, -5.440088680355550821 ) ) ;
#2969 = CARTESIAN_POINT ( 'NONE',  ( 6.565887622018943937, 5.165301336597086568, 12.81628187352647430 ) ) ;
#2970 = CARTESIAN_POINT ( 'NONE',  ( 18.52753015748618282, 63.92559781766745886, -4.923371831947291888 ) ) ;
#2971 = CARTESIAN_POINT ( 'NONE',  ( -45.72097266785441150, 104.7202616008577678, -5.189651444387643586 ) ) ;
#2972 = CARTESIAN_POINT ( 'NONE',  ( 7.361572987183169658, 9.967264484334119601, -9.846743663894592657 ) ) ;
#2973 = EDGE_CURVE ( 'NONE', #97455, #75793, #44509, .T. ) ;
#2974 = ORIENTED_EDGE ( 'NONE', *, *, #76441, .T. ) ;
#2975 = CARTESIAN_POINT ( 'NONE',  ( -0.8801773607111009756, 28.06368534415484106, 1.068504757029289695E-15 ) ) ;
#2976 = CARTESIAN_POINT ( 'NONE',  ( 22.81628187352647785, 26.62363466993042138, 6.195893100308588602E-16 ) ) ;
#2977 = CARTESIAN_POINT ( 'NONE',  ( 19.72487221294570858, 36.86607318730075633, 6.500000000000000888 ) ) ;
#2978 = ADVANCED_FACE ( 'NONE', ( #1258 ), #62208, .T. ) ;
#2979 = CARTESIAN_POINT ( 'NONE',  ( 14.92337183194729988, 64.34226448433412315, -8.527530157486177487 ) ) ;
#2980 = CARTESIAN_POINT ( 'NONE',  ( -0.8801773607111009756, 68.06368534415484817, 1.068504757029289695E-15 ) ) ;
#2981 = EDGE_CURVE ( 'NONE', #27481, #37579, #94009, .T. ) ;
#2982 = CARTESIAN_POINT ( 'NONE',  ( 12.63842701281683922, 9.550597817667449974, -9.846743663894590881 ) ) ;
#2983 = CARTESIAN_POINT ( 'NONE',  ( 6.565887622018943937, 30.16530133659708568, 12.81628187352647430 ) ) ;
#2985 = CARTESIAN_POINT ( 'NONE',  ( -4.838527690343711996, 14.63595249122789177, 14.19819177887725026 ) ) ;
#2984 = CARTESIAN_POINT ( 'NONE',  ( 12.91533473730993009, 56.60535201082151247, -10.88017736071109987 ) ) ;
#2986 = EDGE_LOOP ( 'NONE', ( #97343, #61026, #74294, #78162 ) ) ;
#2987 = DIRECTION ( 'NONE',  ( 0.000000000000000000, 0.000000000000000000, 1.000000000000000000 ) ) ;
#2988 = CARTESIAN_POINT ( 'NONE',  ( 17.96484262340118221, 9.938685344154837509, 7.964842623401181321 ) ) ;
#2989 = B_SPLINE_CURVE_WITH_KNOTS ( 'NONE', 3,
 ( #57896, #80423, #41458, #26417, #48924, #2966 ),
 .UNSPECIFIED., .F., .F.,
 ( 4, 2, 4 ),
 ( 0.0002800591277523076304, 0.0006862649357714271578, 0.001092470743790546848 ),
 .UNSPECIFIED. ) ;
#2990 = CARTESIAN_POINT ( 'NONE',  ( -1.099225684535947600, 58.70696800326375353, -6.408140936763238038 ) ) ;
#2991 = CARTESIAN_POINT ( 'NONE',  ( 5.076628168052704559, 20.17559781766745175, -8.527530157486179263 ) ) ;
#2992 = VECTOR ( 'NONE', #61922, 1000.000000000000000 ) ;
#2993 = CARTESIAN_POINT ( 'NONE',  ( -0.8801773607110991993, 7.855352010821504471, -2.915334737309923874 ) ) ;
#2994 = CARTESIAN_POINT ( 'NONE',  ( 14.92337183194729988, 24.34226448433411960, -8.527530157486177487 ) ) ;
#2995 = CARTESIAN_POINT ( 'NONE',  ( -4.164238869374099039, 51.80374883491396787, 8.674139862899312516E-16 ) ) ;
#2996 = ORIENTED_EDGE ( 'NONE', *, *, #76081, .F. ) ;
#2997 = CARTESIAN_POINT ( 'NONE',  ( 7.084665262690076126, 12.02201867748817143, -10.88017736071110164 ) ) ;
#2998 = STYLED_ITEM ( 'NONE', ( #39152 ), #60167 ) ;
#2999 = CARTESIAN_POINT ( 'NONE',  ( 12.91533473730993009, 16.60535201082150891, -10.88017736071109987 ) ) ;
#3000 = LINE ( 'NONE', #17985, #910 ) ;
#3001 = AXIS2_PLACEMENT_3D ( 'NONE', #73934, #5463, #59417 ) ;
#3002 = ORIENTED_EDGE ( 'NONE', *, *, #70897, .T. ) ;
#3003 = LINE ( 'NONE', #65925, #79619 ) ;
#3004 = CARTESIAN_POINT ( 'NONE',  ( -0.8801773607111008646, 28.27201867748817321, 2.915334737309923430 ) ) ;
#3005 = CARTESIAN_POINT ( 'NONE',  ( 0.1532563361054100626, 60.80059781766744464, -2.638427012816831230 ) ) ;
#3006 = CARTESIAN_POINT ( 'NONE',  ( 6.565887622018943937, 48.08196800326375353, -12.81628187352647608 ) ) ;
#3007 = CARTESIAN_POINT ( 'NONE',  ( 0.000000000000000000, 15.00000000000000000, 0.000000000000000000 ) ) ;
#3008 = CARTESIAN_POINT ( 'NONE',  ( -2.266590686148945544, 21.38708216824730357, -7.082119434687050408 ) ) ;
#3009 = CARTESIAN_POINT ( 'NONE',  ( 15.44008868035555793, 36.39701867748816966, -9.422509992056140149 ) ) ;
#3010 = CARTESIAN_POINT ( 'NONE',  ( 7.084665262690076126, 22.02201867748817321, -10.88017736071110164 ) ) ;
#3011 = CARTESIAN_POINT ( 'NONE',  ( 12.63842701281683922, 49.55059781766744464, -9.846743663894590881 ) ) ;
#3012 = CARTESIAN_POINT ( 'NONE',  ( 7.684764310694791156, 15.00000000000000000, 12.88194075009940498 ) ) ;
#3013 = CARTESIAN_POINT ( 'NONE',  ( 19.84674366389459266, 33.71726448433410894, -2.638427012816827677 ) ) ;
#3014 = EDGE_CURVE ( 'NONE', #74488, #1418, #76428, .T. ) ;
#3015 = CARTESIAN_POINT ( 'NONE',  ( 7.361572987183170547, 12.05059781766744997, 9.846743663894590881 ) ) ;
#3016 = CARTESIAN_POINT ( 'NONE',  ( -12.81628187352647963, -31.08469866340290721, -3.434112377981046293 ) ) ;
#3017 = ORIENTED_EDGE ( 'NONE', *, *, #18470, .F. ) ;
#3018 = MECHANICAL_DESIGN_GEOMETRIC_PRESENTATION_REPRESENTATION (  '', ( #19187 ), #95778 ) ;
#3019 = CARTESIAN_POINT ( 'NONE',  ( 20.88017736071110519, 15.56368534415483751, 2.639326808657452039E-16 ) ) ;
#3020 = CARTESIAN_POINT ( 'NONE',  ( 0.1532563361054100626, 5.800597817667452638, -2.638427012816831230 ) ) ;
#3021 = CARTESIAN_POINT ( 'NONE',  ( 5.076628168052703671, 66.84226448433412315, 8.527530157486179263 ) ) ;
#3023 = CARTESIAN_POINT ( 'NONE',  ( 2.035157376598824452, 48.68868534415483396, 7.964842623401179544 ) ) ;
#3022 = CARTESIAN_POINT ( 'NONE',  ( 10.00000000000000000, 41.81368534415484106, -10.88017736071110342 ) ) ;
#3025 = CARTESIAN_POINT ( 'NONE',  ( 22.81628187352647785, 46.62363466993041783, 6.195893100308588602E-16 ) ) ;
#3024 = CARTESIAN_POINT ( 'NONE',  ( 2.035157376598824452, 23.68868534415484461, 7.964842623401179544 ) ) ;
#3026 = CARTESIAN_POINT ( 'NONE',  ( 10.00000000000000178, 28.05374883491396787, 14.16423886937410082 ) ) ;
#3027 = LINE ( 'NONE', #49469, #4344 ) ;
#3028 = CARTESIAN_POINT ( 'NONE',  ( 13.43411237798106583, 57.66530133659708923, -12.81628187352647252 ) ) ;
#3029 = ORIENTED_EDGE ( 'NONE', *, *, #67068, .F. ) ;
#3030 = CARTESIAN_POINT ( 'NONE',  ( 10.00000000000000178, 52.25893115100078745, 9.846743663894594434 ) ) ;
#3031 = CARTESIAN_POINT ( 'NONE',  ( 4.559911319644449179, 32.23035201082150536, -9.422509992056141925 ) ) ;
#3032 = ORIENTED_EDGE ( 'NONE', *, *, #52405, .T. ) ;
#3033 = CARTESIAN_POINT ( 'NONE',  ( 14.92337183194729633, 2.675597817667451750, 8.527530157486181039 ) ) ;
#3034 = DIRECTION ( 'NONE',  ( 0.000000000000000000, 1.000000000000000000, 0.000000000000000000 ) ) ;
#3035 = VECTOR ( 'NONE', #87176, 1000.000000000000000 ) ;
#3036 = CARTESIAN_POINT ( 'NONE',  ( 12.63842701281683034, 22.46726448433411605, 9.846743663894596210 ) ) ;
#3037 = CARTESIAN_POINT ( 'NONE',  ( 1.472469842513823179, 1.425597817667451528, 4.923371831947296329 ) ) ;
#3038 = CARTESIAN_POINT ( 'NONE',  ( 18.52753015748618282, 3.925597817667451306, -4.923371831947291888 ) ) ;
#3039 = CARTESIAN_POINT ( 'NONE',  ( 2.035157376598824452, 58.68868534415482685, 7.964842623401179544 ) ) ;
#3040 = CARTESIAN_POINT ( 'NONE',  ( 15.44008868035555793, 66.39701867748817676, -9.422509992056140149 ) ) ;
#3041 = ORIENTED_EDGE ( 'NONE', *, *, #39008, .T. ) ;
#3042 = DIRECTION ( 'NONE',  ( 0.000000000000000000, 1.000000000000000000, 0.000000000000000000 ) ) ;
#3043 = CARTESIAN_POINT ( 'NONE',  ( 17.20831665107776587, 52.88393115100078035, 7.208316651077764980 ) ) ;
#3044 = VERTEX_POINT ( 'NONE', #33669 ) ;
#3045 = CARTESIAN_POINT ( 'NONE',  ( -12.25993886608615568, 14.49999999999999112, 8.642563219313586842 ) ) ;
#3046 = CARTESIAN_POINT ( 'NONE',  ( -4.164238869374099927, 7.012082168247302683, 3.795296366450308767 ) ) ;
#3047 = CARTESIAN_POINT ( 'NONE',  ( 3.059999999999993392, 76.92054879330447648, -9.500000000000000000 ) ) ;
#3048 = CARTESIAN_POINT ( 'NONE',  ( 6.204703633549690345, 7.845415501580634832, 14.16423886937410082 ) ) ;
#3049 = CARTESIAN_POINT ( 'NONE',  ( 6.204703633549690345, 32.84541550158063927, 14.16423886937410082 ) ) ;
#3050 = AXIS2_PLACEMENT_3D ( 'NONE', #50301, #35303, #59289 ) ;
#3051 = DIRECTION ( 'NONE',  ( 0.000000000000000000, -1.000000000000000000, 0.000000000000000000 ) ) ;
#3052 = CARTESIAN_POINT ( 'NONE',  ( 17.08211943468705840, 5.137082168247300906, -12.26659068614894466 ) ) ;
#3053 = CARTESIAN_POINT ( 'NONE',  ( 10.00000000000000000, 26.81368534415484106, -10.88017736071110342 ) ) ;
#3054 = FILL_AREA_STYLE_COLOUR ( '', #32366 ) ;
#3055 = ORIENTED_EDGE ( 'NONE', *, *, #7259, .F. ) ;
#3056 = CARTESIAN_POINT ( 'NONE',  ( 19.84674366389459266, 18.30059781766745175, 2.638427012816836559 ) ) ;
#3058 = CARTESIAN_POINT ( 'NONE',  ( 5.076628168052704559, 20.17559781766745175, -8.527530157486179263 ) ) ;
#3057 = CARTESIAN_POINT ( 'NONE',  ( 17.96484262340118221, 56.18868534415484817, -7.964842623401177768 ) ) ;
#3059 = CARTESIAN_POINT ( 'NONE',  ( 22.81628187352647785, 46.62363466993041783, 6.195893100308588602E-16 ) ) ;
#3060 = CARTESIAN_POINT ( 'NONE',  ( 7.361572987183169658, 39.96726448433411605, -9.846743663894592657 ) ) ;
#3061 = EDGE_CURVE ( 'NONE', #29028, #87186, #28152, .T. ) ;
#3062 = MECHANICAL_DESIGN_GEOMETRIC_PRESENTATION_REPRESENTATION (  '', ( #65331 ), #34994 ) ;
#3063 = CARTESIAN_POINT ( 'NONE',  ( 0.1957200283969089960, 25.25733960839544423, 6.499999999999985789 ) ) ;
#3064 = CARTESIAN_POINT ( 'NONE',  ( -0.8801773607111008646, 53.27201867748816966, 2.915334737309923430 ) ) ;
#3065 = CARTESIAN_POINT ( 'NONE',  ( 3.591859063236761518, 29.95696800326375708, 11.09922568453594849 ) ) ;
#3066 = COLOUR_RGB ( '', 0.31764706, 0.68627451, 0.89019608) ;
#3067 = CARTESIAN_POINT ( 'NONE',  ( 12.26659068614894821, -36.11291783175269643, 7.082119434687044190 ) ) ;
#3068 = CARTESIAN_POINT ( 'NONE',  ( 17.20831665107776587, 27.88393115100078390, 7.208316651077764980 ) ) ;
#3069 = CARTESIAN_POINT ( 'NONE',  ( 6.204703633549690345, 15.76208216824730179, -14.16423886937410259 ) ) ;
#3070 = CARTESIAN_POINT ( 'NONE',  ( 15.44008868035555793, 36.39701867748816966, -9.422509992056140149 ) ) ;
#3071 = CARTESIAN_POINT ( 'NONE',  ( 2.917880565312950480, 35.97041550158063217, -12.26659068614894821 ) ) ;
#3072 = CARTESIAN_POINT ( 'NONE',  ( 5.076628168052703671, 51.84226448433412315, 8.527530157486179263 ) ) ;
#3073 = CARTESIAN_POINT ( 'NONE',  ( 10.00000000000000178, 12.25893115100078568, 9.846743663894594434 ) ) ;
#3075 = DIRECTION ( 'NONE',  ( 0.000000000000000000, 0.000000000000000000, 1.000000000000000000 ) ) ;
#3074 = CARTESIAN_POINT ( 'NONE',  ( 6.565887622018943937, 48.08196800326375353, -12.81628187352647608 ) ) ;
#3076 = CARTESIAN_POINT ( 'NONE',  ( 15.44008868035555793, 41.39701867748817676, -9.422509992056140149 ) ) ;
#3077 = CARTESIAN_POINT ( 'NONE',  ( 3.591859063236763294, 18.29030133659708568, -11.09922568453595026 ) ) ;
#3078 = CARTESIAN_POINT ( 'NONE',  ( 0.1532563361054082862, 46.21726448433411605, 2.638427012816831674 ) ) ;
#3079 = CARTESIAN_POINT ( 'NONE',  ( 10.88017736071109987, 20.77201867748817676, -2.915334737309928315 ) ) ;
#3080 = SURFACE_STYLE_FILL_AREA ( #71568 ) ;
#3082 = DIRECTION ( 'NONE',  ( -1.000000000000000000, 0.000000000000000000, 0.000000000000000000 ) ) ;
#3081 = CARTESIAN_POINT ( 'NONE',  ( 7.084665262690076126, 64.10535201082150536, 10.88017736071109987 ) ) ;
#3083 = STYLED_ITEM ( 'NONE', ( #24289 ), #26841 ) ;
#3084 = CARTESIAN_POINT ( 'NONE',  ( -10.60846762071325067, -98.07569628617517310, 3.999999999999999112 ) ) ;
#3085 = DIRECTION ( 'NONE',  ( 0.7933533402912281707, 0.000000000000000000, 0.6087614290087297597 ) ) ;
#3086 = CARTESIAN_POINT ( 'NONE',  ( 10.00000000000000178, 59.31368534415484106, 10.88017736071110342 ) ) ;
#3087 = CARTESIAN_POINT ( 'NONE',  ( 7.084665262690076126, 62.02201867748816966, -10.88017736071110164 ) ) ;
#3088 = CARTESIAN_POINT ( 'NONE',  ( 4.219999999999999751, 10.25000000000000000, -2.500000000000000000 ) ) ;
#3089 = EDGE_CURVE ( 'NONE', #70273, #56575, #35655, .T. ) ;
#3090 = DIRECTION ( 'NONE',  ( 0.000000000000000000, 0.000000000000000000, -1.000000000000000000 ) ) ;
#3091 = CARTESIAN_POINT ( 'NONE',  ( 17.20831665107776587, 22.88393115100078745, 7.208316651077764980 ) ) ;
#3092 = CARTESIAN_POINT ( 'NONE',  ( 10.00000000000000000, 16.81368534415483751, -10.88017736071110342 ) ) ;
#3093 = ADVANCED_FACE ( 'NONE', ( #27655 ), #42188, .T. ) ;
#3094 = CARTESIAN_POINT ( 'NONE',  ( 22.81628187352647785, 1.415301336597087012, 3.434112377981063169 ) ) ;
#3096 = CARTESIAN_POINT ( 'NONE',  ( -5.810050997930829908, -36.09132698039145737, -3.750000000000001332 ) ) ;
#3095 = CARTESIAN_POINT ( 'NONE',  ( -0.8801773607111008646, 23.27201867748817676, 2.915334737309923430 ) ) ;
#3097 = FILL_AREA_STYLE ('',( #78087 ) ) ;
#3098 = CARTESIAN_POINT ( 'NONE',  ( 13.43411237798105340, 20.58196800326374643, 12.81628187352647963 ) ) ;
#3099 = ORIENTED_EDGE ( 'NONE', *, *, #32567, .T. ) ;
#3100 = CARTESIAN_POINT ( 'NONE',  ( 4.559911319644449179, 52.23035201082151247, -9.422509992056141925 ) ) ;
#3101 = CARTESIAN_POINT ( 'NONE',  ( 10.00000000000000178, 47.25893115100078745, 9.846743663894594434 ) ) ;
#3102 = CARTESIAN_POINT ( 'NONE',  ( 13.43411237798105340, 25.58196800326374998, 12.81628187352647963 ) ) ;
#3103 = CARTESIAN_POINT ( 'NONE',  ( 20.88017736071110164, 25.35535201082150891, 2.915334737309930979 ) ) ;
#3104 = CARTESIAN_POINT ( 'NONE',  ( 2.035157376598824452, 38.68868534415483396, 7.964842623401179544 ) ) ;
#3105 = CARTESIAN_POINT ( 'NONE',  ( 10.00000000000000178, 53.05374883491396787, 14.16423886937410082 ) ) ;
#3106 = CARTESIAN_POINT ( 'NONE',  ( 0.1532563361054082862, 41.21726448433411605, 2.638427012816831674 ) ) ;
#3107 = VECTOR ( 'NONE', #88381, 1000.000000000000114 ) ;
#3108 = CARTESIAN_POINT ( 'NONE',  ( 10.00000000000000000, 9.758931151000785675, -9.846743663894594434 ) ) ;
#3109 = CARTESIAN_POINT ( 'NONE',  ( 20.88017736071110519, 45.56368534415484106, 2.639326808657452039E-16 ) ) ;
#3110 = DIRECTION ( 'NONE',  ( -0.1132032137678971873, 0.000000000000000000, -0.9935718556765885667 ) ) ;
#3111 = CARTESIAN_POINT ( 'NONE',  ( -2.266590686148945544, 16.38708216824730357, -7.082119434687050408 ) ) ;
#3112 = DIRECTION ( 'NONE',  ( 0.000000000000000000, 0.000000000000000000, 1.000000000000000000 ) ) ;
#3113 = CARTESIAN_POINT ( 'NONE',  ( 1.472469842513823179, 66.42559781766745175, 4.923371831947296329 ) ) ;
#3114 = EDGE_LOOP ( 'NONE', ( #52086, #27172, #32033, #12314 ) ) ;
#3115 = CARTESIAN_POINT ( 'NONE',  ( 24.16423886937409904, 44.09541550158063927, 3.795296366450317205 ) ) ;
#3116 = CARTESIAN_POINT ( 'NONE',  ( 20.36894250292379738, 44.92874883491396787, -10.36894250292379027 ) ) ;
#3117 = CARTESIAN_POINT ( 'NONE',  ( 0.1532563361054100626, 15.80059781766745353, -2.638427012816831230 ) ) ;
#3118 = CARTESIAN_POINT ( 'NONE',  ( -13.77308431840578962, 90.93904485323390929, 7.896207356394697285 ) ) ;
#3119 = DIRECTION ( 'NONE',  ( -0.9975640502598243087, 0.06975647374412544122, 0.000000000000000000 ) ) ;
#3120 = CARTESIAN_POINT ( 'NONE',  ( -1.099225684535947600, 34.54030133659708923, 6.408140936763237150 ) ) ;
#3121 = CARTESIAN_POINT ( 'NONE',  ( -4.164238869374099927, 42.01208216824728936, 3.795296366450308767 ) ) ;
#3122 = EDGE_CURVE ( 'NONE', #26466, #76186, #72652, .T. ) ;
#3123 = SURFACE_SIDE_STYLE ('',( #64567 ) ) ;
#3124 = CARTESIAN_POINT ( 'NONE',  ( 3.469446951953614189E-15, -2.741068848999210328, 9.846743663894594434 ) ) ;
#3125 = ORIENTED_EDGE ( 'NONE', *, *, #49226, .F. ) ;
#3126 = CARTESIAN_POINT ( 'NONE',  ( 14.92337183194729633, 17.67559781766745175, 8.527530157486181039 ) ) ;
#3127 = LINE ( 'NONE', #32614, #20601 ) ;
#3128 = ORIENTED_EDGE ( 'NONE', *, *, #56101, .T. ) ;
#3130 = CARTESIAN_POINT ( 'NONE',  ( -0.8801773607110991993, 7.855352010821506248, -2.915334737309923874 ) ) ;
#3129 = CARTESIAN_POINT ( 'NONE',  ( 2.035157376598822676, 12.43868534415483751, -7.964842623401177768 ) ) ;
#3132 = CARTESIAN_POINT ( 'NONE',  ( 21.09922568453595559, 7.040301336597086568, -6.408140936763230044 ) ) ;
#3131 = CARTESIAN_POINT ( 'NONE',  ( 0.1532563361054083140, 56.00893115100078745, 1.131784320476157264E-15 ) ) ;
#3133 = CARTESIAN_POINT ( 'NONE',  ( -14.11874224319625348, 14.76984899115443994, -4.887061453530224142 ) ) ;
#3134 = CARTESIAN_POINT ( 'NONE',  ( -2.816281873526473856, 14.12363466993041961, 9.499525473075851096E-16 ) ) ;
#3135 = ORIENTED_EDGE ( 'NONE', *, *, #5338, .T. ) ;
#3136 = CARTESIAN_POINT ( 'NONE',  ( -2.266590686148945544, 57.22041550158063217, 7.082119434687048631 ) ) ;
#3137 = EDGE_LOOP ( 'NONE', ( #4836, #41624, #56935 ) ) ;
#3138 = CARTESIAN_POINT ( 'NONE',  ( -4.164238869374099039, 51.80374883491396787, 8.674139862899312516E-16 ) ) ;
#3139 = ORIENTED_EDGE ( 'NONE', *, *, #48244, .T. ) ;
#3140 = CARTESIAN_POINT ( 'NONE',  ( 2.035157376598824452, 33.68868534415484106, 7.964842623401179544 ) ) ;
#3141 = VECTOR ( 'NONE', #37398, 1000.000000000000114 ) ;
#3142 = CARTESIAN_POINT ( 'NONE',  ( 12.91533473730992121, 39.52201867748817676, 10.88017736071110164 ) ) ;
#3143 = CARTESIAN_POINT ( 'NONE',  ( -0.8801773607111008646, 63.27201867748817676, 2.915334737309923430 ) ) ;
#3144 = CARTESIAN_POINT ( 'NONE',  ( 7.084665262690076126, 32.02201867748816966, -10.88017736071110164 ) ) ;
#3145 = CIRCLE ( 'NONE', #81349, 3.000000000000000000 ) ;
#3146 = CARTESIAN_POINT ( 'NONE',  ( 0.2751277870542911952, 33.21833443783938122, 6.499999999999992006 ) ) ;
#3147 = CARTESIAN_POINT ( 'NONE',  ( 14.92337183194729633, 12.67559781766745353, 8.527530157486181039 ) ) ;
#3148 = ORIENTED_EDGE ( 'NONE', *, *, #73132, .F. ) ;
#3149 = CARTESIAN_POINT ( 'NONE',  ( 11.08989791444925288, -87.81815274839443930, 4.000000000000000000 ) ) ;
#3150 = CARTESIAN_POINT ( 'NONE',  ( 18.52753015748618282, 43.92559781766745175, -4.923371831947291888 ) ) ;
#3151 = DIRECTION ( 'NONE',  ( 0.000000000000000000, 0.000000000000000000, 1.000000000000000000 ) ) ;
#3152 = CARTESIAN_POINT ( 'NONE',  ( -1.099225684535947600, 48.70696800326375353, -6.408140936763238038 ) ) ;
#3153 =( LENGTH_UNIT ( ) NAMED_UNIT ( * ) SI_UNIT ( .MILLI., .METRE. ) );
#3154 = AXIS2_PLACEMENT_3D ( 'NONE', #28845, #89363, #34874 ) ;
#3155 = CARTESIAN_POINT ( 'NONE',  ( -15.00000000000000000, 83.99999999999998579, -7.750000000000000000 ) ) ;
#3156 = CARTESIAN_POINT ( 'NONE',  ( -44.76764016918902200, 105.1727941590568349, 5.383302543209945945 ) ) ;
#3157 = DIRECTION ( 'NONE',  ( 0.000000000000000000, 0.000000000000000000, 1.000000000000000000 ) ) ;
#3158 = CARTESIAN_POINT ( 'NONE',  ( -4.164238869374099039, 51.80374883491396787, 8.674139862899312516E-16 ) ) ;
#3159 = CARTESIAN_POINT ( 'NONE',  ( 19.05866839779138999, 5.955083851089585600, -6.499999999999964473 ) ) ;
#3160 = ORIENTED_EDGE ( 'NONE', *, *, #47359, .F. ) ;
#3161 = DIRECTION ( 'NONE',  ( 0.000000000000000000, -0.000000000000000000, 1.000000000000000000 ) ) ;
#3162 = CARTESIAN_POINT ( 'NONE',  ( 14.92337183194729633, 27.67559781766745530, 8.527530157486181039 ) ) ;
#3163 =( NAMED_UNIT ( * ) PLANE_ANGLE_UNIT ( ) SI_UNIT ( $, .RADIAN. ) );
#3164 = CARTESIAN_POINT ( 'NONE',  ( 6.565887622018943937, 3.081968003263753531, -12.81628187352647608 ) ) ;
#3165 = CARTESIAN_POINT ( 'NONE',  ( -0.8801773607111009756, 68.06368534415484817, 1.068504757029289695E-15 ) ) ;
#3166 = EDGE_CURVE ( 'NONE', #66548, #85989, #98203, .T. ) ;
#3167 = CARTESIAN_POINT ( 'NONE',  ( 0.1532563361054082862, 56.21726448433411605, 2.638427012816831674 ) ) ;
#3168 = CARTESIAN_POINT ( 'NONE',  ( -0.1491070598754174470, 61.94583914210339515, 5.000000000000000000 ) ) ;
#3169 = EDGE_CURVE ( 'NONE', #15638, #25872, #6220, .T. ) ;
#3170 = ORIENTED_EDGE ( 'NONE', *, *, #59868, .F. ) ;
#3171 = CARTESIAN_POINT ( 'NONE',  ( 10.00000000000000000, 1.813685344154838175, -10.88017736071110342 ) ) ;
#3172 = CARTESIAN_POINT ( 'NONE',  ( -0.7375392941515958034, 14.49999999999999112, -14.98185688723478215 ) ) ;
#3173 = CARTESIAN_POINT ( 'NONE',  ( 0.5774900079438590739, 42.64701867748816966, -5.440088680355550821 ) ) ;
#3175 = CARTESIAN_POINT ( 'NONE',  ( 6.236392532960747914, 13.06690530480599577, -10.05961789237413129 ) ) ;
#3174 = CARTESIAN_POINT ( 'NONE',  ( 16.40814093676323893, 15.79030133659708746, 11.09922568453595026 ) ) ;
#3176 = FACE_OUTER_BOUND ( 'NONE', #51806, .T. ) ;
#3177 = DIRECTION ( 'NONE',  ( 0.000000000000000000, 1.000000000000000000, 0.000000000000000000 ) ) ;
#3178 = CARTESIAN_POINT ( 'NONE',  ( -0.1503990784575247319, 67.22266099184919597, -6.262539305110083276 ) ) ;
#3179 = CARTESIAN_POINT ( 'NONE',  ( 2.791683348922237240, 45.38393115100079456, -7.208316651077763204 ) ) ;
#3180 = CARTESIAN_POINT ( 'NONE',  ( 0.1532563361054100626, 0.8005978176674514168, -2.638427012816831230 ) ) ;
#3181 = CARTESIAN_POINT ( 'NONE',  ( -10.88017736071110342, -31.93631465584515539, 3.903127820947815962E-15 ) ) ;
#3182 = CARTESIAN_POINT ( 'NONE',  ( 19.38216949554541202, 10.99863466993042138, 9.382169495545424454 ) ) ;
#3183 = CARTESIAN_POINT ( 'NONE',  ( -8.159336008804556784, -4.163137246816088322, -4.000000000000000000 ) ) ;
#3185 = CARTESIAN_POINT ( 'NONE',  ( -0.000000000000000000, 40.74999999999999289, -4.000000000000000000 ) ) ;
#3184 = CARTESIAN_POINT ( 'NONE',  ( 12.91533473730992121, 29.52201867748817321, 10.88017736071110164 ) ) ;
#3186 = CARTESIAN_POINT ( 'NONE',  ( 34.56412365047463453, 26.99999999999999645, 9.500000000000000000 ) ) ;
#3187 = CARTESIAN_POINT ( 'NONE',  ( -4.164238869374098151, 36.59541550158063217, -3.795296366450310543 ) ) ;
#3188 = CARTESIAN_POINT ( 'NONE',  ( 2.917880565312950480, 30.97041550158063572, -12.26659068614894821 ) ) ;
#3189 = CARTESIAN_POINT ( 'NONE',  ( 10.00000000000000000, 6.813685344154838397, -10.88017736071110342 ) ) ;
#3190 = CARTESIAN_POINT ( 'NONE',  ( 17.20831665107776587, 37.88393115100078745, 7.208316651077764980 ) ) ;
#3191 = CARTESIAN_POINT ( 'NONE',  ( -1.099225684535947600, 39.54030133659708923, 6.408140936763237150 ) ) ;
#3192 = CARTESIAN_POINT ( 'NONE',  ( 4.559911319644449179, 12.23035201082150536, -9.422509992056141925 ) ) ;
#3193 = ORIENTED_EDGE ( 'NONE', *, *, #78604, .T. ) ;
#3194 = CARTESIAN_POINT ( 'NONE',  ( 10.00000000000000178, 32.25893115100078745, 9.846743663894594434 ) ) ;
#3195 = EDGE_CURVE ( 'NONE', #95706, #77766, #60460, .T. ) ;
#3196 = CARTESIAN_POINT ( 'NONE',  ( 2.035157376598822676, 37.43868534415484106, -7.964842623401177768 ) ) ;
#3197 = CARTESIAN_POINT ( 'NONE',  ( 10.00000000000000000, 2.873634669930420049, -12.81628187352647608 ) ) ;
#3199 = CARTESIAN_POINT ( 'NONE',  ( -6.000000000000000000, 78.07179676972447169, 4.250000000000000000 ) ) ;
#3198 = CARTESIAN_POINT ( 'NONE',  ( 13.79529636645031943, 20.34541550158063572, -14.16423886937409904 ) ) ;
#3200 = CARTESIAN_POINT ( 'NONE',  ( -2.361410439757122059, 14.76930270348881180, -14.75336556272939781 ) ) ;
#3201 = UNCERTAINTY_MEASURE_WITH_UNIT (LENGTH_MEASURE( 1.000000000000000082E-05 ), #69237, 'distance_accuracy_value', 'NONE');
#3202 = CARTESIAN_POINT ( 'NONE',  ( 12.63842701281683922, 24.55059781766745175, -9.846743663894590881 ) ) ;
#3203 = CARTESIAN_POINT ( 'NONE',  ( 10.00000000000000178, 50.37363466993042493, 12.81628187352647608 ) ) ;
#3204 = CARTESIAN_POINT ( 'NONE',  ( 5.076628168052704559, 60.17559781766745175, -8.527530157486179263 ) ) ;
#3205 = ORIENTED_EDGE ( 'NONE', *, *, #62192, .F. ) ;
#3206 = CARTESIAN_POINT ( 'NONE',  ( 8.650319761818652253, -1.048872767148395280, -4.000000000000000000 ) ) ;
#3207 = CARTESIAN_POINT ( 'NONE',  ( 4.722628015970558479, -9.822377395415374579, 3.750000000000001776 ) ) ;
#3208 = AXIS2_PLACEMENT_3D ( 'NONE', #58771, #7135, #42302 ) ;
#3209 = CARTESIAN_POINT ( 'NONE',  ( 20.88017736071110875, 5.772018677488170546, -2.915334737309920765 ) ) ;
#3210 = CARTESIAN_POINT ( 'NONE',  ( 24.16423886937410614, 9.512082168247301794, -3.795296366450302550 ) ) ;
#3211 = CARTESIAN_POINT ( 'NONE',  ( 0.1532563361054082862, 1.217264484334117824, 2.638427012816831674 ) ) ;
#3212 = CARTESIAN_POINT ( 'NONE',  ( 19.84674366389459266, 48.71726448433413026, -2.638427012816827677 ) ) ;
#3213 = CARTESIAN_POINT ( 'NONE',  ( 10.00000000000000000, 26.81368534415484106, -10.88017736071110342 ) ) ;
#3214 = CARTESIAN_POINT ( 'NONE',  ( 3.969999999999999751, 10.25000000000000000, -2.750000000000000000 ) ) ;
#3215 = CARTESIAN_POINT ( 'NONE',  ( 19.84674366389459266, 58.30059781766745886, 2.638427012816836559 ) ) ;
#3216 = VERTEX_POINT ( 'NONE', #4685 ) ;
#3217 = SURFACE_STYLE_FILL_AREA ( #10226 ) ;
#3218 = ORIENTED_EDGE ( 'NONE', *, *, #60294, .F. ) ;
#3219 = ORIENTED_EDGE ( 'NONE', *, *, #36268, .F. ) ;
#3220 = CARTESIAN_POINT ( 'NONE',  ( -4.698669664746495833, 0.000000000000000000, 2.767727949825290690 ) ) ;
#3221 = CARTESIAN_POINT ( 'NONE',  ( 2.917880565312950480, 5.970415501580634832, -12.26659068614894821 ) ) ;
#3222 = CARTESIAN_POINT ( 'NONE',  ( 2.917880565312948704, 42.63708216824729647, 12.26659068614894643 ) ) ;
#3223 = CARTESIAN_POINT ( 'NONE',  ( 17.20831665107776587, 54.13393115100079456, -7.208316651077762316 ) ) ;
#3224 = CARTESIAN_POINT ( 'NONE',  ( 10.00000000000000000, 39.75893115100078745, -9.846743663894594434 ) ) ;
#3225 = DIRECTION ( 'NONE',  ( -0.000000000000000000, -1.000000000000000000, -0.000000000000000000 ) ) ;
#3227 = CARTESIAN_POINT ( 'NONE',  ( 0.1532563361054082862, 66.21726448433413736, 2.638427012816831674 ) ) ;
#3226 = CARTESIAN_POINT ( 'NONE',  ( 12.91533473730993009, 26.60535201082150536, -10.88017736071109987 ) ) ;
#3228 = CARTESIAN_POINT ( 'NONE',  ( 6.204703633549690345, 37.84541550158063927, 14.16423886937410082 ) ) ;
#3229 = CARTESIAN_POINT ( 'NONE',  ( 19.42250999205614548, 10.98035201082150536, -5.440088680355545492 ) ) ;
#3230 = CARTESIAN_POINT ( 'NONE',  ( 1.472469842513823179, 65.59226448433412315, -4.923371831947296329 ) ) ;
#3231 = CARTESIAN_POINT ( 'NONE',  ( -0.8801773607111008646, 58.27201867748816966, 2.915334737309923430 ) ) ;
#3232 = CARTESIAN_POINT ( 'NONE',  ( 12.63842701281683922, 24.55059781766745175, -9.846743663894590881 ) ) ;
#3233 = CARTESIAN_POINT ( 'NONE',  ( -5.580560104534956878, -28.67655754325946660, 4.000000000000000000 ) ) ;
#3234 = EDGE_CURVE ( 'NONE', #1418, #39614, #35148, .T. ) ;
#3235 = ORIENTED_EDGE ( 'NONE', *, *, #67059, .F. ) ;
#3236 = DIRECTION ( 'NONE',  ( -0.4461978131098006117, 0.000000000000000000, -0.8949343616020291048 ) ) ;
#3237 = ORIENTED_EDGE ( 'NONE', *, *, #29922, .F. ) ;
#3238 = CARTESIAN_POINT ( 'NONE',  ( 1.472469842513823179, 21.42559781766745175, 4.923371831947296329 ) ) ;
#3239 = ORIENTED_EDGE ( 'NONE', *, *, #59709, .T. ) ;
#3240 = CARTESIAN_POINT ( 'NONE',  ( 24.16423886937409904, 29.09541550158063572, 3.795296366450317205 ) ) ;
#3241 = CARTESIAN_POINT ( 'NONE',  ( 12.63842701281683922, 29.55059781766745175, -9.846743663894590881 ) ) ;
#3242 = CARTESIAN_POINT ( 'NONE',  ( 4.559911319644449179, 53.89701867748817676, 9.422509992056141925 ) ) ;
#3243 = EDGE_CURVE ( 'NONE', #13782, #81929, #70748, .T. ) ;
#3244 = CARTESIAN_POINT ( 'NONE',  ( 15.44008868035555793, 41.39701867748817676, -9.422509992056140149 ) ) ;
#3245 = CARTESIAN_POINT ( 'NONE',  ( 1.472469842513823179, 50.59226448433411605, -4.923371831947296329 ) ) ;
#3246 = CARTESIAN_POINT ( 'NONE',  ( -12.81628187352647963, -6.084698663402908991, -3.434112377981046293 ) ) ;
#3247 = ORIENTED_EDGE ( 'NONE', *, *, #16788, .T. ) ;
#3248 = CARTESIAN_POINT ( 'NONE',  ( 7.084665262690076126, 42.02201867748816966, -10.88017736071110164 ) ) ;
#3249 = CARTESIAN_POINT ( 'NONE',  ( -4.164238869374099927, 7.012082168247302683, 3.795296366450308767 ) ) ;
#3250 = ORIENTED_EDGE ( 'NONE', *, *, #3662, .T. ) ;
#3251 = CARTESIAN_POINT ( 'NONE',  ( 22.81628187352647785, 31.62363466993042138, 6.195893100308588602E-16 ) ) ;
#3252 = CARTESIAN_POINT ( 'NONE',  ( 1.472469842513823179, 26.42559781766745175, 4.923371831947296329 ) ) ;
#3253 = CARTESIAN_POINT ( 'NONE',  ( 14.52844422123121682, -3.613442552986844458E-15, -1.683098224408302368 ) ) ;
#3254 = CARTESIAN_POINT ( 'NONE',  ( 3.591859063236763294, 43.29030133659708923, -11.09922568453595026 ) ) ;
#3255 = LINE ( 'NONE', #66703, #12827 ) ;
#3256 = CARTESIAN_POINT ( 'NONE',  ( 19.84674366389459266, 28.71726448433411960, -2.638427012816827677 ) ) ;
#3258 = VECTOR ( 'NONE', #11309, 999.9999999999998863 ) ;
#3257 = CARTESIAN_POINT ( 'NONE',  ( 7.084665262690076126, 64.10535201082150536, 10.88017736071109987 ) ) ;
#3259 = B_SPLINE_CURVE_WITH_KNOTS ( 'NONE', 3,
 ( #18118, #59547, #98575, #43068 ),
 .UNSPECIFIED., .F., .F.,
 ( 4, 4 ),
 ( 0.0004294207726287377542, 0.0005403323854458763099 ),
 .UNSPECIFIED. ) ;
#3260 = DIRECTION ( 'NONE',  ( -1.000000000000000000, 0.000000000000000000, 0.000000000000000000 ) ) ;
#3261 = CARTESIAN_POINT ( 'NONE',  ( 34.56412365047464874, 11.99999999999999645, -9.500000000000000000 ) ) ;
#3262 = CARTESIAN_POINT ( 'NONE',  ( 13.95692576442126942, 0.2301500530278525469, 5.331646315825828708 ) ) ;
#3263 = CARTESIAN_POINT ( 'NONE',  ( 5.076628168052703671, 6.842264484334118713, 8.527530157486179263 ) ) ;
#3264 = CARTESIAN_POINT ( 'NONE',  ( -2.816281873526473856, 14.33196800326375531, 3.434112377981055619 ) ) ;
#3265 = VECTOR ( 'NONE', #52377, 1000.000000000000000 ) ;
#3266 = DIRECTION ( 'NONE',  ( 0.000000000000000000, 0.000000000000000000, -1.000000000000000000 ) ) ;
#3267 = VECTOR ( 'NONE', #90993, 1000.000000000000000 ) ;
#3268 = CARTESIAN_POINT ( 'NONE',  ( 7.361572987183169658, 49.96726448433410894, -9.846743663894592657 ) ) ;
#3269 = CARTESIAN_POINT ( 'NONE',  ( -0.2838433074297238012, 13.12729635533385597, 10.00000000000000000 ) ) ;
#3270 = CARTESIAN_POINT ( 'NONE',  ( 24.16423886937409904, 9.095415501580633943, 3.795296366450317205 ) ) ;
#3271 = CARTESIAN_POINT ( 'NONE',  ( 5.076628168052704559, 35.17559781766745175, -8.527530157486179263 ) ) ;
#3272 = CARTESIAN_POINT ( 'NONE',  ( 10.00000000000000000, 32.87363466993042493, -12.81628187352647608 ) ) ;
#3274 = DIRECTION ( 'NONE',  ( 0.000000000000000000, 0.000000000000000000, 1.000000000000000000 ) ) ;
#3273 = CARTESIAN_POINT ( 'NONE',  ( 9.075906804202286793, -0.03417435944610275333, -13.17214151599837990 ) ) ;
#3275 = CARTESIAN_POINT ( 'NONE',  ( 7.084665262690076126, 54.10535201082151247, 10.88017736071109987 ) ) ;
#3276 = CARTESIAN_POINT ( 'NONE',  ( 21.09922568453595559, 7.040301336597086568, -6.408140936763230044 ) ) ;
#3277 = CARTESIAN_POINT ( 'NONE',  ( 9.820682251645170169, 0.2306972965111888652, -11.26020669458359436 ) ) ;
#3278 = CARTESIAN_POINT ( 'NONE',  ( 0.1532563361054082862, 21.21726448433412315, 2.638427012816831674 ) ) ;
#3279 = CARTESIAN_POINT ( 'NONE',  ( -0.8801773607110991993, 22.85535201082150181, -2.915334737309923874 ) ) ;
#3280 = EDGE_CURVE ( 'NONE', #54272, #19669, #65298, .T. ) ;
#3281 = CARTESIAN_POINT ( 'NONE',  ( 21.09922568453594849, 36.20696800326375353, 6.408140936763242479 ) ) ;
#3282 = CARTESIAN_POINT ( 'NONE',  ( 19.84674366389459266, 23.30059781766745530, 2.638427012816836559 ) ) ;
#3283 =( NAMED_UNIT ( * ) SI_UNIT ( $, .STERADIAN. ) SOLID_ANGLE_UNIT ( ) );
#3284 = CARTESIAN_POINT ( 'NONE',  ( -0.8649609010931206265, -2.456395547037469011E-16, -14.60103384664012971 ) ) ;
#3285 = CARTESIAN_POINT ( 'NONE',  ( 20.88017736071110164, 35.35535201082150536, 2.915334737309930979 ) ) ;
#3286 = CARTESIAN_POINT ( 'NONE',  ( 2.035157376598822676, 62.43868534415483396, -7.964842623401177768 ) ) ;
#3287 = CARTESIAN_POINT ( 'NONE',  ( -0.8801773607110991993, 2.855352010821504471, -2.915334737309923874 ) ) ;
#3289 = CARTESIAN_POINT ( 'NONE',  ( 17.96484262340118221, 24.93868534415484461, 7.964842623401181321 ) ) ;
#3288 = CARTESIAN_POINT ( 'NONE',  ( 10.00000000000000178, 47.25893115100078745, 9.846743663894594434 ) ) ;
#3290 = PRESENTATION_STYLE_ASSIGNMENT (( #70815 ) ) ;
#3291 = CARTESIAN_POINT ( 'NONE',  ( 2.035157376598824452, 43.68868534415484106, 7.964842623401179544 ) ) ;
#3292 = CARTESIAN_POINT ( 'NONE',  ( 2.035157376598824452, 8.688685344154839285, 7.964842623401179544 ) ) ;
#3293 = VECTOR ( 'NONE', #33651, 1000.000000000000000 ) ;
#3294 = DIRECTION ( 'NONE',  ( 0.000000000000000000, 1.000000000000000000, 0.000000000000000000 ) ) ;
#3295 = CARTESIAN_POINT ( 'NONE',  ( 12.63842701281683034, 42.46726448433412315, 9.846743663894596210 ) ) ;
#3296 = CARTESIAN_POINT ( 'NONE',  ( 2.917880565312950480, 50.97041550158064638, -12.26659068614894821 ) ) ;
#3297 = DIRECTION ( 'NONE',  ( 0.000000000000000000, -1.000000000000000000, 0.000000000000000000 ) ) ;
#3298 = CARTESIAN_POINT ( 'NONE',  ( 24.16423886937410614, 19.51208216824729647, -3.795296366450302550 ) ) ;
#3300 = CARTESIAN_POINT ( 'NONE',  ( -0.5000000000000073275, 80.99999999999994316, 0.000000000000000000 ) ) ;
#3299 = CIRCLE ( 'NONE', #38429, 14.49999999999999822 ) ;
#3301 = ORIENTED_EDGE ( 'NONE', *, *, #37855, .F. ) ;
#3302 = EDGE_CURVE ( 'NONE', #86850, #53420, #50661, .T. ) ;
#3303 = CARTESIAN_POINT ( 'NONE',  ( 24.16423886937410614, 64.51208216824728936, -3.795296366450302550 ) ) ;
#3304 = CARTESIAN_POINT ( 'NONE',  ( 17.20831665107776587, 34.13393115100078745, -7.208316651077762316 ) ) ;
#3305 = DIRECTION ( 'NONE',  ( -0.000000000000000000, -1.000000000000000000, -0.000000000000000000 ) ) ;
#3306 = CARTESIAN_POINT ( 'NONE',  ( 0.5774900079438590739, 57.64701867748817676, -5.440088680355550821 ) ) ;
#3307 = CARTESIAN_POINT ( 'NONE',  ( -2.816281873526473856, 59.33196800326374643, 3.434112377981055619 ) ) ;
#3308 = CARTESIAN_POINT ( 'NONE',  ( 15.44008868035555260, 24.73035201082150891, 9.422509992056143702 ) ) ;
#3309 = CARTESIAN_POINT ( 'NONE',  ( 10.00000000000000178, 65.37363466993042493, 12.81628187352647608 ) ) ;
#3310 = CARTESIAN_POINT ( 'NONE',  ( 13.43411237798105340, 15.58196800326374998, 12.81628187352647963 ) ) ;
#3311 = CARTESIAN_POINT ( 'NONE',  ( 18.52753015748617571, 13.09226448433411960, 4.923371831947298993 ) ) ;
#3313 = ORIENTED_EDGE ( 'NONE', *, *, #81525, .T. ) ;
#3312 = EDGE_CURVE ( 'NONE', #2779, #94935, #84456, .T. ) ;
#3314 = DIRECTION ( 'NONE',  ( 0.000000000000000000, 0.000000000000000000, 1.000000000000000000 ) ) ;
#3315 = CARTESIAN_POINT ( 'NONE',  ( 22.26659068614895176, 64.72041550158064638, -7.082119434687042414 ) ) ;
#3316 = CARTESIAN_POINT ( 'NONE',  ( -4.164238869374098151, 21.59541550158063217, -3.795296366450310543 ) ) ;
#3317 = CARTESIAN_POINT ( 'NONE',  ( 20.88017736071110164, 30.35535201082151247, 2.915334737309930979 ) ) ;
#3318 = CARTESIAN_POINT ( 'NONE',  ( 17.96484262340118221, 44.93868534415483396, 7.964842623401181321 ) ) ;
#3319 = CARTESIAN_POINT ( 'NONE',  ( 0.1034006766821536916, 0.000000000000000000, -14.49963131600461352 ) ) ;
#3320 = CARTESIAN_POINT ( 'NONE',  ( 11.10647200087811548, -65.08385396171316017, -3.999999999999999112 ) ) ;
#3321 = CARTESIAN_POINT ( 'NONE',  ( 19.84674366389459621, 13.50893115100078568, 7.409399052514197653E-17 ) ) ;
#3322 = FILL_AREA_STYLE ('',( #11307 ) ) ;
#3323 = CARTESIAN_POINT ( 'NONE',  ( 5.076628168052703671, 21.84226448433411960, 8.527530157486179263 ) ) ;
#3324 = CARTESIAN_POINT ( 'NONE',  ( -14.82679024690672875, 14.76930270348881002, 1.845086899513189049 ) ) ;
#3325 = CARTESIAN_POINT ( 'NONE',  ( 14.35000000000000142, 98.49999999999998579, 8.000000000000000000 ) ) ;
#3326 = CARTESIAN_POINT ( 'NONE',  ( 10.00000000000000000, 19.75893115100078390, -9.846743663894594434 ) ) ;
#3327 = CARTESIAN_POINT ( 'NONE',  ( 19.84674366389459621, 53.50893115100078745, 7.409399052514197653E-17 ) ) ;
#3328 = AXIS2_PLACEMENT_3D ( 'NONE', #4753, #95750, #57240 ) ;
#3329 = CARTESIAN_POINT ( 'NONE',  ( 19.42250999205614548, 25.98035201082150891, -5.440088680355545492 ) ) ;
#3330 = B_SPLINE_CURVE_WITH_KNOTS ( 'NONE', 3,
 ( #81763, #82258, #72294, #50278, #5302, #43767 ),
 .UNSPECIFIED., .F., .F.,
 ( 4, 2, 4 ),
 ( 0.000000000000000000, 0.0002626113303185885592, 0.0005252226606371771184 ),
 .UNSPECIFIED. ) ;
#3331 = UNCERTAINTY_MEASURE_WITH_UNIT (LENGTH_MEASURE( 1.000000000000000082E-05 ), #72088, 'distance_accuracy_value', 'NONE');
#3332 = CARTESIAN_POINT ( 'NONE',  ( 10.00000000000000000, 47.87363466993042493, -12.81628187352647608 ) ) ;
#3333 = CARTESIAN_POINT ( 'NONE',  ( -0.8801773607111008646, 48.27201867748816966, 2.915334737309923430 ) ) ;
#3334 = CARTESIAN_POINT ( 'NONE',  ( 19.84674366389459266, 28.71726448433411960, -2.638427012816827677 ) ) ;
#3336 = CARTESIAN_POINT ( 'NONE',  ( 17.20831665107776587, 24.13393115100078035, -7.208316651077762316 ) ) ;
#3335 = CARTESIAN_POINT ( 'NONE',  ( -4.164238869374098151, 41.59541550158061796, -3.795296366450310543 ) ) ;
#3337 = CARTESIAN_POINT ( 'NONE',  ( 14.24131928502211331, 15.00000000000000000, 0.4973178280106892446 ) ) ;
#3338 = CARTESIAN_POINT ( 'NONE',  ( 12.63842701281683922, 64.55059781766745175, -9.846743663894590881 ) ) ;
#3339 = CARTESIAN_POINT ( 'NONE',  ( 22.26659068614895176, 9.720415501580633943, -7.082119434687042414 ) ) ;
#3340 = CARTESIAN_POINT ( 'NONE',  ( 13.79529636645031943, 25.34541550158063572, -14.16423886937409904 ) ) ;
#3341 = CARTESIAN_POINT ( 'NONE',  ( 10.00000000000000178, 32.25893115100078745, 9.846743663894594434 ) ) ;
#3342 = LINE ( 'NONE', #95316, #42729 ) ;
#3343 = CARTESIAN_POINT ( 'NONE',  ( 20.88017736071110875, 20.77201867748816611, -2.915334737309920765 ) ) ;
#3344 = CARTESIAN_POINT ( 'NONE',  ( 2.035157376598824452, 48.68868534415483396, 7.964842623401179544 ) ) ;
#3345 = CARTESIAN_POINT ( 'NONE',  ( 7.084665262690076126, 44.10535201082151247, 10.88017736071109987 ) ) ;
#3346 = EDGE_LOOP ( 'NONE', ( #87923, #29571, #54331, #19511, #55798, #63038 ) ) ;
#3347 = CARTESIAN_POINT ( 'NONE',  ( 6.565887622018943937, 45.16530133659708923, 12.81628187352647430 ) ) ;
#3348 = CARTESIAN_POINT ( 'NONE',  ( 20.88017736071110519, 50.56368534415484106, 2.639326808657452039E-16 ) ) ;
#3349 = ORIENTED_EDGE ( 'NONE', *, *, #80392, .T. ) ;
#3350 = CARTESIAN_POINT ( 'NONE',  ( 2.518025504887051458, 0.000000000000000000, 4.837081990145644106 ) ) ;
#3351 = EDGE_CURVE ( 'NONE', #107, #61640, #69627, .T. ) ;
#3352 = CARTESIAN_POINT ( 'NONE',  ( 20.88017736071110164, 65.35535201082150536, 2.915334737309930979 ) ) ;
#3353 = ORIENTED_EDGE ( 'NONE', *, *, #39054, .T. ) ;
#3354 = CARTESIAN_POINT ( 'NONE',  ( 2.035157376598824452, 63.68868534415484106, 7.964842623401179544 ) ) ;
#3355 = CARTESIAN_POINT ( 'NONE',  ( 0.5774900079438607392, 3.480352010821504027, 5.440088680355550821 ) ) ;
#3356 = CARTESIAN_POINT ( 'NONE',  ( 19.10478245763052740, 40.10160829253885595, 5.990408912944308994 ) ) ;
#3357 = CARTESIAN_POINT ( 'NONE',  ( 14.82269085861175384, 14.49999999999999112, -2.299529454046946864 ) ) ;
#3358 = CARTESIAN_POINT ( 'NONE',  ( 19.42250999205614548, 5.980352010821504471, -5.440088680355545492 ) ) ;
#3359 = CARTESIAN_POINT ( 'NONE',  ( 12.63842701281683034, 7.467264484334118713, 9.846743663894596210 ) ) ;
#3360 = CARTESIAN_POINT ( 'NONE',  ( 13.79529636645031943, 10.34541550158063394, -14.16423886937409904 ) ) ;
#3361 = CARTESIAN_POINT ( 'NONE',  ( 1.472469842513823179, 10.59226448433411782, -4.923371831947296329 ) ) ;
#3362 = CARTESIAN_POINT ( 'NONE',  ( 7.084665262690076126, 12.02201867748817143, -10.88017736071110164 ) ) ;
#3363 = CARTESIAN_POINT ( 'NONE',  ( 1.472469842513823179, 50.59226448433411605, -4.923371831947296329 ) ) ;
#3364 = B_SPLINE_CURVE_WITH_KNOTS ( 'NONE', 3,
 ( #26424, #35900, #18945, #49421, #79924, #11432, #41952, #87914, #15801, #44427 ),
 .UNSPECIFIED., .F., .F.,
 ( 4, 3, 3, 4 ),
 ( 0.000000000000000000, 0.0006253016069560996199, 0.001250604074564917820, 0.002501455912506563017 ),
 .UNSPECIFIED. ) ;
#3365 = ORIENTED_EDGE ( 'NONE', *, *, #44520, .F. ) ;
#3366 = B_SPLINE_CURVE_WITH_KNOTS ( 'NONE', 3,
 ( #72381, #41919, #47423, #9430, #1955, #39934 ),
 .UNSPECIFIED., .F., .F.,
 ( 4, 2, 4 ),
 ( 3.409110551494645334E-05, 0.0004400426677367947573, 0.0008459942299586430342 ),
 .UNSPECIFIED. ) ;
#3367 = CARTESIAN_POINT ( 'NONE',  ( 1.472469842513823179, 46.42559781766745175, 4.923371831947296329 ) ) ;
#3368 = EDGE_LOOP ( 'NONE', ( #67416, #80626, #82600, #56636 ) ) ;
#3369 = CARTESIAN_POINT ( 'NONE',  ( 18.29284471827483571, 30.40189080397291832, -6.500000000000035527 ) ) ;
#3370 = CARTESIAN_POINT ( 'NONE',  ( 0.5774900079438607392, 53.48035201082151247, 5.440088680355550821 ) ) ;
#3371 = CARTESIAN_POINT ( 'NONE',  ( 1.472469842513823179, 50.59226448433411605, -4.923371831947296329 ) ) ;
#3372 = CARTESIAN_POINT ( 'NONE',  ( 22.81628187352647785, 31.62363466993042138, 6.195893100308588602E-16 ) ) ;
#3373 = FILL_AREA_STYLE_COLOUR ( '', #62700 ) ;
#3374 = CARTESIAN_POINT ( 'NONE',  ( 2.035157376598824452, 58.68868534415482685, 7.964842623401179544 ) ) ;
#3375 = CARTESIAN_POINT ( 'NONE',  ( 4.559911319644449179, 2.230352010821504916, -9.422509992056141925 ) ) ;
#3376 = CIRCLE ( 'NONE', #83233, 1.000000000000000888 ) ;
#3377 = CARTESIAN_POINT ( 'NONE',  ( 22.81628187352647785, 41.62363466993042493, 6.195893100308588602E-16 ) ) ;
#3378 = DIRECTION ( 'NONE',  ( 0.000000000000000000, 1.000000000000000000, 0.000000000000000000 ) ) ;
#3379 = VERTEX_POINT ( 'NONE', #90619 ) ;
#3380 = CARTESIAN_POINT ( 'NONE',  ( 16.40814093676324603, 22.45696800326375353, -11.09922568453594671 ) ) ;
#3381 = CARTESIAN_POINT ( 'NONE',  ( 7.084665262690076126, 39.10535201082150536, 10.88017736071109987 ) ) ;
#3382 = EDGE_LOOP ( 'NONE', ( #10392, #45282, #71683, #68252 ) ) ;
#3383 = CARTESIAN_POINT ( 'NONE',  ( 12.63842701281683034, 7.467264484334118713, 9.846743663894596210 ) ) ;
#3384 = CARTESIAN_POINT ( 'NONE',  ( -2.816281873526473856, -0.6680319967362464695, 3.434112377981055619 ) ) ;
#3386 = CARTESIAN_POINT ( 'NONE',  ( 14.92337183194729633, 52.67559781766745175, 8.527530157486181039 ) ) ;
#3385 = CARTESIAN_POINT ( 'NONE',  ( 17.20831665107776587, 17.88393115100078745, 7.208316651077764980 ) ) ;
#3387 = CARTESIAN_POINT ( 'NONE',  ( -11.19909113571437764, -94.48345865769024954, 3.750000000000001776 ) ) ;
#3388 = SURFACE_SIDE_STYLE ('',( #25896 ) ) ;
#3389 = CIRCLE ( 'NONE', #11373, 14.49999999999999822 ) ;
#3390 = CARTESIAN_POINT ( 'NONE',  ( 2.791683348922240793, 41.63393115100078745, 7.208316651077764092 ) ) ;
#3391 = DIRECTION ( 'NONE',  ( -1.000000000000000000, 0.000000000000000000, 0.000000000000000000 ) ) ;
#3392 = CARTESIAN_POINT ( 'NONE',  ( -29.94000000000000838, 92.00000000000000000, -10.09898361729590199 ) ) ;
#3394 = CARTESIAN_POINT ( 'NONE',  ( 7.361572987183169658, -0.03273551566588185635, -9.846743663894592657 ) ) ;
#3393 = CARTESIAN_POINT ( 'NONE',  ( 12.63842701281683922, 24.55059781766745175, -9.846743663894590881 ) ) ;
#3395 =( LENGTH_UNIT ( ) NAMED_UNIT ( * ) SI_UNIT ( .MILLI., .METRE. ) );
#3396 = EDGE_CURVE ( 'NONE', #83574, #67150, #22221, .T. ) ;
#3398 = ORIENTED_EDGE ( 'NONE', *, *, #43235, .F. ) ;
#3397 = CARTESIAN_POINT ( 'NONE',  ( 19.84674366389459266, 63.71726448433412315, -2.638427012816827677 ) ) ;
#3399 = VECTOR ( 'NONE', #5653, 1000.000000000000114 ) ;
#3400 = CARTESIAN_POINT ( 'NONE',  ( 3.591859063236763294, 63.29030133659708923, -11.09922568453595026 ) ) ;
#3401 = DIRECTION ( 'NONE',  ( 0.000000000000000000, 0.000000000000000000, 1.000000000000000000 ) ) ;
#3402 = CARTESIAN_POINT ( 'NONE',  ( 22.81628187352648496, 21.83196800326374643, -3.434112377981050290 ) ) ;
#3403 = CARTESIAN_POINT ( 'NONE',  ( 5.076628168052703671, 41.84226448433411605, 8.527530157486179263 ) ) ;
#3404 = ADVANCED_FACE ( 'NONE', ( #74637 ), #83632, .F. ) ;
#3405 = CARTESIAN_POINT ( 'NONE',  ( -1.915564264621232748, 15.00000000000000000, -14.37291249357993372 ) ) ;
#3407 = ADVANCED_FACE ( 'NONE', ( #61113 ), #83128, .F. ) ;
#3406 = CARTESIAN_POINT ( 'NONE',  ( -4.164238869374098151, 61.59541550158063217, -3.795296366450310543 ) ) ;
#3408 = CARTESIAN_POINT ( 'NONE',  ( 18.52753015748618282, 13.92559781766745175, -4.923371831947291888 ) ) ;
#3409 = ORIENTED_EDGE ( 'NONE', *, *, #87810, .F. ) ;
#3410 = VECTOR ( 'NONE', #96554, 1000.000000000000000 ) ;
#3411 = CARTESIAN_POINT ( 'NONE',  ( 11.34661744925197624, 54.08985607419765529, -3.000000000000000000 ) ) ;
#3412 = CARTESIAN_POINT ( 'NONE',  ( 13.79529636645030344, 63.26208216824730357, 14.16423886937410614 ) ) ;
#3413 = CARTESIAN_POINT ( 'NONE',  ( 18.52753015748617571, 58.09226448433411605, 4.923371831947298993 ) ) ;
#3414 = CARTESIAN_POINT ( 'NONE',  ( 17.96484262340118221, 9.938685344154839285, 7.964842623401181321 ) ) ;
#3415 = CARTESIAN_POINT ( 'NONE',  ( -0.3689425029237881626, 37.42874883491396787, 10.36894250292379027 ) ) ;
#3416 = CARTESIAN_POINT ( 'NONE',  ( 13.79529636645031943, 45.34541550158062506, -14.16423886937409904 ) ) ;
#3417 = DIRECTION ( 'NONE',  ( -0.000000000000000000, -0.000000000000000000, -1.000000000000000000 ) ) ;
#3418 = VECTOR ( 'NONE', #96069, 1000.000000000000114 ) ;
#3420 = CARTESIAN_POINT ( 'NONE',  ( 19.84674366389459266, 53.30059781766744464, 2.638427012816836559 ) ) ;
#3419 = DIRECTION ( 'NONE',  ( -1.000000000000000000, 0.000000000000000000, 0.000000000000000000 ) ) ;
#3421 = B_SPLINE_CURVE_WITH_KNOTS ( 'NONE', 3,
 ( #98692, #60649, #91148, #22674, #13678, #53153 ),
 .UNSPECIFIED., .F., .F.,
 ( 4, 2, 4 ),
 ( 0.000000000000000000, 0.0002565770811490986373, 0.0005131541622981972747 ),
 .UNSPECIFIED. ) ;
#3422 = VERTEX_POINT ( 'NONE', #30113 ) ;
#3423 = CARTESIAN_POINT ( 'NONE',  ( 17.96484262340118221, 31.18868534415483751, -7.964842623401177768 ) ) ;
#3424 = CARTESIAN_POINT ( 'NONE',  ( 8.992322367875814848, -4.150253140106991090, 3.750000000000001332 ) ) ;
#3425 = CARTESIAN_POINT ( 'NONE',  ( 19.84674366389459621, 48.50893115100078745, 7.409399052514197653E-17 ) ) ;
#3426 = DIRECTION ( 'NONE',  ( -0.000000000000000000, -1.000000000000000000, -0.000000000000000000 ) ) ;
#3427 = CARTESIAN_POINT ( 'NONE',  ( -7.082119434687058401, 0.9704155015806334994, -12.26659068614894110 ) ) ;
#3428 = CARTESIAN_POINT ( 'NONE',  ( 0.1532563361054083140, 56.00893115100078745, 1.131784320476157264E-15 ) ) ;
#3429 = CARTESIAN_POINT ( 'NONE',  ( 0.1532563361054082862, 66.21726448433413736, 2.638427012816831674 ) ) ;
#3431 = ADVANCED_FACE ( 'NONE', ( #15642 ), #28642, .F. ) ;
#3430 = ORIENTED_EDGE ( 'NONE', *, *, #28357, .T. ) ;
#3432 = CARTESIAN_POINT ( 'NONE',  ( 22.26659068614894466, 28.88708216824730357, 7.082119434687054849 ) ) ;
#3433 =( NAMED_UNIT ( * ) PLANE_ANGLE_UNIT ( ) SI_UNIT ( $, .RADIAN. ) );
#3435 = CARTESIAN_POINT ( 'NONE',  ( 18.72515096720571037, 45.05509018479935435, 6.499999999999982236 ) ) ;
#3434 = CARTESIAN_POINT ( 'NONE',  ( -3.585386599411524156, -2.690194976751732359, -2.500000000000604405 ) ) ;
#3436 = CARTESIAN_POINT ( 'NONE',  ( -0.8801773607111009756, 23.06368534415484106, 1.068504757029289695E-15 ) ) ;
#3437 = CARTESIAN_POINT ( 'NONE',  ( -1.099225684535947600, 29.54030133659708923, 6.408140936763237150 ) ) ;
#3438 = DIRECTION ( 'NONE',  ( 0.000000000000000000, -1.000000000000000000, 0.000000000000000000 ) ) ;
#3439 = CARTESIAN_POINT ( 'NONE',  ( 1.472469842513823179, 5.592264484334118713, -4.923371831947296329 ) ) ;
#3440 = EDGE_CURVE ( 'NONE', #94114, #26872, #52627, .T. ) ;
#3441 = CARTESIAN_POINT ( 'NONE',  ( 4.906778809679744668, -8.256987753881587011, -4.000000000000000000 ) ) ;
#3442 = CARTESIAN_POINT ( 'NONE',  ( 22.26659068614894466, 28.88708216824730357, 7.082119434687054849 ) ) ;
#3443 = PLANE ( 'NONE',  #6944 ) ;
#3444 = CARTESIAN_POINT ( 'NONE',  ( -4.139423687100486582, -8.271184049145468009, 3.999999999999999112 ) ) ;
#3445 = CARTESIAN_POINT ( 'NONE',  ( 10.00000000000000000, 6.813685344154838397, -10.88017736071110342 ) ) ;
#3446 = CYLINDRICAL_SURFACE ( 'NONE', #79772, 0.5000000000000004441 ) ;
#3447 = DIRECTION ( 'NONE',  ( 0.000000000000000000, 0.000000000000000000, -1.000000000000000000 ) ) ;
#3448 = CARTESIAN_POINT ( 'NONE',  ( 2.035157376598824452, 33.68868534415484106, 7.964842623401179544 ) ) ;
#3449 = CARTESIAN_POINT ( 'NONE',  ( 4.559911319644449179, 42.23035201082151247, -9.422509992056141925 ) ) ;
#3450 = CARTESIAN_POINT ( 'NONE',  ( -2.816281873526473856, -0.6680319967362464695, 3.434112377981055619 ) ) ;
#3451 = CARTESIAN_POINT ( 'NONE',  ( 18.52753015748617571, 63.09226448433412315, 4.923371831947298993 ) ) ;
#3452 = LINE ( 'NONE', #71931, #75477 ) ;
#3453 = CARTESIAN_POINT ( 'NONE',  ( 19.84674366389459621, 3.508931151000785231, 7.409399052514197653E-17 ) ) ;
#3454 = VERTEX_POINT ( 'NONE', #45119 ) ;
#3455 = B_SPLINE_CURVE_WITH_KNOTS ( 'NONE', 3,
 ( #53189, #83196, #82201, #37705, #68690, #98728, #30670, #30178 ),
 .UNSPECIFIED., .F., .F.,
 ( 4, 2, 2, 4 ),
 ( 0.000000000000000000, 0.004806130321901048823, 0.007209195482851595352, 0.009612260643802141014 ),
 .UNSPECIFIED. ) ;
#3456 = AXIS2_PLACEMENT_3D ( 'NONE', #58748, #73747, #74740 ) ;
#3457 = CARTESIAN_POINT ( 'NONE',  ( 0.5774900079438590739, 47.64701867748817676, -5.440088680355550821 ) ) ;
#3458 = UNCERTAINTY_MEASURE_WITH_UNIT (LENGTH_MEASURE( 1.000000000000000082E-05 ), #32392, 'distance_accuracy_value', 'NONE');
#3459 = COLOUR_RGB ( '', 0.40784314, 0.44705882, 0.49803922) ;
#3460 = CARTESIAN_POINT ( 'NONE',  ( 21.09922568453594849, 11.20696800326375531, 6.408140936763242479 ) ) ;
#3461 = CARTESIAN_POINT ( 'NONE',  ( 12.91533473730992121, 59.52201867748816966, 10.88017736071110164 ) ) ;
#3462 = CARTESIAN_POINT ( 'NONE',  ( 0.1532563361054082862, 26.21726448433411605, 2.638427012816831674 ) ) ;
#3463 = CARTESIAN_POINT ( 'NONE',  ( 22.81628187352648496, 31.83196800326375353, -3.434112377981050290 ) ) ;
#3465 = DIRECTION ( 'NONE',  ( -0.9961946980917462113, 0.08715574274765114371, 0.000000000000000000 ) ) ;
#3464 = CARTESIAN_POINT ( 'NONE',  ( 14.92337183194729633, 7.675597817667451750, 8.527530157486181039 ) ) ;
#3466 = ORIENTED_EDGE ( 'NONE', *, *, #7847, .T. ) ;
#3467 = CARTESIAN_POINT ( 'NONE',  ( 0.8952175423695025724, 48.52576239577081907, 5.990408912944351627 ) ) ;
#3468 = FACE_OUTER_BOUND ( 'NONE', #66664, .T. ) ;
#3469 = CARTESIAN_POINT ( 'NONE',  ( 0.5774900079438607392, 8.480352010821505360, 5.440088680355550821 ) ) ;
#3470 = CARTESIAN_POINT ( 'NONE',  ( -1.099225684535947600, 63.70696800326376774, -6.408140936763238038 ) ) ;
#3471 = CARTESIAN_POINT ( 'NONE',  ( 18.52753015748617571, 13.09226448433411960, 4.923371831947298993 ) ) ;
#3472 = PRESENTATION_STYLE_ASSIGNMENT (( #40980 ) ) ;
#3473 = CARTESIAN_POINT ( 'NONE',  ( -0.8801773607110991993, 7.855352010821506248, -2.915334737309923874 ) ) ;
#3474 = EDGE_LOOP ( 'NONE', ( #29821, #1595, #46121, #23054 ) ) ;
#3475 = CARTESIAN_POINT ( 'NONE',  ( 7.084665262690076126, 17.02201867748817676, -10.88017736071110164 ) ) ;
#3476 = EDGE_CURVE ( 'NONE', #587, #18033, #97663, .T. ) ;
#3477 = CARTESIAN_POINT ( 'NONE',  ( -0.8801773607111008646, 18.27201867748817321, 2.915334737309923430 ) ) ;
#3478 = CARTESIAN_POINT ( 'NONE',  ( 2.603489959281581889, 30.43575266056827999, -6.499999999999995559 ) ) ;
#3479 = CIRCLE ( 'NONE', #88097, 0.2500000000000002220 ) ;
#3480 = EDGE_LOOP ( 'NONE', ( #88404, #88335, #52226, #16128, #25037 ) ) ;
#3481 = CARTESIAN_POINT ( 'NONE',  ( 10.00000000000000178, 62.25893115100078745, 9.846743663894594434 ) ) ;
#3482 = CARTESIAN_POINT ( 'NONE',  ( 20.88017736071110519, 20.56368534415484106, 2.639326808657452039E-16 ) ) ;
#3484 = STYLED_ITEM ( 'NONE', ( #72806 ), #32638 ) ;
#3483 = CARTESIAN_POINT ( 'NONE',  ( 0.1532563361054100626, 50.80059781766745175, -2.638427012816831230 ) ) ;
#3485 = CARTESIAN_POINT ( 'NONE',  ( -8.564643372776705732, 14.63595249122789177, 12.31449893000736040 ) ) ;
#3486 = CARTESIAN_POINT ( 'NONE',  ( -1.926860441876562025, 4.479976035794175360, -3.195792623639529761 ) ) ;
#3487 = CARTESIAN_POINT ( 'NONE',  ( 24.16423886937410614, 29.30374883491396787, 8.672049930838204340E-16 ) ) ;
#3488 = CARTESIAN_POINT ( 'NONE',  ( 2.035157376598824452, 38.68868534415483396, 7.964842623401179544 ) ) ;
#3489 = CARTESIAN_POINT ( 'NONE',  ( 10.00000000000000000, 11.81368534415483751, -10.88017736071110342 ) ) ;
#3490 = CARTESIAN_POINT ( 'NONE',  ( 2.791683348922237240, 60.38393115100078745, -7.208316651077763204 ) ) ;
#3491 = CARTESIAN_POINT ( 'NONE',  ( -10.79821277343923569, -44.62913131165727521, -3.749999999999999556 ) ) ;
#3492 = CARTESIAN_POINT ( 'NONE',  ( 12.63842701281683034, 42.46726448433412315, 9.846743663894596210 ) ) ;
#3493 = CIRCLE ( 'NONE', #6686, 14.49999999999999822 ) ;
#3494 = CARTESIAN_POINT ( 'NONE',  ( 17.20831665107776587, 12.88393115100078390, 7.208316651077764980 ) ) ;
#3495 = CARTESIAN_POINT ( 'NONE',  ( -11.09922568453594316, -35.45969866340291077, 6.408140936763246920 ) ) ;
#3496 = ORIENTED_EDGE ( 'NONE', *, *, #58377, .T. ) ;
#3497 = VECTOR ( 'NONE', #5120, 1000.000000000000000 ) ;
#3498 = CARTESIAN_POINT ( 'NONE',  ( 12.91533473730993009, 11.60535201082150536, -10.88017736071109987 ) ) ;
#3499 = CARTESIAN_POINT ( 'NONE',  ( 12.63842701281683034, 12.46726448433411782, 9.846743663894596210 ) ) ;
#3500 = CARTESIAN_POINT ( 'NONE',  ( 14.92337183194729988, 64.34226448433412315, -8.527530157486177487 ) ) ;
#3501 = CARTESIAN_POINT ( 'NONE',  ( 19.42250999205614193, 45.14701867748817676, 5.440088680355555262 ) ) ;
#3503 = CARTESIAN_POINT ( 'NONE',  ( 10.00000000000000000, 42.87363466993042493, -12.81628187352647608 ) ) ;
#3502 = CARTESIAN_POINT ( 'NONE',  ( 4.559911319644449179, 23.89701867748817321, 9.422509992056141925 ) ) ;
#3504 = CARTESIAN_POINT ( 'NONE',  ( 2.917880565312948704, 37.63708216824731068, 12.26659068614894643 ) ) ;
#3505 = CARTESIAN_POINT ( 'NONE',  ( -14.97687855664607248, 0.5000000000000004441, -0.8325315005902533816 ) ) ;
#3506 = CARTESIAN_POINT ( 'NONE',  ( -1.099225684535947600, 64.54030133659709634, 6.408140936763237150 ) ) ;
#3507 = ORIENTED_EDGE ( 'NONE', *, *, #71148, .T. ) ;
#3508 = CARTESIAN_POINT ( 'NONE',  ( 12.63842701281683034, 52.46726448433413026, 9.846743663894596210 ) ) ;
#3509 = CARTESIAN_POINT ( 'NONE',  ( -14.82269085861165792, 0.5000000000000004441, -2.299529454047158250 ) ) ;
#3510 = CARTESIAN_POINT ( 'NONE',  ( 2.035157376598824452, 33.68868534415484106, 7.964842623401179544 ) ) ;
#3511 = ORIENTED_EDGE ( 'NONE', *, *, #78014, .T. ) ;
#3512 = CARTESIAN_POINT ( 'NONE',  ( 17.20831665107776587, 4.133931151000785675, -7.208316651077762316 ) ) ;
#3513 = CARTESIAN_POINT ( 'NONE',  ( 8.731067818237031375, 7.813309369127511061, -8.731067818237036704 ) ) ;
#3514 = CARTESIAN_POINT ( 'NONE',  ( 18.52753015748617571, 8.092264484334117824, 4.923371831947298993 ) ) ;
#3515 = CARTESIAN_POINT ( 'NONE',  ( 10.00000000000000000, 24.75893115100078745, -9.846743663894594434 ) ) ;
#3516 = ADVANCED_FACE ( 'NONE', ( #98158 ), #51654, .T. ) ;
#3517 = CARTESIAN_POINT ( 'NONE',  ( 7.361572987183169658, 4.967264484334119601, -9.846743663894592657 ) ) ;
#3518 = CARTESIAN_POINT ( 'NONE',  ( 10.00000000000000000, -0.2410688489992152128, -9.846743663894594434 ) ) ;
#3520 = FILL_AREA_STYLE_COLOUR ( '', #12041 ) ;
#3519 = CARTESIAN_POINT ( 'NONE',  ( 12.91533473730993009, 61.60535201082150536, -10.88017736071109987 ) ) ;
#3521 = CARTESIAN_POINT ( 'NONE',  ( 20.88017736071110164, 60.35535201082151957, 2.915334737309930979 ) ) ;
#3523 = EDGE_LOOP ( 'NONE', ( #75525, #72701, #98043, #81908 ) ) ;
#3522 = CARTESIAN_POINT ( 'NONE',  ( 2.791683348922240793, 16.63393115100078745, 7.208316651077764092 ) ) ;
#3524 = EDGE_CURVE ( 'NONE', #29181, #68203, #24300, .T. ) ;
#3525 = AXIS2_PLACEMENT_3D ( 'NONE', #97580, #29041, #59549 ) ;
#3526 = DIRECTION ( 'NONE',  ( 1.224646799147353207E-16, -1.540077580099091490E-33, 1.000000000000000000 ) ) ;
#3527 = CARTESIAN_POINT ( 'NONE',  ( 7.361572987183169658, 49.96726448433410894, -9.846743663894592657 ) ) ;
#3528 = ORIENTED_EDGE ( 'NONE', *, *, #92910, .F. ) ;
#3529 = FACE_OUTER_BOUND ( 'NONE', #93113, .T. ) ;
#3531 = EDGE_CURVE ( 'NONE', #34568, #83562, #70881, .T. ) ;
#3530 = CARTESIAN_POINT ( 'NONE',  ( 13.79529636645030344, 3.262082168247301350, 14.16423886937410614 ) ) ;
#3532 =( BOUNDED_SURFACE ( )  B_SPLINE_SURFACE ( 1, 2, ( 
 ( #81264, #58756, #97280, #12763, #21263, #31705, #75737, #22263, #38250, #98276, #37270, #61227, #45743, #38735, #91732, #7256, #760, #85219, #23254, #31211, #47198, #46236, #8717, #67757, #37760, #68256, #30224, #83244, #39235, #8241, #14767, #53729, #54697, #54209, #16723, #84726, #84246, #7756, #29733, #60241, #90736, #62198, #45240, #69236, #91228, #98776, #69723, #61707, #52737, #60729, #15750, #92221, #92706, #24231, #6753, #22752, #68741, #53235, #23749, #273, #30718, #15262, #1249, #83740, #76239, #76722, #16231, #46711, #77211, #39725, #48677, #86201, #70218, #33180, #95157, #64646, #78195, #40206, #79180, #48185, #41694, #25708, #47703, #93193, #10207, #1737, #9212, #63673, #17713, #10695, #94177, #9708, #71687, #57160, #56200, #3198, #19171, #18197, #79677, #32191, #70712, #2230, #32689, #55193, #11174, #41207, #85710, #86692, #26666, #26185, #87658, #56677, #33662, #78697, #62693, #24720, #17224, #3691, #63184, #64158, #93691, #25225, #72164, #94676, #55705, #40700, #87166, #18692, #77701, #34152, #71203, #2726, #49175, #34650, #89141, #27646, #58132, #35140, #5659, #80662, #65640, #65146, #35646, #89634, #66644, #11669, #66133, #96164, #42182, #50654, #21146, #59125, #57653, #19662, #96664, #88642, #36137, #43143, #88150, #28144, #58642, #20651, #51646, #81142, #27151, #13138, #12645, #97168, #50152, #73634, #4179, #12157, #20149, #5160, #51142, #81631, #43636, #74122, #28636, #42662, #82126, #49651, #80159, #95666, #73138, #72646, #4678, #41357, #86343, #54840, #48331, #24864, #24375, #63328, #71348, #85854, #17366, #3335, #79328, #17846, #91510, #78835, #10346, #7537, #47835, #25362, #83518, #10838, #30498, #2866, #78338, #2374, #71826, #85353, #64304, #32340, #15037, #22533, #93342, #16867, #63812, #76009, #51, #40846, #33317, #33797, #61000, #38028, #9353, #53004, #68520, #9859, #40358, #94322, #70859, #47341, #32829, #45509, #25843, #55347, #93836, #55848, #56341, #86835, #18339, #48819, #77844, #39858, #70364, #1881, #62842, #57795, #80309, #73294, #43289, #57305, #34293, #81293, #35792, #19801, #87314, #96318, #42317, #3834, #13290, #58278, #26811, #20304, #95816, #95307, #35292, #73784, #88303, #50292, #74269, #51290, #88796, #64790, #50804, #12789, #79814, #80805, #27793, #56816, #81775, #87797, #18832, #94815, #58785, #26318, #72304, #65785, #4818, #5314, #19315, #49801, #11809, #12302, #96815, #72790, #4327, #34799, #66280, #42810, #43778, #49312, #28291, #5800, #36290, #65289, #89291, #20801, #27296, #11318, #41837, #45772, #68770, #28779, #37786, #75272, #67285, #21293, #84275, #37296, #8265 ),
 ( #59277, #302, #51786, #52276, #23281, #82272, #52764, #60267, #60756, #29759, #44274, #14796, #15774, #91256, #98305, #90766, #22291, #68283, #30746, #83272, #83767, #13787, #45269, #61253, #89776, #98804, #75764, #82775, #7285, #15290, #29274, #6288, #53261, #7782, #30252, #74779, #22782, #14295, #36791, #46263, #76265, #97813, #38277, #67783, #59770, #91758, #53757, #76748, #66788, #97307, #90263, #21796, #44767, #6782, #2261, #23776, #32221, #40237, #785, #94206, #46741, #31238, #38765, #2753, #69265, #16259, #9737, #47728, #55737, #77239, #1281, #31734, #93222, #40728, #92737, #62230, #24261, #78725, #55225, #25736, #61733, #10235, #56228, #79209, #47226, #24746, #71230, #54725, #33209, #86228, #17739, #63703, #92251, #70745, #77729, #39264, #54241, #86722, #9241, #84754, #8743, #69753, #62722, #85245, #16751, #39752, #48215, #17252, #18226, #70249, #1765, #48706, #85739, #78225, #32716, #63214, #93718, #25252, #19200, #3226, #10719, #80187, #41723, #50686, #64188, #87197, #4710, #73171, #28176, #49202, #43177, #34183, #49683, #56706, #80690, #58670, #5192, #71714, #12186, #11700, #33690, #65176, #89172, #96697, #11204, #72193, #42692, #42209, #73665, #57683, #3722, #35172, #65673, #96194, #20683, #95697, #79706, #20183, #27181, #35680, #64675, #88179, #94708, #95185, #72676, #4211, #27679, #58164, #88675, #81178, #12678, #26693, #51177, #41236, #66164, #26213, #57189, #18720, #34681, #87686, #19693, #50180, #61131, #22665, #7669, #14172, #15165, #82156, #5687, #53141, #75648, #21677, #23159, #67670, #22166, #98683, #44152, #90147, #44656, #36675, #83650, #38160, #51677, #97198, #75151, #74154, #13170, #37177, #52163, #14676, #98180, #13668, #7160, #91641, #29636, #37663, #81660, #52648, #45646, #43667, #74660, #6171, #67163, #59158, #76143, #83151, #89664, #60144, #30624, #30132, #36173, #60638, #90641, #82656, #66673, #28666, #21175, #68646, #97687, #45142, #29149, #59656, #176, #68163, #6661, #91139, #62598, #9617, #40615, #10117, #2641, #53634, #54606, #69142, #40118, #85122, #16633, #62105, #84633, #33095, #93602, #78608, #47108, #86114, #54120, #76629, #25139, #47616, #92615, #94097, #39636, #93103, #70619, #16135, #24139, #77608, #8631, #55617, #71114, #23658, #670, #9121, #46143, #84154, #70125, #1647, #85620, #32099, #46621, #78111, #63588, #24633, #2144, #15660, #55100, #17625, #8148, #77119, #39140, #69630, #31120, #48095, #17137, #61615, #32604, #38641, #63100, #92133, #1154, #31614, #26576, #56111, #86605, #48589, #50565, #64071, #57565, #11095, #94586, #27560, #19575, #71608, #10604, #34558, #80576 ) ),
 .UNSPECIFIED., .F., .F., .F. ) 
 B_SPLINE_SURFACE_WITH_KNOTS ( ( 2, 2 ),
 ( 3, 2, 2, 2, 2, 2, 2, 2, 2, 2, 2, 2, 2, 2, 2, 2, 2, 2, 2, 2, 2, 2, 2, 2, 2, 2, 2, 2, 2, 2, 2, 2, 2, 2, 2, 2, 2, 2, 2, 2, 2, 2, 2, 2, 2, 2, 2, 2, 2, 2, 2, 2, 2, 2, 2, 2, 2, 2, 2, 2, 2, 2, 2, 2, 2, 2, 2, 2, 2, 2, 2, 2, 2, 2, 2, 2, 2, 2, 2, 2, 2, 2, 2, 2, 2, 2, 2, 2, 2, 2, 2, 2, 2, 2, 2, 2, 2, 2, 2, 2, 2, 2, 2, 2, 2, 2, 2, 2, 2, 2, 2, 2, 2, 2, 2, 2, 2, 2, 2, 2, 2, 2, 2, 2, 2, 2, 2, 2, 2, 2, 2, 2, 2, 2, 2, 2, 2, 2, 2, 2, 2, 2, 2, 2, 2, 2, 2, 2, 2, 2, 2, 2, 2, 2, 2, 2, 2, 2, 2, 2, 2, 2, 3 ),
 ( 0.000000000000000000, 1.000000000000000000 ),
 ( 0.000000000000000000, 0.005952380952380952051, 0.01190476190476190410, 0.01785714285714285615, 0.02380952380952380820, 0.02976190476190476025, 0.03571428571428571230, 0.04166666666666666435, 0.04761904761904761640, 0.05357142857142856845, 0.05952380952380952051, 0.06547619047619047949, 0.07142857142857142461, 0.07738095238095238360, 0.08333333333333332871, 0.08928571428571428770, 0.09523809523809523281, 0.1011904761904761918, 0.1071428571428571369, 0.1130952380952380959, 0.1190476190476190410, 0.1250000000000000000, 0.1309523809523809590, 0.1369047619047619180, 0.1428571428571428492, 0.1488095238095238082, 0.1547619047619047672, 0.1607142857142857262, 0.1666666666666666574, 0.1726190476190476164, 0.1785714285714285754, 0.1845238095238095344, 0.1904761904761904656, 0.1964285714285714246, 0.2023809523809523836, 0.2083333333333333426, 0.2142857142857142738, 0.2202380952380952328, 0.2261904761904761918, 0.2321428571428571508, 0.2380952380952380820, 0.2440476190476190410, 0.2500000000000000000, 0.2559523809523809312, 0.2619047619047619180, 0.2678571428571428492, 0.2738095238095238360, 0.2797619047619047672, 0.2857142857142856984, 0.2916666666666666852, 0.2976190476190476164, 0.3035714285714285476, 0.3095238095238095344, 0.3154761904761904656, 0.3214285714285714524, 0.3273809523809523836, 0.3333333333333333148, 0.3392857142857143016, 0.3452380952380952328, 0.3511904761904761640, 0.3571428571428571508, 0.3630952380952380820, 0.3690476190476190688, 0.3750000000000000000, 0.3809523809523809312, 0.3869047619047619180, 0.3928571428571428492, 0.3988095238095238360, 0.4047619047619047672, 0.4107142857142856984, 0.4166666666666666852, 0.4226190476190476164, 0.4285714285714285476, 0.4345238095238095344, 0.4404761904761904656, 0.4464285714285714524, 0.4523809523809523836, 0.4583333333333333148, 0.4642857142857143016, 0.4702380952380952328, 0.4761904761904761640, 0.4821428571428571508, 0.4880952380952380820, 0.4940476190476190688, 0.5000000000000000000, 0.5059523809523809312, 0.5119047619047618625, 0.5178571428571429047, 0.5238095238095238360, 0.5297619047619047672, 0.5357142857142856984, 0.5416666666666666297, 0.5476190476190476719, 0.5535714285714286031, 0.5595238095238095344, 0.5654761904761904656, 0.5714285714285713969, 0.5773809523809523281, 0.5833333333333333703, 0.5892857142857143016, 0.5952380952380952328, 0.6011904761904761640, 0.6071428571428570953, 0.6130952380952381375, 0.6190476190476190688, 0.6250000000000000000, 0.6309523809523809312, 0.6369047619047618625, 0.6428571428571429047, 0.6488095238095238360, 0.6547619047619047672, 0.6607142857142856984, 0.6666666666666666297, 0.6726190476190476719, 0.6785714285714286031, 0.6845238095238095344, 0.6904761904761904656, 0.6964285714285713969, 0.7023809523809523281, 0.7083333333333333703, 0.7142857142857143016, 0.7202380952380952328, 0.7261904761904761640, 0.7321428571428570953, 0.7380952380952381375, 0.7440476190476190688, 0.7500000000000000000, 0.7559523809523809312, 0.7619047619047618625, 0.7678571428571429047, 0.7738095238095238360, 0.7797619047619047672, 0.7857142857142856984, 0.7916666666666666297, 0.7976190476190476719, 0.8035714285714286031, 0.8095238095238095344, 0.8154761904761904656, 0.8214285714285713969, 0.8273809523809523281, 0.8333333333333333703, 0.8392857142857143016, 0.8452380952380952328, 0.8511904761904761640, 0.8571428571428570953, 0.8630952380952381375, 0.8690476190476190688, 0.8750000000000000000, 0.8809523809523809312, 0.8869047619047618625, 0.8928571428571429047, 0.8988095238095238360, 0.9047619047619047672, 0.9107142857142856984, 0.9166666666666666297, 0.9226190476190476719, 0.9285714285714286031, 0.9345238095238095344, 0.9404761904761904656, 0.9464285714285713969, 0.9523809523809523281, 0.9583333333333333703, 0.9642857142857143016 ),
 .UNSPECIFIED. ) 
 GEOMETRIC_REPRESENTATION_ITEM ( )  RATIONAL_B_SPLINE_SURFACE ( (
 ( 1.000000000000000000, 0.9659258262890683122, 1.000000000000000000, 0.9659258262890683122, 1.000000000000000000, 0.9659258262890683122, 1.000000000000000000, 0.9659258262890683122, 1.000000000000000000, 0.9659258262890683122, 1.000000000000000000, 0.9659258262890683122, 1.000000000000000000, 0.9659258262890683122, 1.000000000000000000, 0.9659258262890683122, 1.000000000000000000, 0.9659258262890683122, 1.000000000000000000, 0.9659258262890683122, 1.000000000000000000, 0.9659258262890683122, 1.000000000000000000, 0.9659258262890683122, 1.000000000000000000, 0.9659258262890683122, 1.000000000000000000, 0.9659258262890683122, 1.000000000000000000, 0.9659258262890683122, 1.000000000000000000, 0.9659258262890683122, 1.000000000000000000, 0.9659258262890683122, 1.000000000000000000, 0.9659258262890683122, 1.000000000000000000, 0.9659258262890683122, 1.000000000000000000, 0.9659258262890683122, 1.000000000000000000, 0.9659258262890683122, 1.000000000000000000, 0.9659258262890683122, 1.000000000000000000, 0.9659258262890683122, 1.000000000000000000, 0.9659258262890683122, 1.000000000000000000, 0.9659258262890683122, 1.000000000000000000, 0.9659258262890683122, 1.000000000000000000, 0.9659258262890683122, 1.000000000000000000, 0.9659258262890683122, 1.000000000000000000, 0.9659258262890683122, 1.000000000000000000, 0.9659258262890683122, 1.000000000000000000, 0.9659258262890683122, 1.000000000000000000, 0.9659258262890683122, 1.000000000000000000, 0.9659258262890683122, 1.000000000000000000, 0.9659258262890683122, 1.000000000000000000, 0.9659258262890683122, 1.000000000000000000, 0.9659258262890683122, 1.000000000000000000, 0.9659258262890683122, 1.000000000000000000, 0.9659258262890683122, 1.000000000000000000, 0.9659258262890683122, 1.000000000000000000, 0.9659258262890683122, 1.000000000000000000, 0.9659258262890683122, 1.000000000000000000, 0.9659258262890683122, 1.000000000000000000, 0.9659258262890683122, 1.000000000000000000, 0.9659258262890683122, 1.000000000000000000, 0.9659258262890683122, 1.000000000000000000, 0.9659258262890683122, 1.000000000000000000, 0.9659258262890683122, 1.000000000000000000, 0.9659258262890683122, 1.000000000000000000, 0.9659258262890683122, 1.000000000000000000, 0.9659258262890683122, 1.000000000000000000, 0.9659258262890683122, 1.000000000000000000, 0.9659258262890683122, 1.000000000000000000, 0.9659258262890683122, 1.000000000000000000, 0.9659258262890683122, 1.000000000000000000, 0.9659258262890683122, 1.000000000000000000, 0.9659258262890683122, 1.000000000000000000, 0.9659258262890683122, 1.000000000000000000, 0.9659258262890683122, 1.000000000000000000, 0.9659258262890683122, 1.000000000000000000, 0.9659258262890683122, 1.000000000000000000, 0.9659258262890683122, 1.000000000000000000, 0.9659258262890683122, 1.000000000000000000, 0.9659258262890683122, 1.000000000000000000, 0.9659258262890683122, 1.000000000000000000, 0.9659258262890683122, 1.000000000000000000, 0.9659258262890683122, 1.000000000000000000, 0.9659258262890683122, 1.000000000000000000, 0.9659258262890683122, 1.000000000000000000, 0.9659258262890683122, 1.000000000000000000, 0.9659258262890683122, 1.000000000000000000, 0.9659258262890683122, 1.000000000000000000, 0.9659258262890683122, 1.000000000000000000, 0.9659258262890683122, 1.000000000000000000, 0.9659258262890683122, 1.000000000000000000, 0.9659258262890683122, 1.000000000000000000, 0.9659258262890683122, 1.000000000000000000, 0.9659258262890683122, 1.000000000000000000, 0.9659258262890683122, 1.000000000000000000, 0.9659258262890683122, 1.000000000000000000, 0.9659258262890683122, 1.000000000000000000, 0.9659258262890683122, 1.000000000000000000, 0.9659258262890683122, 1.000000000000000000, 0.9659258262890683122, 1.000000000000000000, 0.9659258262890683122, 1.000000000000000000, 0.9659258262890683122, 1.000000000000000000, 0.9659258262890683122, 1.000000000000000000, 0.9659258262890683122, 1.000000000000000000, 0.9659258262890683122, 1.000000000000000000, 0.9659258262890683122, 1.000000000000000000, 0.9659258262890683122, 1.000000000000000000, 0.9659258262890683122, 1.000000000000000000, 0.9659258262890683122, 1.000000000000000000, 0.9659258262890683122, 1.000000000000000000, 0.9659258262890683122, 1.000000000000000000, 0.9659258262890683122, 1.000000000000000000, 0.9659258262890683122, 1.000000000000000000, 0.9659258262890683122, 1.000000000000000000, 0.9659258262890683122, 1.000000000000000000, 0.9659258262890683122, 1.000000000000000000, 0.9659258262890683122, 1.000000000000000000, 0.9659258262890683122, 1.000000000000000000, 0.9659258262890683122, 1.000000000000000000, 0.9659258262890683122, 1.000000000000000000, 0.9659258262890683122, 1.000000000000000000, 0.9659258262890683122, 1.000000000000000000, 0.9659258262890683122, 1.000000000000000000, 0.9659258262890683122, 1.000000000000000000, 0.9659258262890683122, 1.000000000000000000, 0.9659258262890683122, 1.000000000000000000, 0.9659258262890683122, 1.000000000000000000, 0.9659258262890683122, 1.000000000000000000, 0.9659258262890683122, 1.000000000000000000, 0.9659258262890683122, 1.000000000000000000, 0.9659258262890683122, 1.000000000000000000, 0.9659258262890683122, 1.000000000000000000, 0.9659258262890683122, 1.000000000000000000, 0.9659258262890683122, 1.000000000000000000, 0.9659258262890683122, 1.000000000000000000, 0.9659258262890683122, 1.000000000000000000, 0.9659258262890683122, 1.000000000000000000, 0.9659258262890683122, 1.000000000000000000, 0.9659258262890683122, 1.000000000000000000, 0.9659258262890683122, 1.000000000000000000, 0.9659258262890683122, 1.000000000000000000, 0.9659258262890683122, 1.000000000000000000, 0.9659258262890683122, 1.000000000000000000, 0.9659258262890683122, 1.000000000000000000, 0.9659258262890683122, 1.000000000000000000, 0.9659258262890683122, 1.000000000000000000, 0.9659258262890683122, 1.000000000000000000, 0.9659258262890683122, 1.000000000000000000, 0.9659258262890683122, 1.000000000000000000, 0.9659258262890683122, 1.000000000000000000, 0.9659258262890683122, 1.000000000000000000, 0.9659258262890683122, 1.000000000000000000, 0.9659258262890683122, 1.000000000000000000, 0.9659258262890683122, 1.000000000000000000, 0.9659258262890683122, 1.000000000000000000, 0.9659258262890683122, 1.000000000000000000, 0.9659258262890683122, 1.000000000000000000, 0.9659258262890683122, 1.000000000000000000, 0.9659258262890683122, 1.000000000000000000, 0.9659258262890683122, 1.000000000000000000, 0.9659258262890683122, 1.000000000000000000, 0.9659258262890683122, 1.000000000000000000, 0.9659258262890683122, 1.000000000000000000, 0.9659258262890683122, 1.000000000000000000, 0.9659258262890683122, 1.000000000000000000, 0.9659258262890683122, 1.000000000000000000, 0.9659258262890683122, 1.000000000000000000, 0.9659258262890683122, 1.000000000000000000, 0.9659258262890683122, 1.000000000000000000, 0.9659258262890683122, 1.000000000000000000, 0.9659258262890683122, 1.000000000000000000, 0.9659258262890683122, 1.000000000000000000, 0.9659258262890683122, 1.000000000000000000, 0.9659258262890683122, 1.000000000000000000, 0.9659258262890683122, 1.000000000000000000, 0.9659258262890683122, 1.000000000000000000, 0.9659258262890683122, 1.000000000000000000, 0.9659258262890683122, 1.000000000000000000, 0.9659258262890683122, 1.000000000000000000),
 ( 1.000000000000000000, 0.9659258262890683122, 1.000000000000000000, 0.9659258262890683122, 1.000000000000000000, 0.9659258262890683122, 1.000000000000000000, 0.9659258262890683122, 1.000000000000000000, 0.9659258262890683122, 1.000000000000000000, 0.9659258262890683122, 1.000000000000000000, 0.9659258262890683122, 1.000000000000000000, 0.9659258262890683122, 1.000000000000000000, 0.9659258262890683122, 1.000000000000000000, 0.9659258262890683122, 1.000000000000000000, 0.9659258262890683122, 1.000000000000000000, 0.9659258262890683122, 1.000000000000000000, 0.9659258262890683122, 1.000000000000000000, 0.9659258262890683122, 1.000000000000000000, 0.9659258262890683122, 1.000000000000000000, 0.9659258262890683122, 1.000000000000000000, 0.9659258262890683122, 1.000000000000000000, 0.9659258262890683122, 1.000000000000000000, 0.9659258262890683122, 1.000000000000000000, 0.9659258262890683122, 1.000000000000000000, 0.9659258262890683122, 1.000000000000000000, 0.9659258262890683122, 1.000000000000000000, 0.9659258262890683122, 1.000000000000000000, 0.9659258262890683122, 1.000000000000000000, 0.9659258262890683122, 1.000000000000000000, 0.9659258262890683122, 1.000000000000000000, 0.9659258262890683122, 1.000000000000000000, 0.9659258262890683122, 1.000000000000000000, 0.9659258262890683122, 1.000000000000000000, 0.9659258262890683122, 1.000000000000000000, 0.9659258262890683122, 1.000000000000000000, 0.9659258262890683122, 1.000000000000000000, 0.9659258262890683122, 1.000000000000000000, 0.9659258262890683122, 1.000000000000000000, 0.9659258262890683122, 1.000000000000000000, 0.9659258262890683122, 1.000000000000000000, 0.9659258262890683122, 1.000000000000000000, 0.9659258262890683122, 1.000000000000000000, 0.9659258262890683122, 1.000000000000000000, 0.9659258262890683122, 1.000000000000000000, 0.9659258262890683122, 1.000000000000000000, 0.9659258262890683122, 1.000000000000000000, 0.9659258262890683122, 1.000000000000000000, 0.9659258262890683122, 1.000000000000000000, 0.9659258262890683122, 1.000000000000000000, 0.9659258262890683122, 1.000000000000000000, 0.9659258262890683122, 1.000000000000000000, 0.9659258262890683122, 1.000000000000000000, 0.9659258262890683122, 1.000000000000000000, 0.9659258262890683122, 1.000000000000000000, 0.9659258262890683122, 1.000000000000000000, 0.9659258262890683122, 1.000000000000000000, 0.9659258262890683122, 1.000000000000000000, 0.9659258262890683122, 1.000000000000000000, 0.9659258262890683122, 1.000000000000000000, 0.9659258262890683122, 1.000000000000000000, 0.9659258262890683122, 1.000000000000000000, 0.9659258262890683122, 1.000000000000000000, 0.9659258262890683122, 1.000000000000000000, 0.9659258262890683122, 1.000000000000000000, 0.9659258262890683122, 1.000000000000000000, 0.9659258262890683122, 1.000000000000000000, 0.9659258262890683122, 1.000000000000000000, 0.9659258262890683122, 1.000000000000000000, 0.9659258262890683122, 1.000000000000000000, 0.9659258262890683122, 1.000000000000000000, 0.9659258262890683122, 1.000000000000000000, 0.9659258262890683122, 1.000000000000000000, 0.9659258262890683122, 1.000000000000000000, 0.9659258262890683122, 1.000000000000000000, 0.9659258262890683122, 1.000000000000000000, 0.9659258262890683122, 1.000000000000000000, 0.9659258262890683122, 1.000000000000000000, 0.9659258262890683122, 1.000000000000000000, 0.9659258262890683122, 1.000000000000000000, 0.9659258262890683122, 1.000000000000000000, 0.9659258262890683122, 1.000000000000000000, 0.9659258262890683122, 1.000000000000000000, 0.9659258262890683122, 1.000000000000000000, 0.9659258262890683122, 1.000000000000000000, 0.9659258262890683122, 1.000000000000000000, 0.9659258262890683122, 1.000000000000000000, 0.9659258262890683122, 1.000000000000000000, 0.9659258262890683122, 1.000000000000000000, 0.9659258262890683122, 1.000000000000000000, 0.9659258262890683122, 1.000000000000000000, 0.9659258262890683122, 1.000000000000000000, 0.9659258262890683122, 1.000000000000000000, 0.9659258262890683122, 1.000000000000000000, 0.9659258262890683122, 1.000000000000000000, 0.9659258262890683122, 1.000000000000000000, 0.9659258262890683122, 1.000000000000000000, 0.9659258262890683122, 1.000000000000000000, 0.9659258262890683122, 1.000000000000000000, 0.9659258262890683122, 1.000000000000000000, 0.9659258262890683122, 1.000000000000000000, 0.9659258262890683122, 1.000000000000000000, 0.9659258262890683122, 1.000000000000000000, 0.9659258262890683122, 1.000000000000000000, 0.9659258262890683122, 1.000000000000000000, 0.9659258262890683122, 1.000000000000000000, 0.9659258262890683122, 1.000000000000000000, 0.9659258262890683122, 1.000000000000000000, 0.9659258262890683122, 1.000000000000000000, 0.9659258262890683122, 1.000000000000000000, 0.9659258262890683122, 1.000000000000000000, 0.9659258262890683122, 1.000000000000000000, 0.9659258262890683122, 1.000000000000000000, 0.9659258262890683122, 1.000000000000000000, 0.9659258262890683122, 1.000000000000000000, 0.9659258262890683122, 1.000000000000000000, 0.9659258262890683122, 1.000000000000000000, 0.9659258262890683122, 1.000000000000000000, 0.9659258262890683122, 1.000000000000000000, 0.9659258262890683122, 1.000000000000000000, 0.9659258262890683122, 1.000000000000000000, 0.9659258262890683122, 1.000000000000000000, 0.9659258262890683122, 1.000000000000000000, 0.9659258262890683122, 1.000000000000000000, 0.9659258262890683122, 1.000000000000000000, 0.9659258262890683122, 1.000000000000000000, 0.9659258262890683122, 1.000000000000000000, 0.9659258262890683122, 1.000000000000000000, 0.9659258262890683122, 1.000000000000000000, 0.9659258262890683122, 1.000000000000000000, 0.9659258262890683122, 1.000000000000000000, 0.9659258262890683122, 1.000000000000000000, 0.9659258262890683122, 1.000000000000000000, 0.9659258262890683122, 1.000000000000000000, 0.9659258262890683122, 1.000000000000000000, 0.9659258262890683122, 1.000000000000000000, 0.9659258262890683122, 1.000000000000000000, 0.9659258262890683122, 1.000000000000000000, 0.9659258262890683122, 1.000000000000000000, 0.9659258262890683122, 1.000000000000000000, 0.9659258262890683122, 1.000000000000000000, 0.9659258262890683122, 1.000000000000000000, 0.9659258262890683122, 1.000000000000000000, 0.9659258262890683122, 1.000000000000000000, 0.9659258262890683122, 1.000000000000000000, 0.9659258262890683122, 1.000000000000000000, 0.9659258262890683122, 1.000000000000000000, 0.9659258262890683122, 1.000000000000000000, 0.9659258262890683122, 1.000000000000000000, 0.9659258262890683122, 1.000000000000000000, 0.9659258262890683122, 1.000000000000000000, 0.9659258262890683122, 1.000000000000000000, 0.9659258262890683122, 1.000000000000000000, 0.9659258262890683122, 1.000000000000000000, 0.9659258262890683122, 1.000000000000000000, 0.9659258262890683122, 1.000000000000000000, 0.9659258262890683122, 1.000000000000000000, 0.9659258262890683122, 1.000000000000000000, 0.9659258262890683122, 1.000000000000000000, 0.9659258262890683122, 1.000000000000000000, 0.9659258262890683122, 1.000000000000000000, 0.9659258262890683122, 1.000000000000000000, 0.9659258262890683122, 1.000000000000000000, 0.9659258262890683122, 1.000000000000000000, 0.9659258262890683122, 1.000000000000000000, 0.9659258262890683122, 1.000000000000000000, 0.9659258262890683122, 1.000000000000000000) ) ) 
 REPRESENTATION_ITEM ( '' )  SURFACE ( )  );
#3533 = UNCERTAINTY_MEASURE_WITH_UNIT (LENGTH_MEASURE( 1.000000000000000082E-05 ), #4520, 'distance_accuracy_value', 'NONE');
#3534 = FACE_OUTER_BOUND ( 'NONE', #20812, .T. ) ;
#3535 = CARTESIAN_POINT ( 'NONE',  ( 13.79529636645030344, 23.26208216824730002, 14.16423886937410614 ) ) ;
#3536 = CARTESIAN_POINT ( 'NONE',  ( 10.00000000000000178, 28.05374883491396787, 14.16423886937410082 ) ) ;
#3537 = CARTESIAN_POINT ( 'NONE',  ( 2.917880565312948704, 2.637082168247300906, 12.26659068614894643 ) ) ;
#3538 = CARTESIAN_POINT ( 'NONE',  ( 4.555630843329476320, 77.03495325336415078, 9.500000000000000000 ) ) ;
#3539 = CARTESIAN_POINT ( 'NONE',  ( 0.5774900079438590739, 32.64701867748816966, -5.440088680355550821 ) ) ;
#3540 = CARTESIAN_POINT ( 'NONE',  ( -1.829604203029787435, 15.00000000000000000, 15.89119079541584334 ) ) ;
#3541 = VERTEX_POINT ( 'NONE', #60619 ) ;
#3542 = CARTESIAN_POINT ( 'NONE',  ( 0.1532563361054082862, 21.21726448433412315, 2.638427012816831674 ) ) ;
#3544 = CARTESIAN_POINT ( 'NONE',  ( 14.92337183194729988, 19.34226448433411960, -8.527530157486177487 ) ) ;
#3543 = CARTESIAN_POINT ( 'NONE',  ( 7.084665262690076126, 52.02201867748816255, -10.88017736071110164 ) ) ;
#3545 = EDGE_CURVE ( 'NONE', #2502, #13075, #52604, .T. ) ;
#3546 = VERTEX_POINT ( 'NONE', #61597 ) ;
#3547 = CARTESIAN_POINT ( 'NONE',  ( 19.38216949554541202, 45.99863466993041072, 9.382169495545424454 ) ) ;
#3548 = CARTESIAN_POINT ( 'NONE',  ( 18.52753015748618282, 38.92559781766745175, -4.923371831947291888 ) ) ;
#3549 = DIRECTION ( 'NONE',  ( 0.000000000000000000, 1.000000000000000000, 0.000000000000000000 ) ) ;
#3550 = CARTESIAN_POINT ( 'NONE',  ( 19.38216949554541202, 30.99863466993042138, 9.382169495545424454 ) ) ;
#3551 = CARTESIAN_POINT ( 'NONE',  ( 3.795296366450306547, -34.65458449841935362, -14.16423886937410259 ) ) ;
#3552 = COLOUR_RGB ( '', 0.40784314, 0.44705882, 0.49803922) ;
#3553 = CARTESIAN_POINT ( 'NONE',  ( 5.076628168052704559, 25.17559781766745175, -8.527530157486179263 ) ) ;
#3554 = CARTESIAN_POINT ( 'NONE',  ( 20.36894250292379382, 13.67874883491396965, 10.36894250292379205 ) ) ;
#3555 = EDGE_LOOP ( 'NONE', ( #49020, #19116, #92730, #26142 ) ) ;
#3556 = CARTESIAN_POINT ( 'NONE',  ( 19.42250999205614548, 40.98035201082150536, -5.440088680355545492 ) ) ;
#3557 = CARTESIAN_POINT ( 'NONE',  ( 12.91533473730992121, 49.52201867748817676, 10.88017736071110164 ) ) ;
#3558 = CARTESIAN_POINT ( 'NONE',  ( 13.79529636645031943, 40.34541550158063217, -14.16423886937409904 ) ) ;
#3559 = CARTESIAN_POINT ( 'NONE',  ( 7.361572987183170547, 57.05059781766744464, 9.846743663894590881 ) ) ;
#3560 = CARTESIAN_POINT ( 'NONE',  ( 17.20831665107776587, 14.13393115100078568, -7.208316651077762316 ) ) ;
#3561 = CIRCLE ( 'NONE', #80194, 14.49999999999999822 ) ;
#3563 = CARTESIAN_POINT ( 'NONE',  ( 0.000000000000000000, 15.00000000000000000, 0.000000000000000000 ) ) ;
#3562 = CARTESIAN_POINT ( 'NONE',  ( 1.114591949024916984, 15.00000000000000000, 14.45709807627962817 ) ) ;
#3564 = CARTESIAN_POINT ( 'NONE',  ( -0.8801773607111008646, 43.27201867748817676, 2.915334737309923430 ) ) ;
#3565 = EDGE_CURVE ( 'NONE', #78790, #60237, #48075, .T. ) ;
#3566 = VECTOR ( 'NONE', #79091, 1000.000000000000000 ) ;
#3567 = CARTESIAN_POINT ( 'NONE',  ( -3.250000000000000444, 1.019547802438465656, -2.500000000000000000 ) ) ;
#3568 = CARTESIAN_POINT ( 'NONE',  ( 21.09922568453594849, 16.20696800326375353, 6.408140936763242479 ) ) ;
#3569 = CARTESIAN_POINT ( 'NONE',  ( 0.1532563361054083140, 51.00893115100078745, 1.131784320476157264E-15 ) ) ;
#3570 = CARTESIAN_POINT ( 'NONE',  ( 10.88017736071110519, 15.56368534415484461, -2.602085213965210642E-15 ) ) ;
#3571 = SURFACE_SIDE_STYLE ('',( #26063 ) ) ;
#3572 = VECTOR ( 'NONE', #46827, 1000.000000000000114 ) ;
#3573 = CARTESIAN_POINT ( 'NONE',  ( 12.91533473730992121, 64.52201867748817676, 10.88017736071110164 ) ) ;
#3574 = CARTESIAN_POINT ( 'NONE',  ( -8.218805110708677475, -9.361916056596390590, 4.000000000000000000 ) ) ;
#3575 = DIRECTION ( 'NONE',  ( -0.8703556959398977000, 0.000000000000000000, -0.4924235601034707699 ) ) ;
#3576 = CIRCLE ( 'NONE', #38757, 0.09999999999999982514 ) ;
#3577 = CARTESIAN_POINT ( 'NONE',  ( 0.1532563361054083140, 1.008931151000784787, 1.131784320476157264E-15 ) ) ;
#3578 = CARTESIAN_POINT ( 'NONE',  ( 7.361572987183169658, -0.03273551566588185635, -9.846743663894592657 ) ) ;
#3579 = DIRECTION ( 'NONE',  ( 0.000000000000000000, 0.000000000000000000, 1.000000000000000000 ) ) ;
#3580 = CARTESIAN_POINT ( 'NONE',  ( 0.1532563361054100626, 25.80059781766744820, -2.638427012816831230 ) ) ;
#3581 = CARTESIAN_POINT ( 'NONE',  ( -0.8801773607110991993, 17.85535201082150536, -2.915334737309923874 ) ) ;
#3582 = CARTESIAN_POINT ( 'NONE',  ( 7.361572987183170547, 62.05059781766745886, 9.846743663894590881 ) ) ;
#3584 = CARTESIAN_POINT ( 'NONE',  ( 19.39188664607695145, 55.83703382326400799, -6.499999999999960920 ) ) ;
#3583 = CARTESIAN_POINT ( 'NONE',  ( 19.42250999205614548, 40.98035201082150536, -5.440088680355545492 ) ) ;
#3585 = CARTESIAN_POINT ( 'NONE',  ( -2.816281873526473856, 44.33196800326375353, 3.434112377981055619 ) ) ;
#3586 = VERTEX_POINT ( 'NONE', #85602 ) ;
#3587 = CARTESIAN_POINT ( 'NONE',  ( 20.88017736071110875, 50.77201867748817676, -2.915334737309920765 ) ) ;
#3589 = SURFACE_SIDE_STYLE ('',( #48571 ) ) ;
#3588 = CARTESIAN_POINT ( 'NONE',  ( -1.099225684535947600, 23.70696800326375708, -6.408140936763238038 ) ) ;
#3590 = CARTESIAN_POINT ( 'NONE',  ( 17.08211943468705130, 48.47041550158063927, 12.26659068614894998 ) ) ;
#3591 = CARTESIAN_POINT ( 'NONE',  ( 0.1532563361054082862, 46.21726448433411605, 2.638427012816831674 ) ) ;
#3592 = CARTESIAN_POINT ( 'NONE',  ( 1.472469842513823179, 1.425597817667451528, 4.923371831947296329 ) ) ;
#3593 = CARTESIAN_POINT ( 'NONE',  ( 7.084665262690076126, 69.10535201082151957, 10.88017736071109987 ) ) ;
#3594 = CARTESIAN_POINT ( 'NONE',  ( 2.781662917646512463E-16, 22.11937003968011695, 0.000000000000000000 ) ) ;
#3595 = CARTESIAN_POINT ( 'NONE',  ( 22.26659068614895176, 29.72041550158063572, -7.082119434687042414 ) ) ;
#3596 = CARTESIAN_POINT ( 'NONE',  ( -45.94000000000001194, 107.5383484153110061, -12.00000000000000000 ) ) ;
#3597 = CARTESIAN_POINT ( 'NONE',  ( 9.065164099344587001, 14.49999999999999112, -11.95084933600771038 ) ) ;
#3598 = ORIENTED_EDGE ( 'NONE', *, *, #21717, .T. ) ;
#3599 = VERTEX_POINT ( 'NONE', #47599 ) ;
#3600 = AXIS2_PLACEMENT_3D ( 'NONE', #83921, #45930, #15451 ) ;
#3601 = CARTESIAN_POINT ( 'NONE',  ( 20.36894250292379382, 48.67874883491396076, 10.36894250292379205 ) ) ;
#3602 = CARTESIAN_POINT ( 'NONE',  ( -4.164238869374099927, 52.01208216824729647, 3.795296366450308767 ) ) ;
#3603 = CARTESIAN_POINT ( 'NONE',  ( 1.472469842513823179, 11.42559781766745175, 4.923371831947296329 ) ) ;
#3604 = CARTESIAN_POINT ( 'NONE',  ( 11.36220558718857099, 4.586546245355948473E-16, 9.008345252845320061 ) ) ;
#3605 = DIRECTION ( 'NONE',  ( 0.000000000000000000, 0.000000000000000000, -1.000000000000000000 ) ) ;
#3607 = CARTESIAN_POINT ( 'NONE',  ( 13.43411237798106583, 32.66530133659708213, -12.81628187352647252 ) ) ;
#3606 = CARTESIAN_POINT ( 'NONE',  ( 19.42250999205614548, 5.980352010821504471, -5.440088680355545492 ) ) ;
#3608 = CARTESIAN_POINT ( 'NONE',  ( 20.36894250292379382, 48.67874883491396076, 10.36894250292379205 ) ) ;
#3609 = CARTESIAN_POINT ( 'NONE',  ( 9.846743663894590881, -1.699402182332547362, 2.638427012816828565 ) ) ;
#3610 = ADVANCED_FACE ( 'NONE', ( #16614 ), #32081, .T. ) ;
#3611 = VERTEX_POINT ( 'NONE', #54590 ) ;
#3612 = CARTESIAN_POINT ( 'NONE',  ( 10.00000000000000000, 24.75893115100078745, -9.846743663894594434 ) ) ;
#3613 = ORIENTED_EDGE ( 'NONE', *, *, #97214, .F. ) ;
#3615 = CARTESIAN_POINT ( 'NONE',  ( 10.00000000000000178, 9.313685344154839285, 10.88017736071110342 ) ) ;
#3614 = CARTESIAN_POINT ( 'NONE',  ( 10.00000000000000178, 9.313685344154839285, 10.88017736071110342 ) ) ;
#3617 = CARTESIAN_POINT ( 'NONE',  ( -1.099225684535947600, 8.706968003263753531, -6.408140936763238038 ) ) ;
#3616 = CARTESIAN_POINT ( 'NONE',  ( 7.361572987183169658, 44.96726448433412315, -9.846743663894592657 ) ) ;
#3618 = FILL_AREA_STYLE ('',( #18134 ) ) ;
#3619 = ADVANCED_FACE ( 'NONE', ( #78588 ), #654, .T. ) ;
#3620 = LINE ( 'NONE', #54624, #14493 ) ;
#3621 = VECTOR ( 'NONE', #34408, 1000.000000000000000 ) ;
#3622 = CARTESIAN_POINT ( 'NONE',  ( 19.38216949554541202, 20.99863466993042138, 9.382169495545424454 ) ) ;
#3623 = ORIENTED_EDGE ( 'NONE', *, *, #17437, .T. ) ;
#3624 = VECTOR ( 'NONE', #76938, 1000.000000000000000 ) ;
#3625 = CARTESIAN_POINT ( 'NONE',  ( 24.16423886937410614, 54.51208216824730357, -3.795296366450302550 ) ) ;
#3626 = ORIENTED_EDGE ( 'NONE', *, *, #17312, .T. ) ;
#3627 = AXIS2_PLACEMENT_3D ( 'NONE', #11825, #31981, #54984 ) ;
#3628 = CARTESIAN_POINT ( 'NONE',  ( -4.164238869374098151, 56.59541550158063927, -3.795296366450310543 ) ) ;
#3629 = ORIENTED_EDGE ( 'NONE', *, *, #87817, .F. ) ;
#3630 = CARTESIAN_POINT ( 'NONE',  ( 2.035157376598824452, 38.68868534415483396, 7.964842623401179544 ) ) ;
#3631 = CARTESIAN_POINT ( 'NONE',  ( 4.559911319644449179, 47.23035201082150536, -9.422509992056141925 ) ) ;
#3632 = CARTESIAN_POINT ( 'NONE',  ( 17.96484262340118221, 34.93868534415482685, 7.964842623401181321 ) ) ;
#3633 = PRESENTATION_LAYER_ASSIGNMENT (  '', '', ( #18047 ) ) ;
#3634 = CARTESIAN_POINT ( 'NONE',  ( -4.000000000000000000, 9.750000000000000000, 3.750000000000000000 ) ) ;
#3635 = CARTESIAN_POINT ( 'NONE',  ( 10.00000000000000000, 46.81368534415484106, -10.88017736071110342 ) ) ;
#3636 = AXIS2_PLACEMENT_3D ( 'NONE', #1639, #80067, #78596 ) ;
#3637 = EDGE_CURVE ( 'NONE', #55747, #22305, #17116, .T. ) ;
#3638 = CARTESIAN_POINT ( 'NONE',  ( 1.472469842513823179, 15.59226448433411960, -4.923371831947296329 ) ) ;
#3639 = ORIENTED_EDGE ( 'NONE', *, *, #10567, .T. ) ;
#3640 = CARTESIAN_POINT ( 'NONE',  ( -7.750355510519348456, 84.07179676972448590, 3.750000000000000000 ) ) ;
#3641 = CARTESIAN_POINT ( 'NONE',  ( 0.1532563361054100626, 40.80059781766745886, -2.638427012816831230 ) ) ;
#3643 = EDGE_CURVE ( 'NONE', #45856, #25477, #79177, .T. ) ;
#3642 = DIRECTION ( 'NONE',  ( 0.000000000000000000, -1.000000000000000000, -0.000000000000000000 ) ) ;
#3644 = CARTESIAN_POINT ( 'NONE',  ( 13.43411237798105340, 60.58196800326376064, 12.81628187352647963 ) ) ;
#3645 = VECTOR ( 'NONE', #52937, 1000.000000000000000 ) ;
#3646 = CARTESIAN_POINT ( 'NONE',  ( 0.000000000000000000, 91.00000000000000000, -8.000000000000000000 ) ) ;
#3647 = LINE ( 'NONE', #34112, #18881 ) ;
#3648 = CARTESIAN_POINT ( 'NONE',  ( -43.79988333157628233, 106.6859424350824668, 5.014248105693637214 ) ) ;
#3649 = CARTESIAN_POINT ( 'NONE',  ( 0.000000000000000000, 14.49999999999999822, 0.000000000000000000 ) ) ;
#3650 = CARTESIAN_POINT ( 'NONE',  ( -0.3689425029237898834, 61.17874883491396076, -10.36894250292378850 ) ) ;
#3651 = CARTESIAN_POINT ( 'NONE',  ( 1.274849032794278747, 57.55509018479938277, -6.499999999999960032 ) ) ;
#3652 = ORIENTED_EDGE ( 'NONE', *, *, #46207, .T. ) ;
#3653 = DIRECTION ( 'NONE',  ( -1.000000000000000000, 0.000000000000000000, 0.000000000000000000 ) ) ;
#3654 = CARTESIAN_POINT ( 'NONE',  ( 10.00000000000000178, 32.25893115100078745, 9.846743663894594434 ) ) ;
#3655 = CARTESIAN_POINT ( 'NONE',  ( 10.83696084481538691, -98.17058944465519232, -3.750000000000001776 ) ) ;
#3656 = CARTESIAN_POINT ( 'NONE',  ( 13.43411237798105340, 10.58196800326375353, 12.81628187352647963 ) ) ;
#3657 = CARTESIAN_POINT ( 'NONE',  ( 20.88017736071110519, 60.56368534415484106, 2.639326808657452039E-16 ) ) ;
#3658 =( NAMED_UNIT ( * ) PLANE_ANGLE_UNIT ( ) SI_UNIT ( $, .RADIAN. ) );
#3659 = CARTESIAN_POINT ( 'NONE',  ( 5.076628168052704559, 15.17559781766745175, -8.527530157486179263 ) ) ;
#3660 = CARTESIAN_POINT ( 'NONE',  ( 10.00000000000000000, 54.75893115100078745, -9.846743663894594434 ) ) ;
#3661 = CARTESIAN_POINT ( 'NONE',  ( 24.35999999999999233, 44.99999999999997158, -9.500000000000000000 ) ) ;
#3662 = EDGE_CURVE ( 'NONE', #79731, #25163, #48380, .T. ) ;
#3663 = EDGE_CURVE ( 'NONE', #95321, #60992, #18094, .T. ) ;
#3664 = ORIENTED_EDGE ( 'NONE', *, *, #18435, .F. ) ;
#3665 = CARTESIAN_POINT ( 'NONE',  ( 24.16423886937410614, 64.51208216824728936, -3.795296366450302550 ) ) ;
#3666 = FACE_OUTER_BOUND ( 'NONE', #86022, .T. ) ;
#3667 = CARTESIAN_POINT ( 'NONE',  ( 19.42250999205614193, 40.14701867748817676, 5.440088680355555262 ) ) ;
#3669 = CARTESIAN_POINT ( 'NONE',  ( 11.23445519025490036, 12.65797429472845792, -2.010653977028116213 ) ) ;
#3668 = CARTESIAN_POINT ( 'NONE',  ( 19.38216949554541202, 25.99863466993042138, 9.382169495545424454 ) ) ;
#3670 = DIRECTION ( 'NONE',  ( 0.000000000000000000, -0.000000000000000000, -1.000000000000000000 ) ) ;
#3671 = EDGE_CURVE ( 'NONE', #42104, #71871, #71908, .T. ) ;
#3672 = DIRECTION ( 'NONE',  ( -0.08715574274765140739, -0.9961946980917462113, 0.000000000000000000 ) ) ;
#3673 = DIRECTION ( 'NONE',  ( -0.000000000000000000, -0.000000000000000000, -1.000000000000000000 ) ) ;
#3674 = CARTESIAN_POINT ( 'NONE',  ( 0.1532563361054100626, 50.80059781766745175, -2.638427012816831230 ) ) ;
#3675 = CARTESIAN_POINT ( 'NONE',  ( 5.076628168052704559, 10.17559781766745175, -8.527530157486179263 ) ) ;
#3676 = CARTESIAN_POINT ( 'NONE',  ( 7.964842623401177768, -18.81131465584515894, -7.964842623401181321 ) ) ;
#3677 = CARTESIAN_POINT ( 'NONE',  ( 0.6178305044545838731, 19.74863466993042138, 9.382169495545420901 ) ) ;
#3678 = CARTESIAN_POINT ( 'NONE',  ( -11.62646502377548607, -81.99905065409454608, -3.750000000000000000 ) ) ;
#3680 = CARTESIAN_POINT ( 'NONE',  ( 8.470897558477529898, 2.354751593366954943E-16, 11.92401951126086779 ) ) ;
#3679 = CARTESIAN_POINT ( 'NONE',  ( 7.084665262690076126, 24.10535201082150181, 10.88017736071109987 ) ) ;
#3681 = DIRECTION ( 'NONE',  ( 0.000000000000000000, 1.000000000000000000, 0.000000000000000000 ) ) ;
#3682 = CARTESIAN_POINT ( 'NONE',  ( 2.917880565312950480, 40.97041550158063217, -12.26659068614894821 ) ) ;
#3683 = CARTESIAN_POINT ( 'NONE',  ( 13.79529636645031943, 35.34541550158063927, -14.16423886937409904 ) ) ;
#3684 = STYLED_ITEM ( 'NONE', ( #40350 ), #65927 ) ;
#3685 = CARTESIAN_POINT ( 'NONE',  ( 7.361572987183169658, 39.96726448433411605, -9.846743663894592657 ) ) ;
#3686 = CARTESIAN_POINT ( 'NONE',  ( -2.816281873526473856, 34.12363466993042493, 9.499525473075851096E-16 ) ) ;
#3687 = CARTESIAN_POINT ( 'NONE',  ( 7.084665262690076126, 27.02201867748817676, -10.88017736071110164 ) ) ;
#3688 = CARTESIAN_POINT ( 'NONE',  ( 14.92337183194729988, 54.34226448433412315, -8.527530157486177487 ) ) ;
#3689 = CARTESIAN_POINT ( 'NONE',  ( 4.559911319644449179, 42.23035201082151247, -9.422509992056141925 ) ) ;
#3690 = CARTESIAN_POINT ( 'NONE',  ( 16.40814093676323893, 5.790301336597087456, 11.09922568453595026 ) ) ;
#3691 = CARTESIAN_POINT ( 'NONE',  ( 20.36894250292379738, 24.92874883491396787, -10.36894250292379027 ) ) ;
#3692 = CARTESIAN_POINT ( 'NONE',  ( -0.1503990784575359729, 13.10158574516642105, 6.262539305110062848 ) ) ;
#3693 = VECTOR ( 'NONE', #41023, 1000.000000000000000 ) ;
#3694 = PRESENTATION_LAYER_ASSIGNMENT (  '', '', ( #89897 ) ) ;
#3695 = CARTESIAN_POINT ( 'NONE',  ( 19.84674366389459266, 28.71726448433411960, -2.638427012816827677 ) ) ;
#3696 = CARTESIAN_POINT ( 'NONE',  ( 21.09922568453594849, 51.20696800326375353, 6.408140936763242479 ) ) ;
#3697 = CARTESIAN_POINT ( 'NONE',  ( -2.816281873526473856, 4.123634669930420493, 9.499525473075851096E-16 ) ) ;
#3698 = ORIENTED_EDGE ( 'NONE', *, *, #74061, .F. ) ;
#3699 =( GEOMETRIC_REPRESENTATION_CONTEXT ( 3 ) GLOBAL_UNCERTAINTY_ASSIGNED_CONTEXT ( ( #59462 ) ) GLOBAL_UNIT_ASSIGNED_CONTEXT ( ( #69104, #98138, #6134 ) ) REPRESENTATION_CONTEXT ( 'NONE', 'WORKASPACE' ) );
#3700 = CARTESIAN_POINT ( 'NONE',  ( 20.00000000000000355, 70.00000000000000000, 4.500000000000000888 ) ) ;
#3701 = CARTESIAN_POINT ( 'NONE',  ( 5.510795456469524289, -25.29786701974074603, 2.750000000000000000 ) ) ;
#3702 = CARTESIAN_POINT ( 'NONE',  ( 10.00000000000000178, 68.05374883491397497, 14.16423886937410082 ) ) ;
#3703 = CARTESIAN_POINT ( 'NONE',  ( 4.559911319644449179, 62.23035201082150536, -9.422509992056141925 ) ) ;
#3704 = CARTESIAN_POINT ( 'NONE',  ( -4.164238869374099927, 17.01208216824730357, 3.795296366450308767 ) ) ;
#3705 = CARTESIAN_POINT ( 'NONE',  ( 2.791683348922240793, 1.633931151000784565, 7.208316651077764092 ) ) ;
#3706 = CARTESIAN_POINT ( 'NONE',  ( 19.84674366389459266, 48.30059781766745175, 2.638427012816836559 ) ) ;
#3707 = CARTESIAN_POINT ( 'NONE',  ( 2.035157376598824452, 28.68868534415484106, 7.964842623401179544 ) ) ;
#3708 = CIRCLE ( 'NONE', #14922, 15.00000000000000000 ) ;
#3709 = CARTESIAN_POINT ( 'NONE',  ( 0.000000000000000000, 15.00000000000000000, 0.000000000000000000 ) ) ;
#3710 = CARTESIAN_POINT ( 'NONE',  ( 7.361572987183169658, 64.96726448433412315, -9.846743663894592657 ) ) ;
#3711 = ORIENTED_EDGE ( 'NONE', *, *, #553, .F. ) ;
#3712 = PLANE ( 'NONE',  #75430 ) ;
#3713 = VERTEX_POINT ( 'NONE', #9103 ) ;
#3714 = ORIENTED_EDGE ( 'NONE', *, *, #98402, .F. ) ;
#3715 = CARTESIAN_POINT ( 'NONE',  ( -5.302565485995475392, 0.000000000000000000, -1.273033341818904818 ) ) ;
#3716 = CARTESIAN_POINT ( 'NONE',  ( -4.164238869374098151, 6.595415501580634832, -3.795296366450310543 ) ) ;
#3717 = CARTESIAN_POINT ( 'NONE',  ( 20.36894250292379738, 4.928748834913967869, -10.36894250292379027 ) ) ;
#3718 = CARTESIAN_POINT ( 'NONE',  ( -2.266590686148945544, 57.22041550158063217, 7.082119434687048631 ) ) ;
#3719 = CARTESIAN_POINT ( 'NONE',  ( 18.52753015748617571, 63.09226448433412315, 4.923371831947298993 ) ) ;
#3720 = CARTESIAN_POINT ( 'NONE',  ( 1.472469842513823179, 40.59226448433411605, -4.923371831947296329 ) ) ;
#3721 =( NAMED_UNIT ( * ) SI_UNIT ( $, .STERADIAN. ) SOLID_ANGLE_UNIT ( ) );
#3723 = CARTESIAN_POINT ( 'NONE',  ( 2.791683348922240793, 56.63393115100078035, 7.208316651077764092 ) ) ;
#3722 = CARTESIAN_POINT ( 'NONE',  ( -0.8801773607111009756, 33.06368534415484106, 1.068504757029289695E-15 ) ) ;
#3724 =( NAMED_UNIT ( * ) PLANE_ANGLE_UNIT ( ) SI_UNIT ( $, .RADIAN. ) );
#3725 = CARTESIAN_POINT ( 'NONE',  ( 22.26659068614894466, 53.88708216824731068, 7.082119434687054849 ) ) ;
#3726 = CARTESIAN_POINT ( 'NONE',  ( 20.88017736071110519, 5.563685344154838397, 2.639326808657452039E-16 ) ) ;
#3727 = FACE_OUTER_BOUND ( 'NONE', #57692, .T. ) ;
#3728 = DIRECTION ( 'NONE',  ( 0.000000000000000000, 0.000000000000000000, 1.000000000000000000 ) ) ;
#3729 = CARTESIAN_POINT ( 'NONE',  ( 7.084665262690076126, 67.02201867748817676, -10.88017736071110164 ) ) ;
#3730 = CARTESIAN_POINT ( 'NONE',  ( 17.20831665107776587, 34.13393115100078745, -7.208316651077762316 ) ) ;
#3731 = CARTESIAN_POINT ( 'NONE',  ( -3.469446951953614189E-15, -40.24106884899921255, -9.846743663894594434 ) ) ;
#3732 = VERTEX_POINT ( 'NONE', #2620 ) ;
#3733 = CYLINDRICAL_SURFACE ( 'NONE', #61901, 0.5000000000000004441 ) ;
#3734 =( BOUNDED_SURFACE ( )  B_SPLINE_SURFACE ( 1, 2, ( 
 ( #38910, #97953, #69397, #919, #92385, #21944, #82921, #6930, #37438, #60411, #67929, #22434, #33344, #2404, #40876, #39403, #86373, #24896, #87345, #79357, #71382, #62368, #70886, #78864, #2894, #55874, #56846, #48848, #18860, #94352, #70390, #10864, #63838, #17875, #56369, #16896, #41385, #40389, #32862, #86861, #69896, #77374, #47862, #18367, #63360, #62872, #64333, #93863, #71852, #3362, #1416, #26345, #32367, #9381, #33826, #94844, #25391, #8887, #55381, #93369, #31869, #92872, #77871, #24404, #78368, #54872, #85382, #47373, #39886, #85881, #1909, #17394, #9887, #57822, #80831, #73319, #66306, #27818, #34825, #19344, #49341, #19828, #74295, #4842, #88331, #81321, #35318, #43314, #96345, #28802, #41865, #50316, #89318, #95841, #12331, #42344, #5822, #20332, #42835, #3861, #49827, #80339, #36315, #34322, #65813, #66809, #96843, #57330, #26836, #58303, #88820, #28317, #87826, #50828, #12815, #73808, #65315, #11837, #51315, #5341, #81798, #97331, #59302, #35819, #58809, #89799, #20825, #72821, #13315, #4359, #64820, #95337, #27326, #43802, #79840, #11345, #72328, #60781, #91784, #75295, #60297, #37319, #46285, #52304, #90789, #21822, #52788, #810, #90284, #45295, #22316, #61275, #74801, #67811, #15314, #59792, #91283, #51809, #45798, #326, #15799, #82797, #98327, #76773, #23307, #6807, #22805, #75789, #29297, #29786, #38787, #31264, #37811, #53284, #84300, #8289, #83793, #30770, #13817, #44299, #76289, #69288, #7803, #61762, #21318, #38302, #82296, #6309, #36814, #67307, #97833, #24775, #9765, #3248, #70274, #71739, #55760, #40753, #24284, #18251, #55251, #17277, #33235, #46765, #39288, #62749, #63728, #85766, #77753, #79234, #48730, #10747, #41265, #69779, #1791, #32246, #93251, #81202, #12703, #80713, #81681, #11720, #19225, #72218, #64699, #80214, #73197, #65198, #4234, #96220, #50710, #73685, #5221, #85032, #84545, #87969, #95731, #20218, #44933, #74946, #44444, #30422, #75441, #43944, #59935, #22955, #66453, #83928, #6448, #14961, #90425, #67454, #15457, #7456, #96989, #6953, #81950, #52445, #21966, #36958, #97975, #74442, #60432, #22454, #5969, #82945, #28466, #52928, #53421, #37461, #90925, #58963, #67948, #13462, #29431, #82445, #14460, #36463, #59444, #37954, #66958, #97476, #45430, #83440, #13969, #98472, #28941, #45938, #29926, #75933, #5487, #68447, #89459, #98968, #51960, #60922, #35957, #91428, #89945, #20977, #21463, #51460, #8424, #32387, #1438, #39907, #38439, #85404, #23933, #17896, #78387, #1929, #61412, #31890, #77892, #62892, #54889, #55897, #47885, #76427, #93391, #69419, #9908, #47391, #9405 ),
 ( #2425, #24916, #15930, #62387, #93885, #68936, #7943, #77393, #85902, #92894, #39423, #466, #70905, #30914, #55401, #53923, #24426, #17416, #8907, #32882, #46421, #63381, #25413, #76913, #91921, #23446, #84433, #38931, #940, #31402, #61903, #92409, #54402, #84913, #16425, #46901, #41406, #3383, #73340, #64356, #94865, #88353, #50342, #56865, #41889, #4867, #27840, #35344, #58328, #88845, #48379, #2914, #78882, #10393, #33364, #68325, #97852, #89338, #29808, #43824, #20848, #51339, #75316, #44322, #82817, #81342, #29316, #66831, #30299, #22336, #14337, #5363, #13840, #21843, #44810, #59812, #98845, #90808, #60801, #37342, #13340, #52810, #90307, #52324, #67832, #58831, #83317, #82320, #74823, #6828, #12838, #20353, #89824, #98350, #6327, #5846, #7333, #36839, #60317, #14842, #43338, #50849, #74319, #81823, #45314, #75811, #67327, #37834, #97353, #36337, #73834, #35842, #28822, #66329, #21342, #96865, #28341, #59322, #51833, #53304, #70791, #92295, #1811, #46788, #54282, #2308, #93274, #83812, #62272, #68816, #39309, #77281, #23819, #84797, #61296, #47273, #9287, #30796, #8792, #15338, #39796, #40283, #24309, #77774, #45821, #54774, #349, #16306, #69305, #69802, #91805, #46307, #24797, #23327, #53808, #32266, #70296, #827, #1325, #84318, #32763, #31777, #85290, #91301, #92778, #76308, #16797, #38812, #47772, #22828, #62775, #15819, #55274, #76793, #8309, #31287, #85785, #17297, #78270, #7826, #9784, #61785, #38322, #65217, #26739, #48259, #56749, #64721, #57234, #41766, #42738, #34726, #4747, #80235, #56273, #95744, #34224, #72237, #11743, #2800, #27228, #26253, #87242, #87732, #25293, #73219, #33732, #3770, #18768, #48750, #50220, #49250, #42251, #57723, #55780, #12229, #18271, #94251, #72721, #4255, #79750, #80734, #10769, #79258, #88226, #19735, #63746, #11248, #64233, #63258, #93767, #33255, #86275, #78772, #86768, #25779, #41284, #17784, #95231, #19244, #94750, #3268, #10278, #49728, #71758, #40778, #71278, #89221, #35723, #66211, #90197, #59204, #97739, #96243, #44201, #81705, #45201, #37228, #29201, #20231, #28713, #36725, #59700, #13717, #14725, #6710, #75700, #52209, #28218, #67715, #6221, #74711, #82703, #73712, #98228, #97244, #89707, #21727, #27723, #35217, #5733, #67216, #21221, #20730, #22222, #51725, #44701, #29689, #58203, #83203, #51221, #13219, #75200, #60198, #82207, #52698, #43715, #74199, #90693, #88720, #36219, #81224, #66719, #12723, #43218, #5245, #85173, #91187, #229, #38212, #45696, #70176, #718, #46672, #76679, #46196, #32148, #77170, #76196, #61663, #24678, #68214, #85663, #8199, #16683 ) ),
 .UNSPECIFIED., .F., .F., .T. ) 
 B_SPLINE_SURFACE_WITH_KNOTS ( ( 2, 2 ),
 ( 3, 2, 2, 2, 2, 2, 2, 2, 2, 2, 2, 2, 2, 2, 2, 2, 2, 2, 2, 2, 2, 2, 2, 2, 2, 2, 2, 2, 2, 2, 2, 2, 2, 2, 2, 2, 2, 2, 2, 2, 2, 2, 2, 2, 2, 2, 2, 2, 2, 2, 2, 2, 2, 2, 2, 2, 2, 2, 2, 2, 2, 2, 2, 2, 2, 2, 2, 2, 2, 2, 2, 2, 2, 2, 2, 2, 2, 2, 2, 2, 2, 2, 2, 2, 2, 2, 2, 2, 2, 2, 2, 2, 2, 2, 2, 2, 2, 2, 2, 2, 2, 2, 2, 2, 2, 2, 2, 2, 2, 2, 2, 2, 2, 2, 2, 2, 2, 2, 2, 2, 2, 2, 2, 2, 2, 2, 2, 2, 2, 2, 2, 2, 2, 2, 2, 2, 2, 2, 2, 2, 2, 2, 2, 2, 2, 2, 2, 2, 2, 2, 2, 2, 2, 2, 2, 2, 2, 2, 2, 2, 2, 2, 3 ),
 ( 0.000000000000000000, 1.000000000000000000 ),
 ( 0.000000000000000000, 0.005952380952380952051, 0.01190476190476190410, 0.01785714285714285615, 0.02380952380952380820, 0.02976190476190476025, 0.03571428571428571230, 0.04166666666666666435, 0.04761904761904761640, 0.05357142857142856845, 0.05952380952380952051, 0.06547619047619047949, 0.07142857142857142461, 0.07738095238095238360, 0.08333333333333332871, 0.08928571428571428770, 0.09523809523809523281, 0.1011904761904761918, 0.1071428571428571369, 0.1130952380952380959, 0.1190476190476190410, 0.1250000000000000000, 0.1309523809523809590, 0.1369047619047619180, 0.1428571428571428492, 0.1488095238095238082, 0.1547619047619047672, 0.1607142857142857262, 0.1666666666666666574, 0.1726190476190476164, 0.1785714285714285754, 0.1845238095238095344, 0.1904761904761904656, 0.1964285714285714246, 0.2023809523809523836, 0.2083333333333333426, 0.2142857142857142738, 0.2202380952380952328, 0.2261904761904761918, 0.2321428571428571508, 0.2380952380952380820, 0.2440476190476190410, 0.2500000000000000000, 0.2559523809523809312, 0.2619047619047619180, 0.2678571428571428492, 0.2738095238095238360, 0.2797619047619047672, 0.2857142857142856984, 0.2916666666666666852, 0.2976190476190476164, 0.3035714285714285476, 0.3095238095238095344, 0.3154761904761904656, 0.3214285714285714524, 0.3273809523809523836, 0.3333333333333333148, 0.3392857142857143016, 0.3452380952380952328, 0.3511904761904761640, 0.3571428571428571508, 0.3630952380952380820, 0.3690476190476190688, 0.3750000000000000000, 0.3809523809523809312, 0.3869047619047619180, 0.3928571428571428492, 0.3988095238095238360, 0.4047619047619047672, 0.4107142857142856984, 0.4166666666666666852, 0.4226190476190476164, 0.4285714285714285476, 0.4345238095238095344, 0.4404761904761904656, 0.4464285714285714524, 0.4523809523809523836, 0.4583333333333333148, 0.4642857142857143016, 0.4702380952380952328, 0.4761904761904761640, 0.4821428571428571508, 0.4880952380952380820, 0.4940476190476190688, 0.5000000000000000000, 0.5059523809523809312, 0.5119047619047618625, 0.5178571428571429047, 0.5238095238095238360, 0.5297619047619047672, 0.5357142857142856984, 0.5416666666666666297, 0.5476190476190476719, 0.5535714285714286031, 0.5595238095238095344, 0.5654761904761904656, 0.5714285714285713969, 0.5773809523809523281, 0.5833333333333333703, 0.5892857142857143016, 0.5952380952380952328, 0.6011904761904761640, 0.6071428571428570953, 0.6130952380952381375, 0.6190476190476190688, 0.6250000000000000000, 0.6309523809523809312, 0.6369047619047618625, 0.6428571428571429047, 0.6488095238095238360, 0.6547619047619047672, 0.6607142857142856984, 0.6666666666666666297, 0.6726190476190476719, 0.6785714285714286031, 0.6845238095238095344, 0.6904761904761904656, 0.6964285714285713969, 0.7023809523809523281, 0.7083333333333333703, 0.7142857142857143016, 0.7202380952380952328, 0.7261904761904761640, 0.7321428571428570953, 0.7380952380952381375, 0.7440476190476190688, 0.7500000000000000000, 0.7559523809523809312, 0.7619047619047618625, 0.7678571428571429047, 0.7738095238095238360, 0.7797619047619047672, 0.7857142857142856984, 0.7916666666666666297, 0.7976190476190476719, 0.8035714285714286031, 0.8095238095238095344, 0.8154761904761904656, 0.8214285714285713969, 0.8273809523809523281, 0.8333333333333333703, 0.8392857142857143016, 0.8452380952380952328, 0.8511904761904761640, 0.8571428571428570953, 0.8630952380952381375, 0.8690476190476190688, 0.8750000000000000000, 0.8809523809523809312, 0.8869047619047618625, 0.8928571428571429047, 0.8988095238095238360, 0.9047619047619047672, 0.9107142857142856984, 0.9166666666666666297, 0.9226190476190476719, 0.9285714285714286031, 0.9345238095238095344, 0.9404761904761904656, 0.9464285714285713969, 0.9523809523809523281, 0.9583333333333333703, 0.9642857142857143016 ),
 .UNSPECIFIED. ) 
 GEOMETRIC_REPRESENTATION_ITEM ( )  RATIONAL_B_SPLINE_SURFACE ( (
 ( 1.000000000000000000, 0.9659258262890683122, 1.000000000000000000, 0.9659258262890683122, 1.000000000000000000, 0.9659258262890683122, 1.000000000000000000, 0.9659258262890683122, 1.000000000000000000, 0.9659258262890683122, 1.000000000000000000, 0.9659258262890683122, 1.000000000000000000, 0.9659258262890683122, 1.000000000000000000, 0.9659258262890683122, 1.000000000000000000, 0.9659258262890683122, 1.000000000000000000, 0.9659258262890683122, 1.000000000000000000, 0.9659258262890683122, 1.000000000000000000, 0.9659258262890683122, 1.000000000000000000, 0.9659258262890683122, 1.000000000000000000, 0.9659258262890683122, 1.000000000000000000, 0.9659258262890683122, 1.000000000000000000, 0.9659258262890683122, 1.000000000000000000, 0.9659258262890683122, 1.000000000000000000, 0.9659258262890683122, 1.000000000000000000, 0.9659258262890683122, 1.000000000000000000, 0.9659258262890683122, 1.000000000000000000, 0.9659258262890683122, 1.000000000000000000, 0.9659258262890683122, 1.000000000000000000, 0.9659258262890683122, 1.000000000000000000, 0.9659258262890683122, 1.000000000000000000, 0.9659258262890683122, 1.000000000000000000, 0.9659258262890683122, 1.000000000000000000, 0.9659258262890683122, 1.000000000000000000, 0.9659258262890683122, 1.000000000000000000, 0.9659258262890683122, 1.000000000000000000, 0.9659258262890683122, 1.000000000000000000, 0.9659258262890683122, 1.000000000000000000, 0.9659258262890683122, 1.000000000000000000, 0.9659258262890683122, 1.000000000000000000, 0.9659258262890683122, 1.000000000000000000, 0.9659258262890683122, 1.000000000000000000, 0.9659258262890683122, 1.000000000000000000, 0.9659258262890683122, 1.000000000000000000, 0.9659258262890683122, 1.000000000000000000, 0.9659258262890683122, 1.000000000000000000, 0.9659258262890683122, 1.000000000000000000, 0.9659258262890683122, 1.000000000000000000, 0.9659258262890683122, 1.000000000000000000, 0.9659258262890683122, 1.000000000000000000, 0.9659258262890683122, 1.000000000000000000, 0.9659258262890683122, 1.000000000000000000, 0.9659258262890683122, 1.000000000000000000, 0.9659258262890683122, 1.000000000000000000, 0.9659258262890683122, 1.000000000000000000, 0.9659258262890683122, 1.000000000000000000, 0.9659258262890683122, 1.000000000000000000, 0.9659258262890683122, 1.000000000000000000, 0.9659258262890683122, 1.000000000000000000, 0.9659258262890683122, 1.000000000000000000, 0.9659258262890683122, 1.000000000000000000, 0.9659258262890683122, 1.000000000000000000, 0.9659258262890683122, 1.000000000000000000, 0.9659258262890683122, 1.000000000000000000, 0.9659258262890683122, 1.000000000000000000, 0.9659258262890683122, 1.000000000000000000, 0.9659258262890683122, 1.000000000000000000, 0.9659258262890683122, 1.000000000000000000, 0.9659258262890683122, 1.000000000000000000, 0.9659258262890683122, 1.000000000000000000, 0.9659258262890683122, 1.000000000000000000, 0.9659258262890683122, 1.000000000000000000, 0.9659258262890683122, 1.000000000000000000, 0.9659258262890683122, 1.000000000000000000, 0.9659258262890683122, 1.000000000000000000, 0.9659258262890683122, 1.000000000000000000, 0.9659258262890683122, 1.000000000000000000, 0.9659258262890683122, 1.000000000000000000, 0.9659258262890683122, 1.000000000000000000, 0.9659258262890683122, 1.000000000000000000, 0.9659258262890683122, 1.000000000000000000, 0.9659258262890683122, 1.000000000000000000, 0.9659258262890683122, 1.000000000000000000, 0.9659258262890683122, 1.000000000000000000, 0.9659258262890683122, 1.000000000000000000, 0.9659258262890683122, 1.000000000000000000, 0.9659258262890683122, 1.000000000000000000, 0.9659258262890683122, 1.000000000000000000, 0.9659258262890683122, 1.000000000000000000, 0.9659258262890683122, 1.000000000000000000, 0.9659258262890683122, 1.000000000000000000, 0.9659258262890683122, 1.000000000000000000, 0.9659258262890683122, 1.000000000000000000, 0.9659258262890683122, 1.000000000000000000, 0.9659258262890683122, 1.000000000000000000, 0.9659258262890683122, 1.000000000000000000, 0.9659258262890683122, 1.000000000000000000, 0.9659258262890683122, 1.000000000000000000, 0.9659258262890683122, 1.000000000000000000, 0.9659258262890683122, 1.000000000000000000, 0.9659258262890683122, 1.000000000000000000, 0.9659258262890683122, 1.000000000000000000, 0.9659258262890683122, 1.000000000000000000, 0.9659258262890683122, 1.000000000000000000, 0.9659258262890683122, 1.000000000000000000, 0.9659258262890683122, 1.000000000000000000, 0.9659258262890683122, 1.000000000000000000, 0.9659258262890683122, 1.000000000000000000, 0.9659258262890683122, 1.000000000000000000, 0.9659258262890683122, 1.000000000000000000, 0.9659258262890683122, 1.000000000000000000, 0.9659258262890683122, 1.000000000000000000, 0.9659258262890683122, 1.000000000000000000, 0.9659258262890683122, 1.000000000000000000, 0.9659258262890683122, 1.000000000000000000, 0.9659258262890683122, 1.000000000000000000, 0.9659258262890683122, 1.000000000000000000, 0.9659258262890683122, 1.000000000000000000, 0.9659258262890683122, 1.000000000000000000, 0.9659258262890683122, 1.000000000000000000, 0.9659258262890683122, 1.000000000000000000, 0.9659258262890683122, 1.000000000000000000, 0.9659258262890683122, 1.000000000000000000, 0.9659258262890683122, 1.000000000000000000, 0.9659258262890683122, 1.000000000000000000, 0.9659258262890683122, 1.000000000000000000, 0.9659258262890683122, 1.000000000000000000, 0.9659258262890683122, 1.000000000000000000, 0.9659258262890683122, 1.000000000000000000, 0.9659258262890683122, 1.000000000000000000, 0.9659258262890683122, 1.000000000000000000, 0.9659258262890683122, 1.000000000000000000, 0.9659258262890683122, 1.000000000000000000, 0.9659258262890683122, 1.000000000000000000, 0.9659258262890683122, 1.000000000000000000, 0.9659258262890683122, 1.000000000000000000, 0.9659258262890683122, 1.000000000000000000, 0.9659258262890683122, 1.000000000000000000, 0.9659258262890683122, 1.000000000000000000, 0.9659258262890683122, 1.000000000000000000, 0.9659258262890683122, 1.000000000000000000, 0.9659258262890683122, 1.000000000000000000, 0.9659258262890683122, 1.000000000000000000, 0.9659258262890683122, 1.000000000000000000, 0.9659258262890683122, 1.000000000000000000, 0.9659258262890683122, 1.000000000000000000, 0.9659258262890683122, 1.000000000000000000, 0.9659258262890683122, 1.000000000000000000, 0.9659258262890683122, 1.000000000000000000, 0.9659258262890683122, 1.000000000000000000, 0.9659258262890683122, 1.000000000000000000, 0.9659258262890683122, 1.000000000000000000, 0.9659258262890683122, 1.000000000000000000, 0.9659258262890683122, 1.000000000000000000, 0.9659258262890683122, 1.000000000000000000, 0.9659258262890683122, 1.000000000000000000, 0.9659258262890683122, 1.000000000000000000, 0.9659258262890683122, 1.000000000000000000, 0.9659258262890683122, 1.000000000000000000, 0.9659258262890683122, 1.000000000000000000, 0.9659258262890683122, 1.000000000000000000, 0.9659258262890683122, 1.000000000000000000, 0.9659258262890683122, 1.000000000000000000, 0.9659258262890683122, 1.000000000000000000, 0.9659258262890683122, 1.000000000000000000, 0.9659258262890683122, 1.000000000000000000, 0.9659258262890683122, 1.000000000000000000, 0.9659258262890683122, 1.000000000000000000, 0.9659258262890683122, 1.000000000000000000),
 ( 1.000000000000000000, 0.9659258262890683122, 1.000000000000000000, 0.9659258262890683122, 1.000000000000000000, 0.9659258262890683122, 1.000000000000000000, 0.9659258262890683122, 1.000000000000000000, 0.9659258262890683122, 1.000000000000000000, 0.9659258262890683122, 1.000000000000000000, 0.9659258262890683122, 1.000000000000000000, 0.9659258262890683122, 1.000000000000000000, 0.9659258262890683122, 1.000000000000000000, 0.9659258262890683122, 1.000000000000000000, 0.9659258262890683122, 1.000000000000000000, 0.9659258262890683122, 1.000000000000000000, 0.9659258262890683122, 1.000000000000000000, 0.9659258262890683122, 1.000000000000000000, 0.9659258262890683122, 1.000000000000000000, 0.9659258262890683122, 1.000000000000000000, 0.9659258262890683122, 1.000000000000000000, 0.9659258262890683122, 1.000000000000000000, 0.9659258262890683122, 1.000000000000000000, 0.9659258262890683122, 1.000000000000000000, 0.9659258262890683122, 1.000000000000000000, 0.9659258262890683122, 1.000000000000000000, 0.9659258262890683122, 1.000000000000000000, 0.9659258262890683122, 1.000000000000000000, 0.9659258262890683122, 1.000000000000000000, 0.9659258262890683122, 1.000000000000000000, 0.9659258262890683122, 1.000000000000000000, 0.9659258262890683122, 1.000000000000000000, 0.9659258262890683122, 1.000000000000000000, 0.9659258262890683122, 1.000000000000000000, 0.9659258262890683122, 1.000000000000000000, 0.9659258262890683122, 1.000000000000000000, 0.9659258262890683122, 1.000000000000000000, 0.9659258262890683122, 1.000000000000000000, 0.9659258262890683122, 1.000000000000000000, 0.9659258262890683122, 1.000000000000000000, 0.9659258262890683122, 1.000000000000000000, 0.9659258262890683122, 1.000000000000000000, 0.9659258262890683122, 1.000000000000000000, 0.9659258262890683122, 1.000000000000000000, 0.9659258262890683122, 1.000000000000000000, 0.9659258262890683122, 1.000000000000000000, 0.9659258262890683122, 1.000000000000000000, 0.9659258262890683122, 1.000000000000000000, 0.9659258262890683122, 1.000000000000000000, 0.9659258262890683122, 1.000000000000000000, 0.9659258262890683122, 1.000000000000000000, 0.9659258262890683122, 1.000000000000000000, 0.9659258262890683122, 1.000000000000000000, 0.9659258262890683122, 1.000000000000000000, 0.9659258262890683122, 1.000000000000000000, 0.9659258262890683122, 1.000000000000000000, 0.9659258262890683122, 1.000000000000000000, 0.9659258262890683122, 1.000000000000000000, 0.9659258262890683122, 1.000000000000000000, 0.9659258262890683122, 1.000000000000000000, 0.9659258262890683122, 1.000000000000000000, 0.9659258262890683122, 1.000000000000000000, 0.9659258262890683122, 1.000000000000000000, 0.9659258262890683122, 1.000000000000000000, 0.9659258262890683122, 1.000000000000000000, 0.9659258262890683122, 1.000000000000000000, 0.9659258262890683122, 1.000000000000000000, 0.9659258262890683122, 1.000000000000000000, 0.9659258262890683122, 1.000000000000000000, 0.9659258262890683122, 1.000000000000000000, 0.9659258262890683122, 1.000000000000000000, 0.9659258262890683122, 1.000000000000000000, 0.9659258262890683122, 1.000000000000000000, 0.9659258262890683122, 1.000000000000000000, 0.9659258262890683122, 1.000000000000000000, 0.9659258262890683122, 1.000000000000000000, 0.9659258262890683122, 1.000000000000000000, 0.9659258262890683122, 1.000000000000000000, 0.9659258262890683122, 1.000000000000000000, 0.9659258262890683122, 1.000000000000000000, 0.9659258262890683122, 1.000000000000000000, 0.9659258262890683122, 1.000000000000000000, 0.9659258262890683122, 1.000000000000000000, 0.9659258262890683122, 1.000000000000000000, 0.9659258262890683122, 1.000000000000000000, 0.9659258262890683122, 1.000000000000000000, 0.9659258262890683122, 1.000000000000000000, 0.9659258262890683122, 1.000000000000000000, 0.9659258262890683122, 1.000000000000000000, 0.9659258262890683122, 1.000000000000000000, 0.9659258262890683122, 1.000000000000000000, 0.9659258262890683122, 1.000000000000000000, 0.9659258262890683122, 1.000000000000000000, 0.9659258262890683122, 1.000000000000000000, 0.9659258262890683122, 1.000000000000000000, 0.9659258262890683122, 1.000000000000000000, 0.9659258262890683122, 1.000000000000000000, 0.9659258262890683122, 1.000000000000000000, 0.9659258262890683122, 1.000000000000000000, 0.9659258262890683122, 1.000000000000000000, 0.9659258262890683122, 1.000000000000000000, 0.9659258262890683122, 1.000000000000000000, 0.9659258262890683122, 1.000000000000000000, 0.9659258262890683122, 1.000000000000000000, 0.9659258262890683122, 1.000000000000000000, 0.9659258262890683122, 1.000000000000000000, 0.9659258262890683122, 1.000000000000000000, 0.9659258262890683122, 1.000000000000000000, 0.9659258262890683122, 1.000000000000000000, 0.9659258262890683122, 1.000000000000000000, 0.9659258262890683122, 1.000000000000000000, 0.9659258262890683122, 1.000000000000000000, 0.9659258262890683122, 1.000000000000000000, 0.9659258262890683122, 1.000000000000000000, 0.9659258262890683122, 1.000000000000000000, 0.9659258262890683122, 1.000000000000000000, 0.9659258262890683122, 1.000000000000000000, 0.9659258262890683122, 1.000000000000000000, 0.9659258262890683122, 1.000000000000000000, 0.9659258262890683122, 1.000000000000000000, 0.9659258262890683122, 1.000000000000000000, 0.9659258262890683122, 1.000000000000000000, 0.9659258262890683122, 1.000000000000000000, 0.9659258262890683122, 1.000000000000000000, 0.9659258262890683122, 1.000000000000000000, 0.9659258262890683122, 1.000000000000000000, 0.9659258262890683122, 1.000000000000000000, 0.9659258262890683122, 1.000000000000000000, 0.9659258262890683122, 1.000000000000000000, 0.9659258262890683122, 1.000000000000000000, 0.9659258262890683122, 1.000000000000000000, 0.9659258262890683122, 1.000000000000000000, 0.9659258262890683122, 1.000000000000000000, 0.9659258262890683122, 1.000000000000000000, 0.9659258262890683122, 1.000000000000000000, 0.9659258262890683122, 1.000000000000000000, 0.9659258262890683122, 1.000000000000000000, 0.9659258262890683122, 1.000000000000000000, 0.9659258262890683122, 1.000000000000000000, 0.9659258262890683122, 1.000000000000000000, 0.9659258262890683122, 1.000000000000000000, 0.9659258262890683122, 1.000000000000000000, 0.9659258262890683122, 1.000000000000000000, 0.9659258262890683122, 1.000000000000000000, 0.9659258262890683122, 1.000000000000000000, 0.9659258262890683122, 1.000000000000000000, 0.9659258262890683122, 1.000000000000000000, 0.9659258262890683122, 1.000000000000000000, 0.9659258262890683122, 1.000000000000000000, 0.9659258262890683122, 1.000000000000000000, 0.9659258262890683122, 1.000000000000000000, 0.9659258262890683122, 1.000000000000000000, 0.9659258262890683122, 1.000000000000000000, 0.9659258262890683122, 1.000000000000000000, 0.9659258262890683122, 1.000000000000000000, 0.9659258262890683122, 1.000000000000000000, 0.9659258262890683122, 1.000000000000000000, 0.9659258262890683122, 1.000000000000000000, 0.9659258262890683122, 1.000000000000000000, 0.9659258262890683122, 1.000000000000000000, 0.9659258262890683122, 1.000000000000000000, 0.9659258262890683122, 1.000000000000000000, 0.9659258262890683122, 1.000000000000000000, 0.9659258262890683122, 1.000000000000000000, 0.9659258262890683122, 1.000000000000000000, 0.9659258262890683122, 1.000000000000000000) ) ) 
 REPRESENTATION_ITEM ( '' )  SURFACE ( )  );
#3735 = ORIENTED_EDGE ( 'NONE', *, *, #87534, .F. ) ;
#3736 = CARTESIAN_POINT ( 'NONE',  ( 12.63842701281683034, 17.46726448433411250, 9.846743663894596210 ) ) ;
#3737 = ORIENTED_EDGE ( 'NONE', *, *, #98702, .T. ) ;
#3738 = CARTESIAN_POINT ( 'NONE',  ( -2.266590686148945544, 37.22041550158063217, 7.082119434687048631 ) ) ;
#3739 = CARTESIAN_POINT ( 'NONE',  ( 10.00000000000000178, 37.25893115100078745, 9.846743663894594434 ) ) ;
#3740 = CARTESIAN_POINT ( 'NONE',  ( 10.00000000000000178, 54.31368534415484106, 10.88017736071110342 ) ) ;
#3741 = EDGE_CURVE ( 'NONE', #63150, #37315, #33075, .T. ) ;
#3742 = FILL_AREA_STYLE ('',( #86247 ) ) ;
#3743 =( BOUNDED_CURVE ( )  B_SPLINE_CURVE ( 3, ( #84826, #93302, #2336, #93795 ),
 .UNSPECIFIED., .F., .T. ) 
 B_SPLINE_CURVE_WITH_KNOTS ( ( 4, 4 ),
 ( 4.712388980384682569, 6.283185307179586232 ),
 .UNSPECIFIED. ) 
 CURVE ( )  GEOMETRIC_REPRESENTATION_ITEM ( )  RATIONAL_B_SPLINE_CURVE ( ( 1.000000000000000000, 0.8047378541243632721, 0.8047378541243632721, 1.000000000000000000 ) ) 
 REPRESENTATION_ITEM ( '' )  );
#3744 = CARTESIAN_POINT ( 'NONE',  ( 10.00000000000000178, 54.31368534415484106, 10.88017736071110342 ) ) ;
#3745 = AXIS2_PLACEMENT_3D ( 'NONE', #53930, #8430, #947 ) ;
#3746 = CARTESIAN_POINT ( 'NONE',  ( 0.1532563361054082862, 46.21726448433411605, 2.638427012816831674 ) ) ;
#3747 = CARTESIAN_POINT ( 'NONE',  ( -11.09922568453594316, 14.54030133659709634, 6.408140936763246920 ) ) ;
#3748 = ORIENTED_EDGE ( 'NONE', *, *, #55444, .F. ) ;
#3749 = CARTESIAN_POINT ( 'NONE',  ( -2.266590686148945544, 26.38708216824730357, -7.082119434687050408 ) ) ;
#3750 = EDGE_LOOP ( 'NONE', ( #53698, #7579, #8790, #57197, #21652, #23651 ) ) ;
#3751 = EDGE_LOOP ( 'NONE', ( #70168, #28982, #43924, #31444, #82295, #45389 ) ) ;
#3752 = CARTESIAN_POINT ( 'NONE',  ( 0.6178305044545838731, 29.74863466993042138, 9.382169495545420901 ) ) ;
#3753 = CARTESIAN_POINT ( 'NONE',  ( 19.84674366389459266, 18.71726448433411960, -2.638427012816827677 ) ) ;
#3754 = SURFACE_SIDE_STYLE ('',( #78759 ) ) ;
#3755 = CARTESIAN_POINT ( 'NONE',  ( -1.099225684535947600, 53.70696800326376064, -6.408140936763238038 ) ) ;
#3756 = FACE_OUTER_BOUND ( 'NONE', #55982, .T. ) ;
#3757 = CARTESIAN_POINT ( 'NONE',  ( 19.84674366389459266, 33.30059781766744464, 2.638427012816836559 ) ) ;
#3758 = CARTESIAN_POINT ( 'NONE',  ( 10.09777502097877289, 0.04922511925147150802, 10.75551206493387824 ) ) ;
#3759 = EDGE_CURVE ( 'NONE', #72785, #16271, #76612, .T. ) ;
#3760 = TOROIDAL_SURFACE ( 'NONE', #30867, 14.49999999999999822, 0.5000000000000000000 ) ;
#3761 = CARTESIAN_POINT ( 'NONE',  ( -0.8801773607111009756, 68.06368534415484817, 1.068504757029289695E-15 ) ) ;
#3762 = CARTESIAN_POINT ( 'NONE',  ( 17.39651004071838969, 39.08210964143329846, -6.500000000000027534 ) ) ;
#3763 = CARTESIAN_POINT ( 'NONE',  ( 1.915564264621439472, 15.00000000000000000, -14.37291249357988043 ) ) ;
#3764 = CARTESIAN_POINT ( 'NONE',  ( 19.84674366389459621, 3.508931151000785231, 7.409399052514197653E-17 ) ) ;
#3765 = AXIS2_PLACEMENT_3D ( 'NONE', #39904, #85900, #55400 ) ;
#3766 = EDGE_CURVE ( 'NONE', #44163, #68545, #38622, .T. ) ;
#3767 = CARTESIAN_POINT ( 'NONE',  ( 3.591859063236763294, 18.29030133659708568, -11.09922568453595026 ) ) ;
#3769 = SURFACE_STYLE_USAGE ( .BOTH. , #49248 ) ;
#3768 = COLOUR_RGB ( '', 0.66274510, 0.83137255, 0.94901961) ;
#3770 = CARTESIAN_POINT ( 'NONE',  ( 17.20831665107776587, 42.88393115100077324, 7.208316651077764980 ) ) ;
#3771 = LINE ( 'NONE', #25294, #10607 ) ;
#3772 = CARTESIAN_POINT ( 'NONE',  ( 24.16423886937410614, 9.512082168247301794, -3.795296366450302550 ) ) ;
#3773 = CARTESIAN_POINT ( 'NONE',  ( 14.92337183194729988, 34.34226448433411605, -8.527530157486177487 ) ) ;
#3774 = AXIS2_PLACEMENT_3D ( 'NONE', #88231, #42743, #4260 ) ;
#3775 = CARTESIAN_POINT ( 'NONE',  ( 3.591859063236761518, 29.95696800326375708, 11.09922568453594849 ) ) ;
#3777 = FACE_OUTER_BOUND ( 'NONE', #50735, .T. ) ;
#3776 = CARTESIAN_POINT ( 'NONE',  ( 17.39651004071841456, 14.08210964143329669, -6.500000000000003553 ) ) ;
#3778 = CARTESIAN_POINT ( 'NONE',  ( 19.42250999205614548, 55.98035201082150536, -5.440088680355545492 ) ) ;
#3779 = CARTESIAN_POINT ( 'NONE',  ( 0.6178305044545818747, 8.498634669930421381, -9.382169495545419124 ) ) ;
#3780 = CARTESIAN_POINT ( 'NONE',  ( 4.838527690343520149, 14.49999999999999112, 14.19819177887736927 ) ) ;
#3781 = CARTESIAN_POINT ( 'NONE',  ( 0.1532563361054083140, 41.00893115100078745, 1.131784320476157264E-15 ) ) ;
#3782 = CARTESIAN_POINT ( 'NONE',  ( 2.035157376598822676, 22.43868534415483396, -7.964842623401177768 ) ) ;
#3783 = CARTESIAN_POINT ( 'NONE',  ( -1.099225684535947600, 28.70696800326375353, -6.408140936763238038 ) ) ;
#3784 = CARTESIAN_POINT ( 'NONE',  ( 7.361572987183170547, 17.05059781766745530, 9.846743663894590881 ) ) ;
#3785 = CARTESIAN_POINT ( 'NONE',  ( -11.88867004768947488, 90.28252147127371074, 6.948627224671861669 ) ) ;
#3786 = CARTESIAN_POINT ( 'NONE',  ( -0.8801773607111009756, 33.06368534415484106, 1.068504757029289695E-15 ) ) ;
#3787 = CARTESIAN_POINT ( 'NONE',  ( 20.88017736071110875, 65.77201867748817676, -2.915334737309920765 ) ) ;
#3788 = CARTESIAN_POINT ( 'NONE',  ( 12.91533473730993009, 6.605352010821504471, -10.88017736071109987 ) ) ;
#3790 = CARTESIAN_POINT ( 'NONE',  ( 0.5774900079438607392, 28.48035201082150891, 5.440088680355550821 ) ) ;
#3789 = CARTESIAN_POINT ( 'NONE',  ( 2.791683348922237240, 40.38393115100078035, -7.208316651077763204 ) ) ;
#3791 = CARTESIAN_POINT ( 'NONE',  ( 5.500000000000000000, 11.00000000000000000, -6.500000000000000888 ) ) ;
#3792 = CARTESIAN_POINT ( 'NONE',  ( 19.42250999205614548, 40.98035201082150536, -5.440088680355545492 ) ) ;
#3793 = CARTESIAN_POINT ( 'NONE',  ( 10.00000000000000000, 6.813685344154838397, -10.88017736071110342 ) ) ;
#3794 = FACE_OUTER_BOUND ( 'NONE', #19494, .T. ) ;
#3795 = PRESENTATION_STYLE_ASSIGNMENT (( #72749 ) ) ;
#3796 = CARTESIAN_POINT ( 'NONE',  ( 18.52753015748617571, 58.09226448433411605, 4.923371831947298993 ) ) ;
#3797 = CARTESIAN_POINT ( 'NONE',  ( 20.36894250292379382, 48.67874883491396076, 10.36894250292379205 ) ) ;
#3798 = FACE_OUTER_BOUND ( 'NONE', #59290, .T. ) ;
#3799 = ADVANCED_FACE ( 'NONE', ( #72541 ), #9510, .T. ) ;
#3800 = CARTESIAN_POINT ( 'NONE',  ( -12.60589901313216998, 14.49999999999999112, -8.129656208642240145 ) ) ;
#3801 = CARTESIAN_POINT ( 'NONE',  ( 20.36894250292379738, 39.92874883491396787, -10.36894250292379027 ) ) ;
#3802 = LINE ( 'NONE', #34257, #37806 ) ;
#3803 = VERTEX_POINT ( 'NONE', #41595 ) ;
#3804 = CARTESIAN_POINT ( 'NONE',  ( 24.16423886937409904, 64.09541550158064638, 3.795296366450317205 ) ) ;
#3805 = CARTESIAN_POINT ( 'NONE',  ( 0.1532563361054083140, 36.00893115100078745, 1.131784320476157264E-15 ) ) ;
#3807 = FACE_OUTER_BOUND ( 'NONE', #24358, .T. ) ;
#3806 =( NAMED_UNIT ( * ) SI_UNIT ( $, .STERADIAN. ) SOLID_ANGLE_UNIT ( ) );
#3808 = CARTESIAN_POINT ( 'NONE',  ( 2.035157376598824452, 63.68868534415484106, 7.964842623401179544 ) ) ;
#3809 = CARTESIAN_POINT ( 'NONE',  ( 16.40814093676324603, 62.45696800326376064, -11.09922568453594671 ) ) ;
#3810 = CARTESIAN_POINT ( 'NONE',  ( 15.44008868035555260, 34.73035201082151247, 9.422509992056143702 ) ) ;
#3811 = CARTESIAN_POINT ( 'NONE',  ( 21.09922568453594849, 56.20696800326375353, 6.408140936763242479 ) ) ;
#3812 = CARTESIAN_POINT ( 'NONE',  ( 21.09922568453595559, 17.04030133659708923, -6.408140936763230044 ) ) ;
#3813 = CARTESIAN_POINT ( 'NONE',  ( 19.84674366389459266, 13.30059781766745353, 2.638427012816836559 ) ) ;
#3814 = ORIENTED_EDGE ( 'NONE', *, *, #25409, .F. ) ;
#3815 =( NAMED_UNIT ( * ) SI_UNIT ( $, .STERADIAN. ) SOLID_ANGLE_UNIT ( ) );
#3816 =( LENGTH_UNIT ( ) NAMED_UNIT ( * ) SI_UNIT ( .MILLI., .METRE. ) );
#3817 = CARTESIAN_POINT ( 'NONE',  ( -0.8801773607111008646, 3.272018677488171434, 2.915334737309923430 ) ) ;
#3818 = CARTESIAN_POINT ( 'NONE',  ( -0.3689425029237881626, 32.42874883491395366, 10.36894250292379027 ) ) ;
#3819 = CARTESIAN_POINT ( 'NONE',  ( 4.559911319644449179, 38.89701867748817676, 9.422509992056141925 ) ) ;
#3820 = CARTESIAN_POINT ( 'NONE',  ( 12.91533473730993009, 46.60535201082150536, -10.88017736071109987 ) ) ;
#3821 = CARTESIAN_POINT ( 'NONE',  ( -2.815433093576927170, 0.5000000000000004441, -14.73340885523753663 ) ) ;
#3822 = CARTESIAN_POINT ( 'NONE',  ( -7.595945211628163385, 4.385640548506873962E-16, -12.35117874301652030 ) ) ;
#3823 = CARTESIAN_POINT ( 'NONE',  ( 17.20831665107776587, 4.133931151000785675, -7.208316651077762316 ) ) ;
#3824 = DIRECTION ( 'NONE',  ( 1.000000000000000000, -0.000000000000000000, 0.000000000000000000 ) ) ;
#3825 =( NAMED_UNIT ( * ) SI_UNIT ( $, .STERADIAN. ) SOLID_ANGLE_UNIT ( ) );
#3826 = CARTESIAN_POINT ( 'NONE',  ( -46.52481518344757205, 102.2792363782860576, 7.261093659072778372 ) ) ;
#3827 = CARTESIAN_POINT ( 'NONE',  ( 10.00000000000000000, 24.75893115100078745, -9.846743663894594434 ) ) ;
#3828 = CARTESIAN_POINT ( 'NONE',  ( 0.1532563361054082862, 56.21726448433411605, 2.638427012816831674 ) ) ;
#3829 = CARTESIAN_POINT ( 'NONE',  ( 0.5774900079438590739, 22.64701867748817321, -5.440088680355550821 ) ) ;
#3830 = CARTESIAN_POINT ( 'NONE',  ( 22.81628187352648496, 41.83196800326375353, -3.434112377981050290 ) ) ;
#3831 = AXIS2_PLACEMENT_3D ( 'NONE', #33776, #73273, #4305 ) ;
#3832 = CARTESIAN_POINT ( 'NONE',  ( 20.88017736071110875, 60.77201867748817676, -2.915334737309920765 ) ) ;
#3833 = CARTESIAN_POINT ( 'NONE',  ( 5.076628168052703671, 26.84226448433411960, 8.527530157486179263 ) ) ;
#3835 = CARTESIAN_POINT ( 'NONE',  ( 12.63842701281683034, 27.46726448433411250, 9.846743663894596210 ) ) ;
#3834 = CARTESIAN_POINT ( 'NONE',  ( 13.79529636645031943, 55.34541550158062506, -14.16423886937409904 ) ) ;
#3836 = CARTESIAN_POINT ( 'NONE',  ( 0.1129803114748860748, 44.29427333184091964, -6.480634945678686698 ) ) ;
#3837 = CARTESIAN_POINT ( 'NONE',  ( -42.60666666666667624, 92.50000000000000000, -9.500000000000000000 ) ) ;
#3838 = CARTESIAN_POINT ( 'NONE',  ( 2.917880565312950480, 5.970415501580634832, -12.26659068614894821 ) ) ;
#3839 = CARTESIAN_POINT ( 'NONE',  ( 2.917880565312948704, 37.63708216824731068, 12.26659068614894643 ) ) ;
#3840 = CARTESIAN_POINT ( 'NONE',  ( 2.791683348922240793, 31.63393115100078745, 7.208316651077764092 ) ) ;
#3841 = PLANE ( 'NONE',  #95399 ) ;
#3842 = CARTESIAN_POINT ( 'NONE',  ( 19.42250999205614193, 20.14701867748817321, 5.440088680355555262 ) ) ;
#3843 = CIRCLE ( 'NONE', #67712, 11.92686044187656513 ) ;
#3844 = CARTESIAN_POINT ( 'NONE',  ( 0.5774900079438607392, 53.48035201082151247, 5.440088680355550821 ) ) ;
#3845 = CARTESIAN_POINT ( 'NONE',  ( 13.75801628063879711, 15.00000000000000000, -4.578972376164444746 ) ) ;
#3846 = EDGE_LOOP ( 'NONE', ( #4746, #67108, #37781, #17654 ) ) ;
#3847 = CARTESIAN_POINT ( 'NONE',  ( -1.099225684535947600, 38.70696800326375353, -6.408140936763238038 ) ) ;
#3848 = CARTESIAN_POINT ( 'NONE',  ( 0.5774900079438607392, 48.48035201082150536, 5.440088680355550821 ) ) ;
#3849 = VERTEX_POINT ( 'NONE', #58034 ) ;
#3850 = FACE_OUTER_BOUND ( 'NONE', #26365, .T. ) ;
#3851 = EDGE_CURVE ( 'NONE', #88606, #59795, #66031, .T. ) ;
#3852 = CARTESIAN_POINT ( 'NONE',  ( 12.91533473730993009, 61.60535201082150536, -10.88017736071109987 ) ) ;
#3853 = ORIENTED_EDGE ( 'NONE', *, *, #76791, .T. ) ;
#3854 = CARTESIAN_POINT ( 'NONE',  ( 4.559911319644449179, 62.23035201082150536, -9.422509992056141925 ) ) ;
#3855 = DIRECTION ( 'NONE',  ( -0.8338858220671658827, 0.000000000000000000, -0.5519369853120617009 ) ) ;
#3856 = CARTESIAN_POINT ( 'NONE',  ( 0.000000000000000000, 0.5000000000000004441, 0.000000000000000000 ) ) ;
#3857 = CARTESIAN_POINT ( 'NONE',  ( 2.035157376598822676, 7.438685344154837509, -7.964842623401177768 ) ) ;
#3858 = CARTESIAN_POINT ( 'NONE',  ( 5.076628168052703671, 6.842264484334118713, 8.527530157486179263 ) ) ;
#3859 = CARTESIAN_POINT ( 'NONE',  ( -0.3689425029237881626, 12.42874883491396609, 10.36894250292379027 ) ) ;
#3860 = CARTESIAN_POINT ( 'NONE',  ( 18.52753015748618282, 8.925597817667451750, -4.923371831947291888 ) ) ;
#3861 = CARTESIAN_POINT ( 'NONE',  ( 2.035157376598822676, 22.43868534415483396, -7.964842623401177768 ) ) ;
#3862 = CARTESIAN_POINT ( 'NONE',  ( 10.00000000000000000, 59.75893115100078745, -9.846743663894594434 ) ) ;
#3863 = VERTEX_POINT ( 'NONE', #72062 ) ;
#3864 = CARTESIAN_POINT ( 'NONE',  ( 5.076628168052703671, 46.84226448433412315, 8.527530157486179263 ) ) ;
#3865 = EDGE_LOOP ( 'NONE', ( #8215, #61037, #25643, #64355, #6806, #79339, #24164, #19615 ) ) ;
#3866 = CARTESIAN_POINT ( 'NONE',  ( 19.72487221294570858, 70.00000000000000000, 6.000000000000000000 ) ) ;
#3867 = CARTESIAN_POINT ( 'NONE',  ( 15.44008868035555793, 56.39701867748817676, -9.422509992056140149 ) ) ;
#3868 = CARTESIAN_POINT ( 'NONE',  ( 17.20831665107776587, 52.88393115100078035, 7.208316651077764980 ) ) ;
#3870 = DIRECTION ( 'NONE',  ( -1.000000000000000000, -1.927470528863123732E-16, 0.000000000000000000 ) ) ;
#3869 = CARTESIAN_POINT ( 'NONE',  ( 2.035157376598822676, 12.43868534415483751, -7.964842623401177768 ) ) ;
#3871 = CARTESIAN_POINT ( 'NONE',  ( 7.084665262690076126, 64.10535201082150536, 10.88017736071109987 ) ) ;
#3872 = CARTESIAN_POINT ( 'NONE',  ( 6.204703633549690345, 65.76208216824731778, -14.16423886937410259 ) ) ;
#3873 = VERTEX_POINT ( 'NONE', #12051 ) ;
#3874 = ADVANCED_FACE ( 'NONE', ( #27047 ), #35538, .T. ) ;
#3875 = CARTESIAN_POINT ( 'NONE',  ( 0.6178305044545838731, 44.74863466993042493, 9.382169495545420901 ) ) ;
#3876 = CARTESIAN_POINT ( 'NONE',  ( -0.8801773607111009756, 33.06368534415484106, 1.068504757029289695E-15 ) ) ;
#3877 = DIRECTION ( 'NONE',  ( 0.000000000000000000, 1.000000000000000000, 0.000000000000000000 ) ) ;
#3878 = VERTEX_POINT ( 'NONE', #56580 ) ;
#3879 = CARTESIAN_POINT ( 'NONE',  ( 16.40814093676324603, 42.45696800326375353, -11.09922568453594671 ) ) ;
#3880 = CARTESIAN_POINT ( 'NONE',  ( 10.00000000000000000, 36.81368534415484106, -10.88017736071110342 ) ) ;
#3881 = EDGE_CURVE ( 'NONE', #85215, #57334, #12414, .T. ) ;
#3882 = EDGE_LOOP ( 'NONE', ( #36369, #73407, #25454, #32022 ) ) ;
#3883 = CARTESIAN_POINT ( 'NONE',  ( 0.1532563361054100626, 65.80059781766745175, -2.638427012816831230 ) ) ;
#3885 = CARTESIAN_POINT ( 'NONE',  ( 0.1532563361054100626, 45.80059781766745886, -2.638427012816831230 ) ) ;
#3884 = CARTESIAN_POINT ( 'NONE',  ( 12.63842701281683922, 14.55059781766744997, -9.846743663894590881 ) ) ;
#3886 = CARTESIAN_POINT ( 'NONE',  ( 10.00000000000000000, 16.81368534415483751, -10.88017736071110342 ) ) ;
#3887 = DIRECTION ( 'NONE',  ( -1.000000000000000000, 0.000000000000000000, 0.000000000000000000 ) ) ;
#3888 = CARTESIAN_POINT ( 'NONE',  ( 2.791683348922237240, 40.38393115100078035, -7.208316651077763204 ) ) ;
#3889 = FACE_OUTER_BOUND ( 'NONE', #88582, .T. ) ;
#3890 = CARTESIAN_POINT ( 'NONE',  ( 14.94699059465101776, 0.5000000000000004441, -1.259949270174818059 ) ) ;
#3892 = CARTESIAN_POINT ( 'NONE',  ( 17.20831665107776587, 14.13393115100078568, -7.208316651077762316 ) ) ;
#3891 = CARTESIAN_POINT ( 'NONE',  ( 14.92337183194729988, 24.34226448433411960, -8.527530157486177487 ) ) ;
#3893 = LINE ( 'NONE', #34361, #45735 ) ;
#3895 = ORIENTED_EDGE ( 'NONE', *, *, #37450, .T. ) ;
#3894 = CARTESIAN_POINT ( 'NONE',  ( 10.00000000000000178, 62.25893115100078745, 9.846743663894594434 ) ) ;
#3896 = CARTESIAN_POINT ( 'NONE',  ( 20.10239578412225470, 7.633775574782964313, -6.340343622311918281 ) ) ;
#3897 = CARTESIAN_POINT ( 'NONE',  ( -2.816281873526471635, 43.91530133659708923, -3.434112377981056508 ) ) ;
#3898 = CARTESIAN_POINT ( 'NONE',  ( 2.791683348922240793, 46.63393115100077324, 7.208316651077764092 ) ) ;
#3899 = AXIS2_PLACEMENT_3D ( 'NONE', #71999, #3526, #32526 ) ;
#3900 = CARTESIAN_POINT ( 'NONE',  ( 0.1916775849787255848, 12.25868815902069642, -6.500000000000001776 ) ) ;
#3901 = CARTESIAN_POINT ( 'NONE',  ( 17.08211943468705130, 63.47041550158063927, 12.26659068614894998 ) ) ;
#3902 = CARTESIAN_POINT ( 'NONE',  ( 12.63842701281683922, 24.55059781766745175, -9.846743663894590881 ) ) ;
#3903 = DIRECTION ( 'NONE',  ( 0.08715574274765139351, 0.9961946980917461003, -0.000000000000000000 ) ) ;
#3904 = VECTOR ( 'NONE', #60597, 1000.000000000000000 ) ;
#3905 = CARTESIAN_POINT ( 'NONE',  ( 17.08211943468705130, 53.47041550158063217, 12.26659068614894998 ) ) ;
#3906 = CARTESIAN_POINT ( 'NONE',  ( 19.84674366389459266, 63.71726448433412315, -2.638427012816827677 ) ) ;
#3907 = CARTESIAN_POINT ( 'NONE',  ( 17.96484262340118221, 4.938685344154837509, 7.964842623401181321 ) ) ;
#3908 = CARTESIAN_POINT ( 'NONE',  ( -2.266590686148945544, 31.38708216824730002, -7.082119434687050408 ) ) ;
#3910 = DIRECTION ( 'NONE',  ( 0.000000000000000000, -1.000000000000000000, 0.000000000000000000 ) ) ;
#3909 = CARTESIAN_POINT ( 'NONE',  ( 22.26659068614895176, 34.72041550158063927, -7.082119434687042414 ) ) ;
#3912 = CARTESIAN_POINT ( 'NONE',  ( 0.1532563361054100626, 60.80059781766744464, -2.638427012816831230 ) ) ;
#3911 = CARTESIAN_POINT ( 'NONE',  ( -8.209432707284724628, 0.3639311627136666005, -12.55409154915499492 ) ) ;
#3913 = CARTESIAN_POINT ( 'NONE',  ( 19.42250999205614548, 45.98035201082150536, -5.440088680355545492 ) ) ;
#3914 = CARTESIAN_POINT ( 'NONE',  ( 11.33945612263218372, -87.84223371190563512, 3.750000000000000000 ) ) ;
#3915 = EDGE_CURVE ( 'NONE', #62655, #12737, #90924, .T. ) ;
#3916 = DIRECTION ( 'NONE',  ( 0.6246950475544237324, 0.7808688094430306093, 0.000000000000000000 ) ) ;
#3917 = CARTESIAN_POINT ( 'NONE',  ( 18.52753015748617571, 58.09226448433411605, 4.923371831947298993 ) ) ;
#3918 = CARTESIAN_POINT ( 'NONE',  ( 2.917880565312950480, 0.9704155015806342766, -12.26659068614894821 ) ) ;
#3919 = VERTEX_POINT ( 'NONE', #42552 ) ;
#3920 = CARTESIAN_POINT ( 'NONE',  ( 24.16423886937410614, 24.30374883491396787, 8.672049930838204340E-16 ) ) ;
#3921 = CARTESIAN_POINT ( 'NONE',  ( 17.75000000000000000, 78.32179676972447169, -4.000000000000000000 ) ) ;
#3923 = CARTESIAN_POINT ( 'NONE',  ( -12.25993886608593364, 0.5000000000000004441, -8.642563219313787570 ) ) ;
#3922 = CARTESIAN_POINT ( 'NONE',  ( -3.335599319945496077, -2.700684445898925645, -2.499999999999999112 ) ) ;
#3924 = CARTESIAN_POINT ( 'NONE',  ( 2.035157376598822676, 17.43868534415483751, -7.964842623401177768 ) ) ;
#3925 = CARTESIAN_POINT ( 'NONE',  ( 22.81628187352648496, 26.83196800326374998, -3.434112377981050290 ) ) ;
#3926 = CARTESIAN_POINT ( 'NONE',  ( -14.35840480524201190, 14.49999999999999112, -4.340070442839034648 ) ) ;
#3927 = CARTESIAN_POINT ( 'NONE',  ( 7.361572987183170547, 12.05059781766744997, 9.846743663894590881 ) ) ;
#3928 = VERTEX_POINT ( 'NONE', #58529 ) ;
#3929 = CARTESIAN_POINT ( 'NONE',  ( 7.184035427668765017, -73.16388022040806050, -4.000000000000000000 ) ) ;
#3930 = ADVANCED_FACE ( 'NONE', ( #57545 ), #81039, .F. ) ;
#3931 = DIRECTION ( 'NONE',  ( -0.000000000000000000, 0.000000000000000000, 1.000000000000000000 ) ) ;
#3932 = CARTESIAN_POINT ( 'NONE',  ( -7.374944882893554876, -78.83129233208416053, 4.000000000000000888 ) ) ;
#3933 = CARTESIAN_POINT ( 'NONE',  ( 7.084665262690076126, 7.022018677488170546, -10.88017736071110164 ) ) ;
#3934 = CARTESIAN_POINT ( 'NONE',  ( 4.181050312905074229, 2.541098841762901017E-16, -14.01631781289604106 ) ) ;
#3935 = CARTESIAN_POINT ( 'NONE',  ( 20.88017736071110164, 35.35535201082150536, 2.915334737309930979 ) ) ;
#3936 = CARTESIAN_POINT ( 'NONE',  ( -0.8801773607111008646, 43.27201867748817676, 2.915334737309923430 ) ) ;
#3937 = CARTESIAN_POINT ( 'NONE',  ( 22.81628187352647785, 11.62363466993042138, 6.195893100308588602E-16 ) ) ;
#3938 = CARTESIAN_POINT ( 'NONE',  ( 1.472469842513823179, 61.42559781766745175, 4.923371831947296329 ) ) ;
#3939 = CARTESIAN_POINT ( 'NONE',  ( -6.000000000000009770, 40.99999999999999289, 6.500000000000000888 ) ) ;
#3940 = CARTESIAN_POINT ( 'NONE',  ( 19.84674366389459266, 13.71726448433411782, -2.638427012816827677 ) ) ;
#3941 = CARTESIAN_POINT ( 'NONE',  ( -3.750000000000000000, 10.00000000000000000, -2.750000000000000000 ) ) ;
#3942 = TOROIDAL_SURFACE ( 'NONE', #74139, 14.49999999999999822, 0.5000000000000000000 ) ;
#3943 = CARTESIAN_POINT ( 'NONE',  ( 19.42250999205614548, 45.98035201082150536, -5.440088680355545492 ) ) ;
#3944 = CARTESIAN_POINT ( 'NONE',  ( 13.43411237798105340, 0.5819680032637533085, 12.81628187352647963 ) ) ;
#3945 = CARTESIAN_POINT ( 'NONE',  ( 19.42250999205614193, 60.14701867748817676, 5.440088680355555262 ) ) ;
#3946 = CARTESIAN_POINT ( 'NONE',  ( 12.63842701281683922, 24.55059781766745175, -9.846743663894590881 ) ) ;
#3947 = CARTESIAN_POINT ( 'NONE',  ( 13.43411237798105340, 45.58196800326374643, 12.81628187352647963 ) ) ;
#3949 = CARTESIAN_POINT ( 'NONE',  ( 5.500000000000000000, 10.49999999999999822, 6.500000000000000888 ) ) ;
#3948 = CARTESIAN_POINT ( 'NONE',  ( 10.00000000000000000, -0.2410688489992152128, -9.846743663894594434 ) ) ;
#3950 = EDGE_LOOP ( 'NONE', ( #20486, #28079, #72349, #18746 ) ) ;
#3951 = CARTESIAN_POINT ( 'NONE',  ( 4.873787042390789637, 15.00000000000000000, -13.39061984619918988 ) ) ;
#3952 = LINE ( 'NONE', #71474, #73349 ) ;
#3953 = CARTESIAN_POINT ( 'NONE',  ( 19.42250999205614548, 5.980352010821504471, -5.440088680355545492 ) ) ;
#3955 = CARTESIAN_POINT ( 'NONE',  ( 17.08211943468705130, 23.47041550158063572, 12.26659068614894998 ) ) ;
#3954 = CARTESIAN_POINT ( 'NONE',  ( 6.565887622018943937, 60.16530133659707502, 12.81628187352647430 ) ) ;
#3956 = CARTESIAN_POINT ( 'NONE',  ( 2.791683348922237240, 25.38393115100078390, -7.208316651077763204 ) ) ;
#3957 = CARTESIAN_POINT ( 'NONE',  ( 20.88017736071110875, 20.77201867748816611, -2.915334737309920765 ) ) ;
#3958 = CARTESIAN_POINT ( 'NONE',  ( 2.917880565312948704, 67.63708216824730357, 12.26659068614894643 ) ) ;
#3959 = VERTEX_POINT ( 'NONE', #80056 ) ;
#3960 = VECTOR ( 'NONE', #4331, 1000.000000000000000 ) ;
#3961 = CARTESIAN_POINT ( 'NONE',  ( 20.88017736071110164, 15.35535201082150358, 2.915334737309930979 ) ) ;
#3962 = EDGE_CURVE ( 'NONE', #97016, #51739, #66195, .T. ) ;
#3963 = CARTESIAN_POINT ( 'NONE',  ( 4.559911319644449179, 27.23035201082150536, -9.422509992056141925 ) ) ;
#3965 = CARTESIAN_POINT ( 'NONE',  ( 12.91533473730993009, 31.60535201082150891, -10.88017736071109987 ) ) ;
#3964 = DIRECTION ( 'NONE',  ( -0.2164396139380971307, 0.000000000000000000, -0.9762960071199346945 ) ) ;
#3966 = ORIENTED_EDGE ( 'NONE', *, *, #9045, .F. ) ;
#3967 = CARTESIAN_POINT ( 'NONE',  ( 18.52753015748617571, 63.09226448433412315, 4.923371831947298993 ) ) ;
#3968 = CARTESIAN_POINT ( 'NONE',  ( 15.44008868035555260, 24.73035201082150891, 9.422509992056143702 ) ) ;
#3969 = CARTESIAN_POINT ( 'NONE',  ( 18.52753015748617571, 63.09226448433412315, 4.923371831947298993 ) ) ;
#3970 = DIRECTION ( 'NONE',  ( -0.000000000000000000, -0.000000000000000000, 1.000000000000000000 ) ) ;
#3971 = CARTESIAN_POINT ( 'NONE',  ( 10.00000000000000000, 57.87363466993042493, -12.81628187352647608 ) ) ;
#3972 = CARTESIAN_POINT ( 'NONE',  ( 0.8952175423694801459, 67.60160829253887016, -5.990408912944315212 ) ) ;
#3974 = CARTESIAN_POINT ( 'NONE',  ( 20.36894250292379738, 34.92874883491396076, -10.36894250292379027 ) ) ;
#3973 = TOROIDAL_SURFACE ( 'NONE', #85396, 1.750000000000000888, 0.2500000000000000000 ) ;
#3975 = CARTESIAN_POINT ( 'NONE',  ( 20.88017736071110875, 45.77201867748816966, -2.915334737309920765 ) ) ;
#3976 = CARTESIAN_POINT ( 'NONE',  ( 4.559911319644449179, 12.23035201082150714, -9.422509992056141925 ) ) ;
#3977 = ADVANCED_FACE ( 'NONE', ( #73527 ), #10732, .T. ) ;
#3978 = CARTESIAN_POINT ( 'NONE',  ( 19.84674366389459266, 53.71726448433411605, -2.638427012816827677 ) ) ;
#3979 = AXIS2_PLACEMENT_3D ( 'NONE', #75483, #92447, #10437 ) ;
#3980 = CARTESIAN_POINT ( 'NONE',  ( 0.1532563361054100626, 45.80059781766745886, -2.638427012816831230 ) ) ;
#3981 = VECTOR ( 'NONE', #89387, 1000.000000000000000 ) ;
#3982 = CARTESIAN_POINT ( 'NONE',  ( 20.15039907845753930, 70.00000000000000000, -6.262539305110068177 ) ) ;
#3983 = CARTESIAN_POINT ( 'NONE',  ( 0.1532563361054083140, 11.00893115100078568, 1.131784320476157264E-15 ) ) ;
#3984 = CARTESIAN_POINT ( 'NONE',  ( -6.408140936763246032, -36.70969866340291077, -11.09922568453594316 ) ) ;
#3985 = ORIENTED_EDGE ( 'NONE', *, *, #43233, .F. ) ;
#3986 = AXIS2_PLACEMENT_3D ( 'NONE', #30316, #15352, #45838 ) ;
#3987 = CARTESIAN_POINT ( 'NONE',  ( 2.035157376598824452, 13.68868534415483751, 7.964842623401179544 ) ) ;
#3988 = CARTESIAN_POINT ( 'NONE',  ( 12.63842701281683034, 7.467264484334118713, 9.846743663894596210 ) ) ;
#3989 = EDGE_CURVE ( 'NONE', #16659, #32093, #30185, .T. ) ;
#3990 = CARTESIAN_POINT ( 'NONE',  ( 10.00000000000000000, 64.75893115100078035, -9.846743663894594434 ) ) ;
#3992 = CARTESIAN_POINT ( 'NONE',  ( 15.44008868035555260, 49.73035201082150536, 9.422509992056143702 ) ) ;
#3991 = CARTESIAN_POINT ( 'NONE',  ( 20.88017736071110164, 65.35535201082150536, 2.915334737309930979 ) ) ;
#3994 = CARTESIAN_POINT ( 'NONE',  ( 10.00000000000000000, 62.87363466993042493, -12.81628187352647608 ) ) ;
#3993 = CARTESIAN_POINT ( 'NONE',  ( -0.8801773607110991993, 22.85535201082150181, -2.915334737309923874 ) ) ;
#3995 = CARTESIAN_POINT ( 'NONE',  ( 13.79529636645031943, 30.34541550158063927, -14.16423886937409904 ) ) ;
#3996 = CARTESIAN_POINT ( 'NONE',  ( 2.791683348922240793, 11.63393115100078568, 7.208316651077764092 ) ) ;
#3997 = AXIS2_PLACEMENT_3D ( 'NONE', #60355, #44853, #91851 ) ;
#3998 = ADVANCED_FACE ( 'NONE', ( #51481, #13487 ), #74469, .T. ) ;
#3999 = CARTESIAN_POINT ( 'NONE',  ( 3.591859063236763294, 53.29030133659708923, -11.09922568453595026 ) ) ;
#4000 = EDGE_LOOP ( 'NONE', ( #88897, #61277, #8691, #69244, #4087, #19191 ) ) ;
#4001 = CARTESIAN_POINT ( 'NONE',  ( 10.00000000000000178, 5.373634669930420493, 12.81628187352647608 ) ) ;
#4002 = DIRECTION ( 'NONE',  ( 0.000000000000000000, 0.000000000000000000, -1.000000000000000000 ) ) ;
#4003 = CARTESIAN_POINT ( 'NONE',  ( 0.5774900079438607392, 28.48035201082150891, 5.440088680355550821 ) ) ;
#4005 = EDGE_CURVE ( 'NONE', #10110, #86010, #76692, .T. ) ;
#4004 = LINE ( 'NONE', #4497, #95246 ) ;
#4006 = VERTEX_POINT ( 'NONE', #54428 ) ;
#4008 = CARTESIAN_POINT ( 'NONE',  ( -15.00000000000000000, 83.99999999999998579, -3.750000000000000000 ) ) ;
#4007 = CARTESIAN_POINT ( 'NONE',  ( 17.20831665107776587, 9.133931151000787452, -7.208316651077762316 ) ) ;
#4009 = CARTESIAN_POINT ( 'NONE',  ( 19.84674366389459621, 8.508931151000785675, 7.409399052514197653E-17 ) ) ;
#4010 = CARTESIAN_POINT ( 'NONE',  ( 1.472469842513823179, 25.59226448433412315, -4.923371831947296329 ) ) ;
#4011 = CARTESIAN_POINT ( 'NONE',  ( 0.1532563361054082862, 11.21726448433411605, 2.638427012816831674 ) ) ;
#4012 = CARTESIAN_POINT ( 'NONE',  ( 14.92337183194729633, 2.675597817667451750, 8.527530157486181039 ) ) ;
#4013 = AXIS2_PLACEMENT_3D ( 'NONE', #22187, #44675, #76163 ) ;
#4015 = CARTESIAN_POINT ( 'NONE',  ( -14.47650479471830387, 14.49999999999999112, 3.928206833721953561 ) ) ;
#4014 = CARTESIAN_POINT ( 'NONE',  ( 0.5774900079438607392, 53.48035201082151247, 5.440088680355550821 ) ) ;
#4016 = CARTESIAN_POINT ( 'NONE',  ( 19.42250999205614548, 60.98035201082151247, -5.440088680355545492 ) ) ;
#4018 = ORIENTED_EDGE ( 'NONE', *, *, #69832, .T. ) ;
#4017 = CARTESIAN_POINT ( 'NONE',  ( 2.791683348922240793, 21.63393115100078745, 7.208316651077764092 ) ) ;
#4019 = CARTESIAN_POINT ( 'NONE',  ( -9.065164099344617199, 0.3640475087720972946, 11.95084933600761623 ) ) ;
#4020 = CARTESIAN_POINT ( 'NONE',  ( 12.63842701281683922, 54.55059781766745175, -9.846743663894590881 ) ) ;
#4021 = EDGE_LOOP ( 'NONE', ( #65373, #62874, #89486, #27328 ) ) ;
#4022 = CARTESIAN_POINT ( 'NONE',  ( 19.42250999205614193, 5.147018677488171434, 5.440088680355555262 ) ) ;
#4023 = CARTESIAN_POINT ( 'NONE',  ( 22.26659068614895176, 24.72041550158063572, -7.082119434687042414 ) ) ;
#4024 = B_SPLINE_CURVE_WITH_KNOTS ( 'NONE', 3,
 ( #18326, #33307, #48807, #79315, #41343, #3822 ),
 .UNSPECIFIED., .F., .F.,
 ( 4, 2, 4 ),
 ( 3.409110551496115105E-05, 0.0004400426677367866800, 0.0008459942299586121345 ),
 .UNSPECIFIED. ) ;
#4025 = CARTESIAN_POINT ( 'NONE',  ( 0.000000000000000000, 0.5000000000000004441, 0.000000000000000000 ) ) ;
#4026 = CARTESIAN_POINT ( 'NONE',  ( 20.36894250292379738, 14.92874883491396432, -10.36894250292379027 ) ) ;
#4027 = CARTESIAN_POINT ( 'NONE',  ( 13.79529636645031943, 30.34541550158063927, -14.16423886937409904 ) ) ;
#4028 = LINE ( 'NONE', #73476, #50263 ) ;
#4029 =( NAMED_UNIT ( * ) PLANE_ANGLE_UNIT ( ) SI_UNIT ( $, .RADIAN. ) );
#4030 = CARTESIAN_POINT ( 'NONE',  ( 17.96484262340118221, 39.93868534415484106, 7.964842623401181321 ) ) ;
#4031 = CARTESIAN_POINT ( 'NONE',  ( -6.689969769698787871, 0.000000000000000000, -12.58200319823979285 ) ) ;
#4032 = CARTESIAN_POINT ( 'NONE',  ( 5.076628168052704559, 15.17559781766745175, -8.527530157486179263 ) ) ;
#4034 = CARTESIAN_POINT ( 'NONE',  ( 2.791683348922237240, 20.38393115100078745, -7.208316651077763204 ) ) ;
#4033 = CARTESIAN_POINT ( 'NONE',  ( 0.5774900079438607392, 58.48035201082151247, 5.440088680355550821 ) ) ;
#4035 = CARTESIAN_POINT ( 'NONE',  ( 17.96484262340118221, 9.938685344154839285, 7.964842623401181321 ) ) ;
#4036 = CARTESIAN_POINT ( 'NONE',  ( 10.00000000000000000, 42.87363466993042493, -12.81628187352647608 ) ) ;
#4037 = CARTESIAN_POINT ( 'NONE',  ( 7.361572987183169658, 44.96726448433412315, -9.846743663894592657 ) ) ;
#4038 = CARTESIAN_POINT ( 'NONE',  ( 18.04007052943772749, 58.01528370094807485, 5.767676674365840306 ) ) ;
#4039 = EDGE_CURVE ( 'NONE', #7321, #79142, #30291, .T. ) ;
#4040 = CARTESIAN_POINT ( 'NONE',  ( 13.43411237798106583, 32.66530133659708213, -12.81628187352647252 ) ) ;
#4041 = CARTESIAN_POINT ( 'NONE',  ( 12.26659068614894466, -30.27958449841936428, -7.082119434687053960 ) ) ;
#4042 = CARTESIAN_POINT ( 'NONE',  ( 19.84674366389459621, 28.50893115100078745, 7.409399052514197653E-17 ) ) ;
#4043 = CARTESIAN_POINT ( 'NONE',  ( 10.00000000000000000, 10.55374883491396787, -14.16423886937410082 ) ) ;
#4044 = ORIENTED_EDGE ( 'NONE', *, *, #36141, .F. ) ;
#4045 = DIRECTION ( 'NONE',  ( -0.000000000000000000, 1.000000000000000000, -0.000000000000000000 ) ) ;
#4046 = AXIS2_PLACEMENT_3D ( 'NONE', #90205, #20241, #50744 ) ;
#4047 = CARTESIAN_POINT ( 'NONE',  ( 19.42250999205614193, 45.14701867748817676, 5.440088680355555262 ) ) ;
#4048 = CARTESIAN_POINT ( 'NONE',  ( 12.91533473730993009, 46.60535201082150536, -10.88017736071109987 ) ) ;
#4049 = CARTESIAN_POINT ( 'NONE',  ( 20.36894250292379382, 48.67874883491396076, 10.36894250292379205 ) ) ;
#4050 = CARTESIAN_POINT ( 'NONE',  ( 18.52753015748618282, 53.92559781766745175, -4.923371831947291888 ) ) ;
#4051 = CARTESIAN_POINT ( 'NONE',  ( 19.84674366389459621, 8.508931151000785675, 7.409399052514197653E-17 ) ) ;
#4052 = CARTESIAN_POINT ( 'NONE',  ( -14.88232117145532030, 14.63606897487788849, -1.875237731503358152 ) ) ;
#4053 = CARTESIAN_POINT ( 'NONE',  ( 2.035157376598822676, 47.43868534415484817, -7.964842623401177768 ) ) ;
#4054 = FACE_OUTER_BOUND ( 'NONE', #51584, .T. ) ;
#4055 = CARTESIAN_POINT ( 'NONE',  ( 16.40814093676324603, 27.45696800326375708, -11.09922568453594671 ) ) ;
#4056 = CARTESIAN_POINT ( 'NONE',  ( 17.20831665107776587, 57.88393115100078745, 7.208316651077764980 ) ) ;
#4057 = CARTESIAN_POINT ( 'NONE',  ( 2.915334737309921209, 16.60535201082150891, -10.88017736071110164 ) ) ;
#4058 = CARTESIAN_POINT ( 'NONE',  ( 10.00000000000000000, 66.81368534415484817, -10.88017736071110342 ) ) ;
#4059 =( LENGTH_UNIT ( ) NAMED_UNIT ( * ) SI_UNIT ( .MILLI., .METRE. ) );
#4060 = CARTESIAN_POINT ( 'NONE',  ( 10.00000000000000178, 2.258931151000784787, 9.846743663894594434 ) ) ;
#4061 = CARTESIAN_POINT ( 'NONE',  ( 0.5774900079438607392, 68.48035201082150536, 5.440088680355550821 ) ) ;
#4062 = CARTESIAN_POINT ( 'NONE',  ( 24.35999999999999233, 37.99999999999997868, -9.500000000000000000 ) ) ;
#4063 = AXIS2_PLACEMENT_3D ( 'NONE', #64970, #11991, #27478 ) ;
#4064 = CARTESIAN_POINT ( 'NONE',  ( 18.52753015748617571, 33.09226448433411605, 4.923371831947298993 ) ) ;
#4065 = CARTESIAN_POINT ( 'NONE',  ( 10.00000000000000000, 21.81368534415484106, -10.88017736071110342 ) ) ;
#4066 = CARTESIAN_POINT ( 'NONE',  ( 0.1532563361054100626, 60.80059781766744464, -2.638427012816831230 ) ) ;
#4068 = CARTESIAN_POINT ( 'NONE',  ( -3.771300132029604679, -6.411618995301440194, -3.750000000000000888 ) ) ;
#4067 = CARTESIAN_POINT ( 'NONE',  ( 2.035157376598824452, 33.68868534415484106, 7.964842623401179544 ) ) ;
#4069 = CARTESIAN_POINT ( 'NONE',  ( -27.43587634952538323, 44.49999999999997158, 9.500000000000000000 ) ) ;
#4070 = CARTESIAN_POINT ( 'NONE',  ( 3.591859063236761518, 39.95696800326375353, 11.09922568453594849 ) ) ;
#4071 = EDGE_LOOP ( 'NONE', ( #17052, #49010, #96186, #82986, #22920, #1584 ) ) ;
#4072 = CARTESIAN_POINT ( 'NONE',  ( 19.42250999205614193, 55.14701867748817676, 5.440088680355555262 ) ) ;
#4074 = CARTESIAN_POINT ( 'NONE',  ( -18.89999999999999503, 98.99999999999998579, 8.000000000000000000 ) ) ;
#4073 = CARTESIAN_POINT ( 'NONE',  ( 16.40814093676324603, 17.45696800326375353, -11.09922568453594671 ) ) ;
#4075 = CARTESIAN_POINT ( 'NONE',  ( 12.63842701281683034, 2.467264484334118269, 9.846743663894596210 ) ) ;
#4076 = CARTESIAN_POINT ( 'NONE',  ( 17.96484262340118221, 29.93868534415484106, 7.964842623401181321 ) ) ;
#4077 = CARTESIAN_POINT ( 'NONE',  ( 22.26659068614895176, 59.72041550158063927, -7.082119434687042414 ) ) ;
#4078 = CARTESIAN_POINT ( 'NONE',  ( 10.00000000000000000, 49.75893115100078745, -9.846743663894594434 ) ) ;
#4079 = CARTESIAN_POINT ( 'NONE',  ( 17.20831665107776587, 7.883931151000784787, 7.208316651077764980 ) ) ;
#4080 = CARTESIAN_POINT ( 'NONE',  ( 4.559911319644449179, 62.23035201082150536, -9.422509992056141925 ) ) ;
#4081 = CARTESIAN_POINT ( 'NONE',  ( -8.549759589250404801, 14.76984986100782393, -12.25250350990841319 ) ) ;
#4082 = CARTESIAN_POINT ( 'NONE',  ( 24.16423886937409904, 29.09541550158063572, 3.795296366450317205 ) ) ;
#4083 = CARTESIAN_POINT ( 'NONE',  ( 6.689969769698956625, 0.000000000000000000, -12.58200319823970226 ) ) ;
#4084 = CARTESIAN_POINT ( 'NONE',  ( -3.878348535190609958, -3.630205232350322664, -4.000000000000000000 ) ) ;
#4086 = VERTEX_POINT ( 'NONE', #61437 ) ;
#4085 = EDGE_CURVE ( 'NONE', #16659, #26486, #41434, .T. ) ;
#4087 = ORIENTED_EDGE ( 'NONE', *, *, #95830, .F. ) ;
#4088 = CARTESIAN_POINT ( 'NONE',  ( 2.917880565312948704, 52.63708216824730357, 12.26659068614894643 ) ) ;
#4089 = CARTESIAN_POINT ( 'NONE',  ( 2.917880565312948704, 47.63708216824730357, 12.26659068614894643 ) ) ;
#4090 = CARTESIAN_POINT ( 'NONE',  ( 10.00000000000000178, 22.25893115100078745, 9.846743663894594434 ) ) ;
#4092 = CARTESIAN_POINT ( 'NONE',  ( -1.099225684535947600, 14.54030133659708568, 6.408140936763237150 ) ) ;
#4091 = CIRCLE ( 'NONE', #55162, 6.349999999999995204 ) ;
#4093 = CARTESIAN_POINT ( 'NONE',  ( -1.354709868695410657, 14.49999999999999822, -14.93870011653153718 ) ) ;
#4094 = DIRECTION ( 'NONE',  ( 0.7132504491541801217, -0.000000000000000000, 0.7009092642998523415 ) ) ;
#4096 = CARTESIAN_POINT ( 'NONE',  ( 22.81628187352647785, 51.41530133659708923, 3.434112377981063169 ) ) ;
#4095 = SURFACE_SIDE_STYLE ('',( #12072 ) ) ;
#4097 = CARTESIAN_POINT ( 'NONE',  ( 22.26659068614894466, 48.88708216824730357, 7.082119434687054849 ) ) ;
#4098 = EDGE_CURVE ( 'NONE', #24454, #17231, #14305, .T. ) ;
#4099 = EDGE_CURVE ( 'NONE', #40524, #88245, #31425, .T. ) ;
#4100 = DIRECTION ( 'NONE',  ( 2.220446049250313396E-14, 0.000000000000000000, 1.000000000000000000 ) ) ;
#4101 = CARTESIAN_POINT ( 'NONE',  ( 19.84674366389459266, 8.717264484334116048, -2.638427012816827677 ) ) ;
#4102 = CARTESIAN_POINT ( 'NONE',  ( 3.469446951953614189E-15, 2.258931151000794113, 9.846743663894594434 ) ) ;
#4103 = ORIENTED_EDGE ( 'NONE', *, *, #18120, .T. ) ;
#4104 = CARTESIAN_POINT ( 'NONE',  ( 18.52753015748618282, 13.92559781766745175, -4.923371831947291888 ) ) ;
#4105 = ORIENTED_EDGE ( 'NONE', *, *, #89557, .T. ) ;
#4107 = CARTESIAN_POINT ( 'NONE',  ( 19.42250999205614548, 30.98035201082150536, -5.440088680355545492 ) ) ;
#4106 = CARTESIAN_POINT ( 'NONE',  ( 20.88017736071110164, 5.355352010821503583, 2.915334737309930979 ) ) ;
#4109 = CARTESIAN_POINT ( 'NONE',  ( 21.09922568453594849, 6.206968003263753531, 6.408140936763242479 ) ) ;
#4108 = CARTESIAN_POINT ( 'NONE',  ( 17.20831665107776587, 49.13393115100078745, -7.208316651077762316 ) ) ;
#4110 = DIRECTION ( 'NONE',  ( -1.000000000000000000, 0.000000000000000000, -0.000000000000000000 ) ) ;
#4111 = VECTOR ( 'NONE', #3903, 1000.000000000000114 ) ;
#4113 = CARTESIAN_POINT ( 'NONE',  ( 0.6178305044545818747, 18.49863466993041428, -9.382169495545419124 ) ) ;
#4112 = COLOUR_RGB ( '', 0.08235294, 0.09019608, 0.10196078) ;
#4114 = ORIENTED_EDGE ( 'NONE', *, *, #3061, .T. ) ;
#4115 =( BOUNDED_CURVE ( )  B_SPLINE_CURVE ( 2, ( #19207, #21682, #28182, #21182, #51682, #45149, #6666, #60643, #82161 ),
 .UNSPECIFIED., .F., .T. ) 
 B_SPLINE_CURVE_WITH_KNOTS ( ( 3, 2, 2, 2, 3 ),
 ( 0.9401409369402312644, 0.9404761904761904656, 0.9464285714285713969, 0.9523809523809524391, 0.9527162059169116404 ),
 .UNSPECIFIED. ) 
 CURVE ( )  GEOMETRIC_REPRESENTATION_ITEM ( )  RATIONAL_B_SPLINE_CURVE ( ( 0.9963778908391753841, 0.9980808541467917072, 1.000000000000000000, 0.9659258262890682012, 1.000000000000000000, 0.9659258262890682012, 1.000000000000000000, 0.9980808541467917072, 0.9963778908391753841 ) ) 
 REPRESENTATION_ITEM ( '' )  );
#4116 = CARTESIAN_POINT ( 'NONE',  ( 1.472469842513823179, 35.59226448433412315, -4.923371831947296329 ) ) ;
#4117 = CARTESIAN_POINT ( 'NONE',  ( -0.3689425029237881626, 57.42874883491397497, 10.36894250292379027 ) ) ;
#4118 = ORIENTED_EDGE ( 'NONE', *, *, #43513, .T. ) ;
#4119 = EDGE_CURVE ( 'NONE', #86711, #69773, #25442, .T. ) ;
#4120 = CARTESIAN_POINT ( 'NONE',  ( 20.36894250292379382, 58.67874883491396076, 10.36894250292379205 ) ) ;
#4121 = ORIENTED_EDGE ( 'NONE', *, *, #50935, .F. ) ;
#4122 = CARTESIAN_POINT ( 'NONE',  ( 0.5774900079438607392, 28.48035201082150891, 5.440088680355550821 ) ) ;
#4123 = CARTESIAN_POINT ( 'NONE',  ( 15.44008868035555793, 41.39701867748817676, -9.422509992056140149 ) ) ;
#4124 = CARTESIAN_POINT ( 'NONE',  ( 2.035157376598822676, 52.43868534415483396, -7.964842623401177768 ) ) ;
#4125 = CARTESIAN_POINT ( 'NONE',  ( 17.97673228209724883, 77.65180420275405027, -4.136168975609629150 ) ) ;
#4126 = CARTESIAN_POINT ( 'NONE',  ( 4.559911319644449179, 43.89701867748816966, 9.422509992056141925 ) ) ;
#4127 = CARTESIAN_POINT ( 'NONE',  ( 1.236172813752370869, 0.04922511925149002099, -14.70095156538450176 ) ) ;
#4128 = EDGE_CURVE ( 'NONE', #64978, #53779, #37980, .T. ) ;
#4130 = ORIENTED_EDGE ( 'NONE', *, *, #83673, .F. ) ;
#4129 = CARTESIAN_POINT ( 'NONE',  ( 9.997910040112534702, 15.00000000000000000, 10.50199004140724490 ) ) ;
#4131 = VECTOR ( 'NONE', #74732, 1000.000000000000000 ) ;
#4132 = CARTESIAN_POINT ( 'NONE',  ( 19.84674366389459266, 18.30059781766745175, 2.638427012816836559 ) ) ;
#4133 = ORIENTED_EDGE ( 'NONE', *, *, #15488, .F. ) ;
#4134 = CARTESIAN_POINT ( 'NONE',  ( 10.88666287862788273, -94.01511732728891957, 4.000000000000000000 ) ) ;
#4135 = CARTESIAN_POINT ( 'NONE',  ( 1.472469842513823179, 61.42559781766745175, 4.923371831947296329 ) ) ;
#4136 = DIRECTION ( 'NONE',  ( 0.000000000000000000, 0.000000000000000000, 1.000000000000000000 ) ) ;
#4137 = CARTESIAN_POINT ( 'NONE',  ( 22.81628187352647785, 61.41530133659709634, 3.434112377981063169 ) ) ;
#4138 = DIRECTION ( 'NONE',  ( 0.000000000000000000, 0.000000000000000000, 1.000000000000000000 ) ) ;
#4139 = DIRECTION ( 'NONE',  ( 0.6246950475544238435, 0.7808688094430307203, 0.000000000000000000 ) ) ;
#4140 = CARTESIAN_POINT ( 'NONE',  ( 11.10000000000000142, 98.49999999999998579, 8.000000000000000000 ) ) ;
#4141 = CARTESIAN_POINT ( 'NONE',  ( -3.420591144908373682, 0.3639311400139669250, -14.60477854057963931 ) ) ;
#4142 = CARTESIAN_POINT ( 'NONE',  ( 17.08211943468705130, 63.47041550158063927, 12.26659068614894998 ) ) ;
#4143 = CARTESIAN_POINT ( 'NONE',  ( 0.000000000000000000, -97.00000000000000000, -4.000000000000000000 ) ) ;
#4144 = VERTEX_POINT ( 'NONE', #489 ) ;
#4145 = DIRECTION ( 'NONE',  ( -1.049065152435176504E-16, 1.000000000000000000, 0.000000000000000000 ) ) ;
#4146 = CARTESIAN_POINT ( 'NONE',  ( 19.84674366389459266, 33.30059781766744464, 2.638427012816836559 ) ) ;
#4147 = CARTESIAN_POINT ( 'NONE',  ( 19.38216949554541557, 62.24863466993041072, -9.382169495545420901 ) ) ;
#4148 = CARTESIAN_POINT ( 'NONE',  ( -1.099225684535947600, -0.4596986634029132657, 6.408140936763237150 ) ) ;
#4149 = CARTESIAN_POINT ( 'NONE',  ( 17.96484262340118221, 61.18868534415482685, -7.964842623401177768 ) ) ;
#4150 = LINE ( 'NONE', #65111, #1075 ) ;
#4151 = CARTESIAN_POINT ( 'NONE',  ( 1.472469842513823179, 15.59226448433411960, -4.923371831947296329 ) ) ;
#4152 = CARTESIAN_POINT ( 'NONE',  ( 0.1532563361054083140, 61.00893115100078745, 1.131784320476157264E-15 ) ) ;
#4153 = FACE_OUTER_BOUND ( 'NONE', #9824, .T. ) ;
#4154 = ORIENTED_EDGE ( 'NONE', *, *, #35093, .F. ) ;
#4155 = CARTESIAN_POINT ( 'NONE',  ( 12.91533473730993009, 16.60535201082150891, -10.88017736071109987 ) ) ;
#4156 = CARTESIAN_POINT ( 'NONE',  ( 0.1532563361054082862, 11.21726448433411605, 2.638427012816831674 ) ) ;
#4157 = CARTESIAN_POINT ( 'NONE',  ( 10.00000000000000000, 36.81368534415484106, -10.88017736071110342 ) ) ;
#4159 = CARTESIAN_POINT ( 'NONE',  ( 10.90209973789213116, 12.73026364691592072, -3.659052390917571174 ) ) ;
#4158 = CARTESIAN_POINT ( 'NONE',  ( 22.81628187352647785, 31.41530133659709279, 3.434112377981063169 ) ) ;
#4160 =( NAMED_UNIT ( * ) PLANE_ANGLE_UNIT ( ) SI_UNIT ( $, .RADIAN. ) );
#4161 = CARTESIAN_POINT ( 'NONE',  ( -0.2418659066527703572, 58.09014588040358262, 6.114288769123046308 ) ) ;
#4162 = CARTESIAN_POINT ( 'NONE',  ( 1.472469842513823179, 50.59226448433411605, -4.923371831947296329 ) ) ;
#4163 = CARTESIAN_POINT ( 'NONE',  ( 7.361572987183170547, 17.05059781766745530, 9.846743663894590881 ) ) ;
#4164 = CARTESIAN_POINT ( 'NONE',  ( 2.915334737309928315, -20.47798132251182679, 10.88017736071109987 ) ) ;
#4165 = CARTESIAN_POINT ( 'NONE',  ( 6.565887622018943937, 20.16530133659708213, 12.81628187352647430 ) ) ;
#4166 = FACE_OUTER_BOUND ( 'NONE', #50419, .T. ) ;
#4168 = CARTESIAN_POINT ( 'NONE',  ( -6.767445849361341637, 14.49999999999999112, 13.38662304974498873 ) ) ;
#4167 = CARTESIAN_POINT ( 'NONE',  ( 17.96484262340118221, 26.18868534415483396, -7.964842623401177768 ) ) ;
#4169 = CARTESIAN_POINT ( 'NONE',  ( 7.684764310694791156, 0.5000000000000004441, 12.88194075009940498 ) ) ;
#4170 = EDGE_CURVE ( 'NONE', #3546, #61160, #15953, .T. ) ;
#4171 = CARTESIAN_POINT ( 'NONE',  ( 13.79529636645030344, 48.26208216824728936, 14.16423886937410614 ) ) ;
#4172 = DIRECTION ( 'NONE',  ( 0.000000000000000000, 1.000000000000000000, 0.000000000000000000 ) ) ;
#4173 = CARTESIAN_POINT ( 'NONE',  ( 12.63842701281683922, 39.55059781766744464, -9.846743663894590881 ) ) ;
#4174 = CARTESIAN_POINT ( 'NONE',  ( 21.09922568453595559, 32.04030133659708923, -6.408140936763230044 ) ) ;
#4175 = CARTESIAN_POINT ( 'NONE',  ( 17.96484262340118221, 31.18868534415483751, -7.964842623401177768 ) ) ;
#4176 = CARTESIAN_POINT ( 'NONE',  ( 2.791683348922237240, 50.38393115100078035, -7.208316651077763204 ) ) ;
#4177 = CARTESIAN_POINT ( 'NONE',  ( -0.8801773607111009756, 43.06368534415484106, 1.068504757029289695E-15 ) ) ;
#4178 = CARTESIAN_POINT ( 'NONE',  ( 22.81628187352647785, 11.62363466993042138, 6.195893100308588602E-16 ) ) ;
#4179 = CARTESIAN_POINT ( 'NONE',  ( 2.917880565312950480, 35.97041550158063217, -12.26659068614894821 ) ) ;
#4180 = CARTESIAN_POINT ( 'NONE',  ( 0.000000000000000000, 14.49999999999999822, 0.000000000000000000 ) ) ;
#4181 = AXIS2_PLACEMENT_3D ( 'NONE', #14712, #75685, #30172 ) ;
#4182 = UNCERTAINTY_MEASURE_WITH_UNIT (LENGTH_MEASURE( 1.000000000000000082E-05 ), #71788, 'distance_accuracy_value', 'NONE');
#4183 = CARTESIAN_POINT ( 'NONE',  ( 5.076628168052704559, 25.17559781766745175, -8.527530157486179263 ) ) ;
#4184 = CARTESIAN_POINT ( 'NONE',  ( 6.565887622018943937, 58.08196800326376064, -12.81628187352647608 ) ) ;
#4185 = CARTESIAN_POINT ( 'NONE',  ( 5.076628168052703671, 61.84226448433412315, 8.527530157486179263 ) ) ;
#4186 = ORIENTED_EDGE ( 'NONE', *, *, #89747, .T. ) ;
#4187 = CARTESIAN_POINT ( 'NONE',  ( 20.15039907845753575, 7.627771745786129820, -6.262539305110077059 ) ) ;
#4188 = CARTESIAN_POINT ( 'NONE',  ( 5.510795456469524289, -25.29786701974074603, 3.750000000000001776 ) ) ;
#4189 = CARTESIAN_POINT ( 'NONE',  ( -0.8801773607111008646, 8.272018677488171434, 2.915334737309923430 ) ) ;
#4190 = CARTESIAN_POINT ( 'NONE',  ( 20.88017736071110519, 60.56368534415484106, 2.639326808657452039E-16 ) ) ;
#4191 = CARTESIAN_POINT ( 'NONE',  ( 2.917880565312950480, 30.97041550158063572, -12.26659068614894821 ) ) ;
#4192 = CARTESIAN_POINT ( 'NONE',  ( 0.1532563361054082862, 6.217264484334118713, 2.638427012816831674 ) ) ;
#4193 = CARTESIAN_POINT ( 'NONE',  ( 18.52753015748618282, 53.92559781766745175, -4.923371831947291888 ) ) ;
#4194 = CARTESIAN_POINT ( 'NONE',  ( 0.5774900079438607392, 38.48035201082150536, 5.440088680355550821 ) ) ;
#4195 = LINE ( 'NONE', #20166, #16040 ) ;
#4196 = CARTESIAN_POINT ( 'NONE',  ( -43.49126349454923712, 106.3716649516064479, -5.070890430955789618 ) ) ;
#4197 = EDGE_CURVE ( 'NONE', #61531, #89575, #68957, .T. ) ;
#4198 = EDGE_LOOP ( 'NONE', ( #31507, #60425, #30575, #60085, #77162, #13104 ) ) ;
#4199 = CARTESIAN_POINT ( 'NONE',  ( -4.862001128006591344, 4.779775600002961917E-16, -13.66056166602466604 ) ) ;
#4201 = ORIENTED_EDGE ( 'NONE', *, *, #92578, .T. ) ;
#4200 = ADVANCED_FACE ( 'NONE', ( #30938 ), #97316, .T. ) ;
#4202 = ORIENTED_EDGE ( 'NONE', *, *, #72345, .T. ) ;
#4203 = CARTESIAN_POINT ( 'NONE',  ( 0.000000000000000000, 0.5000000000000004441, 0.000000000000000000 ) ) ;
#4204 = CARTESIAN_POINT ( 'NONE',  ( 13.79529636645030344, 3.262082168247301350, 14.16423886937410614 ) ) ;
#4205 = CARTESIAN_POINT ( 'NONE',  ( 13.79529636645031943, 15.34541550158063750, -14.16423886937409904 ) ) ;
#4206 = CARTESIAN_POINT ( 'NONE',  ( 4.559911319644449179, 47.23035201082150536, -9.422509992056141925 ) ) ;
#4207 = CARTESIAN_POINT ( 'NONE',  ( 6.204703633549690345, 60.76208216824730357, -14.16423886937410259 ) ) ;
#4208 = CARTESIAN_POINT ( 'NONE',  ( 7.361572987183169658, 59.96726448433410894, -9.846743663894592657 ) ) ;
#4209 = CARTESIAN_POINT ( 'NONE',  ( 18.52753015748618282, 33.92559781766745886, -4.923371831947291888 ) ) ;
#4210 = DIRECTION ( 'NONE',  ( 0.000000000000000000, 0.000000000000000000, -1.000000000000000000 ) ) ;
#4212 = CARTESIAN_POINT ( 'NONE',  ( 5.076628168052703671, 56.84226448433412315, 8.527530157486179263 ) ) ;
#4211 = CARTESIAN_POINT ( 'NONE',  ( 17.96484262340118221, 36.18868534415484106, -7.964842623401177768 ) ) ;
#4213 =( NAMED_UNIT ( * ) SI_UNIT ( $, .STERADIAN. ) SOLID_ANGLE_UNIT ( ) );
#4214 = CARTESIAN_POINT ( 'NONE',  ( 2.917880565312948704, 47.63708216824730357, 12.26659068614894643 ) ) ;
#4215 = EDGE_CURVE ( 'NONE', #90918, #14329, #66068, .T. ) ;
#4216 = CARTESIAN_POINT ( 'NONE',  ( 10.00000000000000178, 4.313685344154837509, 10.88017736071110342 ) ) ;
#4217 = CARTESIAN_POINT ( 'NONE',  ( 17.39651004071838969, 39.08210964143329846, -6.500000000000027534 ) ) ;
#4218 = DIRECTION ( 'NONE',  ( 0.000000000000000000, 1.000000000000000000, 0.000000000000000000 ) ) ;
#4219 = CARTESIAN_POINT ( 'NONE',  ( -2.638427012816840111, -40.03273551566587685, -9.846743663894590881 ) ) ;
#4220 = ORIENTED_EDGE ( 'NONE', *, *, #79658, .F. ) ;
#4221 = CARTESIAN_POINT ( 'NONE',  ( -7.551349515323020789, -0.03417435944610275333, -12.08468537022916323 ) ) ;
#4222 = ORIENTED_EDGE ( 'NONE', *, *, #59994, .F. ) ;
#4223 = CARTESIAN_POINT ( 'NONE',  ( 17.20831665107776587, 24.13393115100078035, -7.208316651077762316 ) ) ;
#4224 = ORIENTED_EDGE ( 'NONE', *, *, #3545, .F. ) ;
#4225 = VECTOR ( 'NONE', #90119, 1000.000000000000000 ) ;
#4226 = CARTESIAN_POINT ( 'NONE',  ( 24.16423886937410614, 39.51208216824731068, -3.795296366450302550 ) ) ;
#4227 = CARTESIAN_POINT ( 'NONE',  ( 0.1532563361054082862, 31.21726448433412315, 2.638427012816831674 ) ) ;
#4228 = CARTESIAN_POINT ( 'NONE',  ( 12.91533473730993009, 61.60535201082150536, -10.88017736071109987 ) ) ;
#4229 = CARTESIAN_POINT ( 'NONE',  ( 19.88701968852527102, 36.79427333184084858, 6.480634945678612091 ) ) ;
#4230 = CARTESIAN_POINT ( 'NONE',  ( 15.44008868035555793, 56.39701867748817676, -9.422509992056140149 ) ) ;
#4231 = EDGE_CURVE ( 'NONE', #90354, #87694, #86076, .T. ) ;
#4232 = CARTESIAN_POINT ( 'NONE',  ( 6.408140936763243367, 10.79030133659709279, 11.09922568453594494 ) ) ;
#4233 = ORIENTED_EDGE ( 'NONE', *, *, #87033, .T. ) ;
#4234 = CARTESIAN_POINT ( 'NONE',  ( 10.00000000000000178, 49.31368534415484106, 10.88017736071110342 ) ) ;
#4235 = CARTESIAN_POINT ( 'NONE',  ( -2.266590686148945544, 17.22041550158063572, 7.082119434687048631 ) ) ;
#4236 = EDGE_CURVE ( 'NONE', #98371, #507, #24760, .T. ) ;
#4237 = ORIENTED_EDGE ( 'NONE', *, *, #53624, .T. ) ;
#4238 = CARTESIAN_POINT ( 'NONE',  ( -2.816281873526471635, 48.91530133659708213, -3.434112377981056508 ) ) ;
#4239 = CARTESIAN_POINT ( 'NONE',  ( 19.42250999205614193, 20.14701867748817321, 5.440088680355555262 ) ) ;
#4240 = CARTESIAN_POINT ( 'NONE',  ( 7.361572987183170547, 22.05059781766745530, 9.846743663894590881 ) ) ;
#4241 = CARTESIAN_POINT ( 'NONE',  ( 7.084665262690076126, 19.10535201082150181, 10.88017736071109987 ) ) ;
#4242 = CARTESIAN_POINT ( 'NONE',  ( 0.6178305044545818747, 48.49863466993042493, -9.382169495545419124 ) ) ;
#4243 = LINE ( 'NONE', #27213, #33587 ) ;
#4244 = CARTESIAN_POINT ( 'NONE',  ( 0.1532563361054100626, 35.80059781766745175, -2.638427012816831230 ) ) ;
#4245 = EDGE_CURVE ( 'NONE', #48019, #20819, #7882, .T. ) ;
#4246 = FACE_OUTER_BOUND ( 'NONE', #85101, .T. ) ;
#4247 = DIRECTION ( 'NONE',  ( 1.000000000000000000, 0.000000000000000000, 0.000000000000000000 ) ) ;
#4248 = CARTESIAN_POINT ( 'NONE',  ( -3.750000000000000000, 9.750000000000000000, -4.000000000000000000 ) ) ;
#4249 = B_SPLINE_SURFACE_WITH_KNOTS ( 'NONE', 3, 1, ( 
 ( #17669, #84198 ),
 ( #69192, #48142 ),
 ( #31170, #78656 ),
 ( #40659, #62151 ),
 ( #64115, #11132 ),
 ( #58091, #57115 ),
 ( #19123, #41651 ),
 ( #4632, #18641 ),
 ( #42614, #96121 ),
 ( #48632, #57605 ),
 ( #12601, #5116 ),
 ( #26620, #79135 ),
 ( #49604, #71645 ),
 ( #88106, #11621 ),
 ( #19614, #26141 ),
 ( #50109, #41160 ),
 ( #80619, #12113 ),
 ( #35602, #27604 ) ),
 .UNSPECIFIED., .F., .F., .F.,
 ( 4, 2, 2, 2, 2, 2, 2, 2, 4 ),
 ( 2, 2 ),
 ( 0.000000000000000000, 0.06249999999999988898, 0.1249999999999998890, 0.2499999999999997780, 0.4999999999999994449, 0.5624999999999994449, 0.6249999999999994449, 0.7499999999999995559, 0.8570805329376185444 ),
 ( 0.000000000000000000, 1.000000000000000000 ),
 .UNSPECIFIED. ) ;
#4250 = AXIS2_PLACEMENT_3D ( 'NONE', #22093, #75074, #61052 ) ;
#4251 = CARTESIAN_POINT ( 'NONE',  ( -0.3289641300568005855, 44.27164270246084499, -5.963430220938281678 ) ) ;
#4252 = CARTESIAN_POINT ( 'NONE',  ( 10.00000000000000000, -0.2410688489992152128, -9.846743663894594434 ) ) ;
#4253 = CARTESIAN_POINT ( 'NONE',  ( 16.40814093676324603, 27.45696800326375708, -11.09922568453594671 ) ) ;
#4254 = FILL_AREA_STYLE ('',( #96741 ) ) ;
#4255 = CARTESIAN_POINT ( 'NONE',  ( 2.791683348922237240, 45.38393115100079456, -7.208316651077763204 ) ) ;
#4256 = LINE ( 'NONE', #82208, #74544 ) ;
#4257 = CARTESIAN_POINT ( 'NONE',  ( 13.79529636645030344, 18.26208216824730002, 14.16423886937410614 ) ) ;
#4258 = CARTESIAN_POINT ( 'NONE',  ( 2.791683348922240793, 26.63393115100078745, 7.208316651077764092 ) ) ;
#4259 = CARTESIAN_POINT ( 'NONE',  ( -1.099225684535947600, 38.70696800326375353, -6.408140936763238038 ) ) ;
#4261 = CARTESIAN_POINT ( 'NONE',  ( 19.72487221294570858, 70.00000000000000000, 6.000000000000000000 ) ) ;
#4260 = DIRECTION ( 'NONE',  ( 0.000000000000000000, 0.000000000000000000, 1.000000000000000000 ) ) ;
#4262 = CARTESIAN_POINT ( 'NONE',  ( 7.084665262690076126, 69.10535201082151957, 10.88017736071109987 ) ) ;
#4263 = CARTESIAN_POINT ( 'NONE',  ( -2.816281873526471635, 3.915301336597087456, -3.434112377981056508 ) ) ;
#4264 = CARTESIAN_POINT ( 'NONE',  ( 2.791683348922237240, 30.38393115100078390, -7.208316651077763204 ) ) ;
#4265 = CARTESIAN_POINT ( 'NONE',  ( 12.91533473730993009, 21.60535201082150536, -10.88017736071109987 ) ) ;
#4266 = CARTESIAN_POINT ( 'NONE',  ( 21.09922568453595559, 32.04030133659708923, -6.408140936763230044 ) ) ;
#4267 = VECTOR ( 'NONE', #45715, 1000.000000000000114 ) ;
#4268 = COLOUR_RGB ( '', 0.66274510, 0.83137255, 0.94901961) ;
#4269 =( NAMED_UNIT ( * ) PLANE_ANGLE_UNIT ( ) SI_UNIT ( $, .RADIAN. ) );
#4270 = CARTESIAN_POINT ( 'NONE',  ( -13.83909701985790974, 90.94176541299273708, 7.900788997805663350 ) ) ;
#4271 = CARTESIAN_POINT ( 'NONE',  ( 7.084665262690076126, 34.10535201082151247, 10.88017736071109987 ) ) ;
#4272 = ORIENTED_EDGE ( 'NONE', *, *, #60871, .F. ) ;
#4273 = CARTESIAN_POINT ( 'NONE',  ( -11.25000000000000178, 2.921802177851545945, 3.951965214266261022E-15 ) ) ;
#4274 = LINE ( 'NONE', #19264, #7402 ) ;
#4276 = CARTESIAN_POINT ( 'NONE',  ( 19.42250999205614193, 35.14701867748816966, 5.440088680355555262 ) ) ;
#4275 = CARTESIAN_POINT ( 'NONE',  ( 17.20831665107776587, 59.13393115100078745, -7.208316651077762316 ) ) ;
#4277 = DIRECTION ( 'NONE',  ( 0.000000000000000000, 1.000000000000000000, 0.000000000000000000 ) ) ;
#4278 = CARTESIAN_POINT ( 'NONE',  ( 0.5774900079438590739, 62.64701867748817676, -5.440088680355550821 ) ) ;
#4280 = DIRECTION ( 'NONE',  ( 0.000000000000000000, 1.000000000000000000, 0.000000000000000000 ) ) ;
#4279 = CARTESIAN_POINT ( 'NONE',  ( 7.084665262690076126, 27.02201867748817676, -10.88017736071110164 ) ) ;
#4281 = CARTESIAN_POINT ( 'NONE',  ( 12.63842701281683034, 2.467264484334118269, 9.846743663894596210 ) ) ;
#4282 = DIRECTION ( 'NONE',  ( -0.000000000000000000, -0.000000000000000000, 1.000000000000000000 ) ) ;
#4283 = CARTESIAN_POINT ( 'NONE',  ( 19.84674366389459266, 53.30059781766744464, 2.638427012816836559 ) ) ;
#4285 = CYLINDRICAL_SURFACE ( 'NONE', #66457, 3.000000000000000888 ) ;
#4284 = CARTESIAN_POINT ( 'NONE',  ( 24.16423886937410614, 49.30374883491396787, 8.672049930838204340E-16 ) ) ;
#4286 = FILL_AREA_STYLE ('',( #36253 ) ) ;
#4287 = EDGE_CURVE ( 'NONE', #94783, #87107, #77936, .T. ) ;
#4288 = CARTESIAN_POINT ( 'NONE',  ( 24.16423886937410614, 14.51208216824730179, -3.795296366450302550 ) ) ;
#4289 = CARTESIAN_POINT ( 'NONE',  ( 22.26659068614894466, 38.88708216824731068, 7.082119434687054849 ) ) ;
#4290 = VECTOR ( 'NONE', #80103, 1000.000000000000227 ) ;
#4291 = CARTESIAN_POINT ( 'NONE',  ( 19.38216949554541202, 10.99863466993042138, 9.382169495545424454 ) ) ;
#4292 = CARTESIAN_POINT ( 'NONE',  ( -5.329507111614364412, -28.66964109972052199, 2.750000000000000444 ) ) ;
#4293 = ORIENTED_EDGE ( 'NONE', *, *, #65811, .F. ) ;
#4294 = CARTESIAN_POINT ( 'NONE',  ( -4.164238869374099927, 67.01208216824728936, 3.795296366450308767 ) ) ;
#4295 = CARTESIAN_POINT ( 'NONE',  ( 12.63842701281683034, 37.46726448433411605, 9.846743663894596210 ) ) ;
#4297 = CARTESIAN_POINT ( 'NONE',  ( -12.80781515976318907, 0.000000000000000000, 6.246788841744232990 ) ) ;
#4296 = DIRECTION ( 'NONE',  ( 1.000000000000000000, -5.818595309480553908E-17, 0.000000000000000000 ) ) ;
#4298 = CARTESIAN_POINT ( 'NONE',  ( 10.00000000000000178, 59.31368534415484106, 10.88017736071110342 ) ) ;
#4299 = LINE ( 'NONE', #34773, #71110 ) ;
#4300 = STYLED_ITEM ( 'NONE', ( #86456 ), #29558 ) ;
#4301 = CARTESIAN_POINT ( 'NONE',  ( -2.816281873526471635, 63.91530133659708923, -3.434112377981056508 ) ) ;
#4302 = CARTESIAN_POINT ( 'NONE',  ( 6.565887622018943937, 30.16530133659708568, 12.81628187352647430 ) ) ;
#4303 = CARTESIAN_POINT ( 'NONE',  ( 0.1532563361054082862, 26.21726448433411605, 2.638427012816831674 ) ) ;
#4304 = ORIENTED_EDGE ( 'NONE', *, *, #93124, .F. ) ;
#4305 = DIRECTION ( 'NONE',  ( 0.000000000000000000, 0.000000000000000000, 1.000000000000000000 ) ) ;
#4306 = CARTESIAN_POINT ( 'NONE',  ( 0.000000000000000000, 0.000000000000000000, -14.25000000000000000 ) ) ;
#4307 = CARTESIAN_POINT ( 'NONE',  ( 10.00000000000000000, 1.813685344154838175, -10.88017736071110342 ) ) ;
#4308 = CARTESIAN_POINT ( 'NONE',  ( 24.16423886937410614, 34.51208216824731068, -3.795296366450302550 ) ) ;
#4309 = CARTESIAN_POINT ( 'NONE',  ( 0.5774900079438590739, 27.64701867748817676, -5.440088680355550821 ) ) ;
#4310 = CARTESIAN_POINT ( 'NONE',  ( 10.00000000000000178, 49.31368534415484106, 10.88017736071110342 ) ) ;
#4311 = CARTESIAN_POINT ( 'NONE',  ( -11.62719953690051788, 15.00000000000000000, -9.476720473301954328 ) ) ;
#4312 = CARTESIAN_POINT ( 'NONE',  ( 8.959589291341636397, -9.312544548371912256, -4.000000000000000000 ) ) ;
#4313 = CARTESIAN_POINT ( 'NONE',  ( 14.92337183194729988, 14.34226448433411782, -8.527530157486177487 ) ) ;
#4314 =( NAMED_UNIT ( * ) PLANE_ANGLE_UNIT ( ) SI_UNIT ( $, .RADIAN. ) );
#4315 = FACE_OUTER_BOUND ( 'NONE', #2899, .T. ) ;
#4316 = CARTESIAN_POINT ( 'NONE',  ( 2.791683348922237240, 40.38393115100078035, -7.208316651077763204 ) ) ;
#4317 = CARTESIAN_POINT ( 'NONE',  ( 0.1532563361054100626, 50.80059781766745175, -2.638427012816831230 ) ) ;
#4318 = CARTESIAN_POINT ( 'NONE',  ( 2.035157376598824452, 23.68868534415484461, 7.964842623401179544 ) ) ;
#4319 = UNCERTAINTY_MEASURE_WITH_UNIT (LENGTH_MEASURE( 1.000000000000000082E-05 ), #64257, 'distance_accuracy_value', 'NONE');
#4320 =( BOUNDED_CURVE ( )  B_SPLINE_CURVE ( 2, ( #86993, #57474, #27466, #49974, #42481, #26482, #34960, #18500, #65458 ),
 .UNSPECIFIED., .F., .T. ) 
 B_SPLINE_CURVE_WITH_KNOTS ( ( 3, 2, 2, 2, 3 ),
 ( 0.7258552226545170738, 0.7261904761904762751, 0.7321428571428572063, 0.7380952380952381375, 0.7384304916311973388 ),
 .UNSPECIFIED. ) 
 CURVE ( )  GEOMETRIC_REPRESENTATION_ITEM ( )  RATIONAL_B_SPLINE_CURVE ( ( 0.9963778908391753841, 0.9980808541467917072, 1.000000000000000000, 0.9659258262890683122, 1.000000000000000000, 0.9659258262890683122, 1.000000000000000000, 0.9980808541467917072, 0.9963778908391753841 ) ) 
 REPRESENTATION_ITEM ( '' )  );
#4321 = ADVANCED_FACE ( 'NONE', ( #44348 ), #65368, .T. ) ;
#4322 = VERTEX_POINT ( 'NONE', #12378 ) ;
#4323 = CARTESIAN_POINT ( 'NONE',  ( 22.81628187352648496, 51.83196800326376064, -3.434112377981050290 ) ) ;
#4324 = DIRECTION ( 'NONE',  ( 0.000000000000000000, 0.000000000000000000, 1.000000000000000000 ) ) ;
#4325 = CARTESIAN_POINT ( 'NONE',  ( 4.559911319644449179, 68.89701867748817676, 9.422509992056141925 ) ) ;
#4326 = CARTESIAN_POINT ( 'NONE',  ( 1.472469842513823179, 25.59226448433412315, -4.923371831947296329 ) ) ;
#4328 = CARTESIAN_POINT ( 'NONE',  ( 14.92337183194729633, 17.67559781766745175, 8.527530157486181039 ) ) ;
#4327 = CARTESIAN_POINT ( 'NONE',  ( 10.00000000000000178, 63.05374883491396076, 14.16423886937410082 ) ) ;
#4329 = CARTESIAN_POINT ( 'NONE',  ( 0.000000000000000000, -97.00000000000000000, 2.500000000000000000 ) ) ;
#4330 = CIRCLE ( 'NONE', #17105, 0.2500000000000002220 ) ;
#4331 = DIRECTION ( 'NONE',  ( 0.000000000000000000, 1.000000000000000000, 0.000000000000000000 ) ) ;
#4332 = CARTESIAN_POINT ( 'NONE',  ( 20.36894250292379382, 23.67874883491397142, 10.36894250292379205 ) ) ;
#4333 = EDGE_CURVE ( 'NONE', #7776, #62748, #65865, .T. ) ;
#4334 = CARTESIAN_POINT ( 'NONE',  ( 17.08211943468705130, 33.47041550158063927, 12.26659068614894998 ) ) ;
#4335 = CARTESIAN_POINT ( 'NONE',  ( 19.84674366389459266, 43.71726448433410894, -2.638427012816827677 ) ) ;
#4336 = DIRECTION ( 'NONE',  ( 0.000000000000000000, 0.000000000000000000, 1.000000000000000000 ) ) ;
#4337 = CARTESIAN_POINT ( 'NONE',  ( 15.44008868035555260, 29.73035201082150891, 9.422509992056143702 ) ) ;
#4338 = CARTESIAN_POINT ( 'NONE',  ( 12.91533473730993009, 56.60535201082151247, -10.88017736071109987 ) ) ;
#4339 = CARTESIAN_POINT ( 'NONE',  ( 14.17193700899789022, 15.00000000000000000, 1.489530601564113654 ) ) ;
#4340 = ORIENTED_EDGE ( 'NONE', *, *, #58179, .T. ) ;
#4341 = CARTESIAN_POINT ( 'NONE',  ( 22.81628187352647785, 51.62363466993042493, 6.195893100308588602E-16 ) ) ;
#4342 = PRODUCT_DEFINITION ( 'UNKNOWN', '', #18381, #74461 ) ;
#4343 = ORIENTED_EDGE ( 'NONE', *, *, #22957, .T. ) ;
#4344 = VECTOR ( 'NONE', #48493, 1000.000000000000000 ) ;
#4345 = CARTESIAN_POINT ( 'NONE',  ( 2.035157376598822676, 47.43868534415484817, -7.964842623401177768 ) ) ;
#4346 = EDGE_LOOP ( 'NONE', ( #80800, #84672, #36624, #58557 ) ) ;
#4347 = CARTESIAN_POINT ( 'NONE',  ( -9.383624259803923451, 14.76984980006450066, -11.62625599701892298 ) ) ;
#4348 = TOROIDAL_SURFACE ( 'NONE', #42655, 14.49999999999999822, 0.5000000000000000000 ) ;
#4349 = CARTESIAN_POINT ( 'NONE',  ( 2.347401019785370746, 0.3355287360789229734, -6.482960602445015041 ) ) ;
#4350 = VERTEX_POINT ( 'NONE', #89851 ) ;
#4351 = VECTOR ( 'NONE', #72548, 1000.000000000000000 ) ;
#4352 = CARTESIAN_POINT ( 'NONE',  ( 4.559911319644449179, 67.23035201082150536, -9.422509992056141925 ) ) ;
#4353 = CARTESIAN_POINT ( 'NONE',  ( 12.91533473730992121, 9.522018677488171434, 10.88017736071110164 ) ) ;
#4354 = CARTESIAN_POINT ( 'NONE',  ( -10.64017930668212664, 15.00000000000000000, 10.57291749337208309 ) ) ;
#4355 = DIRECTION ( 'NONE',  ( 0.000000000000000000, 1.000000000000000000, 0.000000000000000000 ) ) ;
#4356 = CARTESIAN_POINT ( 'NONE',  ( 20.88017736071110164, 5.355352010821503583, 2.915334737309930979 ) ) ;
#4357 = CARTESIAN_POINT ( 'NONE',  ( 2.791683348922240793, 6.633931151000785675, 7.208316651077764092 ) ) ;
#4358 = CARTESIAN_POINT ( 'NONE',  ( 17.08211943468705840, 15.13708216824730179, -12.26659068614894466 ) ) ;
#4359 = CARTESIAN_POINT ( 'NONE',  ( 2.035157376598824452, 28.68868534415484106, 7.964842623401179544 ) ) ;
#4360 = CARTESIAN_POINT ( 'NONE',  ( 2.791683348922237240, 60.38393115100078745, -7.208316651077763204 ) ) ;
#4361 = ORIENTED_EDGE ( 'NONE', *, *, #26104, .T. ) ;
#4362 = CARTESIAN_POINT ( 'NONE',  ( 12.63842701281683034, 62.46726448433410894, 9.846743663894596210 ) ) ;
#4363 = VERTEX_POINT ( 'NONE', #58352 ) ;
#4364 = DIRECTION ( 'NONE',  ( 0.000000000000000000, 0.000000000000000000, -1.000000000000000000 ) ) ;
#4365 = CARTESIAN_POINT ( 'NONE',  ( -0.8801773607111008646, 53.27201867748816966, 2.915334737309923430 ) ) ;
#4366 = CARTESIAN_POINT ( 'NONE',  ( 2.791683348922237240, 60.38393115100078745, -7.208316651077763204 ) ) ;
#4367 = CARTESIAN_POINT ( 'NONE',  ( 19.38216949554541557, 42.24863466993041783, -9.382169495545420901 ) ) ;
#4369 = CARTESIAN_POINT ( 'NONE',  ( -7.793944756043282851, 2.100340034815855628, -8.673230486701367425 ) ) ;
#4368 = CARTESIAN_POINT ( 'NONE',  ( 10.00000000000000000, 6.813685344154838397, -10.88017736071110342 ) ) ;
#4370 = CARTESIAN_POINT ( 'NONE',  ( 12.91533473730993009, 56.60535201082151247, -10.88017736071109987 ) ) ;
#4371 = CARTESIAN_POINT ( 'NONE',  ( 17.96484262340118221, 6.188685344154837509, -7.964842623401177768 ) ) ;
#4372 = CARTESIAN_POINT ( 'NONE',  ( 21.09922568453595559, 47.04030133659708923, -6.408140936763230044 ) ) ;
#4373 = CARTESIAN_POINT ( 'NONE',  ( 19.42250999205614193, 25.14701867748817321, 5.440088680355555262 ) ) ;
#4374 = CARTESIAN_POINT ( 'NONE',  ( -46.94000000000002615, 100.7935499705929203, -8.437539667946047928 ) ) ;
#4375 = EDGE_LOOP ( 'NONE', ( #49231, #70006, #82050, #1924, #46258, #57177 ) ) ;
#4376 = CARTESIAN_POINT ( 'NONE',  ( 13.43411237798105340, 35.58196800326375353, 12.81628187352647963 ) ) ;
#4377 = CARTESIAN_POINT ( 'NONE',  ( 19.42250999205614548, 40.98035201082150536, -5.440088680355545492 ) ) ;
#4378 = CARTESIAN_POINT ( 'NONE',  ( 1.472469842513823179, 51.42559781766745886, 4.923371831947296329 ) ) ;
#4379 = VERTEX_POINT ( 'NONE', #49878 ) ;
#4380 = CARTESIAN_POINT ( 'NONE',  ( 10.00000000000000000, 59.75893115100078745, -9.846743663894594434 ) ) ;
#4382 = CARTESIAN_POINT ( 'NONE',  ( 1.472469842513823179, 50.59226448433411605, -4.923371831947296329 ) ) ;
#4381 = CARTESIAN_POINT ( 'NONE',  ( 11.96291822454875842, 4.834832779786913688E-16, 8.193813980849165901 ) ) ;
#4383 = CARTESIAN_POINT ( 'NONE',  ( -0.8801773607111008646, 23.27201867748817676, 2.915334737309923430 ) ) ;
#4384 = FILL_AREA_STYLE_COLOUR ( '', #53679 ) ;
#4385 = CARTESIAN_POINT ( 'NONE',  ( 19.84674366389459621, 33.50893115100078745, 7.409399052514197653E-17 ) ) ;
#4386 = DIRECTION ( 'NONE',  ( 1.000000000000000000, -5.818595309480553908E-17, 0.000000000000000000 ) ) ;
#4387 = DIRECTION ( 'NONE',  ( 0.000000000000000000, 0.000000000000000000, 1.000000000000000000 ) ) ;
#4388 = CARTESIAN_POINT ( 'NONE',  ( 7.361572987183170547, 47.05059781766745175, 9.846743663894590881 ) ) ;
#4389 =( LENGTH_UNIT ( ) NAMED_UNIT ( * ) SI_UNIT ( .MILLI., .METRE. ) );
#4391 = ORIENTED_EDGE ( 'NONE', *, *, #11802, .T. ) ;
#4390 = CARTESIAN_POINT ( 'NONE',  ( 17.20831665107776587, 52.88393115100078035, 7.208316651077764980 ) ) ;
#4392 =( BOUNDED_SURFACE ( )  B_SPLINE_SURFACE ( 1, 2, ( 
 ( #71327, #56320, #2846, #63792, #42788, #94300, #25823, #65265, #27275, #88279, #58763, #51269, #44254, #66258, #29739, #21270, #5780, #68263, #89267, #43759, #20778, #50779, #36270, #6266, #60735, #66764, #21777, #90742, #13267, #83252, #37276, #75250, #59749, #12771, #81753, #74248, #14274, #35770, #98783, #60249, #90246, #28761, #97287, #37766, #59253, #97790, #30231, #67765, #29253, #52744, #89753, #43267, #22270, #98284, #82251, #14774, #51767, #13766, #74758, #36771, #73762, #20282, #67263, #7265, #52256, #6762, #82752, #44747, #45247, #75743, #81271, #5293, #96793, #28268, #85227, #77219, #84733, #16730, #54216, #16239, #280, #46719, #62207, #23756, #8724, #39242, #92713, #69730, #91740, #47207, #38744, #1257, #77708, #24239, #92230, #8247, #31712, #94556, #54706, #61234, #9220, #61714, #69245, #766, #41082, #31219, #26074, #72051, #15757, #71580, #30727, #3091, #33547, #23261, #64043, #56565, #87059, #18568, #49061, #46242, #79566, #53736, #11064, #84255, #41584, #3580, #34037, #91237, #22760, #53242, #76728, #83747, #15270, #45751, #76247, #7763, #38256, #68748, #65021, #58520, #12042, #50534, #89028, #66022, #65524, #80545, #43036, #66523, #73517, #34525, #81029, #35023, #42541, #73025, #5045, #4560, #97050, #44008, #88033, #96047, #4064, #20538, #27531, #95549, #35528, #13022, #58023, #88531, #74510, #20033, #96548, #28524, #51522, #28023, #49536, #12535, #51022, #26549, #21032, #72530, #57044, #64533, #59016, #95040, #42069, #81516, #43519, #74014, #27037, #57536, #5543, #11549, #36020, #89522, #50041, #13525, #19546, #82014, #6031, #87547, #19058, #80044, #76978, #52502, #38014, #8005, #29490, #532, #53485, #91496, #75996, #29002, #6513, #75008, #30485, #52021, #84493, #46002, #7524, #44998, #98036, #53985, #83010, #15023, #46482, #83996, #45494, #68999, #60000, #59513, #38503, #15520, #98540, #30979, #37021, #7015, #90493, #75503, #90007, #36531, #37522, #23513, #83506, #23017, #90988, #22029, #14528, #61477, #76492, #15994, #91983, #67020, #97541, #68013, #82512, #21527, #29992, #14030, #44508, #67518, #60499, #22519, #52991, #68507, #37, #60984, #24491, #69981, #1504, #77462, #48937, #54955, #86941, #32949, #54469, #10459, #77964, #71466, #55469, #8974, #55965, #62455, #63449, #32459, #62955, #46968, #17963, #93460, #17482, #47948, #38995, #40476, #92470, #85473, #93956, #48450, #78948, #86466, #85972, #25481, #23996, #92957, #61970, #16984, #84974, #31468, #40969, #2493, #39490, #47462, #2979, #25952, #33428, #63925, #39972, #94440, #31953, #16492, #56455, #18453, #1994, #9470, #8491, #69488, #1006 ),
 ( #70474, #78457, #9971, #24986, #70973, #11435, #4447, #26430, #88915, #80432, #64907, #28409, #18947, #3944, #79927, #10945, #95432, #65409, #20917, #26926, #80922, #50909, #72418, #43404, #96433, #35410, #19920, #71937, #49424, #41954, #73402, #94929, #58903, #20423, #50412, #87917, #34416, #96933, #57423, #95934, #19433, #4930, #49921, #27416, #65902, #12415, #11930, #42434, #57908, #81405, #88419, #72917, #42922, #34912, #27905, #58396, #12907, #73901, #5434, #89401, #35904, #66401, #79445, #41469, #3460, #33915, #64422, #56930, #87431, #44877, #30866, #90374, #60376, #83878, #38385, #14905, #36405, #75379, #52877, #13404, #7891, #59389, #43889, #51406, #15405, #81893, #28884, #22402, #90873, #68391, #89890, #82387, #6896, #97418, #60870, #52389, #36903, #415, #21408, #74889, #51903, #74387, #67395, #37408, #91873, #97921, #83387, #22897, #44391, #45888, #98912, #7404, #45377, #5913, #13911, #6388, #75883, #66899, #61364, #91371, #37902, #59883, #29381, #68886, #21913, #29874, #82889, #30365, #53369, #76376, #14405, #67896, #98419, #2370, #85351, #93833, #92360, #92847, #77347, #31844, #15886, #23395, #24374, #10342, #70362, #9856, #77842, #8858, #9351, #39374, #39856, #61856, #93340, #16373, #17363, #1879, #16863, #47832, #47339, #32338, #31355, #62839, #24861, #54838, #55345, #85852, #78335, #71345, #46852, #62340, #69372, #40355, #70855, #53880, #69869, #84864, #1389, #23886, #63809, #32825, #2863, #63325, #893, #25359, #55845, #86340, #17843, #54352, #48328, #78832, #40842, #33314, #84387, #46371, #76860, #8373, #38880, #34796, #25840, #27292, #79325, #72301, #50287, #35288, #65781, #42807, #42312, #19796, #10835, #49309, #48815, #3830, #41354, #18335, #80801, #88298, #94811, #79810, #12298, #12786, #96314, #20300, #26807, #27787, #26314, #71823, #58273, #73290, #87793, #34287, #81290, #73780, #4814, #56813, #64786, #57302, #11314, #88792, #50800, #64301, #3332, #19311, #86831, #56338, #49796, #95303, #57791, #80305, #87311, #43286, #33794, #18830, #95812, #5310, #35787, #94319, #41833, #11804, #72786, #4323, #65285, #98800, #30248, #14792, #52272, #15286, #45265, #45768, #51287, #36787, #22778, #51782, #60263, #58782, #36286, #97303, #6779, #22286, #29270, #67778, #75759, #7280, #89772, #91252, #52760, #53257, #83763, #76261, #66275, #67281, #81772, #83268, #44269, #13286, #28287, #37782, #28775, #74775, #97809, #21289, #68279, #7778, #66784, #43774, #59764, #89287, #96811, #21792, #6284, #98300, #82770, #59273, #20798, #74266, #82267, #29755, #60751, #5795, #90762, #13783, #90258, #44763, #14291, #75268, #37292 ) ),
 .UNSPECIFIED., .F., .F., .F. ) 
 B_SPLINE_SURFACE_WITH_KNOTS ( ( 2, 2 ),
 ( 3, 2, 2, 2, 2, 2, 2, 2, 2, 2, 2, 2, 2, 2, 2, 2, 2, 2, 2, 2, 2, 2, 2, 2, 2, 2, 2, 2, 2, 2, 2, 2, 2, 2, 2, 2, 2, 2, 2, 2, 2, 2, 2, 2, 2, 2, 2, 2, 2, 2, 2, 2, 2, 2, 2, 2, 2, 2, 2, 2, 2, 2, 2, 2, 2, 2, 2, 2, 2, 2, 2, 2, 2, 2, 2, 2, 2, 2, 2, 2, 2, 2, 2, 2, 2, 2, 2, 2, 2, 2, 2, 2, 2, 2, 2, 2, 2, 2, 2, 2, 2, 2, 2, 2, 2, 2, 2, 2, 2, 2, 2, 2, 2, 2, 2, 2, 2, 2, 2, 2, 2, 2, 2, 2, 2, 2, 2, 2, 2, 2, 2, 2, 2, 2, 2, 2, 2, 2, 2, 2, 2, 2, 2, 2, 2, 2, 2, 2, 2, 2, 2, 2, 2, 2, 2, 2, 2, 2, 2, 2, 2, 2, 3 ),
 ( 0.000000000000000000, 1.000000000000000000 ),
 ( 0.000000000000000000, 0.005952380952380952051, 0.01190476190476190410, 0.01785714285714285615, 0.02380952380952380820, 0.02976190476190476025, 0.03571428571428571230, 0.04166666666666666435, 0.04761904761904761640, 0.05357142857142856845, 0.05952380952380952051, 0.06547619047619047949, 0.07142857142857142461, 0.07738095238095238360, 0.08333333333333332871, 0.08928571428571428770, 0.09523809523809523281, 0.1011904761904761918, 0.1071428571428571369, 0.1130952380952380959, 0.1190476190476190410, 0.1250000000000000000, 0.1309523809523809590, 0.1369047619047619180, 0.1428571428571428492, 0.1488095238095238082, 0.1547619047619047672, 0.1607142857142857262, 0.1666666666666666574, 0.1726190476190476164, 0.1785714285714285754, 0.1845238095238095344, 0.1904761904761904656, 0.1964285714285714246, 0.2023809523809523836, 0.2083333333333333426, 0.2142857142857142738, 0.2202380952380952328, 0.2261904761904761918, 0.2321428571428571508, 0.2380952380952380820, 0.2440476190476190410, 0.2500000000000000000, 0.2559523809523809312, 0.2619047619047619180, 0.2678571428571428492, 0.2738095238095238360, 0.2797619047619047672, 0.2857142857142856984, 0.2916666666666666852, 0.2976190476190476164, 0.3035714285714285476, 0.3095238095238095344, 0.3154761904761904656, 0.3214285714285714524, 0.3273809523809523836, 0.3333333333333333148, 0.3392857142857143016, 0.3452380952380952328, 0.3511904761904761640, 0.3571428571428571508, 0.3630952380952380820, 0.3690476190476190688, 0.3750000000000000000, 0.3809523809523809312, 0.3869047619047619180, 0.3928571428571428492, 0.3988095238095238360, 0.4047619047619047672, 0.4107142857142856984, 0.4166666666666666852, 0.4226190476190476164, 0.4285714285714285476, 0.4345238095238095344, 0.4404761904761904656, 0.4464285714285714524, 0.4523809523809523836, 0.4583333333333333148, 0.4642857142857143016, 0.4702380952380952328, 0.4761904761904761640, 0.4821428571428571508, 0.4880952380952380820, 0.4940476190476190688, 0.5000000000000000000, 0.5059523809523809312, 0.5119047619047618625, 0.5178571428571429047, 0.5238095238095238360, 0.5297619047619047672, 0.5357142857142856984, 0.5416666666666666297, 0.5476190476190476719, 0.5535714285714286031, 0.5595238095238095344, 0.5654761904761904656, 0.5714285714285713969, 0.5773809523809523281, 0.5833333333333333703, 0.5892857142857143016, 0.5952380952380952328, 0.6011904761904761640, 0.6071428571428570953, 0.6130952380952381375, 0.6190476190476190688, 0.6250000000000000000, 0.6309523809523809312, 0.6369047619047618625, 0.6428571428571429047, 0.6488095238095238360, 0.6547619047619047672, 0.6607142857142856984, 0.6666666666666666297, 0.6726190476190476719, 0.6785714285714286031, 0.6845238095238095344, 0.6904761904761904656, 0.6964285714285713969, 0.7023809523809523281, 0.7083333333333333703, 0.7142857142857143016, 0.7202380952380952328, 0.7261904761904761640, 0.7321428571428570953, 0.7380952380952381375, 0.7440476190476190688, 0.7500000000000000000, 0.7559523809523809312, 0.7619047619047618625, 0.7678571428571429047, 0.7738095238095238360, 0.7797619047619047672, 0.7857142857142856984, 0.7916666666666666297, 0.7976190476190476719, 0.8035714285714286031, 0.8095238095238095344, 0.8154761904761904656, 0.8214285714285713969, 0.8273809523809523281, 0.8333333333333333703, 0.8392857142857143016, 0.8452380952380952328, 0.8511904761904761640, 0.8571428571428570953, 0.8630952380952381375, 0.8690476190476190688, 0.8750000000000000000, 0.8809523809523809312, 0.8869047619047618625, 0.8928571428571429047, 0.8988095238095238360, 0.9047619047619047672, 0.9107142857142856984, 0.9166666666666666297, 0.9226190476190476719, 0.9285714285714286031, 0.9345238095238095344, 0.9404761904761904656, 0.9464285714285713969, 0.9523809523809523281, 0.9583333333333333703, 0.9642857142857143016 ),
 .UNSPECIFIED. ) 
 GEOMETRIC_REPRESENTATION_ITEM ( )  RATIONAL_B_SPLINE_SURFACE ( (
 ( 1.000000000000000000, 0.9659258262890683122, 1.000000000000000000, 0.9659258262890683122, 1.000000000000000000, 0.9659258262890683122, 1.000000000000000000, 0.9659258262890683122, 1.000000000000000000, 0.9659258262890683122, 1.000000000000000000, 0.9659258262890683122, 1.000000000000000000, 0.9659258262890683122, 1.000000000000000000, 0.9659258262890683122, 1.000000000000000000, 0.9659258262890683122, 1.000000000000000000, 0.9659258262890683122, 1.000000000000000000, 0.9659258262890683122, 1.000000000000000000, 0.9659258262890683122, 1.000000000000000000, 0.9659258262890683122, 1.000000000000000000, 0.9659258262890683122, 1.000000000000000000, 0.9659258262890683122, 1.000000000000000000, 0.9659258262890683122, 1.000000000000000000, 0.9659258262890683122, 1.000000000000000000, 0.9659258262890683122, 1.000000000000000000, 0.9659258262890683122, 1.000000000000000000, 0.9659258262890683122, 1.000000000000000000, 0.9659258262890683122, 1.000000000000000000, 0.9659258262890683122, 1.000000000000000000, 0.9659258262890683122, 1.000000000000000000, 0.9659258262890683122, 1.000000000000000000, 0.9659258262890683122, 1.000000000000000000, 0.9659258262890683122, 1.000000000000000000, 0.9659258262890683122, 1.000000000000000000, 0.9659258262890683122, 1.000000000000000000, 0.9659258262890683122, 1.000000000000000000, 0.9659258262890683122, 1.000000000000000000, 0.9659258262890683122, 1.000000000000000000, 0.9659258262890683122, 1.000000000000000000, 0.9659258262890683122, 1.000000000000000000, 0.9659258262890683122, 1.000000000000000000, 0.9659258262890683122, 1.000000000000000000, 0.9659258262890683122, 1.000000000000000000, 0.9659258262890683122, 1.000000000000000000, 0.9659258262890683122, 1.000000000000000000, 0.9659258262890683122, 1.000000000000000000, 0.9659258262890683122, 1.000000000000000000, 0.9659258262890683122, 1.000000000000000000, 0.9659258262890683122, 1.000000000000000000, 0.9659258262890683122, 1.000000000000000000, 0.9659258262890683122, 1.000000000000000000, 0.9659258262890683122, 1.000000000000000000, 0.9659258262890683122, 1.000000000000000000, 0.9659258262890683122, 1.000000000000000000, 0.9659258262890683122, 1.000000000000000000, 0.9659258262890683122, 1.000000000000000000, 0.9659258262890683122, 1.000000000000000000, 0.9659258262890683122, 1.000000000000000000, 0.9659258262890683122, 1.000000000000000000, 0.9659258262890683122, 1.000000000000000000, 0.9659258262890683122, 1.000000000000000000, 0.9659258262890683122, 1.000000000000000000, 0.9659258262890683122, 1.000000000000000000, 0.9659258262890683122, 1.000000000000000000, 0.9659258262890683122, 1.000000000000000000, 0.9659258262890683122, 1.000000000000000000, 0.9659258262890683122, 1.000000000000000000, 0.9659258262890683122, 1.000000000000000000, 0.9659258262890683122, 1.000000000000000000, 0.9659258262890683122, 1.000000000000000000, 0.9659258262890683122, 1.000000000000000000, 0.9659258262890683122, 1.000000000000000000, 0.9659258262890683122, 1.000000000000000000, 0.9659258262890683122, 1.000000000000000000, 0.9659258262890683122, 1.000000000000000000, 0.9659258262890683122, 1.000000000000000000, 0.9659258262890683122, 1.000000000000000000, 0.9659258262890683122, 1.000000000000000000, 0.9659258262890683122, 1.000000000000000000, 0.9659258262890683122, 1.000000000000000000, 0.9659258262890683122, 1.000000000000000000, 0.9659258262890683122, 1.000000000000000000, 0.9659258262890683122, 1.000000000000000000, 0.9659258262890683122, 1.000000000000000000, 0.9659258262890683122, 1.000000000000000000, 0.9659258262890683122, 1.000000000000000000, 0.9659258262890683122, 1.000000000000000000, 0.9659258262890683122, 1.000000000000000000, 0.9659258262890683122, 1.000000000000000000, 0.9659258262890683122, 1.000000000000000000, 0.9659258262890683122, 1.000000000000000000, 0.9659258262890683122, 1.000000000000000000, 0.9659258262890683122, 1.000000000000000000, 0.9659258262890683122, 1.000000000000000000, 0.9659258262890683122, 1.000000000000000000, 0.9659258262890683122, 1.000000000000000000, 0.9659258262890683122, 1.000000000000000000, 0.9659258262890683122, 1.000000000000000000, 0.9659258262890683122, 1.000000000000000000, 0.9659258262890683122, 1.000000000000000000, 0.9659258262890683122, 1.000000000000000000, 0.9659258262890683122, 1.000000000000000000, 0.9659258262890683122, 1.000000000000000000, 0.9659258262890683122, 1.000000000000000000, 0.9659258262890683122, 1.000000000000000000, 0.9659258262890683122, 1.000000000000000000, 0.9659258262890683122, 1.000000000000000000, 0.9659258262890683122, 1.000000000000000000, 0.9659258262890683122, 1.000000000000000000, 0.9659258262890683122, 1.000000000000000000, 0.9659258262890683122, 1.000000000000000000, 0.9659258262890683122, 1.000000000000000000, 0.9659258262890683122, 1.000000000000000000, 0.9659258262890683122, 1.000000000000000000, 0.9659258262890683122, 1.000000000000000000, 0.9659258262890683122, 1.000000000000000000, 0.9659258262890683122, 1.000000000000000000, 0.9659258262890683122, 1.000000000000000000, 0.9659258262890683122, 1.000000000000000000, 0.9659258262890683122, 1.000000000000000000, 0.9659258262890683122, 1.000000000000000000, 0.9659258262890683122, 1.000000000000000000, 0.9659258262890683122, 1.000000000000000000, 0.9659258262890683122, 1.000000000000000000, 0.9659258262890683122, 1.000000000000000000, 0.9659258262890683122, 1.000000000000000000, 0.9659258262890683122, 1.000000000000000000, 0.9659258262890683122, 1.000000000000000000, 0.9659258262890683122, 1.000000000000000000, 0.9659258262890683122, 1.000000000000000000, 0.9659258262890683122, 1.000000000000000000, 0.9659258262890683122, 1.000000000000000000, 0.9659258262890683122, 1.000000000000000000, 0.9659258262890683122, 1.000000000000000000, 0.9659258262890683122, 1.000000000000000000, 0.9659258262890683122, 1.000000000000000000, 0.9659258262890683122, 1.000000000000000000, 0.9659258262890683122, 1.000000000000000000, 0.9659258262890683122, 1.000000000000000000, 0.9659258262890683122, 1.000000000000000000, 0.9659258262890683122, 1.000000000000000000, 0.9659258262890683122, 1.000000000000000000, 0.9659258262890683122, 1.000000000000000000, 0.9659258262890683122, 1.000000000000000000, 0.9659258262890683122, 1.000000000000000000, 0.9659258262890683122, 1.000000000000000000, 0.9659258262890683122, 1.000000000000000000, 0.9659258262890683122, 1.000000000000000000, 0.9659258262890683122, 1.000000000000000000, 0.9659258262890683122, 1.000000000000000000, 0.9659258262890683122, 1.000000000000000000, 0.9659258262890683122, 1.000000000000000000, 0.9659258262890683122, 1.000000000000000000, 0.9659258262890683122, 1.000000000000000000, 0.9659258262890683122, 1.000000000000000000, 0.9659258262890683122, 1.000000000000000000, 0.9659258262890683122, 1.000000000000000000, 0.9659258262890683122, 1.000000000000000000, 0.9659258262890683122, 1.000000000000000000, 0.9659258262890683122, 1.000000000000000000, 0.9659258262890683122, 1.000000000000000000, 0.9659258262890683122, 1.000000000000000000, 0.9659258262890683122, 1.000000000000000000, 0.9659258262890683122, 1.000000000000000000, 0.9659258262890683122, 1.000000000000000000, 0.9659258262890683122, 1.000000000000000000, 0.9659258262890683122, 1.000000000000000000, 0.9659258262890683122, 1.000000000000000000, 0.9659258262890683122, 1.000000000000000000),
 ( 1.000000000000000000, 0.9659258262890683122, 1.000000000000000000, 0.9659258262890683122, 1.000000000000000000, 0.9659258262890683122, 1.000000000000000000, 0.9659258262890683122, 1.000000000000000000, 0.9659258262890683122, 1.000000000000000000, 0.9659258262890683122, 1.000000000000000000, 0.9659258262890683122, 1.000000000000000000, 0.9659258262890683122, 1.000000000000000000, 0.9659258262890683122, 1.000000000000000000, 0.9659258262890683122, 1.000000000000000000, 0.9659258262890683122, 1.000000000000000000, 0.9659258262890683122, 1.000000000000000000, 0.9659258262890683122, 1.000000000000000000, 0.9659258262890683122, 1.000000000000000000, 0.9659258262890683122, 1.000000000000000000, 0.9659258262890683122, 1.000000000000000000, 0.9659258262890683122, 1.000000000000000000, 0.9659258262890683122, 1.000000000000000000, 0.9659258262890683122, 1.000000000000000000, 0.9659258262890683122, 1.000000000000000000, 0.9659258262890683122, 1.000000000000000000, 0.9659258262890683122, 1.000000000000000000, 0.9659258262890683122, 1.000000000000000000, 0.9659258262890683122, 1.000000000000000000, 0.9659258262890683122, 1.000000000000000000, 0.9659258262890683122, 1.000000000000000000, 0.9659258262890683122, 1.000000000000000000, 0.9659258262890683122, 1.000000000000000000, 0.9659258262890683122, 1.000000000000000000, 0.9659258262890683122, 1.000000000000000000, 0.9659258262890683122, 1.000000000000000000, 0.9659258262890683122, 1.000000000000000000, 0.9659258262890683122, 1.000000000000000000, 0.9659258262890683122, 1.000000000000000000, 0.9659258262890683122, 1.000000000000000000, 0.9659258262890683122, 1.000000000000000000, 0.9659258262890683122, 1.000000000000000000, 0.9659258262890683122, 1.000000000000000000, 0.9659258262890683122, 1.000000000000000000, 0.9659258262890683122, 1.000000000000000000, 0.9659258262890683122, 1.000000000000000000, 0.9659258262890683122, 1.000000000000000000, 0.9659258262890683122, 1.000000000000000000, 0.9659258262890683122, 1.000000000000000000, 0.9659258262890683122, 1.000000000000000000, 0.9659258262890683122, 1.000000000000000000, 0.9659258262890683122, 1.000000000000000000, 0.9659258262890683122, 1.000000000000000000, 0.9659258262890683122, 1.000000000000000000, 0.9659258262890683122, 1.000000000000000000, 0.9659258262890683122, 1.000000000000000000, 0.9659258262890683122, 1.000000000000000000, 0.9659258262890683122, 1.000000000000000000, 0.9659258262890683122, 1.000000000000000000, 0.9659258262890683122, 1.000000000000000000, 0.9659258262890683122, 1.000000000000000000, 0.9659258262890683122, 1.000000000000000000, 0.9659258262890683122, 1.000000000000000000, 0.9659258262890683122, 1.000000000000000000, 0.9659258262890683122, 1.000000000000000000, 0.9659258262890683122, 1.000000000000000000, 0.9659258262890683122, 1.000000000000000000, 0.9659258262890683122, 1.000000000000000000, 0.9659258262890683122, 1.000000000000000000, 0.9659258262890683122, 1.000000000000000000, 0.9659258262890683122, 1.000000000000000000, 0.9659258262890683122, 1.000000000000000000, 0.9659258262890683122, 1.000000000000000000, 0.9659258262890683122, 1.000000000000000000, 0.9659258262890683122, 1.000000000000000000, 0.9659258262890683122, 1.000000000000000000, 0.9659258262890683122, 1.000000000000000000, 0.9659258262890683122, 1.000000000000000000, 0.9659258262890683122, 1.000000000000000000, 0.9659258262890683122, 1.000000000000000000, 0.9659258262890683122, 1.000000000000000000, 0.9659258262890683122, 1.000000000000000000, 0.9659258262890683122, 1.000000000000000000, 0.9659258262890683122, 1.000000000000000000, 0.9659258262890683122, 1.000000000000000000, 0.9659258262890683122, 1.000000000000000000, 0.9659258262890683122, 1.000000000000000000, 0.9659258262890683122, 1.000000000000000000, 0.9659258262890683122, 1.000000000000000000, 0.9659258262890683122, 1.000000000000000000, 0.9659258262890683122, 1.000000000000000000, 0.9659258262890683122, 1.000000000000000000, 0.9659258262890683122, 1.000000000000000000, 0.9659258262890683122, 1.000000000000000000, 0.9659258262890683122, 1.000000000000000000, 0.9659258262890683122, 1.000000000000000000, 0.9659258262890683122, 1.000000000000000000, 0.9659258262890683122, 1.000000000000000000, 0.9659258262890683122, 1.000000000000000000, 0.9659258262890683122, 1.000000000000000000, 0.9659258262890683122, 1.000000000000000000, 0.9659258262890683122, 1.000000000000000000, 0.9659258262890683122, 1.000000000000000000, 0.9659258262890683122, 1.000000000000000000, 0.9659258262890683122, 1.000000000000000000, 0.9659258262890683122, 1.000000000000000000, 0.9659258262890683122, 1.000000000000000000, 0.9659258262890683122, 1.000000000000000000, 0.9659258262890683122, 1.000000000000000000, 0.9659258262890683122, 1.000000000000000000, 0.9659258262890683122, 1.000000000000000000, 0.9659258262890683122, 1.000000000000000000, 0.9659258262890683122, 1.000000000000000000, 0.9659258262890683122, 1.000000000000000000, 0.9659258262890683122, 1.000000000000000000, 0.9659258262890683122, 1.000000000000000000, 0.9659258262890683122, 1.000000000000000000, 0.9659258262890683122, 1.000000000000000000, 0.9659258262890683122, 1.000000000000000000, 0.9659258262890683122, 1.000000000000000000, 0.9659258262890683122, 1.000000000000000000, 0.9659258262890683122, 1.000000000000000000, 0.9659258262890683122, 1.000000000000000000, 0.9659258262890683122, 1.000000000000000000, 0.9659258262890683122, 1.000000000000000000, 0.9659258262890683122, 1.000000000000000000, 0.9659258262890683122, 1.000000000000000000, 0.9659258262890683122, 1.000000000000000000, 0.9659258262890683122, 1.000000000000000000, 0.9659258262890683122, 1.000000000000000000, 0.9659258262890683122, 1.000000000000000000, 0.9659258262890683122, 1.000000000000000000, 0.9659258262890683122, 1.000000000000000000, 0.9659258262890683122, 1.000000000000000000, 0.9659258262890683122, 1.000000000000000000, 0.9659258262890683122, 1.000000000000000000, 0.9659258262890683122, 1.000000000000000000, 0.9659258262890683122, 1.000000000000000000, 0.9659258262890683122, 1.000000000000000000, 0.9659258262890683122, 1.000000000000000000, 0.9659258262890683122, 1.000000000000000000, 0.9659258262890683122, 1.000000000000000000, 0.9659258262890683122, 1.000000000000000000, 0.9659258262890683122, 1.000000000000000000, 0.9659258262890683122, 1.000000000000000000, 0.9659258262890683122, 1.000000000000000000, 0.9659258262890683122, 1.000000000000000000, 0.9659258262890683122, 1.000000000000000000, 0.9659258262890683122, 1.000000000000000000, 0.9659258262890683122, 1.000000000000000000, 0.9659258262890683122, 1.000000000000000000, 0.9659258262890683122, 1.000000000000000000, 0.9659258262890683122, 1.000000000000000000, 0.9659258262890683122, 1.000000000000000000, 0.9659258262890683122, 1.000000000000000000, 0.9659258262890683122, 1.000000000000000000, 0.9659258262890683122, 1.000000000000000000, 0.9659258262890683122, 1.000000000000000000, 0.9659258262890683122, 1.000000000000000000, 0.9659258262890683122, 1.000000000000000000, 0.9659258262890683122, 1.000000000000000000, 0.9659258262890683122, 1.000000000000000000, 0.9659258262890683122, 1.000000000000000000, 0.9659258262890683122, 1.000000000000000000, 0.9659258262890683122, 1.000000000000000000, 0.9659258262890683122, 1.000000000000000000, 0.9659258262890683122, 1.000000000000000000) ) ) 
 REPRESENTATION_ITEM ( '' )  SURFACE ( )  );
#4393 = SURFACE_SIDE_STYLE ('',( #29327 ) ) ;
#4394 = CARTESIAN_POINT ( 'NONE',  ( 6.565887622018943937, 40.16530133659708923, 12.81628187352647430 ) ) ;
#4395 = CARTESIAN_POINT ( 'NONE',  ( 5.076628168052704559, 45.17559781766745175, -8.527530157486179263 ) ) ;
#4396 = CARTESIAN_POINT ( 'NONE',  ( -8.000000000000000000, 41.24999999999999289, 4.250000000000000000 ) ) ;
#4397 = CARTESIAN_POINT ( 'NONE',  ( -0.3689425029237881626, 57.42874883491397497, 10.36894250292379027 ) ) ;
#4398 = CARTESIAN_POINT ( 'NONE',  ( 18.52753015748617571, 38.09226448433412315, 4.923371831947298993 ) ) ;
#4399 = ORIENTED_EDGE ( 'NONE', *, *, #72108, .F. ) ;
#4400 = CARTESIAN_POINT ( 'NONE',  ( -6.000000000000014211, 80.32179676972448590, 4.250000000000000000 ) ) ;
#4401 = CARTESIAN_POINT ( 'NONE',  ( 24.16423886937409904, 54.09541550158063217, 3.795296366450317205 ) ) ;
#4402 = LINE ( 'NONE', #58348, #7220 ) ;
#4403 = CARTESIAN_POINT ( 'NONE',  ( -0.3689425029237881626, 67.42874883491396076, 10.36894250292379027 ) ) ;
#4405 = CIRCLE ( 'NONE', #60277, 2.900000000000001243 ) ;
#4404 = CARTESIAN_POINT ( 'NONE',  ( 24.16423886937409904, 39.09541550158062506, 3.795296366450317205 ) ) ;
#4407 = CARTESIAN_POINT ( 'NONE',  ( 7.313705784284644906, 14.49999999999999112, -13.09617149020747817 ) ) ;
#4406 = CARTESIAN_POINT ( 'NONE',  ( 13.79529636645030344, 58.26208216824728936, 14.16423886937410614 ) ) ;
#4408 = CARTESIAN_POINT ( 'NONE',  ( 19.42250999205614193, 5.147018677488171434, 5.440088680355555262 ) ) ;
#4409 = CARTESIAN_POINT ( 'NONE',  ( 2.791683348922240793, 6.633931151000785675, 7.208316651077764092 ) ) ;
#4411 = CARTESIAN_POINT ( 'NONE',  ( 21.09922568453594849, 1.206968003263753531, 6.408140936763242479 ) ) ;
#4410 = CARTESIAN_POINT ( 'NONE',  ( 6.910443788711833513, -84.29081344372315243, 2.750000000004829026 ) ) ;
#4412 = ORIENTED_EDGE ( 'NONE', *, *, #10740, .T. ) ;
#4413 = CARTESIAN_POINT ( 'NONE',  ( 20.88017736071110519, 50.56368534415484106, 2.639326808657452039E-16 ) ) ;
#4414 = CARTESIAN_POINT ( 'NONE',  ( -0.8801773607111009756, 18.06368534415484106, 1.068504757029289695E-15 ) ) ;
#4415 = EDGE_CURVE ( 'NONE', #45767, #94563, #26889, .T. ) ;
#4416 = CARTESIAN_POINT ( 'NONE',  ( 18.52753015748617571, 48.09226448433412315, 4.923371831947298993 ) ) ;
#4417 = VECTOR ( 'NONE', #17180, 1000.000000000000227 ) ;
#4418 = TOROIDAL_SURFACE ( 'NONE', #53878, 14.49999999999999822, 0.5000000000000000000 ) ;
#4419 = CARTESIAN_POINT ( 'NONE',  ( 18.52753015748618282, 53.92559781766745175, -4.923371831947291888 ) ) ;
#4420 =( NAMED_UNIT ( * ) SI_UNIT ( $, .STERADIAN. ) SOLID_ANGLE_UNIT ( ) );
#4421 = CARTESIAN_POINT ( 'NONE',  ( 13.79529636645030344, 23.26208216824730002, 14.16423886937410614 ) ) ;
#4422 = FILL_AREA_STYLE ('',( #88396 ) ) ;
#4424 = FILL_AREA_STYLE ('',( #5889 ) ) ;
#4423 = PRESENTATION_STYLE_ASSIGNMENT (( #41932 ) ) ;
#4425 = CARTESIAN_POINT ( 'NONE',  ( 20.88017736071110875, 25.77201867748816966, -2.915334737309920765 ) ) ;
#4426 = CARTESIAN_POINT ( 'NONE',  ( -2.816281873526471635, 43.91530133659708923, -3.434112377981056508 ) ) ;
#4427 = CARTESIAN_POINT ( 'NONE',  ( 11.35178980618980304, 14.49999999999999112, -9.804941009311946232 ) ) ;
#4428 = CARTESIAN_POINT ( 'NONE',  ( 18.52753015748617571, 8.092264484334117824, 4.923371831947298993 ) ) ;
#4429 = CARTESIAN_POINT ( 'NONE',  ( 3.591859063236763294, 63.29030133659708923, -11.09922568453595026 ) ) ;
#4430 = ORIENTED_EDGE ( 'NONE', *, *, #52943, .T. ) ;
#4431 = CARTESIAN_POINT ( 'NONE',  ( 4.471658927061713307, -3.629165645961075715, -3.750000000000000000 ) ) ;
#4432 = CARTESIAN_POINT ( 'NONE',  ( 13.79529636645030344, 33.26208216824730357, 14.16423886937410614 ) ) ;
#4433 = CARTESIAN_POINT ( 'NONE',  ( 0.1532563361054083140, 21.00893115100078745, 1.131784320476157264E-15 ) ) ;
#4434 = CYLINDRICAL_SURFACE ( 'NONE', #75816, 11.92686044187656513 ) ;
#4435 = CARTESIAN_POINT ( 'NONE',  ( 12.91533473730993009, 11.60535201082150714, -10.88017736071109987 ) ) ;
#4436 = CARTESIAN_POINT ( 'NONE',  ( -13.21236992757665973, -0.03417435944610275333, -5.338143956176898186 ) ) ;
#4437 = FACE_OUTER_BOUND ( 'NONE', #25861, .T. ) ;
#4438 = CARTESIAN_POINT ( 'NONE',  ( 2.035157376598824452, 43.68868534415484106, 7.964842623401179544 ) ) ;
#4439 = CARTESIAN_POINT ( 'NONE',  ( -0.8801773607111009756, 48.06368534415484817, 1.068504757029289695E-15 ) ) ;
#4440 = CARTESIAN_POINT ( 'NONE',  ( 13.43411237798105340, 15.58196800326374998, 12.81628187352647963 ) ) ;
#4441 = CARTESIAN_POINT ( 'NONE',  ( 12.63842701281683034, 62.46726448433410894, 9.846743663894596210 ) ) ;
#4442 = CARTESIAN_POINT ( 'NONE',  ( 24.35999999999999233, 44.99999999999997868, 9.500000000000000000 ) ) ;
#4443 = CARTESIAN_POINT ( 'NONE',  ( 18.52753015748618282, 3.925597817667451306, -4.923371831947291888 ) ) ;
#4444 = LINE ( 'NONE', #42919, #74822 ) ;
#4445 = CARTESIAN_POINT ( 'NONE',  ( 15.44008868035555793, 46.39701867748817676, -9.422509992056140149 ) ) ;
#4446 = EDGE_CURVE ( 'NONE', #35322, #77981, #80390, .T. ) ;
#4447 = CARTESIAN_POINT ( 'NONE',  ( -2.816281873526473856, -0.8763653300695799508, 9.499525473075851096E-16 ) ) ;
#4448 = CARTESIAN_POINT ( 'NONE',  ( 2.035157376598824452, 58.68868534415482685, 7.964842623401179544 ) ) ;
#4449 = CARTESIAN_POINT ( 'NONE',  ( 0.1532563361054082862, 31.21726448433412315, 2.638427012816831674 ) ) ;
#4450 = CARTESIAN_POINT ( 'NONE',  ( 0.6178305044545838731, 44.74863466993042493, 9.382169495545420901 ) ) ;
#4451 = CARTESIAN_POINT ( 'NONE',  ( 18.52753015748617571, 8.092264484334117824, 4.923371831947298993 ) ) ;
#4452 = ORIENTED_EDGE ( 'NONE', *, *, #61724, .F. ) ;
#4453 = LINE ( 'NONE', #3951, #67648 ) ;
#4454 = CARTESIAN_POINT ( 'NONE',  ( 0.7117905103454439386, 0.000000000000000000, 5.406585696355436177 ) ) ;
#4455 = CARTESIAN_POINT ( 'NONE',  ( 7.084665262690076126, 17.02201867748817676, -10.88017736071110164 ) ) ;
#4456 = DIRECTION ( 'NONE',  ( -0.7604059656000257128, 0.000000000000000000, -0.6494480483301898754 ) ) ;
#4457 = CARTESIAN_POINT ( 'NONE',  ( 5.076628168052703671, 26.84226448433411960, 8.527530157486179263 ) ) ;
#4458 = CARTESIAN_POINT ( 'NONE',  ( 17.96484262340118221, 14.93868534415483751, 7.964842623401181321 ) ) ;
#4459 = CARTESIAN_POINT ( 'NONE',  ( 15.44008868035555260, 4.730352010821505360, 9.422509992056143702 ) ) ;
#4460 = ORIENTED_EDGE ( 'NONE', *, *, #38762, .F. ) ;
#4461 = CARTESIAN_POINT ( 'NONE',  ( 12.91533473730992121, 14.52201867748817143, 10.88017736071110164 ) ) ;
#4462 = CARTESIAN_POINT ( 'NONE',  ( 12.91533473730992121, 29.52201867748817321, 10.88017736071110164 ) ) ;
#4464 = CARTESIAN_POINT ( 'NONE',  ( 17.96484262340118221, 26.18868534415483396, -7.964842623401177768 ) ) ;
#4463 = CARTESIAN_POINT ( 'NONE',  ( 6.336512077239887297, 0.2306972965111900864, -13.53095227201384354 ) ) ;
#4465 = PRESENTATION_LAYER_ASSIGNMENT (  '', '', ( #74682 ) ) ;
#4466 = VERTEX_POINT ( 'NONE', #11893 ) ;
#4467 = CARTESIAN_POINT ( 'NONE',  ( 20.24186590665277663, 26.76028685723174760, 6.114288769123037426 ) ) ;
#4468 = CARTESIAN_POINT ( 'NONE',  ( -0.8801773607111008646, 18.27201867748817321, 2.915334737309923430 ) ) ;
#4469 = DIRECTION ( 'NONE',  ( -0.9025852843498589628, 0.000000000000000000, -0.4305110968082987433 ) ) ;
#4470 = DIRECTION ( 'NONE',  ( -1.049065152435176504E-16, 1.000000000000000000, -0.000000000000000000 ) ) ;
#4471 = CARTESIAN_POINT ( 'NONE',  ( 16.40814093676323893, 60.79030133659709634, 11.09922568453595026 ) ) ;
#4472 = CARTESIAN_POINT ( 'NONE',  ( -0.8801773607110990882, 67.85535201082149115, -2.915334737309924318 ) ) ;
#4473 = CARTESIAN_POINT ( 'NONE',  ( -4.164238869374098151, 36.59541550158063217, -3.795296366450310543 ) ) ;
#4474 = CARTESIAN_POINT ( 'NONE',  ( 7.084665262690076126, 39.10535201082150536, 10.88017736071109987 ) ) ;
#4475 = CARTESIAN_POINT ( 'NONE',  ( 10.00000000000000178, 14.31368534415483929, 10.88017736071110342 ) ) ;
#4476 = CARTESIAN_POINT ( 'NONE',  ( 19.84674366389459266, 63.30059781766745886, 2.638427012816836559 ) ) ;
#4477 = CARTESIAN_POINT ( 'NONE',  ( 10.00000000000000000, 54.75893115100078745, -9.846743663894594434 ) ) ;
#4478 = CARTESIAN_POINT ( 'NONE',  ( 10.00000000000000000, 24.75893115100078745, -9.846743663894594434 ) ) ;
#4479 = CARTESIAN_POINT ( 'NONE',  ( 3.434112377981054287, -32.33469866340291077, -12.81628187352647608 ) ) ;
#4480 = AXIS2_PLACEMENT_3D ( 'NONE', #16144, #46630, #9629 ) ;
#4481 = ADVANCED_FACE ( 'NONE', ( #95898 ), #81366, .F. ) ;
#4482 = CARTESIAN_POINT ( 'NONE',  ( -0.8801773607110991993, 7.855352010821504471, -2.915334737309923874 ) ) ;
#4483 = CARTESIAN_POINT ( 'NONE',  ( 10.00000000000000178, 7.258931151000785675, 9.846743663894594434 ) ) ;
#4484 = CARTESIAN_POINT ( 'NONE',  ( 10.00000000000000000, 56.81368534415484106, -10.88017736071110342 ) ) ;
#4486 = CARTESIAN_POINT ( 'NONE',  ( 22.81628187352648496, 61.83196800326376774, -3.434112377981050290 ) ) ;
#4485 = CARTESIAN_POINT ( 'NONE',  ( 12.91533473730992121, 24.52201867748816966, 10.88017736071110164 ) ) ;
#4487 = CARTESIAN_POINT ( 'NONE',  ( 17.08211943468705130, 33.47041550158063927, 12.26659068614894998 ) ) ;
#4488 = EDGE_CURVE ( 'NONE', #96588, #16656, #12865, .T. ) ;
#4489 = VECTOR ( 'NONE', #80525, 1000.000000000000000 ) ;
#4490 = CARTESIAN_POINT ( 'NONE',  ( 20.32896413005680714, 12.60497603579417536, -5.963430220938276349 ) ) ;
#4491 = TOROIDAL_SURFACE ( 'NONE', #33230, 10.65000000000000036, 0.2500000000000000000 ) ;
#4492 = CARTESIAN_POINT ( 'NONE',  ( 13.43411237798106583, 52.66530133659708213, -12.81628187352647252 ) ) ;
#4493 = ORIENTED_EDGE ( 'NONE', *, *, #93755, .F. ) ;
#4494 = CARTESIAN_POINT ( 'NONE',  ( 2.791683348922237240, 65.38393115100078035, -7.208316651077763204 ) ) ;
#4495 = DIRECTION ( 'NONE',  ( 0.000000000000000000, 0.000000000000000000, 1.000000000000000000 ) ) ;
#4496 = CARTESIAN_POINT ( 'NONE',  ( 20.88017736071110875, 30.77201867748816966, -2.915334737309920765 ) ) ;
#4497 = CARTESIAN_POINT ( 'NONE',  ( -9.075906804202377387, 15.00000000000000000, 13.17214151599831595 ) ) ;
#4498 = VERTEX_POINT ( 'NONE', #4407 ) ;
#4499 = CARTESIAN_POINT ( 'NONE',  ( 2.791683348922240793, 11.63393115100078568, 7.208316651077764092 ) ) ;
#4500 = CARTESIAN_POINT ( 'NONE',  ( 11.92686044187655980, 7.396642702460839658, -3.195792623639533314 ) ) ;
#4501 = B_SPLINE_CURVE_WITH_KNOTS ( 'NONE', 3,
 ( #26248, #33728, #64716, #40770 ),
 .UNSPECIFIED., .F., .F.,
 ( 4, 4 ),
 ( 0.000000000000000000, 0.001036303429213241041 ),
 .UNSPECIFIED. ) ;
#4502 = CARTESIAN_POINT ( 'NONE',  ( 5.076628168052703671, 21.84226448433411960, 8.527530157486179263 ) ) ;
#4503 = CARTESIAN_POINT ( 'NONE',  ( 10.00000000000000000, 9.758931151000785675, -9.846743663894594434 ) ) ;
#4504 = CARTESIAN_POINT ( 'NONE',  ( 2.791683348922240793, 1.633931151000784565, 7.208316651077764092 ) ) ;
#4506 = DIRECTION ( 'NONE',  ( 0.000000000000000000, 0.000000000000000000, -1.000000000000000000 ) ) ;
#4505 = CARTESIAN_POINT ( 'NONE',  ( 10.00000000000000000, 66.81368534415484817, -10.88017736071110342 ) ) ;
#4507 = CARTESIAN_POINT ( 'NONE',  ( 1.472469842513823179, 5.592264484334118713, -4.923371831947296329 ) ) ;
#4509 = ORIENTED_EDGE ( 'NONE', *, *, #3234, .F. ) ;
#4508 = CARTESIAN_POINT ( 'NONE',  ( 5.076628168052704559, 15.17559781766745175, -8.527530157486179263 ) ) ;
#4510 = CARTESIAN_POINT ( 'NONE',  ( 6.284496703633148051, -36.06254290988038491, 3.999999999999999112 ) ) ;
#4511 = CARTESIAN_POINT ( 'NONE',  ( -1.099225684535947600, 4.540301336597087456, 6.408140936763237150 ) ) ;
#4512 = ORIENTED_EDGE ( 'NONE', *, *, #83547, .F. ) ;
#4513 = EDGE_LOOP ( 'NONE', ( #31366, #36200, #2533, #9399, #53295, #97738 ) ) ;
#4514 = SURFACE_STYLE_FILL_AREA ( #72985 ) ;
#4515 = CARTESIAN_POINT ( 'NONE',  ( 17.08211943468705130, 13.47041550158063572, 12.26659068614894998 ) ) ;
#4516 = UNCERTAINTY_MEASURE_WITH_UNIT (LENGTH_MEASURE( 1.000000000000000082E-05 ), #93288, 'distance_accuracy_value', 'NONE');
#4517 = FACE_OUTER_BOUND ( 'NONE', #44073, .T. ) ;
#4518 = CARTESIAN_POINT ( 'NONE',  ( 24.16423886937410614, 14.30374883491396787, 8.672049930838204340E-16 ) ) ;
#4519 = CARTESIAN_POINT ( 'NONE',  ( 17.08211943468705130, 33.47041550158063927, 12.26659068614894998 ) ) ;
#4520 =( LENGTH_UNIT ( ) NAMED_UNIT ( * ) SI_UNIT ( .MILLI., .METRE. ) );
#4521 = CARTESIAN_POINT ( 'NONE',  ( 17.08211943468705130, 3.470415501580634388, 12.26659068614894998 ) ) ;
#4522 = CARTESIAN_POINT ( 'NONE',  ( 0.5774900079438607392, 38.48035201082150536, 5.440088680355550821 ) ) ;
#4523 = CARTESIAN_POINT ( 'NONE',  ( 6.937721053838227014, -80.66520463107747219, -3.750000000000000888 ) ) ;
#4524 = CARTESIAN_POINT ( 'NONE',  ( 7.361572987183169658, 14.96726448433411960, -9.846743663894592657 ) ) ;
#4526 = CARTESIAN_POINT ( 'NONE',  ( 5.076628168052703671, 26.84226448433411960, 8.527530157486179263 ) ) ;
#4525 = CARTESIAN_POINT ( 'NONE',  ( 15.44008868035555793, 51.39701867748816966, -9.422509992056140149 ) ) ;
#4527 = CARTESIAN_POINT ( 'NONE',  ( 19.42250999205614548, 10.98035201082150536, -5.440088680355545492 ) ) ;
#4528 = CARTESIAN_POINT ( 'NONE',  ( 0.6178305044545818747, 48.49863466993042493, -9.382169495545419124 ) ) ;
#4529 = CARTESIAN_POINT ( 'NONE',  ( 0.1532563361054083140, 46.00893115100079456, 1.131784320476157264E-15 ) ) ;
#4530 = CARTESIAN_POINT ( 'NONE',  ( 12.00809552683958614, 0.5000000000000004441, -8.989195838243546177 ) ) ;
#4531 = EDGE_CURVE ( 'NONE', #22303, #88333, #57870, .T. ) ;
#4532 = CARTESIAN_POINT ( 'NONE',  ( 19.38216949554541557, 27.24863466993041783, -9.382169495545420901 ) ) ;
#4533 = CARTESIAN_POINT ( 'NONE',  ( -14.16423886937410437, -28.40458449841936428, -3.795296366450299885 ) ) ;
#4534 = VECTOR ( 'NONE', #5458, 1000.000000000000000 ) ;
#4535 = CARTESIAN_POINT ( 'NONE',  ( 10.00000000000000000, 39.75893115100078745, -9.846743663894594434 ) ) ;
#4536 = CARTESIAN_POINT ( 'NONE',  ( 6.204703633549690345, 7.845415501580634832, 14.16423886937410082 ) ) ;
#4537 = EDGE_LOOP ( 'NONE', ( #85668, #68586, #87009, #52697 ) ) ;
#4538 = CARTESIAN_POINT ( 'NONE',  ( -11.35178980618960409, 15.00000000000000000, -9.804941009312079458 ) ) ;
#4539 = ADVANCED_FACE ( 'NONE', ( #67355 ), #72872, .F. ) ;
#4540 = CARTESIAN_POINT ( 'NONE',  ( 4.559911319644449179, 53.89701867748817676, 9.422509992056141925 ) ) ;
#4541 = CARTESIAN_POINT ( 'NONE',  ( -0.8801773607110991993, 47.85535201082150536, -2.915334737309923874 ) ) ;
#4542 = CARTESIAN_POINT ( 'NONE',  ( 2.917880565312950480, 45.97041550158063927, -12.26659068614894821 ) ) ;
#4543 = CARTESIAN_POINT ( 'NONE',  ( 0.1532563361054082862, 51.21726448433412315, 2.638427012816831674 ) ) ;
#4544 = CARTESIAN_POINT ( 'NONE',  ( -4.873787042390880231, 15.00000000000000000, 13.39061984619915791 ) ) ;
#4545 = CARTESIAN_POINT ( 'NONE',  ( 19.42250999205614193, 35.14701867748816966, 5.440088680355555262 ) ) ;
#4546 = CARTESIAN_POINT ( 'NONE',  ( -6.728851239469183732, -2.645283894275179170E-15, 12.98580270086196542 ) ) ;
#4547 = AXIS2_PLACEMENT_3D ( 'NONE', #15217, #54657, #91691 ) ;
#4548 = CARTESIAN_POINT ( 'NONE',  ( 14.92337183194729633, 57.67559781766745886, 8.527530157486181039 ) ) ;
#4549 = CARTESIAN_POINT ( 'NONE',  ( 9.422509992056141925, 15.14701867748818209, 5.440088680355547268 ) ) ;
#4550 = CARTESIAN_POINT ( 'NONE',  ( 0.2751277870542983006, 13.21833443783938122, 6.500000000000002665 ) ) ;
#4551 = TOROIDAL_SURFACE ( 'NONE', #7775, 6.599999999999995204, 0.2500000000000000000 ) ;
#4552 = CARTESIAN_POINT ( 'NONE',  ( 12.91533473730992121, 4.522018677488169658, 10.88017736071110164 ) ) ;
#4553 = CARTESIAN_POINT ( 'NONE',  ( 0.000000000000000000, 0.000000000000000000, 0.000000000000000000 ) ) ;
#4554 = AXIS2_PLACEMENT_3D ( 'NONE', #69033, #70018, #85508 ) ;
#4555 = CARTESIAN_POINT ( 'NONE',  ( 15.44008868035555793, 61.39701867748817676, -9.422509992056140149 ) ) ;
#4556 = B_SPLINE_CURVE_WITH_KNOTS ( 'NONE', 3,
 ( #9266, #39773, #40749, #25758, #93245, #18246 ),
 .UNSPECIFIED., .F., .F.,
 ( 4, 2, 4 ),
 ( 0.000000000000000000, 0.0002701661927229329508, 0.0005403323854458659016 ),
 .UNSPECIFIED. ) ;
#4557 = CARTESIAN_POINT ( 'NONE',  ( 5.076628168052704559, 0.1755978176674514724, -8.527530157486179263 ) ) ;
#4558 = CARTESIAN_POINT ( 'NONE',  ( 18.00000000000000000, 78.65120189252257887, -3.750000044091261309 ) ) ;
#4559 = EDGE_CURVE ( 'NONE', #97832, #31539, #1606, .T. ) ;
#4560 = CARTESIAN_POINT ( 'NONE',  ( 7.361572987183170547, 32.05059781766745175, 9.846743663894590881 ) ) ;
#4561 = CARTESIAN_POINT ( 'NONE',  ( 17.96484262340118221, 16.18868534415483396, -7.964842623401177768 ) ) ;
#4562 = CARTESIAN_POINT ( 'NONE',  ( 3.591859063236761518, 4.956968003263753531, 11.09922568453594849 ) ) ;
#4564 = DIRECTION ( 'NONE',  ( 1.000000000000000000, 0.000000000000000000, 0.000000000000000000 ) ) ;
#4563 = CARTESIAN_POINT ( 'NONE',  ( -0.8801773607110991993, 32.85535201082151247, -2.915334737309923874 ) ) ;
#4565 = SURFACE_STYLE_USAGE ( .BOTH. , #20038 ) ;
#4566 = CARTESIAN_POINT ( 'NONE',  ( 13.43411237798106583, 37.66530133659708923, -12.81628187352647252 ) ) ;
#4567 = EDGE_LOOP ( 'NONE', ( #94794, #37321, #67176, #9373 ) ) ;
#4568 = CARTESIAN_POINT ( 'NONE',  ( -0.8801773607111008646, 63.27201867748817676, 2.915334737309923430 ) ) ;
#4569 = EDGE_CURVE ( 'NONE', #84772, #86520, #32600, .T. ) ;
#4571 = CARTESIAN_POINT ( 'NONE',  ( 19.84674366389459266, 18.30059781766745175, 2.638427012816836559 ) ) ;
#4570 = CARTESIAN_POINT ( 'NONE',  ( 19.38216949554541557, 17.24863466993041783, -9.382169495545420901 ) ) ;
#4572 =( NAMED_UNIT ( * ) PLANE_ANGLE_UNIT ( ) SI_UNIT ( $, .RADIAN. ) );
#4573 = CARTESIAN_POINT ( 'NONE',  ( 10.00000000000000178, 29.31368534415483751, 10.88017736071110342 ) ) ;
#4574 = CARTESIAN_POINT ( 'NONE',  ( 10.00000000000000178, 63.05374883491396076, 14.16423886937410082 ) ) ;
#4575 = CARTESIAN_POINT ( 'NONE',  ( 14.92337183194729988, 54.34226448433412315, -8.527530157486177487 ) ) ;
#4576 = CARTESIAN_POINT ( 'NONE',  ( 2.791683348922240793, 1.633931151000784565, 7.208316651077764092 ) ) ;
#4577 = CARTESIAN_POINT ( 'NONE',  ( 0.5774900079438607392, 58.48035201082151247, 5.440088680355550821 ) ) ;
#4578 = CARTESIAN_POINT ( 'NONE',  ( 0.2751277870542914172, 43.21833443783938122, 6.499999999999992006 ) ) ;
#4579 = CARTESIAN_POINT ( 'NONE',  ( 2.917880565312948704, 32.63708216824730357, 12.26659068614894643 ) ) ;
#4580 = B_SPLINE_CURVE_WITH_KNOTS ( 'NONE', 3,
 ( #19206, #58677, #12190, #20689 ),
 .UNSPECIFIED., .F., .F.,
 ( 4, 4 ),
 ( 6.046421166978534523E-20, 0.0003153927346769890092 ),
 .UNSPECIFIED. ) ;
#4581 = CARTESIAN_POINT ( 'NONE',  ( 0.000000000000000000, 14.49999999999999822, 0.000000000000000000 ) ) ;
#4582 = CARTESIAN_POINT ( 'NONE',  ( -3.586264863028716388, -2.711807932117549225, -4.000000000000000000 ) ) ;
#4583 = ORIENTED_EDGE ( 'NONE', *, *, #90769, .T. ) ;
#4584 = ORIENTED_EDGE ( 'NONE', *, *, #9279, .T. ) ;
#4585 = CARTESIAN_POINT ( 'NONE',  ( -4.164238869374098151, 46.59541550158063927, -3.795296366450310543 ) ) ;
#4586 = CARTESIAN_POINT ( 'NONE',  ( 22.26659068614894466, 48.88708216824730357, 7.082119434687054849 ) ) ;
#4587 = CARTESIAN_POINT ( 'NONE',  ( 18.52753015748617571, 23.09226448433411960, 4.923371831947298993 ) ) ;
#4588 = CARTESIAN_POINT ( 'NONE',  ( 19.38216949554541557, 32.24863466993041783, -9.382169495545420901 ) ) ;
#4589 = FACE_OUTER_BOUND ( 'NONE', #98723, .T. ) ;
#4590 = CARTESIAN_POINT ( 'NONE',  ( 8.606322355891363074, 4.859979058039186735E-16, -11.66967075398807374 ) ) ;
#4591 =( LENGTH_UNIT ( ) NAMED_UNIT ( * ) SI_UNIT ( .MILLI., .METRE. ) );
#4592 = CARTESIAN_POINT ( 'NONE',  ( 20.36894250292379738, 39.92874883491396787, -10.36894250292379027 ) ) ;
#4593 = DIRECTION ( 'NONE',  ( -0.000000000000000000, -1.000000000000000000, -0.000000000000000000 ) ) ;
#4594 = CARTESIAN_POINT ( 'NONE',  ( 5.076628168052704559, 10.17559781766745175, -8.527530157486179263 ) ) ;
#4595 = CARTESIAN_POINT ( 'NONE',  ( -4.922013193295410538, 0.000000000000000000, -2.347679864819515405 ) ) ;
#4596 = CARTESIAN_POINT ( 'NONE',  ( -7.208316651077756099, -3.366068848999213881, 7.208316651077766757 ) ) ;
#4597 = ORIENTED_EDGE ( 'NONE', *, *, #73216, .F. ) ;
#4598 = DIRECTION ( 'NONE',  ( -0.000000000000000000, -0.000000000000000000, -1.000000000000000000 ) ) ;
#4599 =( BOUNDED_CURVE ( )  B_SPLINE_CURVE ( 2, ( #81791, #73801, #13308, #5331, #35812, #67301, #43794, #66804, #44294 ),
 .UNSPECIFIED., .F., .T. ) 
 B_SPLINE_CURVE_WITH_KNOTS ( ( 3, 2, 2, 2, 3 ),
 ( 0.08299807979737425234, 0.08333333333333337034, 0.08928571428571430157, 0.09523809523809523281, 0.09557334877405435081 ),
 .UNSPECIFIED. ) 
 CURVE ( )  GEOMETRIC_REPRESENTATION_ITEM ( )  RATIONAL_B_SPLINE_CURVE ( ( 0.9963778908391762723, 0.9980808541467921513, 1.000000000000000000, 0.9659258262890683122, 1.000000000000000000, 0.9659258262890683122, 1.000000000000000000, 0.9980808541467921513, 0.9963778908391762723 ) ) 
 REPRESENTATION_ITEM ( '' )  );
#4600 = EDGE_LOOP ( 'NONE', ( #55398, #23260, #22155, #55093, #53646, #56206 ) ) ;
#4601 =( NAMED_UNIT ( * ) SI_UNIT ( $, .STERADIAN. ) SOLID_ANGLE_UNIT ( ) );
#4602 = ORIENTED_EDGE ( 'NONE', *, *, #50023, .F. ) ;
#4603 = CARTESIAN_POINT ( 'NONE',  ( 6.204703633549690345, 12.84541550158063572, 14.16423886937410082 ) ) ;
#4605 = CARTESIAN_POINT ( 'NONE',  ( 20.88017736071110519, 20.56368534415484106, 2.639326808657452039E-16 ) ) ;
#4604 = CARTESIAN_POINT ( 'NONE',  ( 20.88017736071110519, 15.56368534415483751, 2.639326808657452039E-16 ) ) ;
#4607 = CARTESIAN_POINT ( 'NONE',  ( 13.43411237798106583, 17.66530133659708923, -12.81628187352647252 ) ) ;
#4606 = CARTESIAN_POINT ( 'NONE',  ( 7.361572987183170547, 52.05059781766745175, 9.846743663894590881 ) ) ;
#4608 =( LENGTH_UNIT ( ) NAMED_UNIT ( * ) SI_UNIT ( .MILLI., .METRE. ) );
#4609 = EDGE_CURVE ( 'NONE', #15452, #82266, #97377, .T. ) ;
#4610 = CARTESIAN_POINT ( 'NONE',  ( 19.38216949554541557, 17.24863466993041783, -9.382169495545420901 ) ) ;
#4611 = ORIENTED_EDGE ( 'NONE', *, *, #67459, .T. ) ;
#4612 = CARTESIAN_POINT ( 'NONE',  ( 19.84674366389459621, 33.50893115100078745, 7.409399052514197653E-17 ) ) ;
#4613 = CARTESIAN_POINT ( 'NONE',  ( 10.00000000000000178, 63.05374883491396076, 14.16423886937410082 ) ) ;
#4614 = ORIENTED_EDGE ( 'NONE', *, *, #90296, .T. ) ;
#4615 = CARTESIAN_POINT ( 'NONE',  ( 20.88017736071110519, 5.563685344154838397, 2.639326808657452039E-16 ) ) ;
#4616 = ORIENTED_EDGE ( 'NONE', *, *, #36367, .F. ) ;
#4617 = CARTESIAN_POINT ( 'NONE',  ( 4.559911319644449179, 47.23035201082150536, -9.422509992056141925 ) ) ;
#4618 = CARTESIAN_POINT ( 'NONE',  ( 17.96484262340118221, 49.93868534415484106, 7.964842623401181321 ) ) ;
#4619 =( GEOMETRIC_REPRESENTATION_CONTEXT ( 3 ) GLOBAL_UNCERTAINTY_ASSIGNED_CONTEXT ( ( #16234 ) ) GLOBAL_UNIT_ASSIGNED_CONTEXT ( ( #80918, #73400, #81402 ) ) REPRESENTATION_CONTEXT ( 'NONE', 'WORKASPACE' ) );
#4620 = CARTESIAN_POINT ( 'NONE',  ( 15.44008868035555260, 54.73035201082150536, 9.422509992056143702 ) ) ;
#4621 = CARTESIAN_POINT ( 'NONE',  ( 0.5774900079438590739, 37.64701867748817676, -5.440088680355550821 ) ) ;
#4622 = CARTESIAN_POINT ( 'NONE',  ( 5.991992585808628036, 15.00000000000000000, -13.20401548210295140 ) ) ;
#4623 = VECTOR ( 'NONE', #31133, 1000.000000000000000 ) ;
#4624 = STYLED_ITEM ( 'NONE', ( #8786 ), #71604 ) ;
#4626 = ORIENTED_EDGE ( 'NONE', *, *, #54069, .T. ) ;
#4625 = CARTESIAN_POINT ( 'NONE',  ( -10.64017930668191170, 15.00000000000000000, -10.57291749337230158 ) ) ;
#4627 = CARTESIAN_POINT ( 'NONE',  ( 1.472469842513823179, 26.42559781766745175, 4.923371831947296329 ) ) ;
#4628 = ORIENTED_EDGE ( 'NONE', *, *, #66191, .F. ) ;
#4629 = CARTESIAN_POINT ( 'NONE',  ( 14.92337183194729988, 54.34226448433412315, -8.527530157486177487 ) ) ;
#4630 = DIRECTION ( 'NONE',  ( 0.000000000000000000, 1.000000000000000000, 0.000000000000000000 ) ) ;
#4631 = EDGE_CURVE ( 'NONE', #49611, #61145, #13868, .T. ) ;
#4632 = CARTESIAN_POINT ( 'NONE',  ( -5.112373461513591621, -25.53775085953292390, 2.750000000000000000 ) ) ;
#4633 = LINE ( 'NONE', #5616, #50786 ) ;
#4634 = CARTESIAN_POINT ( 'NONE',  ( 8.880000000000020322, 79.82179676972448590, -6.250000000000000000 ) ) ;
#4636 = CARTESIAN_POINT ( 'NONE',  ( 1.472469842513823179, 30.59226448433411960, -4.923371831947296329 ) ) ;
#4635 = CARTESIAN_POINT ( 'NONE',  ( 0.1532563361054083140, 66.00893115100079456, 1.131784320476157264E-15 ) ) ;
#4637 = CARTESIAN_POINT ( 'NONE',  ( 24.16423886937410614, 59.30374883491397497, 8.672049930838204340E-16 ) ) ;
#4638 = CARTESIAN_POINT ( 'NONE',  ( -14.02068044289382875, 15.00000000000000000, 5.331089937175565119 ) ) ;
#4639 = ORIENTED_EDGE ( 'NONE', *, *, #37254, .F. ) ;
#4640 = CARTESIAN_POINT ( 'NONE',  ( -5.204170427930421283E-15, 3.438309369127513726, -11.92686044187656513 ) ) ;
#4641 = CARTESIAN_POINT ( 'NONE',  ( 17.20831665107776587, 32.88393115100078745, 7.208316651077764980 ) ) ;
#4642 = CARTESIAN_POINT ( 'NONE',  ( -2.816281873526473856, 59.33196800326374643, 3.434112377981055619 ) ) ;
#4643 = CARTESIAN_POINT ( 'NONE',  ( 0.6178305044545838731, -0.2513653300695798953, 9.382169495545420901 ) ) ;
#4644 = CARTESIAN_POINT ( 'NONE',  ( 17.20831665107776587, 14.13393115100078568, -7.208316651077762316 ) ) ;
#4645 =( GEOMETRIC_REPRESENTATION_CONTEXT ( 3 ) GLOBAL_UNCERTAINTY_ASSIGNED_CONTEXT ( ( #48187 ) ) GLOBAL_UNIT_ASSIGNED_CONTEXT ( ( #24067, #98612, #67594 ) ) REPRESENTATION_CONTEXT ( 'NONE', 'WORKASPACE' ) );
#4646 = CARTESIAN_POINT ( 'NONE',  ( -4.096035146093346846, 4.802464241948007172E-16, -13.90943910019264429 ) ) ;
#4647 = ADVANCED_FACE ( 'NONE', ( #30824 ), #22856, .T. ) ;
#4648 = CARTESIAN_POINT ( 'NONE',  ( 17.20831665107776587, 7.883931151000784787, 7.208316651077764980 ) ) ;
#4649 = CARTESIAN_POINT ( 'NONE',  ( 5.076628168052704559, 65.17559781766745175, -8.527530157486179263 ) ) ;
#4650 = CARTESIAN_POINT ( 'NONE',  ( -2.253458813454140675, 12.77999999999999936, 10.00000000000000000 ) ) ;
#4651 = ADVANCED_FACE ( 'NONE', ( #91330 ), #60829, .T. ) ;
#4652 = EDGE_CURVE ( 'NONE', #5883, #49695, #54310, .T. ) ;
#4653 = EDGE_LOOP ( 'NONE', ( #16581, #78021, #48136, #88770 ) ) ;
#4654 = CARTESIAN_POINT ( 'NONE',  ( -0.8801773607111009756, 8.063685344154837509, 1.068504757029289695E-15 ) ) ;
#4655 = CARTESIAN_POINT ( 'NONE',  ( 10.00000000000000000, 10.55374883491396787, -14.16423886937410082 ) ) ;
#4656 = CARTESIAN_POINT ( 'NONE',  ( 12.63842701281683922, 9.550597817667449974, -9.846743663894590881 ) ) ;
#4657 = CARTESIAN_POINT ( 'NONE',  ( 4.559911319644449179, 53.89701867748817676, 9.422509992056141925 ) ) ;
#4659 = CARTESIAN_POINT ( 'NONE',  ( 15.44008868035555260, 64.73035201082151957, 9.422509992056143702 ) ) ;
#4658 = CARTESIAN_POINT ( 'NONE',  ( 22.81628187352648496, 21.83196800326374643, -3.434112377981050290 ) ) ;
#4660 = DIRECTION ( 'NONE',  ( 0.000000000000000000, 1.000000000000000000, 0.000000000000000000 ) ) ;
#4661 =( NAMED_UNIT ( * ) SI_UNIT ( $, .STERADIAN. ) SOLID_ANGLE_UNIT ( ) );
#4662 = AXIS2_PLACEMENT_3D ( 'NONE', #16118, #55599, #77587 ) ;
#4663 = CARTESIAN_POINT ( 'NONE',  ( 19.38216949554541557, 7.248634669930421381, -9.382169495545420901 ) ) ;
#4664 = CARTESIAN_POINT ( 'NONE',  ( 6.565887622018943937, 0.1653013365970866511, 12.81628187352647430 ) ) ;
#4665 = CARTESIAN_POINT ( 'NONE',  ( 12.63842701281683922, 9.550597817667449974, -9.846743663894590881 ) ) ;
#4666 = CARTESIAN_POINT ( 'NONE',  ( 10.88017736071109987, -19.22798132251182324, -2.915334737309928315 ) ) ;
#4667 = CARTESIAN_POINT ( 'NONE',  ( 6.565887622018943937, 25.16530133659708213, 12.81628187352647430 ) ) ;
#4668 = CARTESIAN_POINT ( 'NONE',  ( -11.63911236827289919, -77.84336773400825393, -3.999999999996396216 ) ) ;
#4669 = APPLICATION_CONTEXT ( 'automotive_design' ) ;
#4670 = CARTESIAN_POINT ( 'NONE',  ( 0.5774900079438607392, 33.48035201082150536, 5.440088680355550821 ) ) ;
#4671 = DIRECTION ( 'NONE',  ( 0.9099612708765425495, -0.000000000000000000, 0.4146932426562403018 ) ) ;
#4672 = CARTESIAN_POINT ( 'NONE',  ( 20.36894250292379382, 48.67874883491396076, 10.36894250292379205 ) ) ;
#4673 = CARTESIAN_POINT ( 'NONE',  ( -1.783843307429720415, 13.12729635533385597, 9.500000000000000000 ) ) ;
#4674 = CARTESIAN_POINT ( 'NONE',  ( 6.565887622018943937, 38.08196800326376064, -12.81628187352647608 ) ) ;
#4675 = CARTESIAN_POINT ( 'NONE',  ( -0.8801773607111009756, 33.06368534415484106, 1.068504757029289695E-15 ) ) ;
#4676 = CARTESIAN_POINT ( 'NONE',  ( 0.1532563361054082862, 46.21726448433411605, 2.638427012816831674 ) ) ;
#4677 = CARTESIAN_POINT ( 'NONE',  ( 4.559911319644449179, 48.89701867748817676, 9.422509992056141925 ) ) ;
#4678 = CARTESIAN_POINT ( 'NONE',  ( 24.16423886937410614, 39.30374883491396787, 8.672049930838204340E-16 ) ) ;
#4679 = DIRECTION ( 'NONE',  ( 0.7372773368101250835, 0.000000000000000000, 0.6755902076156591329 ) ) ;
#4680 = CARTESIAN_POINT ( 'NONE',  ( 10.00000000000000178, 32.25893115100078745, 9.846743663894594434 ) ) ;
#4681 = CARTESIAN_POINT ( 'NONE',  ( 0.6178305044545838731, 64.74863466993043914, 9.382169495545420901 ) ) ;
#4682 = CARTESIAN_POINT ( 'NONE',  ( 10.00000000000000000, 64.75893115100078035, -9.846743663894594434 ) ) ;
#4683 = VERTEX_POINT ( 'NONE', #853 ) ;
#4684 = ADVANCED_FACE ( 'NONE', ( #83837 ), #15847, .F. ) ;
#4685 = CARTESIAN_POINT ( 'NONE',  ( 8.375939845167756914, 15.00000000000000000, -11.52849216984298941 ) ) ;
#4686 = CARTESIAN_POINT ( 'NONE',  ( 6.732888861736110009, -58.30752899003807954, 2.750000000000000000 ) ) ;
#4687 = CARTESIAN_POINT ( 'NONE',  ( 19.42250999205614548, 15.98035201082150714, -5.440088680355545492 ) ) ;
#4688 = CARTESIAN_POINT ( 'NONE',  ( 20.88017736071110164, 60.35535201082151957, 2.915334737309930979 ) ) ;
#4689 =( GEOMETRIC_REPRESENTATION_CONTEXT ( 3 ) GLOBAL_UNCERTAINTY_ASSIGNED_CONTEXT ( ( #64161 ) ) GLOBAL_UNIT_ASSIGNED_CONTEXT ( ( #36300, #4828, #51301 ) ) REPRESENTATION_CONTEXT ( 'NONE', 'WORKASPACE' ) );
#4690 = CARTESIAN_POINT ( 'NONE',  ( 20.36894250292379738, 24.92874883491396787, -10.36894250292379027 ) ) ;
#4691 = CARTESIAN_POINT ( 'NONE',  ( 2.791683348922240793, 16.63393115100078745, 7.208316651077764092 ) ) ;
#4692 = CARTESIAN_POINT ( 'NONE',  ( 7.361572987183170547, 67.05059781766746596, 9.846743663894590881 ) ) ;
#4693 = CARTESIAN_POINT ( 'NONE',  ( 7.084665262690076126, 32.02201867748816966, -10.88017736071110164 ) ) ;
#4694 = FACE_OUTER_BOUND ( 'NONE', #6859, .T. ) ;
#4695 = CARTESIAN_POINT ( 'NONE',  ( -4.494156999534613561, 0.000000000000000000, 3.088748530746243670 ) ) ;
#4696 = AXIS2_PLACEMENT_3D ( 'NONE', #8045, #84038, #91032 ) ;
#4697 = VERTEX_POINT ( 'NONE', #75340 ) ;
#4698 = DIRECTION ( 'NONE',  ( 1.000000000000000000, 0.000000000000000000, 0.000000000000000000 ) ) ;
#4699 = CARTESIAN_POINT ( 'NONE',  ( 0.1532563361054100626, 45.80059781766745886, -2.638427012816831230 ) ) ;
#4700 = VERTEX_POINT ( 'NONE', #15362 ) ;
#4701 = VERTEX_POINT ( 'NONE', #67859 ) ;
#4702 = DIRECTION ( 'NONE',  ( -0.000000000000000000, 1.000000000000000000, 0.000000000000000000 ) ) ;
#4703 = CARTESIAN_POINT ( 'NONE',  ( -4.164238869374099039, 11.80374883491396965, 8.674139862899312516E-16 ) ) ;
#4704 = CARTESIAN_POINT ( 'NONE',  ( 24.16423886937409904, 9.095415501580633943, 3.795296366450317205 ) ) ;
#4705 = CARTESIAN_POINT ( 'NONE',  ( 19.42250999205614548, 50.98035201082151247, -5.440088680355545492 ) ) ;
#4706 = CARTESIAN_POINT ( 'NONE',  ( 22.26659068614894466, 48.88708216824730357, 7.082119434687054849 ) ) ;
#4707 = CARTESIAN_POINT ( 'NONE',  ( 0.6178305044545838731, -0.2513653300695798953, 9.382169495545420901 ) ) ;
#4708 = CARTESIAN_POINT ( 'NONE',  ( 17.20831665107776587, 34.13393115100078745, -7.208316651077762316 ) ) ;
#4709 = FILL_AREA_STYLE ('',( #82655 ) ) ;
#4711 = CARTESIAN_POINT ( 'NONE',  ( 0.6178305044545838731, 9.748634669930416052, 9.382169495545420901 ) ) ;
#4710 = CARTESIAN_POINT ( 'NONE',  ( -0.8801773607111009756, 28.06368534415484106, 1.068504757029289695E-15 ) ) ;
#4712 = CARTESIAN_POINT ( 'NONE',  ( 24.16423886937409904, 4.095415501580634832, 3.795296366450317205 ) ) ;
#4713 = CARTESIAN_POINT ( 'NONE',  ( -4.164238869374099039, 46.80374883491397497, 8.674139862899312516E-16 ) ) ;
#4714 = CARTESIAN_POINT ( 'NONE',  ( -4.164238869374099039, 66.80374883491396076, 8.674139862899312516E-16 ) ) ;
#4715 = CARTESIAN_POINT ( 'NONE',  ( -1.926860441876564023, 67.87045670184116375, 3.195792623639529761 ) ) ;
#4716 = CARTESIAN_POINT ( 'NONE',  ( -10.77730536144846596, -98.63085534186639336, 4.000000000000000000 ) ) ;
#4717 = ORIENTED_EDGE ( 'NONE', *, *, #92517, .F. ) ;
#4718 = CARTESIAN_POINT ( 'NONE',  ( 8.629999999999995453, 41.24999999999999289, 6.250000000000000000 ) ) ;
#4719 = ORIENTED_EDGE ( 'NONE', *, *, #18023, .F. ) ;
#4720 = ORIENTED_EDGE ( 'NONE', *, *, #82743, .F. ) ;
#4721 = CARTESIAN_POINT ( 'NONE',  ( -4.164238869374099039, 51.80374883491396787, 8.674139862899312516E-16 ) ) ;
#4722 = CARTESIAN_POINT ( 'NONE',  ( 5.076628168052703671, 51.84226448433412315, 8.527530157486179263 ) ) ;
#4723 = CARTESIAN_POINT ( 'NONE',  ( -0.8801773607111009756, 58.06368534415484106, 1.068504757029289695E-15 ) ) ;
#4724 = AXIS2_PLACEMENT_3D ( 'NONE', #49432, #79936, #85981 ) ;
#4725 = DIRECTION ( 'NONE',  ( -0.000000000000000000, -1.000000000000000000, -0.000000000000000000 ) ) ;
#4726 = CARTESIAN_POINT ( 'NONE',  ( 17.96484262340118221, 54.93868534415484106, 7.964842623401181321 ) ) ;
#4727 = CARTESIAN_POINT ( 'NONE',  ( 9.382169495545419124, 5.998634669930423158, 9.382169495545417348 ) ) ;
#4728 = ORIENTED_EDGE ( 'NONE', *, *, #92365, .F. ) ;
#4729 = CARTESIAN_POINT ( 'NONE',  ( 10.00000000000000178, 23.05374883491397142, 14.16423886937410082 ) ) ;
#4730 = CARTESIAN_POINT ( 'NONE',  ( 6.565887622018943937, 30.16530133659708568, 12.81628187352647430 ) ) ;
#4731 = ORIENTED_EDGE ( 'NONE', *, *, #94472, .F. ) ;
#4732 = CARTESIAN_POINT ( 'NONE',  ( 13.43411237798105340, 50.58196800326375353, 12.81628187352647963 ) ) ;
#4733 = AXIS2_PLACEMENT_3D ( 'NONE', #83346, #98378, #92318 ) ;
#4734 = CARTESIAN_POINT ( 'NONE',  ( 15.44008868035555260, 19.73035201082150536, 9.422509992056143702 ) ) ;
#4735 = CARTESIAN_POINT ( 'NONE',  ( 5.076628168052703671, 41.84226448433411605, 8.527530157486179263 ) ) ;
#4736 = CARTESIAN_POINT ( 'NONE',  ( 0.5774900079438607392, 13.48035201082150358, 5.440088680355550821 ) ) ;
#4737 = CARTESIAN_POINT ( 'NONE',  ( 0.1532563361054082862, 41.21726448433411605, 2.638427012816831674 ) ) ;
#4739 = ORIENTED_EDGE ( 'NONE', *, *, #87973, .F. ) ;
#4738 = CARTESIAN_POINT ( 'NONE',  ( 12.60874940350947959, 4.146618495107105809E-16, -7.160268045227032196 ) ) ;
#4740 = CARTESIAN_POINT ( 'NONE',  ( 0.000000000000000000, 14.49999999999999822, 0.000000000000000000 ) ) ;
#4741 = CARTESIAN_POINT ( 'NONE',  ( 15.44008868035555793, 66.39701867748817676, -9.422509992056140149 ) ) ;
#4742 = CARTESIAN_POINT ( 'NONE',  ( 19.72487221294570858, 69.50000000000000000, 6.500000000000000888 ) ) ;
#4743 = DIRECTION ( 'NONE',  ( 0.000000000000000000, 0.000000000000000000, 1.000000000000000000 ) ) ;
#4744 = CARTESIAN_POINT ( 'NONE',  ( 19.84674366389459266, 23.30059781766745530, 2.638427012816836559 ) ) ;
#4745 = CARTESIAN_POINT ( 'NONE',  ( 3.591859063236763294, 23.29030133659708568, -11.09922568453595026 ) ) ;
#4746 = ORIENTED_EDGE ( 'NONE', *, *, #35243, .T. ) ;
#4747 = CARTESIAN_POINT ( 'NONE',  ( 10.00000000000000000, 39.75893115100078745, -9.846743663894594434 ) ) ;
#4748 = CARTESIAN_POINT ( 'NONE',  ( 13.48255862862752430, 15.00000000000000000, -5.335786055104087211 ) ) ;
#4749 = CARTESIAN_POINT ( 'NONE',  ( 17.08211943468705840, 25.13708216824730357, -12.26659068614894466 ) ) ;
#4750 = CARTESIAN_POINT ( 'NONE',  ( 19.84674366389459266, 33.71726448433410894, -2.638427012816827677 ) ) ;
#4751 = CARTESIAN_POINT ( 'NONE',  ( 10.00000000000000178, 45.37363466993041783, 12.81628187352647608 ) ) ;
#4753 = CARTESIAN_POINT ( 'NONE',  ( 19.50000000000000000, 3.304235192336776005E-17, -4.500000000000001776 ) ) ;
#4752 = CARTESIAN_POINT ( 'NONE',  ( 8.979999999999991545, 18.00000000000000355, -2.900000000000000799 ) ) ;
#4754 = CARTESIAN_POINT ( 'NONE',  ( 17.96484262340118221, 61.18868534415482685, -7.964842623401177768 ) ) ;
#4755 = EDGE_CURVE ( 'NONE', #29308, #48625, #45847, .T. ) ;
#4756 = CARTESIAN_POINT ( 'NONE',  ( -2.816281873526473856, 14.33196800326375531, 3.434112377981055619 ) ) ;
#4757 = CARTESIAN_POINT ( 'NONE',  ( 4.999999999999999112, 60.50000000000000000, -6.500000000000000888 ) ) ;
#4758 = CARTESIAN_POINT ( 'NONE',  ( 10.00000000000000000, 39.75893115100078745, -9.846743663894594434 ) ) ;
#4759 = CARTESIAN_POINT ( 'NONE',  ( 4.559911319644449179, 37.23035201082150536, -9.422509992056141925 ) ) ;
#4760 = CARTESIAN_POINT ( 'NONE',  ( 10.00000000000000178, 25.37363466993041783, 12.81628187352647608 ) ) ;
#4761 = CARTESIAN_POINT ( 'NONE',  ( 5.076628168052703671, 31.84226448433412315, 8.527530157486179263 ) ) ;
#4762 =( LENGTH_UNIT ( ) NAMED_UNIT ( * ) SI_UNIT ( .MILLI., .METRE. ) );
#4763 = CARTESIAN_POINT ( 'NONE',  ( -13.05265508282193920, 90.73577164613084278, 7.477963345815892282 ) ) ;
#4764 = EDGE_CURVE ( 'NONE', #82054, #63150, #83025, .T. ) ;
#4765 = CARTESIAN_POINT ( 'NONE',  ( 10.00000000000000000, 26.81368534415484106, -10.88017736071110342 ) ) ;
#4766 = EDGE_CURVE ( 'NONE', #75327, #39241, #33467, .T. ) ;
#4767 = FACE_OUTER_BOUND ( 'NONE', #78218, .T. ) ;
#4769 = CARTESIAN_POINT ( 'NONE',  ( 12.91533473730992121, 29.52201867748817321, 10.88017736071110164 ) ) ;
#4768 = CARTESIAN_POINT ( 'NONE',  ( 19.84674366389459266, 53.30059781766744464, 2.638427012816836559 ) ) ;
#4770 = CARTESIAN_POINT ( 'NONE',  ( 2.035157376598822676, 62.43868534415483396, -7.964842623401177768 ) ) ;
#4771 = AXIS2_PLACEMENT_3D ( 'NONE', #57895, #5901, #5422 ) ;
#4773 = CARTESIAN_POINT ( 'NONE',  ( 3.640395162852212874, 107.5383484153110203, -12.00000000000000000 ) ) ;
#4772 = CARTESIAN_POINT ( 'NONE',  ( 10.00000000000000178, 29.31368534415483751, 10.88017736071110342 ) ) ;
#4774 = PRESENTATION_STYLE_ASSIGNMENT (( #88750 ) ) ;
#4775 = CARTESIAN_POINT ( 'NONE',  ( 2.791683348922237240, 30.38393115100078390, -7.208316651077763204 ) ) ;
#4776 = CARTESIAN_POINT ( 'NONE',  ( 5.076628168052704559, 45.17559781766745175, -8.527530157486179263 ) ) ;
#4777 = CIRCLE ( 'NONE', #12751, 2.899999999999999911 ) ;
#4778 = CARTESIAN_POINT ( 'NONE',  ( 22.26659068614895176, 54.72041550158063217, -7.082119434687042414 ) ) ;
#4779 = LINE ( 'NONE', #12262, #6644 ) ;
#4780 = VECTOR ( 'NONE', #71970, 1000.000000000000114 ) ;
#4781 = CARTESIAN_POINT ( 'NONE',  ( -2.266590686148945544, 12.22041550158063394, 7.082119434687048631 ) ) ;
#4782 = CARTESIAN_POINT ( 'NONE',  ( -0.3689425029237898834, 41.17874883491397497, -10.36894250292378850 ) ) ;
#4783 = CARTESIAN_POINT ( 'NONE',  ( 21.09922568453594849, 11.20696800326375531, 6.408140936763242479 ) ) ;
#4784 = LINE ( 'NONE', #12267, #31352 ) ;
#4785 = CARTESIAN_POINT ( 'NONE',  ( -0.8801773607111009756, 18.06368534415484106, 1.068504757029289695E-15 ) ) ;
#4786 = CARTESIAN_POINT ( 'NONE',  ( 17.20831665107776587, 37.88393115100078745, 7.208316651077764980 ) ) ;
#4787 = LINE ( 'NONE', #20771, #96275 ) ;
#4788 = CARTESIAN_POINT ( 'NONE',  ( 10.00000000000000178, 64.31368534415483396, 10.88017736071110342 ) ) ;
#4789 = FILL_AREA_STYLE_COLOUR ( '', #93108 ) ;
#4790 = CARTESIAN_POINT ( 'NONE',  ( 13.43411237798105340, 60.58196800326376064, 12.81628187352647963 ) ) ;
#4791 = CARTESIAN_POINT ( 'NONE',  ( -1.099225684535947600, 24.54030133659708923, 6.408140936763237150 ) ) ;
#4792 = CARTESIAN_POINT ( 'NONE',  ( 14.92337183194729988, 34.34226448433411605, -8.527530157486177487 ) ) ;
#4793 = ORIENTED_EDGE ( 'NONE', *, *, #98702, .F. ) ;
#4794 = SURFACE_SIDE_STYLE ('',( #80784 ) ) ;
#4795 = EDGE_CURVE ( 'NONE', #96981, #27072, #60342, .T. ) ;
#4796 = CARTESIAN_POINT ( 'NONE',  ( 18.17829156368507526, 4.167925641218962696, 6.500000000000000888 ) ) ;
#4797 = CARTESIAN_POINT ( 'NONE',  ( 20.88017736071110164, 5.355352010821503583, 2.915334737309930979 ) ) ;
#4798 = CARTESIAN_POINT ( 'NONE',  ( 4.559911319644449179, 12.23035201082150536, -9.422509992056141925 ) ) ;
#4799 = CARTESIAN_POINT ( 'NONE',  ( 17.08211943468705840, 45.13708216824730357, -12.26659068614894466 ) ) ;
#4800 = CARTESIAN_POINT ( 'NONE',  ( 12.91533473730992121, 34.52201867748817676, 10.88017736071110164 ) ) ;
#4801 = CARTESIAN_POINT ( 'NONE',  ( -0.8801773607111009756, 63.06368534415484106, 1.068504757029289695E-15 ) ) ;
#4802 = PLANE ( 'NONE',  #6401 ) ;
#4803 = VECTOR ( 'NONE', #82347, 1000.000000000000000 ) ;
#4804 = LINE ( 'NONE', #27779, #1792 ) ;
#4805 = CARTESIAN_POINT ( 'NONE',  ( 10.00000000000000000, 14.75893115100078568, -9.846743663894594434 ) ) ;
#4806 =( LENGTH_UNIT ( ) NAMED_UNIT ( * ) SI_UNIT ( .MILLI., .METRE. ) );
#4807 = CARTESIAN_POINT ( 'NONE',  ( 12.63842701281683034, 7.467264484334118713, 9.846743663894596210 ) ) ;
#4808 = DIRECTION ( 'NONE',  ( -0.000000000000000000, -1.000000000000000000, 0.000000000000000000 ) ) ;
#4809 = CARTESIAN_POINT ( 'NONE',  ( 14.92337183194729988, 34.34226448433411605, -8.527530157486177487 ) ) ;
#4810 = CARTESIAN_POINT ( 'NONE',  ( -2.816281873526473856, -0.8763653300695799508, 9.499525473075851096E-16 ) ) ;
#4811 = CARTESIAN_POINT ( 'NONE',  ( 10.00000000000000178, 24.31368534415484106, 10.88017736071110342 ) ) ;
#4812 = EDGE_CURVE ( 'NONE', #11855, #33481, #21871, .T. ) ;
#4813 = ORIENTED_EDGE ( 'NONE', *, *, #70131, .F. ) ;
#4814 = CARTESIAN_POINT ( 'NONE',  ( 21.09922568453594849, 46.20696800326376064, 6.408140936763242479 ) ) ;
#4815 = CARTESIAN_POINT ( 'NONE',  ( -46.70923076923077133, 98.84615384615385381, -9.500000000000000000 ) ) ;
#4816 = CARTESIAN_POINT ( 'NONE',  ( 10.00000000000000000, -0.2410688489992152128, -9.846743663894594434 ) ) ;
#4817 = CARTESIAN_POINT ( 'NONE',  ( 22.81628187352647785, 41.62363466993042493, 6.195893100308588602E-16 ) ) ;
#4819 = CARTESIAN_POINT ( 'NONE',  ( 10.00000000000000000, 29.75893115100078745, -9.846743663894594434 ) ) ;
#4818 = CARTESIAN_POINT ( 'NONE',  ( -2.266590686148945544, 61.38708216824730357, -7.082119434687050408 ) ) ;
#4820 = DIRECTION ( 'NONE',  ( 0.6626200482157357241, -0.000000000000000000, 0.7489557207890036317 ) ) ;
#4821 = CARTESIAN_POINT ( 'NONE',  ( 19.84674366389459266, 58.71726448433411605, -2.638427012816827677 ) ) ;
#4822 = CARTESIAN_POINT ( 'NONE',  ( -0.3689425029237881626, 17.42874883491397142, 10.36894250292379027 ) ) ;
#4823 = CARTESIAN_POINT ( 'NONE',  ( 24.16423886937409904, 34.09541550158064638, 3.795296366450317205 ) ) ;
#4824 = CARTESIAN_POINT ( 'NONE',  ( 10.00000000000000000, 49.75893115100078745, -9.846743663894594434 ) ) ;
#4825 = CARTESIAN_POINT ( 'NONE',  ( -0.2002492713866858565, 69.97537705844109723, 6.181741512438951425 ) ) ;
#4826 = CARTESIAN_POINT ( 'NONE',  ( 7.084665262690076126, 42.02201867748816966, -10.88017736071110164 ) ) ;
#4827 = CARTESIAN_POINT ( 'NONE',  ( 4.559911319644449179, 52.23035201082151247, -9.422509992056141925 ) ) ;
#4828 =( NAMED_UNIT ( * ) PLANE_ANGLE_UNIT ( ) SI_UNIT ( $, .RADIAN. ) );
#4829 = ORIENTED_EDGE ( 'NONE', *, *, #58243, .F. ) ;
#4830 = CARTESIAN_POINT ( 'NONE',  ( 22.81628187352647785, 41.41530133659708923, 3.434112377981063169 ) ) ;
#4831 = CARTESIAN_POINT ( 'NONE',  ( 12.63842701281683034, 2.467264484334118269, 9.846743663894596210 ) ) ;
#4832 = ORIENTED_EDGE ( 'NONE', *, *, #8372, .T. ) ;
#4833 = LINE ( 'NONE', #24027, #89754 ) ;
#4834 = CARTESIAN_POINT ( 'NONE',  ( 13.61464873478171178, 14.63606918187825201, -6.296136897217842865 ) ) ;
#4835 = DIRECTION ( 'NONE',  ( -0.000000000000000000, -1.000000000000000000, -0.000000000000000000 ) ) ;
#4836 = ORIENTED_EDGE ( 'NONE', *, *, #97835, .T. ) ;
#4837 = AXIS2_PLACEMENT_3D ( 'NONE', #3709, #88659, #96178 ) ;
#4838 = DIRECTION ( 'NONE',  ( 0.000000000000000000, 1.000000000000000000, -0.000000000000000000 ) ) ;
#4839 = CARTESIAN_POINT ( 'NONE',  ( 19.42250999205614548, 15.98035201082150714, -5.440088680355545492 ) ) ;
#4840 = CARTESIAN_POINT ( 'NONE',  ( -10.32896413005679470, 13.07879003517447458, 5.963430220938290560 ) ) ;
#4841 = CARTESIAN_POINT ( 'NONE',  ( -0.3689425029237898834, 21.17874883491396432, -10.36894250292378850 ) ) ;
#4842 = CARTESIAN_POINT ( 'NONE',  ( 7.084665262690076126, 19.10535201082150181, 10.88017736071109987 ) ) ;
#4843 = CARTESIAN_POINT ( 'NONE',  ( 14.92337183194729633, 57.67559781766745886, 8.527530157486181039 ) ) ;
#4844 = ORIENTED_EDGE ( 'NONE', *, *, #25859, .F. ) ;
#4845 = AXIS2_PLACEMENT_3D ( 'NONE', #76117, #69606, #55077 ) ;
#4846 = CARTESIAN_POINT ( 'NONE',  ( 17.20831665107776587, 62.88393115100078745, 7.208316651077764980 ) ) ;
#4847 = VERTEX_POINT ( 'NONE', #61812 ) ;
#4848 = EDGE_CURVE ( 'NONE', #14809, #75433, #98872, .T. ) ;
#4849 = CARTESIAN_POINT ( 'NONE',  ( -0.8801773607110991993, 52.85535201082151247, -2.915334737309923874 ) ) ;
#4850 = CARTESIAN_POINT ( 'NONE',  ( 0.1532563361054082862, 61.21726448433412315, 2.638427012816831674 ) ) ;
#4851 = CARTESIAN_POINT ( 'NONE',  ( -2.816281873526473856, 34.12363466993042493, 9.499525473075851096E-16 ) ) ;
#4853 = CARTESIAN_POINT ( 'NONE',  ( -10.29975640502598289, 43.93058911311638326, 0.000000000000000000 ) ) ;
#4852 = CARTESIAN_POINT ( 'NONE',  ( 12.91533473730992121, 9.522018677488171434, 10.88017736071110164 ) ) ;
#4854 = CARTESIAN_POINT ( 'NONE',  ( 2.791683348922237240, 5.383931151000785675, -7.208316651077763204 ) ) ;
#4855 = VECTOR ( 'NONE', #70283, 1000.000000000000000 ) ;
#4856 = CARTESIAN_POINT ( 'NONE',  ( -0.8801773607111009756, 23.06368534415484106, 1.068504757029289695E-15 ) ) ;
#4857 = EDGE_CURVE ( 'NONE', #52732, #40706, #19125, .T. ) ;
#4858 = EDGE_LOOP ( 'NONE', ( #269, #32627, #83795, #19104 ) ) ;
#4859 = CARTESIAN_POINT ( 'NONE',  ( -2.816281873526473856, 59.12363466993042493, 9.499525473075851096E-16 ) ) ;
#4860 = CARTESIAN_POINT ( 'NONE',  ( 12.91533473730992121, 29.52201867748817321, 10.88017736071110164 ) ) ;
#4861 = CARTESIAN_POINT ( 'NONE',  ( 19.65595853167378948, 92.20263838533996648, 5.361990343729008401 ) ) ;
#4862 = CARTESIAN_POINT ( 'NONE',  ( 10.00000000000000178, 40.37363466993042493, 12.81628187352647608 ) ) ;
#4863 = CARTESIAN_POINT ( 'NONE',  ( 7.084665262690076126, 52.02201867748816255, -10.88017736071110164 ) ) ;
#4864 = CARTESIAN_POINT ( 'NONE',  ( 19.84674366389459621, 53.50893115100078745, 7.409399052514197653E-17 ) ) ;
#4865 = VERTEX_POINT ( 'NONE', #29834 ) ;
#4866 = CARTESIAN_POINT ( 'NONE',  ( -0.03743638938522138304, 49.25197528031019090, -6.399506433553975526 ) ) ;
#4867 = CARTESIAN_POINT ( 'NONE',  ( 17.20831665107776587, 9.133931151000787452, -7.208316651077762316 ) ) ;
#4868 = CARTESIAN_POINT ( 'NONE',  ( 7.361572987183170547, 67.05059781766746596, 9.846743663894590881 ) ) ;
#4870 = CARTESIAN_POINT ( 'NONE',  ( 14.92337183194729988, 49.34226448433411605, -8.527530157486177487 ) ) ;
#4869 = CARTESIAN_POINT ( 'NONE',  ( 17.39651004071841811, 4.082109641433293135, -6.499999999999999112 ) ) ;
#4871 = CARTESIAN_POINT ( 'NONE',  ( 19.42250999205614548, 15.98035201082150714, -5.440088680355545492 ) ) ;
#4872 = CARTESIAN_POINT ( 'NONE',  ( 5.076628168052703671, 36.84226448433412315, 8.527530157486179263 ) ) ;
#4873 = CARTESIAN_POINT ( 'NONE',  ( 2.618367889266248100E-15, 44.99999999999999289, -7.000000000000000000 ) ) ;
#4874 = SURFACE_STYLE_FILL_AREA ( #50350 ) ;
#4876 = CARTESIAN_POINT ( 'NONE',  ( 18.52753015748617571, 8.092264484334117824, 4.923371831947298993 ) ) ;
#4875 = CARTESIAN_POINT ( 'NONE',  ( 0.1532563361054082862, 41.21726448433411605, 2.638427012816831674 ) ) ;
#4878 = EDGE_LOOP ( 'NONE', ( #22808, #90174, #23553, #77987 ) ) ;
#4877 = CARTESIAN_POINT ( 'NONE',  ( 19.84674366389459266, 53.30059781766744464, 2.638427012816836559 ) ) ;
#4879 = CYLINDRICAL_SURFACE ( 'NONE', #7182, 15.00000000000000000 ) ;
#4880 = EDGE_CURVE ( 'NONE', #84834, #53609, #31354, .T. ) ;
#4881 = VECTOR ( 'NONE', #65106, 1000.000000000000000 ) ;
#4882 = CARTESIAN_POINT ( 'NONE',  ( -1.099225684535947600, 38.70696800326375353, -6.408140936763238038 ) ) ;
#4883 = CARTESIAN_POINT ( 'NONE',  ( 1.472469842513823179, 46.42559781766745175, 4.923371831947296329 ) ) ;
#4884 = CYLINDRICAL_SURFACE ( 'NONE', #21739, 11.25000000000000178 ) ;
#4885 = CARTESIAN_POINT ( 'NONE',  ( 22.26659068614895176, 59.72041550158063927, -7.082119434687042414 ) ) ;
#4886 = CARTESIAN_POINT ( 'NONE',  ( 5.076628168052703671, 31.84226448433412315, 8.527530157486179263 ) ) ;
#4887 = EDGE_CURVE ( 'NONE', #4978, #24202, #32405, .T. ) ;
#4888 = CARTESIAN_POINT ( 'NONE',  ( 20.00000000000000000, 88.20477317201525125, 5.338983947147861286 ) ) ;
#4889 = CARTESIAN_POINT ( 'NONE',  ( 2.917880565312948704, 52.63708216824730357, 12.26659068614894643 ) ) ;
#4890 = CARTESIAN_POINT ( 'NONE',  ( -5.999999999999994671, 43.00000000000000000, -6.500000000000000888 ) ) ;
#4891 = CARTESIAN_POINT ( 'NONE',  ( 20.88017736071110519, 20.56368534415484106, 2.639326808657452039E-16 ) ) ;
#4892 = CARTESIAN_POINT ( 'NONE',  ( -4.164238869374099927, 42.01208216824728936, 3.795296366450308767 ) ) ;
#4893 = CARTESIAN_POINT ( 'NONE',  ( 13.79529636645030344, 53.26208216824730357, 14.16423886937410614 ) ) ;
#4894 = CARTESIAN_POINT ( 'NONE',  ( 20.88017736071110519, 5.563685344154838397, 2.639326808657452039E-16 ) ) ;
#4895 = CARTESIAN_POINT ( 'NONE',  ( 19.84674366389459266, 18.30059781766745175, 2.638427012816836559 ) ) ;
#4896 = CARTESIAN_POINT ( 'NONE',  ( 6.565887622018943937, 0.1653013365970866511, 12.81628187352647430 ) ) ;
#4897 = CARTESIAN_POINT ( 'NONE',  ( 4.559911319644449179, 43.89701867748816966, 9.422509992056141925 ) ) ;
#4898 = CARTESIAN_POINT ( 'NONE',  ( 1.274849032794305170, 17.55509018479936145, -6.499999999999995559 ) ) ;
#4899 = CYLINDRICAL_SURFACE ( 'NONE', #2859, 0.09999999999999982514 ) ;
#4900 =( BOUNDED_SURFACE ( )  B_SPLINE_SURFACE ( 1, 2, ( 
 ( #35972, #66472, #88485, #28478, #20988, #51473, #81964, #87988, #5986, #36478, #66972, #42024, #19500, #97491, #19987, #72489, #4022, #34979, #50487, #64979, #80987, #4999, #11999, #35480, #42501, #65976, #84811, #69316, #70804, #16317, #69814, #47284, #91818, #38825, #61798, #54296, #77786, #8805, #15831, #45833, #92306, #21477, #59460, #46800, #838, #62287, #77293, #24320, #39318, #9797, #51976, #76804, #16809, #23833, #82462, #89961, #360, #61307, #23339, #32278, #31298, #1825, #85302, #1337, #15349, #31788, #92791, #85795, #54786, #9298, #39808, #38336, #17308, #53819, #70309, #76319, #62786, #47785, #28957, #84331, #24809, #7837, #30809, #93285, #68829, #46318, #8321, #55286, #78282, #40296, #49740, #95755, #33265, #79269, #57734, #4265, #63757, #72248, #34738, #3782, #41778, #3279, #26751, #34236, #64732, #80247, #2812, #50231, #80745, #72732, #25305, #40789, #11754, #10779, #19746, #27239, #41295, #71769, #55792, #18283, #64244, #17795, #49261, #42263, #79761, #56760, #33743, #42750, #87254, #95244, #19255, #94263, #94762, #26262, #18779, #65229, #11260, #86780, #48270, #57246, #93778, #32774, #87743, #88238, #12240, #2321, #63269, #86287, #78784, #10291, #48762, #71288, #25789, #56284, #35230, #43230, #5255, #96752, #50746, #6721, #74720, #81234, #98241, #82714, #43725, #44212, #97253, #74211, #83214, #28227, #4759, #96254, #29700, #12733, #6232, #58726, #73724, #75210, #89230, #35733, #14232, #51735, #29213, #60209, #90704, #22232, #5741, #97749, #36735, #67226, #52220, #66222, #52707, #14735, #44711, #27733, #20739, #37237, #81716, #73231, #65728, #51232, #36230, #58215, #13228, #66729, #88731, #21232, #67727, #82217, #28723, #59213, #20243, #89718, #13727, #90208, #59712, #21738, #76688, #69203, #62165, #23719, #30686, #60696, #8209, #37722, #75709, #727, #84214, #77179, #31183, #39200, #92193, #24688, #68226, #91702, #31673, #38704, #98746, #7223, #15227, #76207, #68706, #22721, #77667, #46682, #53204, #70186, #54665, #15720, #16200, #61673, #46205, #55160, #238, #30195, #91195, #1703, #83709, #8686, #61194, #45706, #47162, #23220, #7724, #85181, #54178, #1218, #32159, #62661, #93163, #38221, #9181, #53693, #16692, #92670, #84690, #69687, #24198, #39698, #85674, #45211, #3657, #10659, #25192, #4149, #10173, #25674, #78168, #71656, #34614, #17193, #48154, #11633, #47673, #86171, #56647, #9677, #70679, #55671, #94643, #40175, #11143, #64614, #42149, #78667, #94147, #72614, #19139, #40671, #87132, #49616, #18655, #49143, #57128, #65109, #57619, #56168, #3165, #79644, #33627, #86660, #41662, #2200, #87625 ),
 ( #80126, #71169, #17680, #95632, #26153, #72130, #27120, #32661, #63154, #2693, #93657, #18165, #33145, #34122, #48643, #63639, #64126, #95123, #79147, #26630, #41173, #81598, #96134, #75092, #81112, #96631, #50120, #43606, #6598, #88118, #20118, #82595, #19628, #58101, #28607, #80630, #42627, #27615, #66609, #12126, #82097, #36617, #14110, #50621, #66102, #44594, #90090, #12613, #59096, #21617, #89605, #21114, #89110, #13608, #51614, #44089, #67104, #88608, #37111, #67608, #59592, #73105, #43114, #97628, #28108, #98114, #29576, #58608, #20621, #4644, #5128, #51111, #35108, #36103, #29092, #97137, #74092, #13110, #65607, #5626, #74598, #6112, #73603, #52103, #35617, #84084, #77064, #38584, #45584, #75590, #91584, #52587, #90581, #15599, #121, #92070, #46082, #54062, #8088, #39577, #83090, #7608, #46563, #23100, #14619, #22107, #30075, #91076, #53080, #76079, #61562, #83592, #69082, #77546, #22603, #1093, #62050, #15107, #53571, #76570, #16077, #98626, #617, #45085, #60584, #84576, #23598, #9065, #38103, #8575, #68591, #30568, #70066, #31063, #16575, #39079, #1589, #69573, #60080, #31554, #92552, #7102, #24080, #37604, #54547, #61072, #85064, #68099, #47050, #32038, #34008, #33034, #87023, #94038, #17567, #10541, #79532, #93540, #70555, #18535, #72018, #56052, #24580, #33515, #78545, #87517, #80014, #41051, #2083, #19030, #86055, #63530, #32543, #25559, #18050, #64012, #86543, #49507, #94524, #63043, #49026, #26043, #17071, #48527, #56534, #11032, #71550, #11517, #3548, #62541, #95010, #93047, #9554, #3060, #41552, #64504, #25071, #26518, #79029, #57015, #42041, #48032, #71055, #72505, #55554, #55041, #85559, #47554, #78051, #40056, #10056, #40555, #2578, #5513, #20507, #12505, #73988, #4037, #43975, #35990, #96018, #43004, #4529, #57509, #21495, #73488, #44478, #34500, #42515, #89001, #5015, #74477, #27011, #21002, #81488, #36496, #72999, #43487, #95518, #88006, #34993, #12991, #64991, #97019, #51490, #97510, #65498, #81003, #59477, #6002, #27501, #66492, #66988, #28496, #58989, #35498, #89493, #81985, #13496, #28974, #57996, #51992, #82481, #89978, #19517, #88502, #14000, #65993, #50014, #80518, #96520, #27993, #12016, #20005, #58489, #50505, #50993, #84461, #53451, #30451, #14992, #16454, #60951, #15486, #91950, #37491, #83471, #7490, #3, #23482, #83960, #60466, #90461, #37986, #67485, #6483, #91460, #45463, #7974, #22986, #68965, #45969, #54434, #98007, #22487, #61444, #68477, #29460, #36988, #44968, #6987, #98506, #52472, #8453, #76459, #82977, #971, #15959, #75962, #38473, #497, #30946, #84943, #29960, #59968 ) ),
 .UNSPECIFIED., .F., .F., .F. ) 
 B_SPLINE_SURFACE_WITH_KNOTS ( ( 2, 2 ),
 ( 3, 2, 2, 2, 2, 2, 2, 2, 2, 2, 2, 2, 2, 2, 2, 2, 2, 2, 2, 2, 2, 2, 2, 2, 2, 2, 2, 2, 2, 2, 2, 2, 2, 2, 2, 2, 2, 2, 2, 2, 2, 2, 2, 2, 2, 2, 2, 2, 2, 2, 2, 2, 2, 2, 2, 2, 2, 2, 2, 2, 2, 2, 2, 2, 2, 2, 2, 2, 2, 2, 2, 2, 2, 2, 2, 2, 2, 2, 2, 2, 2, 2, 2, 2, 2, 2, 2, 2, 2, 2, 2, 2, 2, 2, 2, 2, 2, 2, 2, 2, 2, 2, 2, 2, 2, 2, 2, 2, 2, 2, 2, 2, 2, 2, 2, 2, 2, 2, 2, 2, 2, 2, 2, 2, 2, 2, 2, 2, 2, 2, 2, 2, 2, 2, 2, 2, 2, 2, 2, 2, 2, 2, 2, 2, 2, 2, 2, 2, 2, 2, 2, 2, 2, 2, 2, 2, 2, 2, 2, 2, 2, 2, 3 ),
 ( 0.000000000000000000, 1.000000000000000000 ),
 ( 0.000000000000000000, 0.005952380952380952051, 0.01190476190476190410, 0.01785714285714285615, 0.02380952380952380820, 0.02976190476190476025, 0.03571428571428571230, 0.04166666666666666435, 0.04761904761904761640, 0.05357142857142856845, 0.05952380952380952051, 0.06547619047619047949, 0.07142857142857142461, 0.07738095238095238360, 0.08333333333333332871, 0.08928571428571428770, 0.09523809523809523281, 0.1011904761904761918, 0.1071428571428571369, 0.1130952380952380959, 0.1190476190476190410, 0.1250000000000000000, 0.1309523809523809590, 0.1369047619047619180, 0.1428571428571428492, 0.1488095238095238082, 0.1547619047619047672, 0.1607142857142857262, 0.1666666666666666574, 0.1726190476190476164, 0.1785714285714285754, 0.1845238095238095344, 0.1904761904761904656, 0.1964285714285714246, 0.2023809523809523836, 0.2083333333333333426, 0.2142857142857142738, 0.2202380952380952328, 0.2261904761904761918, 0.2321428571428571508, 0.2380952380952380820, 0.2440476190476190410, 0.2500000000000000000, 0.2559523809523809312, 0.2619047619047619180, 0.2678571428571428492, 0.2738095238095238360, 0.2797619047619047672, 0.2857142857142856984, 0.2916666666666666852, 0.2976190476190476164, 0.3035714285714285476, 0.3095238095238095344, 0.3154761904761904656, 0.3214285714285714524, 0.3273809523809523836, 0.3333333333333333148, 0.3392857142857143016, 0.3452380952380952328, 0.3511904761904761640, 0.3571428571428571508, 0.3630952380952380820, 0.3690476190476190688, 0.3750000000000000000, 0.3809523809523809312, 0.3869047619047619180, 0.3928571428571428492, 0.3988095238095238360, 0.4047619047619047672, 0.4107142857142856984, 0.4166666666666666852, 0.4226190476190476164, 0.4285714285714285476, 0.4345238095238095344, 0.4404761904761904656, 0.4464285714285714524, 0.4523809523809523836, 0.4583333333333333148, 0.4642857142857143016, 0.4702380952380952328, 0.4761904761904761640, 0.4821428571428571508, 0.4880952380952380820, 0.4940476190476190688, 0.5000000000000000000, 0.5059523809523809312, 0.5119047619047618625, 0.5178571428571429047, 0.5238095238095238360, 0.5297619047619047672, 0.5357142857142856984, 0.5416666666666666297, 0.5476190476190476719, 0.5535714285714286031, 0.5595238095238095344, 0.5654761904761904656, 0.5714285714285713969, 0.5773809523809523281, 0.5833333333333333703, 0.5892857142857143016, 0.5952380952380952328, 0.6011904761904761640, 0.6071428571428570953, 0.6130952380952381375, 0.6190476190476190688, 0.6250000000000000000, 0.6309523809523809312, 0.6369047619047618625, 0.6428571428571429047, 0.6488095238095238360, 0.6547619047619047672, 0.6607142857142856984, 0.6666666666666666297, 0.6726190476190476719, 0.6785714285714286031, 0.6845238095238095344, 0.6904761904761904656, 0.6964285714285713969, 0.7023809523809523281, 0.7083333333333333703, 0.7142857142857143016, 0.7202380952380952328, 0.7261904761904761640, 0.7321428571428570953, 0.7380952380952381375, 0.7440476190476190688, 0.7500000000000000000, 0.7559523809523809312, 0.7619047619047618625, 0.7678571428571429047, 0.7738095238095238360, 0.7797619047619047672, 0.7857142857142856984, 0.7916666666666666297, 0.7976190476190476719, 0.8035714285714286031, 0.8095238095238095344, 0.8154761904761904656, 0.8214285714285713969, 0.8273809523809523281, 0.8333333333333333703, 0.8392857142857143016, 0.8452380952380952328, 0.8511904761904761640, 0.8571428571428570953, 0.8630952380952381375, 0.8690476190476190688, 0.8750000000000000000, 0.8809523809523809312, 0.8869047619047618625, 0.8928571428571429047, 0.8988095238095238360, 0.9047619047619047672, 0.9107142857142856984, 0.9166666666666666297, 0.9226190476190476719, 0.9285714285714286031, 0.9345238095238095344, 0.9404761904761904656, 0.9464285714285713969, 0.9523809523809523281, 0.9583333333333333703, 0.9642857142857143016 ),
 .UNSPECIFIED. ) 
 GEOMETRIC_REPRESENTATION_ITEM ( )  RATIONAL_B_SPLINE_SURFACE ( (
 ( 1.000000000000000000, 0.9659258262890683122, 1.000000000000000000, 0.9659258262890683122, 1.000000000000000000, 0.9659258262890683122, 1.000000000000000000, 0.9659258262890683122, 1.000000000000000000, 0.9659258262890683122, 1.000000000000000000, 0.9659258262890683122, 1.000000000000000000, 0.9659258262890683122, 1.000000000000000000, 0.9659258262890683122, 1.000000000000000000, 0.9659258262890683122, 1.000000000000000000, 0.9659258262890683122, 1.000000000000000000, 0.9659258262890683122, 1.000000000000000000, 0.9659258262890683122, 1.000000000000000000, 0.9659258262890683122, 1.000000000000000000, 0.9659258262890683122, 1.000000000000000000, 0.9659258262890683122, 1.000000000000000000, 0.9659258262890683122, 1.000000000000000000, 0.9659258262890683122, 1.000000000000000000, 0.9659258262890683122, 1.000000000000000000, 0.9659258262890683122, 1.000000000000000000, 0.9659258262890683122, 1.000000000000000000, 0.9659258262890683122, 1.000000000000000000, 0.9659258262890683122, 1.000000000000000000, 0.9659258262890683122, 1.000000000000000000, 0.9659258262890683122, 1.000000000000000000, 0.9659258262890683122, 1.000000000000000000, 0.9659258262890683122, 1.000000000000000000, 0.9659258262890683122, 1.000000000000000000, 0.9659258262890683122, 1.000000000000000000, 0.9659258262890683122, 1.000000000000000000, 0.9659258262890683122, 1.000000000000000000, 0.9659258262890683122, 1.000000000000000000, 0.9659258262890683122, 1.000000000000000000, 0.9659258262890683122, 1.000000000000000000, 0.9659258262890683122, 1.000000000000000000, 0.9659258262890683122, 1.000000000000000000, 0.9659258262890683122, 1.000000000000000000, 0.9659258262890683122, 1.000000000000000000, 0.9659258262890683122, 1.000000000000000000, 0.9659258262890683122, 1.000000000000000000, 0.9659258262890683122, 1.000000000000000000, 0.9659258262890683122, 1.000000000000000000, 0.9659258262890683122, 1.000000000000000000, 0.9659258262890683122, 1.000000000000000000, 0.9659258262890683122, 1.000000000000000000, 0.9659258262890683122, 1.000000000000000000, 0.9659258262890683122, 1.000000000000000000, 0.9659258262890683122, 1.000000000000000000, 0.9659258262890683122, 1.000000000000000000, 0.9659258262890683122, 1.000000000000000000, 0.9659258262890683122, 1.000000000000000000, 0.9659258262890683122, 1.000000000000000000, 0.9659258262890683122, 1.000000000000000000, 0.9659258262890683122, 1.000000000000000000, 0.9659258262890683122, 1.000000000000000000, 0.9659258262890683122, 1.000000000000000000, 0.9659258262890683122, 1.000000000000000000, 0.9659258262890683122, 1.000000000000000000, 0.9659258262890683122, 1.000000000000000000, 0.9659258262890683122, 1.000000000000000000, 0.9659258262890683122, 1.000000000000000000, 0.9659258262890683122, 1.000000000000000000, 0.9659258262890683122, 1.000000000000000000, 0.9659258262890683122, 1.000000000000000000, 0.9659258262890683122, 1.000000000000000000, 0.9659258262890683122, 1.000000000000000000, 0.9659258262890683122, 1.000000000000000000, 0.9659258262890683122, 1.000000000000000000, 0.9659258262890683122, 1.000000000000000000, 0.9659258262890683122, 1.000000000000000000, 0.9659258262890683122, 1.000000000000000000, 0.9659258262890683122, 1.000000000000000000, 0.9659258262890683122, 1.000000000000000000, 0.9659258262890683122, 1.000000000000000000, 0.9659258262890683122, 1.000000000000000000, 0.9659258262890683122, 1.000000000000000000, 0.9659258262890683122, 1.000000000000000000, 0.9659258262890683122, 1.000000000000000000, 0.9659258262890683122, 1.000000000000000000, 0.9659258262890683122, 1.000000000000000000, 0.9659258262890683122, 1.000000000000000000, 0.9659258262890683122, 1.000000000000000000, 0.9659258262890683122, 1.000000000000000000, 0.9659258262890683122, 1.000000000000000000, 0.9659258262890683122, 1.000000000000000000, 0.9659258262890683122, 1.000000000000000000, 0.9659258262890683122, 1.000000000000000000, 0.9659258262890683122, 1.000000000000000000, 0.9659258262890683122, 1.000000000000000000, 0.9659258262890683122, 1.000000000000000000, 0.9659258262890683122, 1.000000000000000000, 0.9659258262890683122, 1.000000000000000000, 0.9659258262890683122, 1.000000000000000000, 0.9659258262890683122, 1.000000000000000000, 0.9659258262890683122, 1.000000000000000000, 0.9659258262890683122, 1.000000000000000000, 0.9659258262890683122, 1.000000000000000000, 0.9659258262890683122, 1.000000000000000000, 0.9659258262890683122, 1.000000000000000000, 0.9659258262890683122, 1.000000000000000000, 0.9659258262890683122, 1.000000000000000000, 0.9659258262890683122, 1.000000000000000000, 0.9659258262890683122, 1.000000000000000000, 0.9659258262890683122, 1.000000000000000000, 0.9659258262890683122, 1.000000000000000000, 0.9659258262890683122, 1.000000000000000000, 0.9659258262890683122, 1.000000000000000000, 0.9659258262890683122, 1.000000000000000000, 0.9659258262890683122, 1.000000000000000000, 0.9659258262890683122, 1.000000000000000000, 0.9659258262890683122, 1.000000000000000000, 0.9659258262890683122, 1.000000000000000000, 0.9659258262890683122, 1.000000000000000000, 0.9659258262890683122, 1.000000000000000000, 0.9659258262890683122, 1.000000000000000000, 0.9659258262890683122, 1.000000000000000000, 0.9659258262890683122, 1.000000000000000000, 0.9659258262890683122, 1.000000000000000000, 0.9659258262890683122, 1.000000000000000000, 0.9659258262890683122, 1.000000000000000000, 0.9659258262890683122, 1.000000000000000000, 0.9659258262890683122, 1.000000000000000000, 0.9659258262890683122, 1.000000000000000000, 0.9659258262890683122, 1.000000000000000000, 0.9659258262890683122, 1.000000000000000000, 0.9659258262890683122, 1.000000000000000000, 0.9659258262890683122, 1.000000000000000000, 0.9659258262890683122, 1.000000000000000000, 0.9659258262890683122, 1.000000000000000000, 0.9659258262890683122, 1.000000000000000000, 0.9659258262890683122, 1.000000000000000000, 0.9659258262890683122, 1.000000000000000000, 0.9659258262890683122, 1.000000000000000000, 0.9659258262890683122, 1.000000000000000000, 0.9659258262890683122, 1.000000000000000000, 0.9659258262890683122, 1.000000000000000000, 0.9659258262890683122, 1.000000000000000000, 0.9659258262890683122, 1.000000000000000000, 0.9659258262890683122, 1.000000000000000000, 0.9659258262890683122, 1.000000000000000000, 0.9659258262890683122, 1.000000000000000000, 0.9659258262890683122, 1.000000000000000000, 0.9659258262890683122, 1.000000000000000000, 0.9659258262890683122, 1.000000000000000000, 0.9659258262890683122, 1.000000000000000000, 0.9659258262890683122, 1.000000000000000000, 0.9659258262890683122, 1.000000000000000000, 0.9659258262890683122, 1.000000000000000000, 0.9659258262890683122, 1.000000000000000000, 0.9659258262890683122, 1.000000000000000000, 0.9659258262890683122, 1.000000000000000000, 0.9659258262890683122, 1.000000000000000000, 0.9659258262890683122, 1.000000000000000000, 0.9659258262890683122, 1.000000000000000000, 0.9659258262890683122, 1.000000000000000000, 0.9659258262890683122, 1.000000000000000000, 0.9659258262890683122, 1.000000000000000000, 0.9659258262890683122, 1.000000000000000000, 0.9659258262890683122, 1.000000000000000000, 0.9659258262890683122, 1.000000000000000000, 0.9659258262890683122, 1.000000000000000000, 0.9659258262890683122, 1.000000000000000000, 0.9659258262890683122, 1.000000000000000000),
 ( 1.000000000000000000, 0.9659258262890683122, 1.000000000000000000, 0.9659258262890683122, 1.000000000000000000, 0.9659258262890683122, 1.000000000000000000, 0.9659258262890683122, 1.000000000000000000, 0.9659258262890683122, 1.000000000000000000, 0.9659258262890683122, 1.000000000000000000, 0.9659258262890683122, 1.000000000000000000, 0.9659258262890683122, 1.000000000000000000, 0.9659258262890683122, 1.000000000000000000, 0.9659258262890683122, 1.000000000000000000, 0.9659258262890683122, 1.000000000000000000, 0.9659258262890683122, 1.000000000000000000, 0.9659258262890683122, 1.000000000000000000, 0.9659258262890683122, 1.000000000000000000, 0.9659258262890683122, 1.000000000000000000, 0.9659258262890683122, 1.000000000000000000, 0.9659258262890683122, 1.000000000000000000, 0.9659258262890683122, 1.000000000000000000, 0.9659258262890683122, 1.000000000000000000, 0.9659258262890683122, 1.000000000000000000, 0.9659258262890683122, 1.000000000000000000, 0.9659258262890683122, 1.000000000000000000, 0.9659258262890683122, 1.000000000000000000, 0.9659258262890683122, 1.000000000000000000, 0.9659258262890683122, 1.000000000000000000, 0.9659258262890683122, 1.000000000000000000, 0.9659258262890683122, 1.000000000000000000, 0.9659258262890683122, 1.000000000000000000, 0.9659258262890683122, 1.000000000000000000, 0.9659258262890683122, 1.000000000000000000, 0.9659258262890683122, 1.000000000000000000, 0.9659258262890683122, 1.000000000000000000, 0.9659258262890683122, 1.000000000000000000, 0.9659258262890683122, 1.000000000000000000, 0.9659258262890683122, 1.000000000000000000, 0.9659258262890683122, 1.000000000000000000, 0.9659258262890683122, 1.000000000000000000, 0.9659258262890683122, 1.000000000000000000, 0.9659258262890683122, 1.000000000000000000, 0.9659258262890683122, 1.000000000000000000, 0.9659258262890683122, 1.000000000000000000, 0.9659258262890683122, 1.000000000000000000, 0.9659258262890683122, 1.000000000000000000, 0.9659258262890683122, 1.000000000000000000, 0.9659258262890683122, 1.000000000000000000, 0.9659258262890683122, 1.000000000000000000, 0.9659258262890683122, 1.000000000000000000, 0.9659258262890683122, 1.000000000000000000, 0.9659258262890683122, 1.000000000000000000, 0.9659258262890683122, 1.000000000000000000, 0.9659258262890683122, 1.000000000000000000, 0.9659258262890683122, 1.000000000000000000, 0.9659258262890683122, 1.000000000000000000, 0.9659258262890683122, 1.000000000000000000, 0.9659258262890683122, 1.000000000000000000, 0.9659258262890683122, 1.000000000000000000, 0.9659258262890683122, 1.000000000000000000, 0.9659258262890683122, 1.000000000000000000, 0.9659258262890683122, 1.000000000000000000, 0.9659258262890683122, 1.000000000000000000, 0.9659258262890683122, 1.000000000000000000, 0.9659258262890683122, 1.000000000000000000, 0.9659258262890683122, 1.000000000000000000, 0.9659258262890683122, 1.000000000000000000, 0.9659258262890683122, 1.000000000000000000, 0.9659258262890683122, 1.000000000000000000, 0.9659258262890683122, 1.000000000000000000, 0.9659258262890683122, 1.000000000000000000, 0.9659258262890683122, 1.000000000000000000, 0.9659258262890683122, 1.000000000000000000, 0.9659258262890683122, 1.000000000000000000, 0.9659258262890683122, 1.000000000000000000, 0.9659258262890683122, 1.000000000000000000, 0.9659258262890683122, 1.000000000000000000, 0.9659258262890683122, 1.000000000000000000, 0.9659258262890683122, 1.000000000000000000, 0.9659258262890683122, 1.000000000000000000, 0.9659258262890683122, 1.000000000000000000, 0.9659258262890683122, 1.000000000000000000, 0.9659258262890683122, 1.000000000000000000, 0.9659258262890683122, 1.000000000000000000, 0.9659258262890683122, 1.000000000000000000, 0.9659258262890683122, 1.000000000000000000, 0.9659258262890683122, 1.000000000000000000, 0.9659258262890683122, 1.000000000000000000, 0.9659258262890683122, 1.000000000000000000, 0.9659258262890683122, 1.000000000000000000, 0.9659258262890683122, 1.000000000000000000, 0.9659258262890683122, 1.000000000000000000, 0.9659258262890683122, 1.000000000000000000, 0.9659258262890683122, 1.000000000000000000, 0.9659258262890683122, 1.000000000000000000, 0.9659258262890683122, 1.000000000000000000, 0.9659258262890683122, 1.000000000000000000, 0.9659258262890683122, 1.000000000000000000, 0.9659258262890683122, 1.000000000000000000, 0.9659258262890683122, 1.000000000000000000, 0.9659258262890683122, 1.000000000000000000, 0.9659258262890683122, 1.000000000000000000, 0.9659258262890683122, 1.000000000000000000, 0.9659258262890683122, 1.000000000000000000, 0.9659258262890683122, 1.000000000000000000, 0.9659258262890683122, 1.000000000000000000, 0.9659258262890683122, 1.000000000000000000, 0.9659258262890683122, 1.000000000000000000, 0.9659258262890683122, 1.000000000000000000, 0.9659258262890683122, 1.000000000000000000, 0.9659258262890683122, 1.000000000000000000, 0.9659258262890683122, 1.000000000000000000, 0.9659258262890683122, 1.000000000000000000, 0.9659258262890683122, 1.000000000000000000, 0.9659258262890683122, 1.000000000000000000, 0.9659258262890683122, 1.000000000000000000, 0.9659258262890683122, 1.000000000000000000, 0.9659258262890683122, 1.000000000000000000, 0.9659258262890683122, 1.000000000000000000, 0.9659258262890683122, 1.000000000000000000, 0.9659258262890683122, 1.000000000000000000, 0.9659258262890683122, 1.000000000000000000, 0.9659258262890683122, 1.000000000000000000, 0.9659258262890683122, 1.000000000000000000, 0.9659258262890683122, 1.000000000000000000, 0.9659258262890683122, 1.000000000000000000, 0.9659258262890683122, 1.000000000000000000, 0.9659258262890683122, 1.000000000000000000, 0.9659258262890683122, 1.000000000000000000, 0.9659258262890683122, 1.000000000000000000, 0.9659258262890683122, 1.000000000000000000, 0.9659258262890683122, 1.000000000000000000, 0.9659258262890683122, 1.000000000000000000, 0.9659258262890683122, 1.000000000000000000, 0.9659258262890683122, 1.000000000000000000, 0.9659258262890683122, 1.000000000000000000, 0.9659258262890683122, 1.000000000000000000, 0.9659258262890683122, 1.000000000000000000, 0.9659258262890683122, 1.000000000000000000, 0.9659258262890683122, 1.000000000000000000, 0.9659258262890683122, 1.000000000000000000, 0.9659258262890683122, 1.000000000000000000, 0.9659258262890683122, 1.000000000000000000, 0.9659258262890683122, 1.000000000000000000, 0.9659258262890683122, 1.000000000000000000, 0.9659258262890683122, 1.000000000000000000, 0.9659258262890683122, 1.000000000000000000, 0.9659258262890683122, 1.000000000000000000, 0.9659258262890683122, 1.000000000000000000, 0.9659258262890683122, 1.000000000000000000, 0.9659258262890683122, 1.000000000000000000, 0.9659258262890683122, 1.000000000000000000, 0.9659258262890683122, 1.000000000000000000, 0.9659258262890683122, 1.000000000000000000, 0.9659258262890683122, 1.000000000000000000, 0.9659258262890683122, 1.000000000000000000, 0.9659258262890683122, 1.000000000000000000, 0.9659258262890683122, 1.000000000000000000, 0.9659258262890683122, 1.000000000000000000, 0.9659258262890683122, 1.000000000000000000, 0.9659258262890683122, 1.000000000000000000, 0.9659258262890683122, 1.000000000000000000, 0.9659258262890683122, 1.000000000000000000, 0.9659258262890683122, 1.000000000000000000, 0.9659258262890683122, 1.000000000000000000) ) ) 
 REPRESENTATION_ITEM ( '' )  SURFACE ( )  );
#4901 = DIRECTION ( 'NONE',  ( 0.000000000000000000, 1.000000000000000000, 0.000000000000000000 ) ) ;
#4902 = CARTESIAN_POINT ( 'NONE',  ( -0.1503990784575328643, 60.12777174578613426, 6.262539305110068177 ) ) ;
#4903 = EDGE_LOOP ( 'NONE', ( #95175, #80610, #75450, #11905, #78013 ) ) ;
#4904 = ADVANCED_FACE ( 'NONE', ( #29341 ), #14366, .T. ) ;
#4905 = CARTESIAN_POINT ( 'NONE',  ( -0.3689425029237898834, 41.17874883491397497, -10.36894250292378850 ) ) ;
#4906 =( LENGTH_UNIT ( ) NAMED_UNIT ( * ) SI_UNIT ( .MILLI., .METRE. ) );
#4907 = FACE_OUTER_BOUND ( 'NONE', #90936, .T. ) ;
#4908 = CARTESIAN_POINT ( 'NONE',  ( 17.96484262340118221, 19.93868534415484106, 7.964842623401181321 ) ) ;
#4909 = CARTESIAN_POINT ( 'NONE',  ( -2.816281873526471635, 33.91530133659708213, -3.434112377981056508 ) ) ;
#4910 = CARTESIAN_POINT ( 'NONE',  ( -7.264948169187289473, 14.76930270348881002, -13.05597881399728699 ) ) ;
#4911 = VECTOR ( 'NONE', #55457, 1000.000000000000000 ) ;
#4912 = CARTESIAN_POINT ( 'NONE',  ( -2.816281873526473856, 59.12363466993042493, 9.499525473075851096E-16 ) ) ;
#4913 = ORIENTED_EDGE ( 'NONE', *, *, #67842, .F. ) ;
#4914 = LINE ( 'NONE', #42416, #2202 ) ;
#4915 = ADVANCED_FACE ( 'NONE', ( #17323 ), #7942, .T. ) ;
#4916 = CIRCLE ( 'NONE', #65556, 0.2500000000000002220 ) ;
#4917 = CARTESIAN_POINT ( 'NONE',  ( 17.08211943468705840, 25.13708216824730357, -12.26659068614894466 ) ) ;
#4918 = CARTESIAN_POINT ( 'NONE',  ( 2.917880565312950480, 5.970415501580634832, -12.26659068614894821 ) ) ;
#4919 = CARTESIAN_POINT ( 'NONE',  ( 20.03743638938529159, 61.75197528031018379, 6.399506433553906248 ) ) ;
#4920 = CARTESIAN_POINT ( 'NONE',  ( 12.91533473730993009, 21.60535201082150536, -10.88017736071109987 ) ) ;
#4921 = DIRECTION ( 'NONE',  ( 0.008726535498360278933, 0.000000000000000000, 0.9999619230641714207 ) ) ;
#4922 = CARTESIAN_POINT ( 'NONE',  ( 20.88017736071110875, 40.77201867748818387, -2.915334737309920765 ) ) ;
#4923 = CARTESIAN_POINT ( 'NONE',  ( 0.5774900079438590739, 57.64701867748817676, -5.440088680355550821 ) ) ;
#4924 = CARTESIAN_POINT ( 'NONE',  ( 19.38216949554541557, 12.24863466993041961, -9.382169495545420901 ) ) ;
#4925 = CARTESIAN_POINT ( 'NONE',  ( -4.000000000000000000, 10.00000000000000000, 2.500000000000000000 ) ) ;
#4926 = CYLINDRICAL_SURFACE ( 'NONE', #54689, 0.5000000000000004441 ) ;
#4927 = CARTESIAN_POINT ( 'NONE',  ( 17.20831665107776587, 29.13393115100078390, -7.208316651077762316 ) ) ;
#4928 = CIRCLE ( 'NONE', #68806, 7.000000000000002665 ) ;
#4929 = CARTESIAN_POINT ( 'NONE',  ( 10.00000000000000178, 39.31368534415484106, 10.88017736071110342 ) ) ;
#4930 = CARTESIAN_POINT ( 'NONE',  ( 22.81628187352647785, 6.415301336597088344, 3.434112377981063169 ) ) ;
#4931 = CARTESIAN_POINT ( 'NONE',  ( 12.91533473730993009, 56.60535201082151247, -10.88017736071109987 ) ) ;
#4932 = CARTESIAN_POINT ( 'NONE',  ( 17.20831665107776587, 22.88393115100078745, 7.208316651077764980 ) ) ;
#4933 = CARTESIAN_POINT ( 'NONE',  ( -1.099225684535947600, 53.70696800326376064, -6.408140936763238038 ) ) ;
#4934 = CARTESIAN_POINT ( 'NONE',  ( 0.1532563361054083140, 11.00893115100078568, 1.131784320476157264E-15 ) ) ;
#4935 = ORIENTED_EDGE ( 'NONE', *, *, #41909, .F. ) ;
#4936 = CARTESIAN_POINT ( 'NONE',  ( -7.750000000000000000, 40.99999999999999289, -4.000000000000000000 ) ) ;
#4937 = DIRECTION ( 'NONE',  ( 0.000000000000000000, -1.000000000000000000, 0.000000000000000000 ) ) ;
#4938 = CARTESIAN_POINT ( 'NONE',  ( 20.88017736071110164, 15.35535201082150358, 2.915334737309930979 ) ) ;
#4940 = CARTESIAN_POINT ( 'NONE',  ( 6.204703633549690345, 22.84541550158062861, 14.16423886937410082 ) ) ;
#4939 = CARTESIAN_POINT ( 'NONE',  ( 22.81628187352647785, 56.41530133659708213, 3.434112377981063169 ) ) ;
#4941 = CARTESIAN_POINT ( 'NONE',  ( 2.791683348922240793, 31.63393115100078745, 7.208316651077764092 ) ) ;
#4942 = CARTESIAN_POINT ( 'NONE',  ( 10.00000000000000178, 19.31368534415484106, 10.88017736071110342 ) ) ;
#4943 = CARTESIAN_POINT ( 'NONE',  ( -2.266590686148945544, 67.22041550158063217, 7.082119434687048631 ) ) ;
#4944 = ORIENTED_EDGE ( 'NONE', *, *, #42116, .T. ) ;
#4945 = CARTESIAN_POINT ( 'NONE',  ( 4.559911319644449179, 17.23035201082150536, -9.422509992056141925 ) ) ;
#4946 = CARTESIAN_POINT ( 'NONE',  ( 4.559911319644449179, 32.23035201082150536, -9.422509992056141925 ) ) ;
#4948 = CARTESIAN_POINT ( 'NONE',  ( 4.559911319644449179, 43.89701867748816966, 9.422509992056141925 ) ) ;
#4947 = CARTESIAN_POINT ( 'NONE',  ( -12.54342190210052621, 14.76984988503095764, 8.116945096741206456 ) ) ;
#4949 = ORIENTED_EDGE ( 'NONE', *, *, #43822, .T. ) ;
#4950 = CARTESIAN_POINT ( 'NONE',  ( 0.1532563361054082862, 66.21726448433413736, 2.638427012816831674 ) ) ;
#4951 = CARTESIAN_POINT ( 'NONE',  ( 4.559911319644449179, 18.89701867748817321, 9.422509992056141925 ) ) ;
#4952 = DIRECTION ( 'NONE',  ( -0.4305110968082986878, 0.000000000000000000, 0.9025852843498588518 ) ) ;
#4953 = COLOUR_RGB ( '', 0.08235294, 0.09019608, 0.10196078) ;
#4954 = CYLINDRICAL_SURFACE ( 'NONE', #20204, 2.000000000000000888 ) ;
#4955 = CARTESIAN_POINT ( 'NONE',  ( -2.816281873526473856, 64.12363466993042493, 9.499525473075851096E-16 ) ) ;
#4956 = CARTESIAN_POINT ( 'NONE',  ( 20.15039907845753220, 30.60158574516642815, -6.262539305110077947 ) ) ;
#4957 = CARTESIAN_POINT ( 'NONE',  ( -2.266590686148945544, 27.22041550158063572, 7.082119434687048631 ) ) ;
#4958 = CARTESIAN_POINT ( 'NONE',  ( -0.8801773607111008646, 53.27201867748816966, 2.915334737309923430 ) ) ;
#4959 = CARTESIAN_POINT ( 'NONE',  ( 19.42250999205614193, 35.14701867748816966, 5.440088680355555262 ) ) ;
#4960 = CARTESIAN_POINT ( 'NONE',  ( 3.715841784917714108, -0.03417435944610275333, 15.55859621770270529 ) ) ;
#4961 = CARTESIAN_POINT ( 'NONE',  ( -4.838527690343430443, 0.5000000000000004441, -14.19819177887733375 ) ) ;
#4962 = CARTESIAN_POINT ( 'NONE',  ( 17.20831665107776587, 52.88393115100078035, 7.208316651077764980 ) ) ;
#4963 = ORIENTED_EDGE ( 'NONE', *, *, #8053, .F. ) ;
#4964 = CARTESIAN_POINT ( 'NONE',  ( 0.1077916266722469679, 22.24062864464239553, -6.478736007405950126 ) ) ;
#4965 = CARTESIAN_POINT ( 'NONE',  ( 7.361572987183170547, 22.05059781766745530, 9.846743663894590881 ) ) ;
#4966 = CARTESIAN_POINT ( 'NONE',  ( 12.81628187352647252, -28.16803199673624292, -3.434112377981059172 ) ) ;
#4967 = CARTESIAN_POINT ( 'NONE',  ( 4.559911319644449179, 17.23035201082150536, -9.422509992056141925 ) ) ;
#4968 = CARTESIAN_POINT ( 'NONE',  ( 2.791683348922237240, 30.38393115100078390, -7.208316651077763204 ) ) ;
#4970 = CARTESIAN_POINT ( 'NONE',  ( 3.591859063236761518, 14.95696800326375531, 11.09922568453594849 ) ) ;
#4969 = VECTOR ( 'NONE', #81230, 1000.000000000000000 ) ;
#4971 = CARTESIAN_POINT ( 'NONE',  ( 2.035157376598824452, 58.68868534415482685, 7.964842623401179544 ) ) ;
#4973 = CARTESIAN_POINT ( 'NONE',  ( 6.565887622018943937, 55.16530133659709634, 12.81628187352647430 ) ) ;
#4972 = CARTESIAN_POINT ( 'NONE',  ( 12.91533473730993009, 16.60535201082150891, -10.88017736071109987 ) ) ;
#4974 = CARTESIAN_POINT ( 'NONE',  ( 24.16423886937410614, 49.30374883491396787, 8.672049930838204340E-16 ) ) ;
#4975 = EDGE_CURVE ( 'NONE', #65472, #96338, #92100, .T. ) ;
#4976 = CIRCLE ( 'NONE', #8186, 14.49999999999999822 ) ;
#4977 = CARTESIAN_POINT ( 'NONE',  ( -42.83369174045569849, 106.9566484930309684, 5.017862233661315230 ) ) ;
#4978 = VERTEX_POINT ( 'NONE', #79774 ) ;
#4979 = CARTESIAN_POINT ( 'NONE',  ( -2.816281873526473856, -0.8763653300695799508, 9.499525473075851096E-16 ) ) ;
#4980 = CARTESIAN_POINT ( 'NONE',  ( 19.05866839779139355, 20.95508385108958649, -6.499999999999974243 ) ) ;
#4981 = CARTESIAN_POINT ( 'NONE',  ( 10.00000000000000178, 29.31368534415483751, 10.88017736071110342 ) ) ;
#4982 = CARTESIAN_POINT ( 'NONE',  ( 19.84674366389459266, 63.30059781766745886, 2.638427012816836559 ) ) ;
#4983 = ORIENTED_EDGE ( 'NONE', *, *, #80581, .F. ) ;
#4984 = CARTESIAN_POINT ( 'NONE',  ( 19.84674366389459621, 13.50893115100078568, 7.409399052514197653E-17 ) ) ;
#4985 = CARTESIAN_POINT ( 'NONE',  ( 10.00000000000000000, 14.75893115100078568, -9.846743663894594434 ) ) ;
#4986 = CARTESIAN_POINT ( 'NONE',  ( 19.84674366389459266, 28.30059781766745886, 2.638427012816836559 ) ) ;
#4987 = CARTESIAN_POINT ( 'NONE',  ( 5.076628168052704559, 5.175597817667451750, -8.527530157486179263 ) ) ;
#4988 = CARTESIAN_POINT ( 'NONE',  ( 19.84674366389459266, 3.717264484334118713, -2.638427012816827677 ) ) ;
#4989 = CARTESIAN_POINT ( 'NONE',  ( -7.124975165218884854, -78.82169502743931844, 2.500000000000000000 ) ) ;
#4991 = CARTESIAN_POINT ( 'NONE',  ( -14.17193700899788134, 15.00000000000000000, -1.489530601564206247 ) ) ;
#4990 = CARTESIAN_POINT ( 'NONE',  ( 17.20831665107776587, 4.133931151000785675, -7.208316651077762316 ) ) ;
#4992 = CARTESIAN_POINT ( 'NONE',  ( 18.52753015748617571, 8.092264484334117824, 4.923371831947298993 ) ) ;
#4994 = VERTEX_POINT ( 'NONE', #11273 ) ;
#4993 = CARTESIAN_POINT ( 'NONE',  ( 19.84674366389459266, 23.71726448433412315, -2.638427012816827677 ) ) ;
#4995 = LINE ( 'NONE', #52455, #67780 ) ;
#4996 = EDGE_CURVE ( 'NONE', #91846, #36347, #58603, .T. ) ;
#4997 = CARTESIAN_POINT ( 'NONE',  ( 10.00000000000000178, 62.25893115100078745, 9.846743663894594434 ) ) ;
#4998 = ORIENTED_EDGE ( 'NONE', *, *, #73140, .F. ) ;
#4999 = CARTESIAN_POINT ( 'NONE',  ( 17.96484262340118221, 6.188685344154836621, -7.964842623401177768 ) ) ;
#5000 = CARTESIAN_POINT ( 'NONE',  ( 2.917880565312948704, 22.63708216824730002, 12.26659068614894643 ) ) ;
#5001 = EDGE_CURVE ( 'NONE', #41516, #16129, #40805, .T. ) ;
#5002 = FACE_OUTER_BOUND ( 'NONE', #78804, .T. ) ;
#5003 = CARTESIAN_POINT ( 'NONE',  ( 13.79529636645031943, 15.34541550158063750, -14.16423886937409904 ) ) ;
#5004 = CARTESIAN_POINT ( 'NONE',  ( 2.917880565312950480, 45.97041550158063927, -12.26659068614894821 ) ) ;
#5005 = FILL_AREA_STYLE_COLOUR ( '', #71005 ) ;
#5006 = CARTESIAN_POINT ( 'NONE',  ( 22.26659068614894466, 18.88708216824730002, 7.082119434687054849 ) ) ;
#5007 = CARTESIAN_POINT ( 'NONE',  ( -0.8801773607111009756, 33.06368534415484106, 1.068504757029289695E-15 ) ) ;
#5008 = LINE ( 'NONE', #65490, #38808 ) ;
#5009 = CARTESIAN_POINT ( 'NONE',  ( 10.00000000000000178, 22.25893115100078745, 9.846743663894594434 ) ) ;
#5011 = CARTESIAN_POINT ( 'NONE',  ( 18.52753015748617571, 23.09226448433411960, 4.923371831947298993 ) ) ;
#5010 = CARTESIAN_POINT ( 'NONE',  ( 0.5774900079438590739, 52.64701867748817676, -5.440088680355550821 ) ) ;
#5012 = CIRCLE ( 'NONE', #60887, 0.2500000000000002220 ) ;
#5013 = CARTESIAN_POINT ( 'NONE',  ( -0.8801773607110991993, 12.85535201082150358, -2.915334737309923874 ) ) ;
#5014 = CARTESIAN_POINT ( 'NONE',  ( 3.591859063236763294, 48.29030133659708923, -11.09922568453595026 ) ) ;
#5015 = CARTESIAN_POINT ( 'NONE',  ( 14.92337183194729633, 47.67559781766745175, 8.527530157486181039 ) ) ;
#5016 = DIRECTION ( 'NONE',  ( 0.000000000000000000, 1.000000000000000000, 0.000000000000000000 ) ) ;
#5017 = CARTESIAN_POINT ( 'NONE',  ( -2.816281873526471635, 48.91530133659708213, -3.434112377981056508 ) ) ;
#5018 = CARTESIAN_POINT ( 'NONE',  ( -3.795296366450322534, -34.23791783175269643, -14.16423886937409904 ) ) ;
#5019 = CARTESIAN_POINT ( 'NONE',  ( 10.00000000000000000, 34.75893115100078745, -9.846743663894594434 ) ) ;
#5020 = CARTESIAN_POINT ( 'NONE',  ( 24.16423886937410614, 24.30374883491396787, 8.672049930838204340E-16 ) ) ;
#5021 = VERTEX_POINT ( 'NONE', #33277 ) ;
#5022 = DIRECTION ( 'NONE',  ( -0.000000000000000000, -0.000000000000000000, -1.000000000000000000 ) ) ;
#5023 = CARTESIAN_POINT ( 'NONE',  ( 20.88017736071110875, 55.77201867748816966, -2.915334737309920765 ) ) ;
#5024 = CARTESIAN_POINT ( 'NONE',  ( 0.5774900079438590739, 62.64701867748817676, -5.440088680355550821 ) ) ;
#5025 = CARTESIAN_POINT ( 'NONE',  ( -4.164238869374099039, 41.80374883491397497, 8.674139862899312516E-16 ) ) ;
#5026 = CARTESIAN_POINT ( 'NONE',  ( 2.791683348922240793, 66.63393115100079456, 7.208316651077764092 ) ) ;
#5027 = CARTESIAN_POINT ( 'NONE',  ( -0.04068437667222699061, 57.21974360917722180, -6.396802510829763477 ) ) ;
#5028 = CARTESIAN_POINT ( 'NONE',  ( 20.88017736071110519, 35.56368534415484106, 2.639326808657452039E-16 ) ) ;
#5029 = CARTESIAN_POINT ( 'NONE',  ( 1.379999999999981908, 20.99999999999999645, -1.249999999999987121 ) ) ;
#5030 = CARTESIAN_POINT ( 'NONE',  ( 13.43411237798106583, 27.66530133659708568, -12.81628187352647252 ) ) ;
#5031 = CARTESIAN_POINT ( 'NONE',  ( 2.791683348922237240, 55.38393115100078745, -7.208316651077763204 ) ) ;
#5032 = CARTESIAN_POINT ( 'NONE',  ( 5.440088680355556150, 14.73035201082151247, 9.422509992056138373 ) ) ;
#5033 = DIRECTION ( 'NONE',  ( -0.7132504491541751257, 0.000000000000000000, -0.7009092642998574485 ) ) ;
#5034 = CARTESIAN_POINT ( 'NONE',  ( 4.559911319644449179, 13.89701867748817321, 9.422509992056141925 ) ) ;
#5035 = LINE ( 'NONE', #58512, #5690 ) ;
#5036 = AXIS2_PLACEMENT_3D ( 'NONE', #65620, #57633, #65125 ) ;
#5037 = ORIENTED_EDGE ( 'NONE', *, *, #82084, .F. ) ;
#5038 = ADVANCED_FACE ( 'NONE', ( #93299 ), #73441, .F. ) ;
#5039 = CARTESIAN_POINT ( 'NONE',  ( 10.00000000000000000, 6.813685344154838397, -10.88017736071110342 ) ) ;
#5040 = PLANE ( 'NONE',  #44846 ) ;
#5041 = CARTESIAN_POINT ( 'NONE',  ( 12.91533473730993009, 66.60535201082150536, -10.88017736071109987 ) ) ;
#5042 = VECTOR ( 'NONE', #62567, 1000.000000000000000 ) ;
#5043 = CARTESIAN_POINT ( 'NONE',  ( 20.88017736071110519, 65.56368534415483396, 2.639326808657452039E-16 ) ) ;
#5044 = FACE_OUTER_BOUND ( 'NONE', #18124, .T. ) ;
#5045 = CARTESIAN_POINT ( 'NONE',  ( 5.076628168052703671, 31.84226448433412315, 8.527530157486179263 ) ) ;
#5046 = CARTESIAN_POINT ( 'NONE',  ( 20.88017736071110519, 25.56368534415483751, 2.639326808657452039E-16 ) ) ;
#5047 = CARTESIAN_POINT ( 'NONE',  ( 13.43411237798106583, 12.66530133659708746, -12.81628187352647252 ) ) ;
#5049 = CARTESIAN_POINT ( 'NONE',  ( 13.75801628063878645, 15.00000000000000000, 4.578972376164554881 ) ) ;
#5048 = CARTESIAN_POINT ( 'NONE',  ( 12.91533473730992121, 29.52201867748817321, 10.88017736071110164 ) ) ;
#5050 = CARTESIAN_POINT ( 'NONE',  ( 9.159723438033129383, -0.03417435944610275333, 10.91613331444548507 ) ) ;
#5051 = CARTESIAN_POINT ( 'NONE',  ( -2.816281873526471635, 33.91530133659708213, -3.434112377981056508 ) ) ;
#5052 = ORIENTED_EDGE ( 'NONE', *, *, #47299, .T. ) ;
#5053 = CARTESIAN_POINT ( 'NONE',  ( 2.035157376598824452, 63.68868534415484106, 7.964842623401179544 ) ) ;
#5054 = CARTESIAN_POINT ( 'NONE',  ( -1.099225684535947600, 24.54030133659708923, 6.408140936763237150 ) ) ;
#5055 = FILL_AREA_STYLE ('',( #42553 ) ) ;
#5056 = CARTESIAN_POINT ( 'NONE',  ( 7.084665262690076126, 44.10535201082151247, 10.88017736071109987 ) ) ;
#5057 = CARTESIAN_POINT ( 'NONE',  ( 0.1957200283969144639, 15.25733960839543890, 6.500000000000003553 ) ) ;
#5058 = CARTESIAN_POINT ( 'NONE',  ( -4.164238869374098151, 66.59541550158060375, -3.795296366450310543 ) ) ;
#5059 = CARTESIAN_POINT ( 'NONE',  ( 17.20831665107776587, 54.13393115100079456, -7.208316651077762316 ) ) ;
#5060 = CARTESIAN_POINT ( 'NONE',  ( 7.084665262690076126, 67.02201867748817676, -10.88017736071110164 ) ) ;
#5061 = CARTESIAN_POINT ( 'NONE',  ( 2.035157376598822676, 67.43868534415484817, -7.964842623401177768 ) ) ;
#5062 = FACE_OUTER_BOUND ( 'NONE', #6236, .T. ) ;
#5063 = CARTESIAN_POINT ( 'NONE',  ( 20.36894250292379738, 24.92874883491396787, -10.36894250292379027 ) ) ;
#5064 = PRESENTATION_LAYER_ASSIGNMENT (  '', '', ( #92895 ) ) ;
#5065 = CARTESIAN_POINT ( 'NONE',  ( 13.95749458852080949, 0.2306972965111896423, -5.331641351773021675 ) ) ;
#5066 = ORIENTED_EDGE ( 'NONE', *, *, #32622, .F. ) ;
#5067 = ORIENTED_EDGE ( 'NONE', *, *, #61966, .F. ) ;
#5068 = CARTESIAN_POINT ( 'NONE',  ( 22.26659068614894466, 63.88708216824730357, 7.082119434687054849 ) ) ;
#5069 = CARTESIAN_POINT ( 'NONE',  ( 10.00000000000000000, 55.55374883491396787, -14.16423886937410082 ) ) ;
#5070 = CARTESIAN_POINT ( 'NONE',  ( 7.361572987183169658, 24.96726448433412315, -9.846743663894592657 ) ) ;
#5071 = CARTESIAN_POINT ( 'NONE',  ( 10.00000000000000000, 22.87363466993042138, -12.81628187352647608 ) ) ;
#5072 = CARTESIAN_POINT ( 'NONE',  ( -13.76201028429828277, 90.94474152336147199, 7.905771670467119705 ) ) ;
#5073 = LINE ( 'NONE', #35052, #35515 ) ;
#5074 = CARTESIAN_POINT ( 'NONE',  ( 0.5774900079438607392, 3.480352010821504027, 5.440088680355550821 ) ) ;
#5075 = CARTESIAN_POINT ( 'NONE',  ( -4.164238869374099039, 61.80374883491397497, 8.674139862899312516E-16 ) ) ;
#5076 = CARTESIAN_POINT ( 'NONE',  ( 4.600000000000003197, 98.49999999999998579, 8.000000000000000000 ) ) ;
#5077 = CARTESIAN_POINT ( 'NONE',  ( 0.1532563361054083140, 6.008931151000784787, 1.131784320476157264E-15 ) ) ;
#5078 = CARTESIAN_POINT ( 'NONE',  ( -0.000000000000000000, 40.74999999999999289, -4.000000000000000000 ) ) ;
#5079 = CARTESIAN_POINT ( 'NONE',  ( 9.846743663894590881, 8.300597817667446421, 2.638427012816828565 ) ) ;
#5080 = ORIENTED_EDGE ( 'NONE', *, *, #38357, .T. ) ;
#5081 = ORIENTED_EDGE ( 'NONE', *, *, #31371, .T. ) ;
#5082 = FACE_OUTER_BOUND ( 'NONE', #20745, .T. ) ;
#5083 = VERTEX_POINT ( 'NONE', #55299 ) ;
#5084 = CARTESIAN_POINT ( 'NONE',  ( 22.26659068614894466, 13.88708216824730179, 7.082119434687054849 ) ) ;
#5086 = CARTESIAN_POINT ( 'NONE',  ( 0.5774900079438590739, 22.64701867748817321, -5.440088680355550821 ) ) ;
#5085 = CARTESIAN_POINT ( 'NONE',  ( -0.8801773607111009756, 23.06368534415484106, 1.068504757029289695E-15 ) ) ;
#5088 = CARTESIAN_POINT ( 'NONE',  ( -1.099225684535947600, 19.54030133659708568, 6.408140936763237150 ) ) ;
#5087 = CARTESIAN_POINT ( 'NONE',  ( 7.361572987183169658, 49.96726448433410894, -9.846743663894592657 ) ) ;
#5089 = ADVANCED_FACE ( 'NONE', ( #66742 ), #24009, .T. ) ;
#5090 = MECHANICAL_DESIGN_GEOMETRIC_PRESENTATION_REPRESENTATION (  '', ( #9945 ), #64154 ) ;
#5091 = CARTESIAN_POINT ( 'NONE',  ( -2.816281873526473856, 34.12363466993042493, 9.499525473075851096E-16 ) ) ;
#5092 = ORIENTED_EDGE ( 'NONE', *, *, #42012, .F. ) ;
#5093 = CARTESIAN_POINT ( 'NONE',  ( 19.84674366389459266, 33.30059781766744464, 2.638427012816836559 ) ) ;
#5094 = CARTESIAN_POINT ( 'NONE',  ( 20.36894250292379382, 58.67874883491396076, 10.36894250292379205 ) ) ;
#5095 = VERTEX_POINT ( 'NONE', #43737 ) ;
#5096 = CARTESIAN_POINT ( 'NONE',  ( 7.084665262690076126, 7.022018677488170546, -10.88017736071110164 ) ) ;
#5097 = ORIENTED_EDGE ( 'NONE', *, *, #26477, .F. ) ;
#5098 = CARTESIAN_POINT ( 'NONE',  ( -0.8801773607110991993, 42.85535201082150536, -2.915334737309923874 ) ) ;
#5099 = CARTESIAN_POINT ( 'NONE',  ( 19.42250999205614193, 45.14701867748817676, 5.440088680355555262 ) ) ;
#5100 = CARTESIAN_POINT ( 'NONE',  ( 0.5774900079438590739, 52.64701867748817676, -5.440088680355550821 ) ) ;
#5101 = CARTESIAN_POINT ( 'NONE',  ( 20.88017736071110164, 40.35535201082150536, 2.915334737309930979 ) ) ;
#5102 = CARTESIAN_POINT ( 'NONE',  ( 20.15039907845753220, 64.72266099184918176, 6.262539305110077947 ) ) ;
#5105 = VERTEX_POINT ( 'NONE', #73740 ) ;
#5104 = AXIS2_PLACEMENT_3D ( 'NONE', #58198, #88713, #20223 ) ;
#5103 = SURFACE_STYLE_USAGE ( .BOTH. , #72109 ) ;
#5106 = PRESENTATION_LAYER_ASSIGNMENT (  '', '', ( #25810 ) ) ;
#5107 = EDGE_CURVE ( 'NONE', #27101, #17129, #42763, .T. ) ;
#5108 = CARTESIAN_POINT ( 'NONE',  ( 1.472469842513823179, 25.59226448433412315, -4.923371831947296329 ) ) ;
#5109 = ORIENTED_EDGE ( 'NONE', *, *, #16488, .T. ) ;
#5110 = CARTESIAN_POINT ( 'NONE',  ( 7.361572987183170547, 62.05059781766745886, 9.846743663894590881 ) ) ;
#5111 = FACE_OUTER_BOUND ( 'NONE', #56104, .T. ) ;
#5112 = AXIS2_PLACEMENT_3D ( 'NONE', #92284, #31765, #46290 ) ;
#5113 = EDGE_CURVE ( 'NONE', #46963, #88123, #79864, .T. ) ;
#5114 = AXIS2_PLACEMENT_3D ( 'NONE', #27559, #73547, #21060 ) ;
#5115 = B_SPLINE_CURVE_WITH_KNOTS ( 'NONE', 3,
 ( #76016, #68032, #59037, #60019, #75520, #30010 ),
 .UNSPECIFIED., .F., .F.,
 ( 4, 2, 4 ),
 ( 0.0002800452451363350925, 0.0006862509172491815680, 0.001092456589362028043 ),
 .UNSPECIFIED. ) ;
#5116 = CARTESIAN_POINT ( 'NONE',  ( -6.560019409699617832, -50.64698701990471363, 3.750000000000000444 ) ) ;
#5117 = VERTEX_POINT ( 'NONE', #41793 ) ;
#5118 = DIRECTION ( 'NONE',  ( -0.000000000000000000, -0.000000000000000000, 1.000000000000000000 ) ) ;
#5119 = CARTESIAN_POINT ( 'NONE',  ( 18.72515096720571037, 45.05509018479935435, 6.499999999999982236 ) ) ;
#5120 = DIRECTION ( 'NONE',  ( -0.000000000000000000, -1.000000000000000000, 0.000000000000000000 ) ) ;
#5121 = CARTESIAN_POINT ( 'NONE',  ( 22.26659068614895176, 54.72041550158063217, -7.082119434687042414 ) ) ;
#5122 = CARTESIAN_POINT ( 'NONE',  ( 18.61655166652077398, 64.87718327197430312, 6.499999999999981348 ) ) ;
#5123 = ORIENTED_EDGE ( 'NONE', *, *, #30312, .T. ) ;
#5124 = DIRECTION ( 'NONE',  ( -1.000000000000000000, 5.818595309480552676E-17, 0.000000000000000000 ) ) ;
#5125 = CARTESIAN_POINT ( 'NONE',  ( 0.1532563361054100626, 35.80059781766745175, -2.638427012816831230 ) ) ;
#5126 = DIRECTION ( 'NONE',  ( 0.000000000000000000, 0.000000000000000000, -1.000000000000000000 ) ) ;
#5127 = CARTESIAN_POINT ( 'NONE',  ( 6.565887622018943937, 8.081968003263751754, -12.81628187352647608 ) ) ;
#5128 = CARTESIAN_POINT ( 'NONE',  ( 14.92337183194729988, 14.34226448433411782, -8.527530157486177487 ) ) ;
#5129 = LINE ( 'NONE', #35619, #63277 ) ;
#5130 = CARTESIAN_POINT ( 'NONE',  ( 5.076628168052704559, 5.175597817667451750, -8.527530157486179263 ) ) ;
#5131 = CARTESIAN_POINT ( 'NONE',  ( -2.816281873526471635, -1.084698663402913210, -3.434112377981056508 ) ) ;
#5132 = DIRECTION ( 'NONE',  ( -1.000000000000000000, 0.000000000000000000, 0.000000000000000000 ) ) ;
#5133 = ORIENTED_EDGE ( 'NONE', *, *, #57378, .T. ) ;
#5134 = CARTESIAN_POINT ( 'NONE',  ( 2.035157376598824452, 3.688685344154837953, 7.964842623401179544 ) ) ;
#5135 = CARTESIAN_POINT ( 'NONE',  ( 24.16423886937409904, 4.095415501580634832, 3.795296366450317205 ) ) ;
#5136 = CARTESIAN_POINT ( 'NONE',  ( 5.076628168052704559, 25.17559781766745175, -8.527530157486179263 ) ) ;
#5137 = CARTESIAN_POINT ( 'NONE',  ( 7.084665262690076126, 49.10535201082149825, 10.88017736071109987 ) ) ;
#5139 = CARTESIAN_POINT ( 'NONE',  ( -3.500000000000000444, 1.019547802438453887, -2.750000000000000444 ) ) ;
#5138 = CARTESIAN_POINT ( 'NONE',  ( 21.09922568453594849, 21.20696800326375353, 6.408140936763242479 ) ) ;
#5140 = CARTESIAN_POINT ( 'NONE',  ( 0.5774900079438590739, 2.647018677488170990, -5.440088680355550821 ) ) ;
#5141 = DIRECTION ( 'NONE',  ( 0.000000000000000000, 1.000000000000000000, 0.000000000000000000 ) ) ;
#5142 = CARTESIAN_POINT ( 'NONE',  ( 8.606322355891363074, 4.859979058039186735E-16, -11.66967075398807374 ) ) ;
#5143 = CARTESIAN_POINT ( 'NONE',  ( 3.591859063236763294, 3.290301336597087012, -11.09922568453595026 ) ) ;
#5144 = CARTESIAN_POINT ( 'NONE',  ( 16.40814093676323893, 0.7903013365970867898, 11.09922568453595026 ) ) ;
#5145 = CARTESIAN_POINT ( 'NONE',  ( 19.84674366389459266, 13.71726448433411782, -2.638427012816827677 ) ) ;
#5146 = CARTESIAN_POINT ( 'NONE',  ( -5.440088680355547268, -26.10298132251182324, 9.422509992056143702 ) ) ;
#5147 = CARTESIAN_POINT ( 'NONE',  ( 22.81628187352648496, 21.83196800326374643, -3.434112377981050290 ) ) ;
#5148 = CARTESIAN_POINT ( 'NONE',  ( -11.42353084996827484, -90.30959216425827663, -4.000000000001802114 ) ) ;
#5150 = CARTESIAN_POINT ( 'NONE',  ( 0.000000000000000000, 14.49999999999999822, 0.000000000000000000 ) ) ;
#5149 = CARTESIAN_POINT ( 'NONE',  ( 4.559911319644449179, 23.89701867748817321, 9.422509992056141925 ) ) ;
#5151 = LINE ( 'NONE', #57151, #10080 ) ;
#5152 = B_SPLINE_CURVE_WITH_KNOTS ( 'NONE', 3,
 ( #3505, #64467, #41998, #94001, #95978, #10993 ),
 .UNSPECIFIED., .F., .F.,
 ( 4, 2, 4 ),
 ( 3.409110551496115783E-05, 0.0004400426677367864632, 0.0008459942299586117008 ),
 .UNSPECIFIED. ) ;
#5153 = CARTESIAN_POINT ( 'NONE',  ( 20.36894250292379738, 49.92874883491396787, -10.36894250292379027 ) ) ;
#5154 = ADVANCED_FACE ( 'NONE', ( #89245 ), #73246, .F. ) ;
#5155 = DIRECTION ( 'NONE',  ( 0.000000000000000000, -1.000000000000000000, 0.000000000000000000 ) ) ;
#5156 = CARTESIAN_POINT ( 'NONE',  ( 19.42250999205614548, 30.98035201082150536, -5.440088680355545492 ) ) ;
#5157 = AXIS2_PLACEMENT_3D ( 'NONE', #29918, #67941, #91914 ) ;
#5158 = CARTESIAN_POINT ( 'NONE',  ( 2.791683348922240793, 46.63393115100077324, 7.208316651077764092 ) ) ;
#5159 = CARTESIAN_POINT ( 'NONE',  ( 20.88017736071110875, 50.77201867748817676, -2.915334737309920765 ) ) ;
#5160 = CARTESIAN_POINT ( 'NONE',  ( -4.164238869374098151, 36.59541550158063217, -3.795296366450310543 ) ) ;
#5161 = CARTESIAN_POINT ( 'NONE',  ( -7.750000000000000000, 79.82179676972448590, 6.250000000000000000 ) ) ;
#5162 = UNCERTAINTY_MEASURE_WITH_UNIT (LENGTH_MEASURE( 1.000000000000000082E-05 ), #13393, 'distance_accuracy_value', 'NONE');
#5163 = CARTESIAN_POINT ( 'NONE',  ( 1.472469842513823179, 41.42559781766745886, 4.923371831947296329 ) ) ;
#5164 = CARTESIAN_POINT ( 'NONE',  ( 3.591859063236763294, 63.29030133659708923, -11.09922568453595026 ) ) ;
#5165 = CARTESIAN_POINT ( 'NONE',  ( -1.099225684535947600, -0.4596986634029132657, 6.408140936763237150 ) ) ;
#5166 = ORIENTED_EDGE ( 'NONE', *, *, #81160, .F. ) ;
#5167 = CARTESIAN_POINT ( 'NONE',  ( 7.084665262690076126, 19.10535201082150181, 10.88017736071109987 ) ) ;
#5168 = EDGE_CURVE ( 'NONE', #26330, #29532, #19761, .T. ) ;
#5169 = CARTESIAN_POINT ( 'NONE',  ( 20.15039907845753930, 70.00000000000000000, 6.262539305110068177 ) ) ;
#5170 = CARTESIAN_POINT ( 'NONE',  ( -0.8801773607111009756, 3.063685344154837509, 1.068504757029289695E-15 ) ) ;
#5171 = CARTESIAN_POINT ( 'NONE',  ( -0.8801773607111009756, 13.06368534415483929, 1.068504757029289695E-15 ) ) ;
#5172 = CARTESIAN_POINT ( 'NONE',  ( 0.1532563361054100626, 5.800597817667452638, -2.638427012816831230 ) ) ;
#5173 = CARTESIAN_POINT ( 'NONE',  ( 10.00000000000000178, 18.05374883491396787, 14.16423886937410082 ) ) ;
#5174 = CARTESIAN_POINT ( 'NONE',  ( 14.92337183194729988, 19.34226448433411960, -8.527530157486177487 ) ) ;
#5175 = CARTESIAN_POINT ( 'NONE',  ( 14.92337183194729633, 62.67559781766745886, 8.527530157486181039 ) ) ;
#5176 = CARTESIAN_POINT ( 'NONE',  ( 19.42250999205614548, 35.98035201082151247, -5.440088680355545492 ) ) ;
#5177 =( BOUNDED_SURFACE ( )  B_SPLINE_SURFACE ( 1, 2, ( 
 ( #33333, #63827, #94341, #56833, #75781, #37803, #5814, #66803, #29776, #60286, #51308, #67802, #50819, #81312, #96832, #37313, #97324, #7304, #83290, #36307, #28794, #51804, #88811, #52295, #6799, #52781, #89309, #59296, #14815, #90783, #20817, #29289, #82288, #66298, #89793, #68300, #98819, #21311, #13808, #22309, #45286, #81790, #98322, #12807, #43307, #28309, #58295, #44292, #20323, #73800, #74796, #6304, #36806, #67300, #5330, #82791, #97827, #14313, #35811, #75289, #58801, #59786, #90279, #21811, #13307, #43793, #44783, #74287, #54258, #47245, #8764, #15791, #32240, #55243, #22798, #1299, #84769, #69280, #62247, #16278, #24278, #77255, #9754, #53276, #76764, #16770, #61751, #83783, #23298, #85757, #31752, #802, #15306, #320, #30762, #17268, #45791, #91276, #62739, #47743, #38293, #7797, #92269, #46760, #77746, #68788, #39281, #23793, #92753, #46279, #61268, #93239, #54742, #24765, #78240, #40256, #69769, #9259, #70763, #70266, #91776, #85263, #53776, #76282, #84292, #8284, #39766, #38781, #1782, #30272, #60774, #31255, #71731, #33225, #32733, #93736, #63720, #41256, #2771, #33707, #80704, #71248, #26229, #3241, #65190, #94223, #56722, #34697, #40744, #79721, #95203, #4227, #19706, #50193, #64207, #87700, #12199, #42224, #25753, #11221, #56247, #55753, #48234, #86740, #19216, #86244, #94722, #41740, #72211, #72690, #87214, #18242, #63233, #25270, #48723, #18737, #79227, #49217, #42708, #10737, #3739, #34199, #95712, #64692, #26708, #27195, #57203, #49697, #17757, #80206, #11712, #57697, #88197, #2277, #78743, #10251, #35694, #44170, #97212, #81193, #81673, #90660, #52667, #20699, #13188, #44674, #75168, #66178, #82674, #65687, #96211, #12694, #52180, #43680, #22186, #98198, #51191, #74167, #66687, #51692, #21694, #97705, #5701, #29171, #60164, #90164, #83169, #82171, #36187, #89679, #14190, #96712, #28680, #59174, #21192, #6678, #13684, #58685, #37198, #29655, #27693, #74678, #6190, #36694, #67182, #59672, #67689, #14694, #73186, #58177, #4722, #35185, #88689, #20197, #28190, #50699, #43190, #73678, #5210, #89186, #45665, #1667, #98700, #7179, #47123, #32116, #53162, #22681, #8167, #69163, #62123, #83667, #687, #38658, #77139, #30641, #15185, #77623, #62614, #31138, #24154, #39654, #37682, #93121, #9138, #53654, #61631, #46163, #92150, #24648, #91659, #194, #70146, #55117, #76162, #23675, #15678, #85635, #45164, #7684, #54622, #30149, #38177, #68667, #61150, #75668, #54137, #84650, #76646, #84173, #68181, #16153, #23177, #46637, #60658, #91157, #8648, #39158, #85143, #69648, #1172, #31632, #92631, #16651, #87100 ),
 ( #41133, #49580, #55631, #94602, #47632, #11109, #64577, #11595, #48112, #94109, #72576, #19099, #78626, #18614, #71621, #25154, #25637, #34573, #95595, #63604, #56127, #87587, #80090, #10137, #26591, #9638, #40136, #86131, #95086, #86622, #65069, #42114, #18133, #48605, #10621, #26119, #57093, #41628, #79109, #72093, #4109, #34086, #27080, #56611, #3132, #33592, #57581, #40632, #64087, #49103, #79606, #17153, #3617, #2657, #78128, #70636, #2164, #32619, #63117, #93619, #17644, #71130, #33109, #36069, #67570, #80591, #35575, #74560, #20585, #42591, #81077, #13069, #6076, #27575, #43561, #51070, #21076, #73564, #58070, #90055, #82060, #21578, #6562, #37072, #81562, #36577, #98082, #29051, #20077, #66570, #50582, #73071, #35068, #12580, #67065, #4607, #74059, #97099, #28570, #59558, #58566, #43078, #19589, #12086, #5088, #28069, #88573, #5592, #29541, #66066, #59063, #89071, #52066, #96594, #89567, #82561, #51574, #13568, #50087, #44055, #97591, #14077, #44557, #75053, #88077, #65567, #96093, #31024, #84044, #68059, #68553, #77505, #39536, #7575, #85, #31516, #62015, #53037, #69535, #52551, #83055, #98589, #39041, #30532, #9019, #85025, #38061, #61033, #53531, #38550, #8540, #84540, #91545, #16037, #47015, #77026, #70028, #69045, #23062, #76535, #1048, #22568, #15565, #46049, #8050, #92515, #579, #45545, #24040, #16538, #14576, #61520, #92030, #23560, #54028, #46526, #54512, #1552, #60046, #45043, #90544, #22076, #75552, #7068, #83553, #37568, #30038, #60546, #91039, #15076, #76042, #87475, #85520, #93007, #33960, #18990, #40017, #9517, #93999, #49467, #79973, #63497, #18494, #11479, #71978, #63003, #10498, #93505, #17030, #78010, #25030, #48982, #47509, #25523, #41011, #71511, #3503, #2539, #55517, #62504, #24541, #86016, #71017, #32505, #56009, #41996, #2044, #86513, #32994, #94972, #17529, #18010, #64465, #70521, #3025, #55002, #26000, #79491, #26474, #47996, #10019, #72460, #56972, #78506, #33473, #48490, #40520, #78993, #31998, #63970, #94482, #56495, #86985, #10991, #41512, #13446, #95478, #26966, #42473, #81936, #12461, #21451, #28928, #80961, #73447, #96476, #81448, #51450, #28450, #42966, #58947, #89934, #20962, #82433, #12949, #4973, #20464, #43933, #65451, #35453, #65949, #27949, #74430, #43444, #88459, #5958, #59432, #57467, #73945, #58441, #88955, #35946, #50953, #96976, #5474, #13958, #87960, #50455, #89449, #66442, #19476, #95976, #51948, #36451, #66943, #49966, #72957, #4486, #44432, #80472, #64950, #97463, #3994, #11970, #34953, #34459, #27459, #57952, #19960, #75921, #83429, #22942, #67939, #82932, #30904 ) ),
 .UNSPECIFIED., .F., .F., .F. ) 
 B_SPLINE_SURFACE_WITH_KNOTS ( ( 2, 2 ),
 ( 3, 2, 2, 2, 2, 2, 2, 2, 2, 2, 2, 2, 2, 2, 2, 2, 2, 2, 2, 2, 2, 2, 2, 2, 2, 2, 2, 2, 2, 2, 2, 2, 2, 2, 2, 2, 2, 2, 2, 2, 2, 2, 2, 2, 2, 2, 2, 2, 2, 2, 2, 2, 2, 2, 2, 2, 2, 2, 2, 2, 2, 2, 2, 2, 2, 2, 2, 2, 2, 2, 2, 2, 2, 2, 2, 2, 2, 2, 2, 2, 2, 2, 2, 2, 2, 2, 2, 2, 2, 2, 2, 2, 2, 2, 2, 2, 2, 2, 2, 2, 2, 2, 2, 2, 2, 2, 2, 2, 2, 2, 2, 2, 2, 2, 2, 2, 2, 2, 2, 2, 2, 2, 2, 2, 2, 2, 2, 2, 2, 2, 2, 2, 2, 2, 2, 2, 2, 2, 2, 2, 2, 2, 2, 2, 2, 2, 2, 2, 2, 2, 2, 2, 2, 2, 2, 2, 2, 2, 2, 2, 2, 2, 3 ),
 ( 0.000000000000000000, 1.000000000000000000 ),
 ( 0.000000000000000000, 0.005952380952380952051, 0.01190476190476190410, 0.01785714285714285615, 0.02380952380952380820, 0.02976190476190476025, 0.03571428571428571230, 0.04166666666666666435, 0.04761904761904761640, 0.05357142857142856845, 0.05952380952380952051, 0.06547619047619047949, 0.07142857142857142461, 0.07738095238095238360, 0.08333333333333332871, 0.08928571428571428770, 0.09523809523809523281, 0.1011904761904761918, 0.1071428571428571369, 0.1130952380952380959, 0.1190476190476190410, 0.1250000000000000000, 0.1309523809523809590, 0.1369047619047619180, 0.1428571428571428492, 0.1488095238095238082, 0.1547619047619047672, 0.1607142857142857262, 0.1666666666666666574, 0.1726190476190476164, 0.1785714285714285754, 0.1845238095238095344, 0.1904761904761904656, 0.1964285714285714246, 0.2023809523809523836, 0.2083333333333333426, 0.2142857142857142738, 0.2202380952380952328, 0.2261904761904761918, 0.2321428571428571508, 0.2380952380952380820, 0.2440476190476190410, 0.2500000000000000000, 0.2559523809523809312, 0.2619047619047619180, 0.2678571428571428492, 0.2738095238095238360, 0.2797619047619047672, 0.2857142857142856984, 0.2916666666666666852, 0.2976190476190476164, 0.3035714285714285476, 0.3095238095238095344, 0.3154761904761904656, 0.3214285714285714524, 0.3273809523809523836, 0.3333333333333333148, 0.3392857142857143016, 0.3452380952380952328, 0.3511904761904761640, 0.3571428571428571508, 0.3630952380952380820, 0.3690476190476190688, 0.3750000000000000000, 0.3809523809523809312, 0.3869047619047619180, 0.3928571428571428492, 0.3988095238095238360, 0.4047619047619047672, 0.4107142857142856984, 0.4166666666666666852, 0.4226190476190476164, 0.4285714285714285476, 0.4345238095238095344, 0.4404761904761904656, 0.4464285714285714524, 0.4523809523809523836, 0.4583333333333333148, 0.4642857142857143016, 0.4702380952380952328, 0.4761904761904761640, 0.4821428571428571508, 0.4880952380952380820, 0.4940476190476190688, 0.5000000000000000000, 0.5059523809523809312, 0.5119047619047618625, 0.5178571428571429047, 0.5238095238095238360, 0.5297619047619047672, 0.5357142857142856984, 0.5416666666666666297, 0.5476190476190476719, 0.5535714285714286031, 0.5595238095238095344, 0.5654761904761904656, 0.5714285714285713969, 0.5773809523809523281, 0.5833333333333333703, 0.5892857142857143016, 0.5952380952380952328, 0.6011904761904761640, 0.6071428571428570953, 0.6130952380952381375, 0.6190476190476190688, 0.6250000000000000000, 0.6309523809523809312, 0.6369047619047618625, 0.6428571428571429047, 0.6488095238095238360, 0.6547619047619047672, 0.6607142857142856984, 0.6666666666666666297, 0.6726190476190476719, 0.6785714285714286031, 0.6845238095238095344, 0.6904761904761904656, 0.6964285714285713969, 0.7023809523809523281, 0.7083333333333333703, 0.7142857142857143016, 0.7202380952380952328, 0.7261904761904761640, 0.7321428571428570953, 0.7380952380952381375, 0.7440476190476190688, 0.7500000000000000000, 0.7559523809523809312, 0.7619047619047618625, 0.7678571428571429047, 0.7738095238095238360, 0.7797619047619047672, 0.7857142857142856984, 0.7916666666666666297, 0.7976190476190476719, 0.8035714285714286031, 0.8095238095238095344, 0.8154761904761904656, 0.8214285714285713969, 0.8273809523809523281, 0.8333333333333333703, 0.8392857142857143016, 0.8452380952380952328, 0.8511904761904761640, 0.8571428571428570953, 0.8630952380952381375, 0.8690476190476190688, 0.8750000000000000000, 0.8809523809523809312, 0.8869047619047618625, 0.8928571428571429047, 0.8988095238095238360, 0.9047619047619047672, 0.9107142857142856984, 0.9166666666666666297, 0.9226190476190476719, 0.9285714285714286031, 0.9345238095238095344, 0.9404761904761904656, 0.9464285714285713969, 0.9523809523809523281, 0.9583333333333333703, 0.9642857142857143016 ),
 .UNSPECIFIED. ) 
 GEOMETRIC_REPRESENTATION_ITEM ( )  RATIONAL_B_SPLINE_SURFACE ( (
 ( 1.000000000000000000, 0.9659258262890683122, 1.000000000000000000, 0.9659258262890683122, 1.000000000000000000, 0.9659258262890683122, 1.000000000000000000, 0.9659258262890683122, 1.000000000000000000, 0.9659258262890683122, 1.000000000000000000, 0.9659258262890683122, 1.000000000000000000, 0.9659258262890683122, 1.000000000000000000, 0.9659258262890683122, 1.000000000000000000, 0.9659258262890683122, 1.000000000000000000, 0.9659258262890683122, 1.000000000000000000, 0.9659258262890683122, 1.000000000000000000, 0.9659258262890683122, 1.000000000000000000, 0.9659258262890683122, 1.000000000000000000, 0.9659258262890683122, 1.000000000000000000, 0.9659258262890683122, 1.000000000000000000, 0.9659258262890683122, 1.000000000000000000, 0.9659258262890683122, 1.000000000000000000, 0.9659258262890683122, 1.000000000000000000, 0.9659258262890683122, 1.000000000000000000, 0.9659258262890683122, 1.000000000000000000, 0.9659258262890683122, 1.000000000000000000, 0.9659258262890683122, 1.000000000000000000, 0.9659258262890683122, 1.000000000000000000, 0.9659258262890683122, 1.000000000000000000, 0.9659258262890683122, 1.000000000000000000, 0.9659258262890683122, 1.000000000000000000, 0.9659258262890683122, 1.000000000000000000, 0.9659258262890683122, 1.000000000000000000, 0.9659258262890683122, 1.000000000000000000, 0.9659258262890683122, 1.000000000000000000, 0.9659258262890683122, 1.000000000000000000, 0.9659258262890683122, 1.000000000000000000, 0.9659258262890683122, 1.000000000000000000, 0.9659258262890683122, 1.000000000000000000, 0.9659258262890683122, 1.000000000000000000, 0.9659258262890683122, 1.000000000000000000, 0.9659258262890683122, 1.000000000000000000, 0.9659258262890683122, 1.000000000000000000, 0.9659258262890683122, 1.000000000000000000, 0.9659258262890683122, 1.000000000000000000, 0.9659258262890683122, 1.000000000000000000, 0.9659258262890683122, 1.000000000000000000, 0.9659258262890683122, 1.000000000000000000, 0.9659258262890683122, 1.000000000000000000, 0.9659258262890683122, 1.000000000000000000, 0.9659258262890683122, 1.000000000000000000, 0.9659258262890683122, 1.000000000000000000, 0.9659258262890683122, 1.000000000000000000, 0.9659258262890683122, 1.000000000000000000, 0.9659258262890683122, 1.000000000000000000, 0.9659258262890683122, 1.000000000000000000, 0.9659258262890683122, 1.000000000000000000, 0.9659258262890683122, 1.000000000000000000, 0.9659258262890683122, 1.000000000000000000, 0.9659258262890683122, 1.000000000000000000, 0.9659258262890683122, 1.000000000000000000, 0.9659258262890683122, 1.000000000000000000, 0.9659258262890683122, 1.000000000000000000, 0.9659258262890683122, 1.000000000000000000, 0.9659258262890683122, 1.000000000000000000, 0.9659258262890683122, 1.000000000000000000, 0.9659258262890683122, 1.000000000000000000, 0.9659258262890683122, 1.000000000000000000, 0.9659258262890683122, 1.000000000000000000, 0.9659258262890683122, 1.000000000000000000, 0.9659258262890683122, 1.000000000000000000, 0.9659258262890683122, 1.000000000000000000, 0.9659258262890683122, 1.000000000000000000, 0.9659258262890683122, 1.000000000000000000, 0.9659258262890683122, 1.000000000000000000, 0.9659258262890683122, 1.000000000000000000, 0.9659258262890683122, 1.000000000000000000, 0.9659258262890683122, 1.000000000000000000, 0.9659258262890683122, 1.000000000000000000, 0.9659258262890683122, 1.000000000000000000, 0.9659258262890683122, 1.000000000000000000, 0.9659258262890683122, 1.000000000000000000, 0.9659258262890683122, 1.000000000000000000, 0.9659258262890683122, 1.000000000000000000, 0.9659258262890683122, 1.000000000000000000, 0.9659258262890683122, 1.000000000000000000, 0.9659258262890683122, 1.000000000000000000, 0.9659258262890683122, 1.000000000000000000, 0.9659258262890683122, 1.000000000000000000, 0.9659258262890683122, 1.000000000000000000, 0.9659258262890683122, 1.000000000000000000, 0.9659258262890683122, 1.000000000000000000, 0.9659258262890683122, 1.000000000000000000, 0.9659258262890683122, 1.000000000000000000, 0.9659258262890683122, 1.000000000000000000, 0.9659258262890683122, 1.000000000000000000, 0.9659258262890683122, 1.000000000000000000, 0.9659258262890683122, 1.000000000000000000, 0.9659258262890683122, 1.000000000000000000, 0.9659258262890683122, 1.000000000000000000, 0.9659258262890683122, 1.000000000000000000, 0.9659258262890683122, 1.000000000000000000, 0.9659258262890683122, 1.000000000000000000, 0.9659258262890683122, 1.000000000000000000, 0.9659258262890683122, 1.000000000000000000, 0.9659258262890683122, 1.000000000000000000, 0.9659258262890683122, 1.000000000000000000, 0.9659258262890683122, 1.000000000000000000, 0.9659258262890683122, 1.000000000000000000, 0.9659258262890683122, 1.000000000000000000, 0.9659258262890683122, 1.000000000000000000, 0.9659258262890683122, 1.000000000000000000, 0.9659258262890683122, 1.000000000000000000, 0.9659258262890683122, 1.000000000000000000, 0.9659258262890683122, 1.000000000000000000, 0.9659258262890683122, 1.000000000000000000, 0.9659258262890683122, 1.000000000000000000, 0.9659258262890683122, 1.000000000000000000, 0.9659258262890683122, 1.000000000000000000, 0.9659258262890683122, 1.000000000000000000, 0.9659258262890683122, 1.000000000000000000, 0.9659258262890683122, 1.000000000000000000, 0.9659258262890683122, 1.000000000000000000, 0.9659258262890683122, 1.000000000000000000, 0.9659258262890683122, 1.000000000000000000, 0.9659258262890683122, 1.000000000000000000, 0.9659258262890683122, 1.000000000000000000, 0.9659258262890683122, 1.000000000000000000, 0.9659258262890683122, 1.000000000000000000, 0.9659258262890683122, 1.000000000000000000, 0.9659258262890683122, 1.000000000000000000, 0.9659258262890683122, 1.000000000000000000, 0.9659258262890683122, 1.000000000000000000, 0.9659258262890683122, 1.000000000000000000, 0.9659258262890683122, 1.000000000000000000, 0.9659258262890683122, 1.000000000000000000, 0.9659258262890683122, 1.000000000000000000, 0.9659258262890683122, 1.000000000000000000, 0.9659258262890683122, 1.000000000000000000, 0.9659258262890683122, 1.000000000000000000, 0.9659258262890683122, 1.000000000000000000, 0.9659258262890683122, 1.000000000000000000, 0.9659258262890683122, 1.000000000000000000, 0.9659258262890683122, 1.000000000000000000, 0.9659258262890683122, 1.000000000000000000, 0.9659258262890683122, 1.000000000000000000, 0.9659258262890683122, 1.000000000000000000, 0.9659258262890683122, 1.000000000000000000, 0.9659258262890683122, 1.000000000000000000, 0.9659258262890683122, 1.000000000000000000, 0.9659258262890683122, 1.000000000000000000, 0.9659258262890683122, 1.000000000000000000, 0.9659258262890683122, 1.000000000000000000, 0.9659258262890683122, 1.000000000000000000, 0.9659258262890683122, 1.000000000000000000, 0.9659258262890683122, 1.000000000000000000, 0.9659258262890683122, 1.000000000000000000, 0.9659258262890683122, 1.000000000000000000, 0.9659258262890683122, 1.000000000000000000, 0.9659258262890683122, 1.000000000000000000, 0.9659258262890683122, 1.000000000000000000, 0.9659258262890683122, 1.000000000000000000, 0.9659258262890683122, 1.000000000000000000, 0.9659258262890683122, 1.000000000000000000, 0.9659258262890683122, 1.000000000000000000, 0.9659258262890683122, 1.000000000000000000, 0.9659258262890683122, 1.000000000000000000),
 ( 1.000000000000000000, 0.9659258262890683122, 1.000000000000000000, 0.9659258262890683122, 1.000000000000000000, 0.9659258262890683122, 1.000000000000000000, 0.9659258262890683122, 1.000000000000000000, 0.9659258262890683122, 1.000000000000000000, 0.9659258262890683122, 1.000000000000000000, 0.9659258262890683122, 1.000000000000000000, 0.9659258262890683122, 1.000000000000000000, 0.9659258262890683122, 1.000000000000000000, 0.9659258262890683122, 1.000000000000000000, 0.9659258262890683122, 1.000000000000000000, 0.9659258262890683122, 1.000000000000000000, 0.9659258262890683122, 1.000000000000000000, 0.9659258262890683122, 1.000000000000000000, 0.9659258262890683122, 1.000000000000000000, 0.9659258262890683122, 1.000000000000000000, 0.9659258262890683122, 1.000000000000000000, 0.9659258262890683122, 1.000000000000000000, 0.9659258262890683122, 1.000000000000000000, 0.9659258262890683122, 1.000000000000000000, 0.9659258262890683122, 1.000000000000000000, 0.9659258262890683122, 1.000000000000000000, 0.9659258262890683122, 1.000000000000000000, 0.9659258262890683122, 1.000000000000000000, 0.9659258262890683122, 1.000000000000000000, 0.9659258262890683122, 1.000000000000000000, 0.9659258262890683122, 1.000000000000000000, 0.9659258262890683122, 1.000000000000000000, 0.9659258262890683122, 1.000000000000000000, 0.9659258262890683122, 1.000000000000000000, 0.9659258262890683122, 1.000000000000000000, 0.9659258262890683122, 1.000000000000000000, 0.9659258262890683122, 1.000000000000000000, 0.9659258262890683122, 1.000000000000000000, 0.9659258262890683122, 1.000000000000000000, 0.9659258262890683122, 1.000000000000000000, 0.9659258262890683122, 1.000000000000000000, 0.9659258262890683122, 1.000000000000000000, 0.9659258262890683122, 1.000000000000000000, 0.9659258262890683122, 1.000000000000000000, 0.9659258262890683122, 1.000000000000000000, 0.9659258262890683122, 1.000000000000000000, 0.9659258262890683122, 1.000000000000000000, 0.9659258262890683122, 1.000000000000000000, 0.9659258262890683122, 1.000000000000000000, 0.9659258262890683122, 1.000000000000000000, 0.9659258262890683122, 1.000000000000000000, 0.9659258262890683122, 1.000000000000000000, 0.9659258262890683122, 1.000000000000000000, 0.9659258262890683122, 1.000000000000000000, 0.9659258262890683122, 1.000000000000000000, 0.9659258262890683122, 1.000000000000000000, 0.9659258262890683122, 1.000000000000000000, 0.9659258262890683122, 1.000000000000000000, 0.9659258262890683122, 1.000000000000000000, 0.9659258262890683122, 1.000000000000000000, 0.9659258262890683122, 1.000000000000000000, 0.9659258262890683122, 1.000000000000000000, 0.9659258262890683122, 1.000000000000000000, 0.9659258262890683122, 1.000000000000000000, 0.9659258262890683122, 1.000000000000000000, 0.9659258262890683122, 1.000000000000000000, 0.9659258262890683122, 1.000000000000000000, 0.9659258262890683122, 1.000000000000000000, 0.9659258262890683122, 1.000000000000000000, 0.9659258262890683122, 1.000000000000000000, 0.9659258262890683122, 1.000000000000000000, 0.9659258262890683122, 1.000000000000000000, 0.9659258262890683122, 1.000000000000000000, 0.9659258262890683122, 1.000000000000000000, 0.9659258262890683122, 1.000000000000000000, 0.9659258262890683122, 1.000000000000000000, 0.9659258262890683122, 1.000000000000000000, 0.9659258262890683122, 1.000000000000000000, 0.9659258262890683122, 1.000000000000000000, 0.9659258262890683122, 1.000000000000000000, 0.9659258262890683122, 1.000000000000000000, 0.9659258262890683122, 1.000000000000000000, 0.9659258262890683122, 1.000000000000000000, 0.9659258262890683122, 1.000000000000000000, 0.9659258262890683122, 1.000000000000000000, 0.9659258262890683122, 1.000000000000000000, 0.9659258262890683122, 1.000000000000000000, 0.9659258262890683122, 1.000000000000000000, 0.9659258262890683122, 1.000000000000000000, 0.9659258262890683122, 1.000000000000000000, 0.9659258262890683122, 1.000000000000000000, 0.9659258262890683122, 1.000000000000000000, 0.9659258262890683122, 1.000000000000000000, 0.9659258262890683122, 1.000000000000000000, 0.9659258262890683122, 1.000000000000000000, 0.9659258262890683122, 1.000000000000000000, 0.9659258262890683122, 1.000000000000000000, 0.9659258262890683122, 1.000000000000000000, 0.9659258262890683122, 1.000000000000000000, 0.9659258262890683122, 1.000000000000000000, 0.9659258262890683122, 1.000000000000000000, 0.9659258262890683122, 1.000000000000000000, 0.9659258262890683122, 1.000000000000000000, 0.9659258262890683122, 1.000000000000000000, 0.9659258262890683122, 1.000000000000000000, 0.9659258262890683122, 1.000000000000000000, 0.9659258262890683122, 1.000000000000000000, 0.9659258262890683122, 1.000000000000000000, 0.9659258262890683122, 1.000000000000000000, 0.9659258262890683122, 1.000000000000000000, 0.9659258262890683122, 1.000000000000000000, 0.9659258262890683122, 1.000000000000000000, 0.9659258262890683122, 1.000000000000000000, 0.9659258262890683122, 1.000000000000000000, 0.9659258262890683122, 1.000000000000000000, 0.9659258262890683122, 1.000000000000000000, 0.9659258262890683122, 1.000000000000000000, 0.9659258262890683122, 1.000000000000000000, 0.9659258262890683122, 1.000000000000000000, 0.9659258262890683122, 1.000000000000000000, 0.9659258262890683122, 1.000000000000000000, 0.9659258262890683122, 1.000000000000000000, 0.9659258262890683122, 1.000000000000000000, 0.9659258262890683122, 1.000000000000000000, 0.9659258262890683122, 1.000000000000000000, 0.9659258262890683122, 1.000000000000000000, 0.9659258262890683122, 1.000000000000000000, 0.9659258262890683122, 1.000000000000000000, 0.9659258262890683122, 1.000000000000000000, 0.9659258262890683122, 1.000000000000000000, 0.9659258262890683122, 1.000000000000000000, 0.9659258262890683122, 1.000000000000000000, 0.9659258262890683122, 1.000000000000000000, 0.9659258262890683122, 1.000000000000000000, 0.9659258262890683122, 1.000000000000000000, 0.9659258262890683122, 1.000000000000000000, 0.9659258262890683122, 1.000000000000000000, 0.9659258262890683122, 1.000000000000000000, 0.9659258262890683122, 1.000000000000000000, 0.9659258262890683122, 1.000000000000000000, 0.9659258262890683122, 1.000000000000000000, 0.9659258262890683122, 1.000000000000000000, 0.9659258262890683122, 1.000000000000000000, 0.9659258262890683122, 1.000000000000000000, 0.9659258262890683122, 1.000000000000000000, 0.9659258262890683122, 1.000000000000000000, 0.9659258262890683122, 1.000000000000000000, 0.9659258262890683122, 1.000000000000000000, 0.9659258262890683122, 1.000000000000000000, 0.9659258262890683122, 1.000000000000000000, 0.9659258262890683122, 1.000000000000000000, 0.9659258262890683122, 1.000000000000000000, 0.9659258262890683122, 1.000000000000000000, 0.9659258262890683122, 1.000000000000000000, 0.9659258262890683122, 1.000000000000000000, 0.9659258262890683122, 1.000000000000000000, 0.9659258262890683122, 1.000000000000000000, 0.9659258262890683122, 1.000000000000000000, 0.9659258262890683122, 1.000000000000000000, 0.9659258262890683122, 1.000000000000000000, 0.9659258262890683122, 1.000000000000000000, 0.9659258262890683122, 1.000000000000000000, 0.9659258262890683122, 1.000000000000000000, 0.9659258262890683122, 1.000000000000000000, 0.9659258262890683122, 1.000000000000000000, 0.9659258262890683122, 1.000000000000000000) ) ) 
 REPRESENTATION_ITEM ( '' )  SURFACE ( )  );
#5178 = CARTESIAN_POINT ( 'NONE',  ( 0.000000000000000000, 15.00000000000000000, 0.000000000000000000 ) ) ;
#5179 = ORIENTED_EDGE ( 'NONE', *, *, #70842, .T. ) ;
#5180 = AXIS2_PLACEMENT_3D ( 'NONE', #6702, #73703, #5237 ) ;
#5181 = CARTESIAN_POINT ( 'NONE',  ( 14.88232117145531141, 0.5000000000000004441, -1.875237731503139438 ) ) ;
#5182 = CARTESIAN_POINT ( 'NONE',  ( 18.52753015748617571, 43.09226448433412315, 4.923371831947298993 ) ) ;
#5183 = ORIENTED_EDGE ( 'NONE', *, *, #2414, .T. ) ;
#5184 = ORIENTED_EDGE ( 'NONE', *, *, #64565, .F. ) ;
#5185 = LINE ( 'NONE', #51169, #75688 ) ;
#5186 = CARTESIAN_POINT ( 'NONE',  ( 6.204703633549690345, 15.76208216824730179, -14.16423886937410259 ) ) ;
#5187 = CARTESIAN_POINT ( 'NONE',  ( 6.204703633549690345, 12.84541550158063572, 14.16423886937410082 ) ) ;
#5188 = CARTESIAN_POINT ( 'NONE',  ( 19.42250999205614193, 55.14701867748817676, 5.440088680355555262 ) ) ;
#5189 = CARTESIAN_POINT ( 'NONE',  ( 20.36894250292379382, 53.67874883491397497, 10.36894250292379205 ) ) ;
#5190 = CARTESIAN_POINT ( 'NONE',  ( 19.84674366389459621, 38.50893115100078745, 7.409399052514197653E-17 ) ) ;
#5191 = DIRECTION ( 'NONE',  ( -0.7132504491541751257, 0.000000000000000000, -0.7009092642998575595 ) ) ;
#5193 = CARTESIAN_POINT ( 'NONE',  ( 22.81628187352647785, 1.623634669930420271, 6.195893100308588602E-16 ) ) ;
#5192 = CARTESIAN_POINT ( 'NONE',  ( 19.42250999205614193, 30.14701867748817321, 5.440088680355555262 ) ) ;
#5194 = CARTESIAN_POINT ( 'NONE',  ( 24.16423886937409904, 9.095415501580633943, 3.795296366450317205 ) ) ;
#5195 = CARTESIAN_POINT ( 'NONE',  ( 6.204703633549690345, 55.76208216824730357, -14.16423886937410259 ) ) ;
#5196 = AXIS2_PLACEMENT_3D ( 'NONE', #85784, #86766, #47272 ) ;
#5197 = CARTESIAN_POINT ( 'NONE',  ( 12.91533473730993009, 21.60535201082150536, -10.88017736071109987 ) ) ;
#5198 = CARTESIAN_POINT ( 'NONE',  ( 18.52753015748617571, 38.09226448433412315, 4.923371831947298993 ) ) ;
#5199 = AXIS2_PLACEMENT_3D ( 'NONE', #49610, #49136, #12119 ) ;
#5200 = DIRECTION ( 'NONE',  ( 0.000000000000000000, 1.000000000000000000, 0.000000000000000000 ) ) ;
#5201 = CARTESIAN_POINT ( 'NONE',  ( 19.42250999205614193, 50.14701867748817676, 5.440088680355555262 ) ) ;
#5202 = VECTOR ( 'NONE', #74933, 1000.000000000000114 ) ;
#5203 = CARTESIAN_POINT ( 'NONE',  ( 0.000000000000000000, 15.00000000000000000, 0.000000000000000000 ) ) ;
#5204 = ORIENTED_EDGE ( 'NONE', *, *, #10522, .T. ) ;
#5205 = DIRECTION ( 'NONE',  ( 1.000000000000000000, 0.000000000000000000, 0.000000000000000000 ) ) ;
#5206 = CIRCLE ( 'NONE', #35521, 2.000000000000000888 ) ;
#5207 = ORIENTED_EDGE ( 'NONE', *, *, #9128, .T. ) ;
#5208 = ORIENTED_EDGE ( 'NONE', *, *, #82294, .F. ) ;
#5209 = CARTESIAN_POINT ( 'NONE',  ( 24.16423886937409904, 44.09541550158063927, 3.795296366450317205 ) ) ;
#5210 = CARTESIAN_POINT ( 'NONE',  ( 19.84674366389459621, 53.50893115100078745, 7.409399052514197653E-17 ) ) ;
#5211 = CARTESIAN_POINT ( 'NONE',  ( 0.5774900079438590739, 62.64701867748817676, -5.440088680355550821 ) ) ;
#5212 = CARTESIAN_POINT ( 'NONE',  ( 0.000000000000000000, 14.49999999999999822, 0.000000000000000000 ) ) ;
#5213 = EDGE_CURVE ( 'NONE', #72980, #65756, #51552, .T. ) ;
#5214 = AXIS2_PLACEMENT_3D ( 'NONE', #77425, #3294, #91949 ) ;
#5215 = CARTESIAN_POINT ( 'NONE',  ( 2.035157376598822676, 52.43868534415483396, -7.964842623401177768 ) ) ;
#5216 = EDGE_CURVE ( 'NONE', #42731, #37334, #43103, .T. ) ;
#5217 = EDGE_CURVE ( 'NONE', #34081, #74857, #90844, .T. ) ;
#5218 = CARTESIAN_POINT ( 'NONE',  ( 10.00000000000000178, 60.37363466993041783, 12.81628187352647608 ) ) ;
#5219 = CARTESIAN_POINT ( 'NONE',  ( -6.408140936763232709, 9.956968003263760636, 11.09922568453595026 ) ) ;
#5220 = ORIENTED_EDGE ( 'NONE', *, *, #11409, .F. ) ;
#5221 = CARTESIAN_POINT ( 'NONE',  ( 19.42250999205614193, 50.14701867748817676, 5.440088680355555262 ) ) ;
#5222 = CARTESIAN_POINT ( 'NONE',  ( 6.204703633549690345, 15.76208216824730179, -14.16423886937410259 ) ) ;
#5223 = CARTESIAN_POINT ( 'NONE',  ( 22.81628187352647785, 21.41530133659708923, 3.434112377981063169 ) ) ;
#5224 = ORIENTED_EDGE ( 'NONE', *, *, #23694, .T. ) ;
#5225 = TOROIDAL_SURFACE ( 'NONE', #37128, 14.49999999999999822, 0.5000000000000000000 ) ;
#5226 = CARTESIAN_POINT ( 'NONE',  ( 19.38216949554541202, 40.99863466993042493, 9.382169495545424454 ) ) ;
#5227 = CARTESIAN_POINT ( 'NONE',  ( 2.035157376598824452, 18.68868534415484106, 7.964842623401179544 ) ) ;
#5228 = CARTESIAN_POINT ( 'NONE',  ( 10.00000000000000000, 39.75893115100078745, -9.846743663894594434 ) ) ;
#5229 = CARTESIAN_POINT ( 'NONE',  ( 10.00000000000000000, 6.813685344154838397, -10.88017736071110342 ) ) ;
#5230 = EDGE_CURVE ( 'NONE', #73066, #9875, #69217, .T. ) ;
#5231 = DIRECTION ( 'NONE',  ( 0.000000000000000000, 0.000000000000000000, -1.000000000000000000 ) ) ;
#5232 = CARTESIAN_POINT ( 'NONE',  ( 18.52753015748618282, 48.92559781766745886, -4.923371831947291888 ) ) ;
#5234 = EDGE_LOOP ( 'NONE', ( #82702, #50428, #14183, #75758 ) ) ;
#5233 = CARTESIAN_POINT ( 'NONE',  ( 20.15039907845753220, 21.74884699246888786, 6.262539305110078836 ) ) ;
#5235 = VECTOR ( 'NONE', #31884, 1000.000000000000000 ) ;
#5236 = CARTESIAN_POINT ( 'NONE',  ( -0.1503990784575328088, 3.101585745166421493, 6.262539305110068177 ) ) ;
#5237 = DIRECTION ( 'NONE',  ( 4.263256414560601115E-14, 0.000000000000000000, 1.000000000000000000 ) ) ;
#5238 = SPHERICAL_SURFACE ( 'NONE', #18077, 0.2500000000000000000 ) ;
#5239 = CARTESIAN_POINT ( 'NONE',  ( -0.1503990784575242878, 44.24884699246889852, -6.262539305110083276 ) ) ;
#5240 = CARTESIAN_POINT ( 'NONE',  ( 12.63842701281683922, 24.55059781766745175, -9.846743663894590881 ) ) ;
#5241 = CARTESIAN_POINT ( 'NONE',  ( 13.43411237798105340, 20.58196800326374643, 12.81628187352647963 ) ) ;
#5242 = ADVANCED_FACE ( 'NONE', ( #13745 ), #52235, .F. ) ;
#5243 = CARTESIAN_POINT ( 'NONE',  ( 6.349999999999995204, -97.00000000000000000, 4.000000000000000000 ) ) ;
#5244 = VERTEX_POINT ( 'NONE', #61211 ) ;
#5245 = CARTESIAN_POINT ( 'NONE',  ( 19.84674366389459266, 63.30059781766745886, 2.638427012816836559 ) ) ;
#5246 = CARTESIAN_POINT ( 'NONE',  ( -13.30156849913876904, 0.2306972965111889762, -6.804875469488247397 ) ) ;
#5247 = CARTESIAN_POINT ( 'NONE',  ( -4.164238869374098151, 26.59541550158063217, -3.795296366450310543 ) ) ;
#5248 = CARTESIAN_POINT ( 'NONE',  ( 2.791683348922237240, 45.38393115100079456, -7.208316651077763204 ) ) ;
#5249 = CARTESIAN_POINT ( 'NONE',  ( 19.38216949554541202, 40.99863466993042493, 9.382169495545424454 ) ) ;
#5251 =( NAMED_UNIT ( * ) SI_UNIT ( $, .STERADIAN. ) SOLID_ANGLE_UNIT ( ) );
#5250 = CARTESIAN_POINT ( 'NONE',  ( -14.47650479471817242, 0.5000000000000004441, -3.928206833722204028 ) ) ;
#5252 = CARTESIAN_POINT ( 'NONE',  ( 19.42250999205614193, 60.14701867748817676, 5.440088680355555262 ) ) ;
#5253 = DIRECTION ( 'NONE',  ( 0.000000000000000000, 1.000000000000000000, 0.000000000000000000 ) ) ;
#5254 = CARTESIAN_POINT ( 'NONE',  ( 5.076628168052704559, 30.17559781766745175, -8.527530157486179263 ) ) ;
#5255 = CARTESIAN_POINT ( 'NONE',  ( 10.00000000000000178, 34.31368534415484106, 10.88017736071110342 ) ) ;
#5256 = CARTESIAN_POINT ( 'NONE',  ( 19.38216949554541202, 40.99863466993042493, 9.382169495545424454 ) ) ;
#5257 =( GEOMETRIC_REPRESENTATION_CONTEXT ( 3 ) GLOBAL_UNCERTAINTY_ASSIGNED_CONTEXT ( ( #75265 ) ) GLOBAL_UNIT_ASSIGNED_CONTEXT ( ( #40154, #55139, #53674 ) ) REPRESENTATION_CONTEXT ( 'NONE', 'WORKASPACE' ) );
#5258 = CARTESIAN_POINT ( 'NONE',  ( -45.94000000000000483, 92.00000000000000000, 9.500000000000000000 ) ) ;
#5259 = CARTESIAN_POINT ( 'NONE',  ( 4.559911319644449179, 28.89701867748817321, 9.422509992056141925 ) ) ;
#5260 = ORIENTED_EDGE ( 'NONE', *, *, #66249, .T. ) ;
#5261 = CIRCLE ( 'NONE', #77052, 15.00000000000000000 ) ;
#5262 = CARTESIAN_POINT ( 'NONE',  ( -45.94000000000001194, 107.5383484153110061, 12.00000000000000000 ) ) ;
#5263 = CARTESIAN_POINT ( 'NONE',  ( 15.44008868035555793, 21.39701867748817321, -9.422509992056140149 ) ) ;
#5265 = CARTESIAN_POINT ( 'NONE',  ( 10.00000000000000178, 39.31368534415484106, 10.88017736071110342 ) ) ;
#5264 = CARTESIAN_POINT ( 'NONE',  ( 5.076628168052703671, 61.84226448433412315, 8.527530157486179263 ) ) ;
#5266 = CARTESIAN_POINT ( 'NONE',  ( 8.880000000000020322, 80.32179676972448590, 4.250000000000000000 ) ) ;
#5267 = STYLED_ITEM ( 'NONE', ( #27313 ), #91888 ) ;
#5268 = CARTESIAN_POINT ( 'NONE',  ( 19.42250999205614193, 55.14701867748817676, 5.440088680355555262 ) ) ;
#5270 = DIRECTION ( 'NONE',  ( -1.000000000000000000, -2.653152395358074805E-16, 0.000000000000000000 ) ) ;
#5269 = CARTESIAN_POINT ( 'NONE',  ( 10.00000000000000000, 31.81368534415483751, -10.88017736071110342 ) ) ;
#5271 = CARTESIAN_POINT ( 'NONE',  ( 17.20831665107776587, 2.883931151000785231, 7.208316651077764980 ) ) ;
#5272 = CARTESIAN_POINT ( 'NONE',  ( 19.84674366389459621, 28.50893115100078745, 7.409399052514197653E-17 ) ) ;
#5273 = CARTESIAN_POINT ( 'NONE',  ( 14.49999999999999822, 75.00000000000000000, -6.500000000000000888 ) ) ;
#5274 = CARTESIAN_POINT ( 'NONE',  ( 3.795296366450314540, 3.262082168247304015, 14.16423886937410082 ) ) ;
#5275 = CARTESIAN_POINT ( 'NONE',  ( 5.076628168052704559, 55.17559781766745175, -8.527530157486179263 ) ) ;
#5277 = CARTESIAN_POINT ( 'NONE',  ( 6.935112714462088768, -80.58076677624440265, 3.750000000000000888 ) ) ;
#5276 = CARTESIAN_POINT ( 'NONE',  ( 24.16423886937409904, 49.09541550158063217, 3.795296366450317205 ) ) ;
#5278 = CARTESIAN_POINT ( 'NONE',  ( 6.000000000000000000, 11.50000000000000000, -6.500000000000000888 ) ) ;
#5279 = CARTESIAN_POINT ( 'NONE',  ( -0.3689425029237898834, 11.17874883491396787, -10.36894250292378850 ) ) ;
#5280 = ADVANCED_FACE ( 'NONE', ( #45224 ), #78296, .T. ) ;
#5281 = CARTESIAN_POINT ( 'NONE',  ( 24.16423886937410614, 34.51208216824731068, -3.795296366450302550 ) ) ;
#5282 = CARTESIAN_POINT ( 'NONE',  ( 21.09922568453595559, 7.040301336597086568, -6.408140936763230044 ) ) ;
#5283 = VERTEX_POINT ( 'NONE', #45723 ) ;
#5284 = CARTESIAN_POINT ( 'NONE',  ( 4.559911319644449179, 12.23035201082150714, -9.422509992056141925 ) ) ;
#5285 = CARTESIAN_POINT ( 'NONE',  ( 2.791683348922237240, 30.38393115100078390, -7.208316651077763204 ) ) ;
#5287 = CARTESIAN_POINT ( 'NONE',  ( 0.000000000000000000, 14.49999999999999822, 0.000000000000000000 ) ) ;
#5286 = DIRECTION ( 'NONE',  ( -0.9799247046208311440, 0.000000000000000000, 0.1993679344171901957 ) ) ;
#5288 = CARTESIAN_POINT ( 'NONE',  ( 24.35999999999999233, 44.49999999999997868, 10.00000000000000000 ) ) ;
#5289 = CARTESIAN_POINT ( 'NONE',  ( 18.52753015748617571, 3.092264484334118269, 4.923371831947298993 ) ) ;
#5290 = CARTESIAN_POINT ( 'NONE',  ( 0.6178305044545818747, 23.49863466993041783, -9.382169495545419124 ) ) ;
#5291 = CARTESIAN_POINT ( 'NONE',  ( 19.84674366389459266, 23.30059781766745530, 2.638427012816836559 ) ) ;
#5292 = VERTEX_POINT ( 'NONE', #90719 ) ;
#5293 = CARTESIAN_POINT ( 'NONE',  ( 12.63842701281683922, 14.55059781766744997, -9.846743663894590881 ) ) ;
#5294 = CARTESIAN_POINT ( 'NONE',  ( 0.5774900079438590739, 2.647018677488171434, -5.440088680355550821 ) ) ;
#5295 = CARTESIAN_POINT ( 'NONE',  ( 20.88017736071110875, 10.77201867748817143, -2.915334737309920765 ) ) ;
#5296 = VECTOR ( 'NONE', #50825, 1000.000000000000000 ) ;
#5297 = CARTESIAN_POINT ( 'NONE',  ( -2.266590686148945544, 36.38708216824730357, -7.082119434687050408 ) ) ;
#5298 = CARTESIAN_POINT ( 'NONE',  ( 20.88017736071110875, 60.77201867748817676, -2.915334737309920765 ) ) ;
#5299 = DIRECTION ( 'NONE',  ( 0.000000000000000000, -1.000000000000000000, 0.000000000000000000 ) ) ;
#5300 = CARTESIAN_POINT ( 'NONE',  ( 17.39651004071843232, 17.93575266056828355, 6.499999999999984013 ) ) ;
#5301 = CARTESIAN_POINT ( 'NONE',  ( 2.791683348922240793, 21.63393115100078745, 7.208316651077764092 ) ) ;
#5302 = CARTESIAN_POINT ( 'NONE',  ( 19.80448550324510038, 21.82703681773340421, 6.500000000002801315 ) ) ;
#5303 = CARTESIAN_POINT ( 'NONE',  ( 1.472469842513823179, 1.425597817667451528, 4.923371831947296329 ) ) ;
#5304 = LINE ( 'NONE', #19791, #19655 ) ;
#5305 = CARTESIAN_POINT ( 'NONE',  ( 14.92337183194729633, 32.67559781766745175, 8.527530157486181039 ) ) ;
#5306 = CARTESIAN_POINT ( 'NONE',  ( 2.791683348922237240, 60.38393115100078745, -7.208316651077763204 ) ) ;
#5307 = TOROIDAL_SURFACE ( 'NONE', #89936, 2.500000000000001776, 0.5000000000000000000 ) ;
#5308 = CARTESIAN_POINT ( 'NONE',  ( 10.00000000000000178, 34.31368534415484106, 10.88017736071110342 ) ) ;
#5309 = VERTEX_POINT ( 'NONE', #21754 ) ;
#5310 = CARTESIAN_POINT ( 'NONE',  ( 13.43411237798105340, 50.58196800326375353, 12.81628187352647963 ) ) ;
#5311 = DIRECTION ( 'NONE',  ( -0.5075383629606967650, 0.000000000000000000, -0.8616291604415300398 ) ) ;
#5312 = CARTESIAN_POINT ( 'NONE',  ( 12.91533473730992121, 64.52201867748817676, 10.88017736071110164 ) ) ;
#5313 = CARTESIAN_POINT ( 'NONE',  ( -2.816281873526473856, 44.12363466993042493, 9.499525473075851096E-16 ) ) ;
#5315 = CARTESIAN_POINT ( 'NONE',  ( 14.92337183194729633, 32.67559781766745175, 8.527530157486181039 ) ) ;
#5314 = CARTESIAN_POINT ( 'NONE',  ( -4.164238869374098151, 61.59541550158063217, -3.795296366450310543 ) ) ;
#5316 = CARTESIAN_POINT ( 'NONE',  ( 0.000000000000000000, 15.00000000000000000, 0.000000000000000000 ) ) ;
#5317 = LINE ( 'NONE', #26321, #42278 ) ;
#5318 = CARTESIAN_POINT ( 'NONE',  ( 17.08211943468705840, 20.13708216824730357, -12.26659068614894466 ) ) ;
#5319 = CARTESIAN_POINT ( 'NONE',  ( 10.00000000000000000, 45.55374883491397497, -14.16423886937410082 ) ) ;
#5320 = CARTESIAN_POINT ( 'NONE',  ( 7.361572987183169658, 49.96726448433410894, -9.846743663894592657 ) ) ;
#5321 = CARTESIAN_POINT ( 'NONE',  ( 20.10239578412225825, 12.63377557478296609, -6.340343622311917393 ) ) ;
#5322 = CARTESIAN_POINT ( 'NONE',  ( -0.8801773607111009756, 38.06368534415484106, 1.068504757029289695E-15 ) ) ;
#5323 = CARTESIAN_POINT ( 'NONE',  ( 17.96484262340118221, 56.18868534415484817, -7.964842623401177768 ) ) ;
#5324 = ORIENTED_EDGE ( 'NONE', *, *, #51919, .T. ) ;
#5325 = CARTESIAN_POINT ( 'NONE',  ( 13.43411237798105340, 40.58196800326375353, 12.81628187352647963 ) ) ;
#5326 = EDGE_CURVE ( 'NONE', #34926, #46257, #22244, .T. ) ;
#5327 = CARTESIAN_POINT ( 'NONE',  ( 20.88017736071110519, 65.56368534415483396, 2.639326808657452039E-16 ) ) ;
#5328 = ORIENTED_EDGE ( 'NONE', *, *, #4766, .F. ) ;
#5329 = CARTESIAN_POINT ( 'NONE',  ( -4.164238869374099039, 1.803748834913967647, 8.674139862899312516E-16 ) ) ;
#5330 = CARTESIAN_POINT ( 'NONE',  ( 0.1532563361054083140, 11.00893115100078568, 1.131784320476157264E-15 ) ) ;
#5331 = CARTESIAN_POINT ( 'NONE',  ( -1.926860441876563801, 59.89664270246083788, 3.195792623639529761 ) ) ;
#5332 = EDGE_LOOP ( 'NONE', ( #20026, #59252, #95572, #77600 ) ) ;
#5334 = EDGE_CURVE ( 'NONE', #16387, #65307, #76658, .T. ) ;
#5333 = DIRECTION ( 'NONE',  ( 0.000000000000000000, -0.000000000000000000, 1.000000000000000000 ) ) ;
#5335 = CARTESIAN_POINT ( 'NONE',  ( 2.035157376598824452, 13.68868534415483751, 7.964842623401179544 ) ) ;
#5336 = DIRECTION ( 'NONE',  ( -0.5519369853120617009, 0.000000000000000000, 0.8338858220671658827 ) ) ;
#5337 = CARTESIAN_POINT ( 'NONE',  ( -4.164238869374099039, 21.80374883491396787, 8.674139862899312516E-16 ) ) ;
#5338 = EDGE_CURVE ( 'NONE', #3713, #15093, #33534, .T. ) ;
#5339 = EDGE_CURVE ( 'NONE', #41390, #43512, #29659, .T. ) ;
#5340 = VECTOR ( 'NONE', #53191, 1000.000000000000227 ) ;
#5341 = CARTESIAN_POINT ( 'NONE',  ( 12.91533473730993009, 26.60535201082150536, -10.88017736071109987 ) ) ;
#5342 = CARTESIAN_POINT ( 'NONE',  ( 0.1532563361054082862, 66.21726448433413736, 2.638427012816831674 ) ) ;
#5343 = ORIENTED_EDGE ( 'NONE', *, *, #15317, .T. ) ;
#5344 =( GEOMETRIC_REPRESENTATION_CONTEXT ( 3 ) GLOBAL_UNCERTAINTY_ASSIGNED_CONTEXT ( ( #7477 ) ) GLOBAL_UNIT_ASSIGNED_CONTEXT ( ( #30333, #16829, #15371 ) ) REPRESENTATION_CONTEXT ( 'NONE', 'WORKASPACE' ) );
#5345 = CARTESIAN_POINT ( 'NONE',  ( 10.00000000000000000, 59.75893115100078745, -9.846743663894594434 ) ) ;
#5346 = ORIENTED_EDGE ( 'NONE', *, *, #11850, .F. ) ;
#5347 = CARTESIAN_POINT ( 'NONE',  ( 14.92337183194729633, 2.675597817667451750, 8.527530157486181039 ) ) ;
#5348 = CARTESIAN_POINT ( 'NONE',  ( 2.791683348922240793, 66.63393115100079456, 7.208316651077764092 ) ) ;
#5349 = CARTESIAN_POINT ( 'NONE',  ( 6.565887622018943937, 38.08196800326376064, -12.81628187352647608 ) ) ;
#5351 = LINE ( 'NONE', #80350, #31879 ) ;
#5350 = CARTESIAN_POINT ( 'NONE',  ( 10.00000000000000000, 11.81368534415483751, -10.88017736071110342 ) ) ;
#5352 = CARTESIAN_POINT ( 'NONE',  ( 2.035157376598824452, 68.68868534415484817, 7.964842623401179544 ) ) ;
#5353 = CARTESIAN_POINT ( 'NONE',  ( -0.8801773607111009756, 13.06368534415483929, 1.068504757029289695E-15 ) ) ;
#5354 = ORIENTED_EDGE ( 'NONE', *, *, #28574, .F. ) ;
#5355 = CARTESIAN_POINT ( 'NONE',  ( 13.43411237798105340, 55.58196800326374643, 12.81628187352647963 ) ) ;
#5356 = CARTESIAN_POINT ( 'NONE',  ( 17.96484262340118221, 41.18868534415484106, -7.964842623401177768 ) ) ;
#5357 = CARTESIAN_POINT ( 'NONE',  ( 19.67858290521088449, 89.80181819993967451, 5.461713021790604472 ) ) ;
#5358 = CARTESIAN_POINT ( 'NONE',  ( 21.09922568453595559, 42.04030133659708213, -6.408140936763230044 ) ) ;
#5359 = CARTESIAN_POINT ( 'NONE',  ( 17.96484262340118221, 49.93868534415484106, 7.964842623401181321 ) ) ;
#5360 = CARTESIAN_POINT ( 'NONE',  ( 18.52753015748617571, 53.09226448433412315, 4.923371831947298993 ) ) ;
#5362 = VERTEX_POINT ( 'NONE', #98759 ) ;
#5361 = EDGE_CURVE ( 'NONE', #11450, #7152, #37743, .T. ) ;
#5363 = CARTESIAN_POINT ( 'NONE',  ( 12.63842701281683922, 14.55059781766744997, -9.846743663894590881 ) ) ;
#5364 = CARTESIAN_POINT ( 'NONE',  ( 10.00000000000000000, 2.873634669930420049, -12.81628187352647608 ) ) ;
#5366 = CARTESIAN_POINT ( 'NONE',  ( 19.84674366389459266, 58.30059781766745886, 2.638427012816836559 ) ) ;
#5365 = CARTESIAN_POINT ( 'NONE',  ( 10.64017930668202183, 0.3639309529147286004, 10.57291749337224296 ) ) ;
#5367 = CARTESIAN_POINT ( 'NONE',  ( 2.035157376598822676, 17.43868534415483751, -7.964842623401177768 ) ) ;
#5368 = CARTESIAN_POINT ( 'NONE',  ( 2.791683348922237240, 55.38393115100078745, -7.208316651077763204 ) ) ;
#5369 = CARTESIAN_POINT ( 'NONE',  ( 5.500000000000000000, 11.00000000000000000, -6.000000000000000000 ) ) ;
#5370 =( NAMED_UNIT ( * ) PLANE_ANGLE_UNIT ( ) SI_UNIT ( $, .RADIAN. ) );
#5371 = VECTOR ( 'NONE', #90727, 1000.000000000000000 ) ;
#5372 = CARTESIAN_POINT ( 'NONE',  ( 1.472469842513823179, 11.42559781766745175, 4.923371831947296329 ) ) ;
#5373 = FILL_AREA_STYLE_COLOUR ( '', #4268 ) ;
#5375 = ORIENTED_EDGE ( 'NONE', *, *, #66083, .F. ) ;
#5374 = CARTESIAN_POINT ( 'NONE',  ( -2.816281873526473856, -0.8763653300695799508, 9.499525473075851096E-16 ) ) ;
#5376 = ADVANCED_FACE ( 'NONE', ( #30209 ), #75994, .T. ) ;
#5377 = CARTESIAN_POINT ( 'NONE',  ( 1.274849032794294290, 63.57228050351031357, 6.499999999999979572 ) ) ;
#5378 = CARTESIAN_POINT ( 'NONE',  ( 6.898461952320324109, 15.00000000000000000, 12.75387089053312373 ) ) ;
#5379 = CARTESIAN_POINT ( 'NONE',  ( 6.565887622018943937, 43.08196800326374643, -12.81628187352647608 ) ) ;
#5380 = CARTESIAN_POINT ( 'NONE',  ( 7.361572987183169658, 29.96726448433411960, -9.846743663894592657 ) ) ;
#5381 = CARTESIAN_POINT ( 'NONE',  ( 1.274849032794278747, 57.55509018479938277, -6.499999999999960032 ) ) ;
#5382 = CARTESIAN_POINT ( 'NONE',  ( 17.08211943468705130, 58.47041550158063927, 12.26659068614894998 ) ) ;
#5383 = CARTESIAN_POINT ( 'NONE',  ( 1.472469842513823179, 31.42559781766745530, 4.923371831947296329 ) ) ;
#5384 = ORIENTED_EDGE ( 'NONE', *, *, #66318, .F. ) ;
#5385 = CARTESIAN_POINT ( 'NONE',  ( -9.399392868737665552, 3.795627280083113010E-16, -11.04089732309487104 ) ) ;
#5386 = CARTESIAN_POINT ( 'NONE',  ( 10.00000000000000000, 50.55374883491396787, -14.16423886937410082 ) ) ;
#5387 = CARTESIAN_POINT ( 'NONE',  ( -9.347645168806021587, 88.42200471242378512, -5.276767730577755167 ) ) ;
#5388 = CARTESIAN_POINT ( 'NONE',  ( 12.91533473730992121, 14.52201867748817143, 10.88017736071110164 ) ) ;
#5389 = CARTESIAN_POINT ( 'NONE',  ( 6.204703633549690345, 35.76208216824729647, -14.16423886937410259 ) ) ;
#5391 = CARTESIAN_POINT ( 'NONE',  ( 0.2751277870542967463, 70.00000000000000000, -6.000000000000000000 ) ) ;
#5390 = CARTESIAN_POINT ( 'NONE',  ( 24.16423886937410614, 59.51208216824728936, -3.795296366450302550 ) ) ;
#5392 = LINE ( 'NONE', #81367, #64332 ) ;
#5393 = CARTESIAN_POINT ( 'NONE',  ( 2.791683348922240793, 11.63393115100078568, 7.208316651077764092 ) ) ;
#5394 = CARTESIAN_POINT ( 'NONE',  ( 13.43411237798105340, 5.581968003263753531, 12.81628187352647963 ) ) ;
#5395 = CARTESIAN_POINT ( 'NONE',  ( 18.28836319691945889, 14.34492782695770785, 6.500000000000000888 ) ) ;
#5396 = ORIENTED_EDGE ( 'NONE', *, *, #9194, .T. ) ;
#5397 = CARTESIAN_POINT ( 'NONE',  ( 10.00000000000000000, 51.81368534415484106, -10.88017736071110342 ) ) ;
#5398 = FACE_OUTER_BOUND ( 'NONE', #18255, .T. ) ;
#5399 = CARTESIAN_POINT ( 'NONE',  ( 4.267749253172036461, 0.000000000000000000, 3.394721039305376387 ) ) ;
#5400 = CYLINDRICAL_SURFACE ( 'NONE', #53149, 4.000000000000001776 ) ;
#5401 = CARTESIAN_POINT ( 'NONE',  ( 20.00000000000000711, 79.40087001978915282, -4.500000000000000000 ) ) ;
#5402 = ORIENTED_EDGE ( 'NONE', *, *, #67548, .T. ) ;
#5403 = CIRCLE ( 'NONE', #61273, 15.00000000000000000 ) ;
#5404 = CARTESIAN_POINT ( 'NONE',  ( -0.3689425029237881626, 37.42874883491396787, 10.36894250292379027 ) ) ;
#5405 = EDGE_LOOP ( 'NONE', ( #34767, #10259, #30265, #6912, #72865, #6651 ) ) ;
#5406 = CARTESIAN_POINT ( 'NONE',  ( 5.076628168052704559, 0.1755978176674514724, -8.527530157486179263 ) ) ;
#5408 = CARTESIAN_POINT ( 'NONE',  ( -3.014428414850141458, 6.880135511184874986, -11.24999999999999822 ) ) ;
#5407 = DIRECTION ( 'NONE',  ( 0.000000000000000000, 1.000000000000000000, 0.000000000000000000 ) ) ;
#5409 = CARTESIAN_POINT ( 'NONE',  ( 20.88017736071110519, 20.56368534415484106, 2.639326808657452039E-16 ) ) ;
#5410 = CARTESIAN_POINT ( 'NONE',  ( 13.43411237798106583, 42.66530133659707502, -12.81628187352647252 ) ) ;
#5411 = CARTESIAN_POINT ( 'NONE',  ( 10.00000000000000000, 6.813685344154838397, -10.88017736071110342 ) ) ;
#5412 = CARTESIAN_POINT ( 'NONE',  ( -1.099225684535947600, 28.70696800326375353, -6.408140936763238038 ) ) ;
#5413 = CARTESIAN_POINT ( 'NONE',  ( 16.40814093676324603, 57.45696800326375353, -11.09922568453594671 ) ) ;
#5414 = ORIENTED_EDGE ( 'NONE', *, *, #90421, .T. ) ;
#5415 = AXIS2_PLACEMENT_3D ( 'NONE', #52469, #75958, #14491 ) ;
#5416 = CARTESIAN_POINT ( 'NONE',  ( -10.82078848414227146, 15.00000000000000000, 11.78082904627290795 ) ) ;
#5417 = LINE ( 'NONE', #35395, #87722 ) ;
#5418 = CARTESIAN_POINT ( 'NONE',  ( 24.16423886937410614, 24.30374883491396787, 8.672049930838204340E-16 ) ) ;
#5419 = CARTESIAN_POINT ( 'NONE',  ( -2.266590686148945544, 6.387082168247300906, -7.082119434687050408 ) ) ;
#5420 = CARTESIAN_POINT ( 'NONE',  ( 14.43100913236846772, 15.00000000000000000, 1.412789942453269054 ) ) ;
#5421 = CARTESIAN_POINT ( 'NONE',  ( 0.5774900079438607392, 28.48035201082150891, 5.440088680355550821 ) ) ;
#5422 = DIRECTION ( 'NONE',  ( 0.000000000000000000, 0.000000000000000000, 1.000000000000000000 ) ) ;
#5423 = CARTESIAN_POINT ( 'NONE',  ( 8.879999999999995453, 40.74999999999999289, 4.250000000000000000 ) ) ;
#5424 = CARTESIAN_POINT ( 'NONE',  ( -0.8801773607111009756, 58.06368534415484106, 1.068504757029289695E-15 ) ) ;
#5425 = CARTESIAN_POINT ( 'NONE',  ( 17.96484262340118221, 49.93868534415484106, 7.964842623401181321 ) ) ;
#5426 = CARTESIAN_POINT ( 'NONE',  ( 19.38216949554541202, 15.99863466993042138, 9.382169495545424454 ) ) ;
#5427 = CARTESIAN_POINT ( 'NONE',  ( 0.1089645850228985746, 48.16234555792571115, 6.479102184480827198 ) ) ;
#5428 = DIRECTION ( 'NONE',  ( -0.000000000000000000, -1.000000000000000000, -0.000000000000000000 ) ) ;
#5429 = CARTESIAN_POINT ( 'NONE',  ( 7.361572987183169658, 24.96726448433412315, -9.846743663894592657 ) ) ;
#5430 = FACE_OUTER_BOUND ( 'NONE', #68172, .T. ) ;
#5431 = EDGE_CURVE ( 'NONE', #15047, #60197, #18477, .T. ) ;
#5432 = CARTESIAN_POINT ( 'NONE',  ( -0.8801773607111008646, 38.27201867748816255, 2.915334737309923430 ) ) ;
#5433 = UNCERTAINTY_MEASURE_WITH_UNIT (LENGTH_MEASURE( 1.000000000000000082E-05 ), #98904, 'distance_accuracy_value', 'NONE');
#5434 = CARTESIAN_POINT ( 'NONE',  ( 3.591859063236761518, 9.956968003263753531, 11.09922568453594849 ) ) ;
#5435 = CARTESIAN_POINT ( 'NONE',  ( 1.472469842513823179, 26.42559781766745175, 4.923371831947296329 ) ) ;
#5436 = CARTESIAN_POINT ( 'NONE',  ( 0.6178305044545838731, 54.74863466993042493, 9.382169495545420901 ) ) ;
#5437 = CARTESIAN_POINT ( 'NONE',  ( 0.1532563361054100626, 10.80059781766745175, -2.638427012816831230 ) ) ;
#5438 = ORIENTED_EDGE ( 'NONE', *, *, #12359, .T. ) ;
#5439 = CARTESIAN_POINT ( 'NONE',  ( 20.15039907845753220, 41.74884699246887720, 6.262539305110078836 ) ) ;
#5440 = CARTESIAN_POINT ( 'NONE',  ( 18.95785429995060767, 27.24216108172003104, 6.499999999999853451 ) ) ;
#5441 = CARTESIAN_POINT ( 'NONE',  ( 0.5774900079438607392, 13.48035201082150358, 5.440088680355550821 ) ) ;
#5443 = CARTESIAN_POINT ( 'NONE',  ( 17.08211943468705840, 30.13708216824730357, -12.26659068614894466 ) ) ;
#5442 =( NAMED_UNIT ( * ) PLANE_ANGLE_UNIT ( ) SI_UNIT ( $, .RADIAN. ) );
#5444 = CARTESIAN_POINT ( 'NONE',  ( 1.472469842513823179, 30.59226448433411960, -4.923371831947296329 ) ) ;
#5445 = CARTESIAN_POINT ( 'NONE',  ( 19.42250999205614548, 15.98035201082150714, -5.440088680355545492 ) ) ;
#5446 = CARTESIAN_POINT ( 'NONE',  ( 0.5774900079438607392, 3.480352010821504916, 5.440088680355550821 ) ) ;
#5447 = ORIENTED_EDGE ( 'NONE', *, *, #15921, .F. ) ;
#5448 = CARTESIAN_POINT ( 'NONE',  ( 19.42250999205614548, 30.98035201082150536, -5.440088680355545492 ) ) ;
#5449 = CARTESIAN_POINT ( 'NONE',  ( -0.8801773607111009756, 38.06368534415484106, 1.068504757029289695E-15 ) ) ;
#5450 = CARTESIAN_POINT ( 'NONE',  ( 5.991992585808628036, 4.207234274712436881E-16, -13.20401548210295140 ) ) ;
#5451 = ORIENTED_EDGE ( 'NONE', *, *, #51194, .F. ) ;
#5452 = CARTESIAN_POINT ( 'NONE',  ( 0.1532563361054082862, 51.21726448433412315, 2.638427012816831674 ) ) ;
#5454 = ADVANCED_FACE ( 'NONE', ( #61689 ), #60712, .T. ) ;
#5453 = CARTESIAN_POINT ( 'NONE',  ( -0.8801773607110991993, 37.85535201082151247, -2.915334737309923874 ) ) ;
#5455 =( LENGTH_UNIT ( ) NAMED_UNIT ( * ) SI_UNIT ( .MILLI., .METRE. ) );
#5456 = CARTESIAN_POINT ( 'NONE',  ( 14.82269085861167035, 0.5000000000000004441, 2.299529454047060550 ) ) ;
#5457 = CARTESIAN_POINT ( 'NONE',  ( 10.00000000000000178, 65.37363466993042493, 12.81628187352647608 ) ) ;
#5458 = DIRECTION ( 'NONE',  ( -0.000000000000000000, 1.000000000000000000, -0.000000000000000000 ) ) ;
#5459 = CARTESIAN_POINT ( 'NONE',  ( 6.204703633549690345, 37.84541550158063927, 14.16423886937410082 ) ) ;
#5460 = CARTESIAN_POINT ( 'NONE',  ( 19.42250999205614193, 55.14701867748817676, 5.440088680355555262 ) ) ;
#5461 = FACE_OUTER_BOUND ( 'NONE', #89791, .T. ) ;
#5462 = EDGE_CURVE ( 'NONE', #49611, #11195, #38233, .T. ) ;
#5463 = DIRECTION ( 'NONE',  ( 0.000000000000000000, 1.000000000000000000, 0.000000000000000000 ) ) ;
#5464 = CARTESIAN_POINT ( 'NONE',  ( 12.63842701281683922, 44.55059781766745175, -9.846743663894590881 ) ) ;
#5465 = EDGE_LOOP ( 'NONE', ( #41750, #43109, #52802, #25495 ) ) ;
#5466 = DIRECTION ( 'NONE',  ( -0.1650476058606810681, 0.000000000000000000, 0.9862856015372308827 ) ) ;
#5467 = CARTESIAN_POINT ( 'NONE',  ( 0.1532563361054083140, 16.00893115100078390, 1.131784320476157264E-15 ) ) ;
#5468 = CARTESIAN_POINT ( 'NONE',  ( -3.434112377981067610, -11.91803199673624292, -12.81628187352647252 ) ) ;
#5469 = CARTESIAN_POINT ( 'NONE',  ( 2.035157376598822676, 27.43868534415483396, -7.964842623401177768 ) ) ;
#5470 = CARTESIAN_POINT ( 'NONE',  ( 12.63842701281683034, 27.46726448433411250, 9.846743663894596210 ) ) ;
#5471 = CARTESIAN_POINT ( 'NONE',  ( 21.09922568453594849, 6.206968003263753531, 6.408140936763242479 ) ) ;
#5472 = CARTESIAN_POINT ( 'NONE',  ( 0.5774900079438607392, 53.48035201082151247, 5.440088680355550821 ) ) ;
#5474 = CARTESIAN_POINT ( 'NONE',  ( -2.816281873526473856, 59.12363466993042493, 9.499525473075851096E-16 ) ) ;
#5473 = CARTESIAN_POINT ( 'NONE',  ( 4.559911319644449179, 32.23035201082150536, -9.422509992056141925 ) ) ;
#5475 = CARTESIAN_POINT ( 'NONE',  ( 20.36894250292379382, 43.67874883491397497, 10.36894250292379205 ) ) ;
#5476 = CARTESIAN_POINT ( 'NONE',  ( 21.92686044187657046, 35.16212336850780673, 4.562052436263912550E-16 ) ) ;
#5477 = ORIENTED_EDGE ( 'NONE', *, *, #33964, .F. ) ;
#5478 = CARTESIAN_POINT ( 'NONE',  ( 1.472469842513823179, 66.42559781766745175, 4.923371831947296329 ) ) ;
#5479 = CARTESIAN_POINT ( 'NONE',  ( 0.5774900079438590739, 12.64701867748817143, -5.440088680355550821 ) ) ;
#5480 = CARTESIAN_POINT ( 'NONE',  ( 19.42250999205614548, 50.98035201082151247, -5.440088680355545492 ) ) ;
#5481 = CARTESIAN_POINT ( 'NONE',  ( 1.472469842513823179, 61.42559781766745175, 4.923371831947296329 ) ) ;
#5482 = AXIS2_PLACEMENT_3D ( 'NONE', #73120, #20635, #81616 ) ;
#5484 = ORIENTED_EDGE ( 'NONE', *, *, #27324, .F. ) ;
#5483 = EDGE_CURVE ( 'NONE', #35669, #12094, #7472, .T. ) ;
#5486 = DIRECTION ( 'NONE',  ( -0.000000000000000000, 0.000000000000000000, 1.000000000000000000 ) ) ;
#5485 = CARTESIAN_POINT ( 'NONE',  ( 19.84674366389459621, 18.50893115100078745, 7.409399052514197653E-17 ) ) ;
#5487 = CARTESIAN_POINT ( 'NONE',  ( 4.559911319644449179, 62.23035201082150536, -9.422509992056141925 ) ) ;
#5488 = CARTESIAN_POINT ( 'NONE',  ( 14.92337183194729633, 42.67559781766745886, 8.527530157486181039 ) ) ;
#5489 = CARTESIAN_POINT ( 'NONE',  ( 5.076628168052704559, 15.17559781766745175, -8.527530157486179263 ) ) ;
#5490 = CARTESIAN_POINT ( 'NONE',  ( 5.076628168052704559, 15.17559781766745175, -8.527530157486179263 ) ) ;
#5491 = CARTESIAN_POINT ( 'NONE',  ( 19.50000000000000711, 79.40087001978915282, 4.500000000000000888 ) ) ;
#5493 = CARTESIAN_POINT ( 'NONE',  ( 6.879999999999995453, 43.00000000000000000, -6.500000000000000888 ) ) ;
#5492 = CARTESIAN_POINT ( 'NONE',  ( 4.559911319644449179, 67.23035201082150536, -9.422509992056141925 ) ) ;
#5494 = CARTESIAN_POINT ( 'NONE',  ( 10.00000000000000178, 7.258931151000785675, 9.846743663894594434 ) ) ;
#5496 = VERTEX_POINT ( 'NONE', #252 ) ;
#5495 = CARTESIAN_POINT ( 'NONE',  ( 0.1532563361054100626, 30.80059781766744820, -2.638427012816831230 ) ) ;
#5497 = DIRECTION ( 'NONE',  ( -0.5905099943842175847, -0.8070303256584298035, 0.000000000000000000 ) ) ;
#5498 = CARTESIAN_POINT ( 'NONE',  ( 3.591859063236763294, 3.290301336597087012, -11.09922568453595026 ) ) ;
#5499 = CARTESIAN_POINT ( 'NONE',  ( -4.164238869374099039, 21.80374883491396787, 8.674139862899312516E-16 ) ) ;
#5500 = PRODUCT_DEFINITION_CONTEXT ( 'detailed design', #67892, 'design' ) ;
#5501 = DIRECTION ( 'NONE',  ( 0.000000000000000000, 1.000000000000000000, 0.000000000000000000 ) ) ;
#5502 = CARTESIAN_POINT ( 'NONE',  ( 20.36894250292379738, 19.92874883491396787, -10.36894250292379027 ) ) ;
#5503 = CARTESIAN_POINT ( 'NONE',  ( -0.3689425029237898834, 41.17874883491397497, -10.36894250292378850 ) ) ;
#5505 = CARTESIAN_POINT ( 'NONE',  ( -0.8801773607111008646, 68.27201867748817676, 2.915334737309923430 ) ) ;
#5504 = CARTESIAN_POINT ( 'NONE',  ( 24.16423886937410614, 19.51208216824729647, -3.795296366450302550 ) ) ;
#5506 = CARTESIAN_POINT ( 'NONE',  ( 15.44008868035555793, 36.39701867748816966, -9.422509992056140149 ) ) ;
#5507 = ORIENTED_EDGE ( 'NONE', *, *, #65382, .T. ) ;
#5508 = CARTESIAN_POINT ( 'NONE',  ( 19.84674366389459621, 33.50893115100078745, 7.409399052514197653E-17 ) ) ;
#5510 = CARTESIAN_POINT ( 'NONE',  ( 17.20831665107776587, 22.88393115100078745, 7.208316651077764980 ) ) ;
#5509 = CARTESIAN_POINT ( 'NONE',  ( 0.2751277870542967463, 70.00000000000000000, -6.500000000000000888 ) ) ;
#5511 = CARTESIAN_POINT ( 'NONE',  ( 15.44008868035555793, 11.39701867748817143, -9.422509992056140149 ) ) ;
#5512 = CARTESIAN_POINT ( 'NONE',  ( 19.38216949554541557, 57.24863466993042493, -9.382169495545420901 ) ) ;
#5513 = CARTESIAN_POINT ( 'NONE',  ( 17.20831665107776587, 44.13393115100078745, -7.208316651077762316 ) ) ;
#5514 = AXIS2_PLACEMENT_3D ( 'NONE', #1767, #78227, #10237 ) ;
#5515 = DIRECTION ( 'NONE',  ( 0.000000000000000000, 1.000000000000000000, 0.000000000000000000 ) ) ;
#5516 = CARTESIAN_POINT ( 'NONE',  ( -1.099225684535947600, 44.54030133659708923, 6.408140936763237150 ) ) ;
#5517 = CARTESIAN_POINT ( 'NONE',  ( -14.16423886937410437, -23.40458449841936428, -3.795296366450299885 ) ) ;
#5518 = CARTESIAN_POINT ( 'NONE',  ( 10.00000000000000178, 49.31368534415484106, 10.88017736071110342 ) ) ;
#5519 = CARTESIAN_POINT ( 'NONE',  ( 0.1532563361054100626, 45.80059781766745886, -2.638427012816831230 ) ) ;
#5520 = CARTESIAN_POINT ( 'NONE',  ( 17.08211943468705840, 20.13708216824730357, -12.26659068614894466 ) ) ;
#5521 = ORIENTED_EDGE ( 'NONE', *, *, #52221, .F. ) ;
#5522 = CARTESIAN_POINT ( 'NONE',  ( 17.96484262340118221, 54.93868534415484106, 7.964842623401181321 ) ) ;
#5523 = CARTESIAN_POINT ( 'NONE',  ( 4.469999999999999751, 10.25000000000000000, -3.750000000000000000 ) ) ;
#5524 = CARTESIAN_POINT ( 'NONE',  ( -2.266590686148945544, 52.22041550158064638, 7.082119434687048631 ) ) ;
#5525 = CARTESIAN_POINT ( 'NONE',  ( 16.40814093676324603, 2.456968003263753531, -11.09922568453594671 ) ) ;
#5526 = CARTESIAN_POINT ( 'NONE',  ( 13.43411237798105340, 60.58196800326376064, 12.81628187352647963 ) ) ;
#5527 = CARTESIAN_POINT ( 'NONE',  ( 20.88017736071110164, 60.35535201082151957, 2.915334737309930979 ) ) ;
#5528 = CARTESIAN_POINT ( 'NONE',  ( -3.250000000000001776, 0.08822490956012368768, -2.500000000000000888 ) ) ;
#5529 = CARTESIAN_POINT ( 'NONE',  ( 10.00000000000000000, 27.87363466993042138, -12.81628187352647608 ) ) ;
#5530 = CARTESIAN_POINT ( 'NONE',  ( 22.81628187352647785, 1.623634669930420271, 6.195893100308588602E-16 ) ) ;
#5531 = CARTESIAN_POINT ( 'NONE',  ( -5.440088680355547268, 33.89701867748817676, 9.422509992056143702 ) ) ;
#5532 = CARTESIAN_POINT ( 'NONE',  ( -0.8801773607110991993, 17.85535201082150536, -2.915334737309923874 ) ) ;
#5533 = CARTESIAN_POINT ( 'NONE',  ( 10.00000000000000178, 9.313685344154839285, 10.88017736071110342 ) ) ;
#5534 = FILL_AREA_STYLE_COLOUR ( '', #4112 ) ;
#5535 = ORIENTED_EDGE ( 'NONE', *, *, #71276, .T. ) ;
#5536 = EDGE_CURVE ( 'NONE', #62370, #89076, #23235, .T. ) ;
#5537 = EDGE_CURVE ( 'NONE', #26466, #93630, #20565, .T. ) ;
#5538 = CARTESIAN_POINT ( 'NONE',  ( 19.42250999205614193, 10.14701867748816966, 5.440088680355555262 ) ) ;
#5539 = DIRECTION ( 'NONE',  ( -0.000000000000000000, -0.000000000000000000, 1.000000000000000000 ) ) ;
#5540 = CARTESIAN_POINT ( 'NONE',  ( 10.00000000000000178, 69.31368534415484817, 10.88017736071110342 ) ) ;
#5541 = CARTESIAN_POINT ( 'NONE',  ( 2.791683348922240793, 1.633931151000784565, 7.208316651077764092 ) ) ;
#5542 = STYLED_ITEM ( 'NONE', ( #14352 ), #54890 ) ;
#5543 = CARTESIAN_POINT ( 'NONE',  ( 14.92337183194729988, 39.34226448433412315, -8.527530157486177487 ) ) ;
#5544 = CARTESIAN_POINT ( 'NONE',  ( 15.44008868035555793, 31.39701867748817676, -9.422509992056140149 ) ) ;
#5545 = VECTOR ( 'NONE', #42897, 1000.000000000000000 ) ;
#5546 = CARTESIAN_POINT ( 'NONE',  ( 22.81628187352647785, 6.415301336597088344, 3.434112377981063169 ) ) ;
#5548 = CARTESIAN_POINT ( 'NONE',  ( 13.96552416078064063, 14.95037115134969241, 4.756200848675177006 ) ) ;
#5547 = CARTESIAN_POINT ( 'NONE',  ( 12.91533473730993009, 41.60535201082149825, -10.88017736071109987 ) ) ;
#5549 = CARTESIAN_POINT ( 'NONE',  ( 0.6178305044545818747, 38.49863466993042493, -9.382169495545419124 ) ) ;
#5550 = ORIENTED_EDGE ( 'NONE', *, *, #43101, .T. ) ;
#5551 = CARTESIAN_POINT ( 'NONE',  ( 17.96484262340118221, 61.18868534415482685, -7.964842623401177768 ) ) ;
#5552 = AXIS2_PLACEMENT_3D ( 'NONE', #33533, #26059, #46580 ) ;
#5554 = CARTESIAN_POINT ( 'NONE',  ( -2.266590686148945544, 7.220415501580634832, 7.082119434687048631 ) ) ;
#5553 = CARTESIAN_POINT ( 'NONE',  ( 0.6178305044545838731, 34.74863466993042493, 9.382169495545420901 ) ) ;
#5555 = CARTESIAN_POINT ( 'NONE',  ( 1.472469842513823179, 0.5922644843341181575, -4.923371831947296329 ) ) ;
#5556 = CARTESIAN_POINT ( 'NONE',  ( 10.00000000000000000, 41.81368534415484106, -10.88017736071110342 ) ) ;
#5557 = CARTESIAN_POINT ( 'NONE',  ( 0.000000000000000000, 0.5000000000000004441, 0.000000000000000000 ) ) ;
#5558 = CARTESIAN_POINT ( 'NONE',  ( 17.08211943468705840, 60.13708216824729647, -12.26659068614894466 ) ) ;
#5559 = CARTESIAN_POINT ( 'NONE',  ( 14.92337183194729633, 47.67559781766745175, 8.527530157486181039 ) ) ;
#5560 = CARTESIAN_POINT ( 'NONE',  ( 19.84674366389459266, 13.71726448433411782, -2.638427012816827677 ) ) ;
#5561 = CARTESIAN_POINT ( 'NONE',  ( 4.559911319644449179, 67.23035201082150536, -9.422509992056141925 ) ) ;
#5562 = CARTESIAN_POINT ( 'NONE',  ( 5.795997163830165277, -0.03417435944610275333, -13.01802277140705932 ) ) ;
#5563 = CARTESIAN_POINT ( 'NONE',  ( 2.917880565312948704, 27.63708216824730357, 12.26659068614894643 ) ) ;
#5564 = LINE ( 'NONE', #36040, #53827 ) ;
#5565 = CARTESIAN_POINT ( 'NONE',  ( -3.889970118670758037, -8.287734203605921834, -4.000000000000000888 ) ) ;
#5566 =( BOUNDED_SURFACE ( )  B_SPLINE_SURFACE ( 1, 2, ( 
 ( #7722, #83707, #53691, #38219, #90702, #68704, #84688, #84211, #30684, #61192, #15718, #46203, #8207, #44709, #38702, #37235, #69201, #46680, #92191, #6719, #23716, #60694, #67724, #60207, #83212, #14733, #7219, #37720, #68224, #30193, #11524, #80021, #86552, #71556, #42046, #4536, #27016, #12021, #18542, #19524, #18056, #10062, #57515, #72510, #26050, #27506, #72026, #26524, #4043, #48534, #94531, #49034, #41058, #88012, #42521, #56058, #2585, #79539, #78551, #17572, #41560, #56540, #19037, #3554, #79034, #34505, #65502, #34014, #11038, #10548, #64511, #96025, #48039, #3069, #33523, #64019, #63536, #50020, #87522, #94044, #95015, #34999, #64997, #86061, #87030, #57020, #80523, #49513, #95524, #40560, #73004, #71060, #33039, #25566, #5520, #29468, #58997, #12998, #90469, #35998, #14006, #44975, #14504, #6994, #58001, #89499, #73493, #44485, #21010, #51497, #66501, #22004, #81494, #97026, #5020, #28981, #37498, #52479, #20010, #59485, #28503, #50512, #13503, #75480, #43494, #67988, #74486, #81992, #81009, #89985, #43984, #12510, #6009, #98514, #73994, #88508, #36503, #66995, #97518, #82985, #21502, #58497, #51999, #82489, #74986, #43011, #6489, #96526, #67493, #36997, #89007, #98014, #35504, #65998, #59976, #27999, #50999, #20514, #54441, #980, #31442, #8948, #45470, #83969, #83479, #7981, #75972, #52967, #84951, #23967, #30459, #15494, #16461, #48781, #69955, #56304, #61452, #63771, #60959, #15000, #1474, #46941, #68974, #71787, #15966, #69460, #77435, #91468, #38480, #91960, #45976, #31928, #86797, #11, #7499, #23489, #22495, #60473, #84468, #506, #61943, #46458, #22993, #39465, #10797, #76952, #53961, #53459, #8462, #41315, #90962, #76466, #30953, #38968, #37992, #94281, #92444, #68484, #25802, #79288, #18298, #29967, #80271, #11771, #73745, #12260, #96277, #94776, #72269, #34252, #56778, #3797, #49759, #5276, #4284, #57265, #35753, #42280, #58235, #89250, #58746, #51250, #3296, #34758, #18794, #88755, #65248, #95775, #72751, #66240, #26770, #27255, #49277, #73251, #81736, #96775, #20265, #65747, #87273, #57755, #4778, #64264, #20760, #11276, #26276, #33760, #28252, #79777, #41796, #35251, #42769, #50764, #64753, #95265, #87760, #88258, #13252, #43743, #19275, #19764, #50249, #80765, #27751, #81253, #43250, #12752, #15741, #82734, #29724, #45730, #67245, #38239, #91215, #257, #68730, #5763, #76231, #13751, #68247, #89736, #23242, #59733, #44235, #14252, #59234, #91721, #44734, #7745, #21254, #22743, #52727, #30706, #97770, #66748, #61218, #53226, #37260, #83232, #53714, #74738, #74230, #75230, #97272, #36252, #6743 ),
 ( #84234, #90725, #67748, #98267, #28744, #22250, #6251, #7244, #98765, #30215, #51752, #60230, #36755, #83729, #14757, #29235, #15252, #82236, #90229, #37749, #21760, #52241, #45230, #60719, #75728, #47690, #25212, #61694, #1238, #748, #24218, #92210, #69223, #70698, #40191, #46701, #31693, #2218, #63659, #86190, #71188, #77687, #78684, #77200, #31201, #17701, #32676, #85206, #86678, #17213, #63170, #46224, #55692, #76710, #55178, #2713, #32178, #33165, #9202, #62184, #24707, #93677, #16216, #62681, #16710, #92694, #54684, #85693, #47183, #48171, #25695, #69708, #39714, #84715, #10194, #70203, #8705, #78183, #40687, #1724, #93181, #56185, #94165, #9696, #39223, #8229, #38723, #23737, #54199, #19651, #79165, #73626, #26172, #10678, #18184, #81133, #48663, #94663, #88138, #27139, #35131, #56664, #79666, #11162, #72635, #20140, #5149, #3679, #87646, #42172, #34636, #35639, #41194, #58123, #66125, #58633, #26653, #4167, #88631, #41682, #12636, #65630, #43134, #96654, #71674, #50644, #87152, #12146, #33650, #28133, #34141, #18677, #57149, #3184, #64146, #19160, #49163, #72151, #96155, #95655, #64633, #95143, #49639, #80147, #27638, #11658, #57643, #65134, #50143, #80652, #42651, #73128, #4670, #59616, #21137, #30097, #43628, #66633, #83112, #52611, #7634, #28629, #60604, #6622, #44109, #51132, #75115, #82618, #14642, #52124, #97161, #37135, #38125, #45104, #21638, #14134, #44619, #51638, #91099, #74114, #59116, #75611, #7122, #68613, #89626, #22627, #67630, #74621, #81623, #98140, #29601, #37626, #60102, #82118, #90603, #142, #68122, #22129, #98648, #53105, #83615, #15130, #30591, #45606, #20643, #76104, #89133, #13131, #5648, #36124, #6135, #13628, #36640, #67123, #97650, #90113, #29113, #39104, #1612, #8596, #63063, #40579, #84601, #77085, #638, #85582, #62071, #61582, #32061, #9579, #24102, #54572, #71075, #17589, #24599, #31087, #17096, #55064, #46109, #85087, #62565, #23123, #48054, #69105, #53594, #61096, #25096, #91606, #38606, #93068, #70088, #78074, #92093, #23621, #54086, #16595, #93562, #78569, #46588, #31577, #47073, #77570, #10078, #84108, #2107, #2600, #15624, #69594, #9086, #32565, #16100, #55579, #40079, #86077, #76593, #8111, #1115, #92579, #47578, #39600, #70581, #18560, #71569, #72043, #18070, #50526, #41575, #65516, #48550, #50034, #11542, #96038, #26064, #25581, #35015, #12035, #95032, #42061, #20025, #3081, #73510, #3573, #56073, #33054, #34030, #63550, #72524, #88523, #19051, #58013, #26541, #49052, #4058, #80537, #33539, #49529, #64526, #79555, #11055, #34519, #57037, #27522, #12525, #56555, #87539 ) ),
 .UNSPECIFIED., .F., .F., .F. ) 
 B_SPLINE_SURFACE_WITH_KNOTS ( ( 2, 2 ),
 ( 3, 2, 2, 2, 2, 2, 2, 2, 2, 2, 2, 2, 2, 2, 2, 2, 2, 2, 2, 2, 2, 2, 2, 2, 2, 2, 2, 2, 2, 2, 2, 2, 2, 2, 2, 2, 2, 2, 2, 2, 2, 2, 2, 2, 2, 2, 2, 2, 2, 2, 2, 2, 2, 2, 2, 2, 2, 2, 2, 2, 2, 2, 2, 2, 2, 2, 2, 2, 2, 2, 2, 2, 2, 2, 2, 2, 2, 2, 2, 2, 2, 2, 2, 2, 2, 2, 2, 2, 2, 2, 2, 2, 2, 2, 2, 2, 2, 2, 2, 2, 2, 2, 2, 2, 2, 2, 2, 2, 2, 2, 2, 2, 2, 2, 2, 2, 2, 2, 2, 2, 2, 2, 2, 2, 2, 2, 2, 2, 2, 2, 2, 2, 2, 2, 2, 2, 2, 2, 2, 2, 2, 2, 2, 2, 2, 2, 2, 2, 2, 2, 2, 2, 2, 2, 2, 2, 2, 2, 2, 2, 2, 2, 3 ),
 ( 0.000000000000000000, 1.000000000000000000 ),
 ( 0.000000000000000000, 0.005952380952380952051, 0.01190476190476190410, 0.01785714285714285615, 0.02380952380952380820, 0.02976190476190476025, 0.03571428571428571230, 0.04166666666666666435, 0.04761904761904761640, 0.05357142857142856845, 0.05952380952380952051, 0.06547619047619047949, 0.07142857142857142461, 0.07738095238095238360, 0.08333333333333332871, 0.08928571428571428770, 0.09523809523809523281, 0.1011904761904761918, 0.1071428571428571369, 0.1130952380952380959, 0.1190476190476190410, 0.1250000000000000000, 0.1309523809523809590, 0.1369047619047619180, 0.1428571428571428492, 0.1488095238095238082, 0.1547619047619047672, 0.1607142857142857262, 0.1666666666666666574, 0.1726190476190476164, 0.1785714285714285754, 0.1845238095238095344, 0.1904761904761904656, 0.1964285714285714246, 0.2023809523809523836, 0.2083333333333333426, 0.2142857142857142738, 0.2202380952380952328, 0.2261904761904761918, 0.2321428571428571508, 0.2380952380952380820, 0.2440476190476190410, 0.2500000000000000000, 0.2559523809523809312, 0.2619047619047619180, 0.2678571428571428492, 0.2738095238095238360, 0.2797619047619047672, 0.2857142857142856984, 0.2916666666666666852, 0.2976190476190476164, 0.3035714285714285476, 0.3095238095238095344, 0.3154761904761904656, 0.3214285714285714524, 0.3273809523809523836, 0.3333333333333333148, 0.3392857142857143016, 0.3452380952380952328, 0.3511904761904761640, 0.3571428571428571508, 0.3630952380952380820, 0.3690476190476190688, 0.3750000000000000000, 0.3809523809523809312, 0.3869047619047619180, 0.3928571428571428492, 0.3988095238095238360, 0.4047619047619047672, 0.4107142857142856984, 0.4166666666666666852, 0.4226190476190476164, 0.4285714285714285476, 0.4345238095238095344, 0.4404761904761904656, 0.4464285714285714524, 0.4523809523809523836, 0.4583333333333333148, 0.4642857142857143016, 0.4702380952380952328, 0.4761904761904761640, 0.4821428571428571508, 0.4880952380952380820, 0.4940476190476190688, 0.5000000000000000000, 0.5059523809523809312, 0.5119047619047618625, 0.5178571428571429047, 0.5238095238095238360, 0.5297619047619047672, 0.5357142857142856984, 0.5416666666666666297, 0.5476190476190476719, 0.5535714285714286031, 0.5595238095238095344, 0.5654761904761904656, 0.5714285714285713969, 0.5773809523809523281, 0.5833333333333333703, 0.5892857142857143016, 0.5952380952380952328, 0.6011904761904761640, 0.6071428571428570953, 0.6130952380952381375, 0.6190476190476190688, 0.6250000000000000000, 0.6309523809523809312, 0.6369047619047618625, 0.6428571428571429047, 0.6488095238095238360, 0.6547619047619047672, 0.6607142857142856984, 0.6666666666666666297, 0.6726190476190476719, 0.6785714285714286031, 0.6845238095238095344, 0.6904761904761904656, 0.6964285714285713969, 0.7023809523809523281, 0.7083333333333333703, 0.7142857142857143016, 0.7202380952380952328, 0.7261904761904761640, 0.7321428571428570953, 0.7380952380952381375, 0.7440476190476190688, 0.7500000000000000000, 0.7559523809523809312, 0.7619047619047618625, 0.7678571428571429047, 0.7738095238095238360, 0.7797619047619047672, 0.7857142857142856984, 0.7916666666666666297, 0.7976190476190476719, 0.8035714285714286031, 0.8095238095238095344, 0.8154761904761904656, 0.8214285714285713969, 0.8273809523809523281, 0.8333333333333333703, 0.8392857142857143016, 0.8452380952380952328, 0.8511904761904761640, 0.8571428571428570953, 0.8630952380952381375, 0.8690476190476190688, 0.8750000000000000000, 0.8809523809523809312, 0.8869047619047618625, 0.8928571428571429047, 0.8988095238095238360, 0.9047619047619047672, 0.9107142857142856984, 0.9166666666666666297, 0.9226190476190476719, 0.9285714285714286031, 0.9345238095238095344, 0.9404761904761904656, 0.9464285714285713969, 0.9523809523809523281, 0.9583333333333333703, 0.9642857142857143016 ),
 .UNSPECIFIED. ) 
 GEOMETRIC_REPRESENTATION_ITEM ( )  RATIONAL_B_SPLINE_SURFACE ( (
 ( 1.000000000000000000, 0.9659258262890683122, 1.000000000000000000, 0.9659258262890683122, 1.000000000000000000, 0.9659258262890683122, 1.000000000000000000, 0.9659258262890683122, 1.000000000000000000, 0.9659258262890683122, 1.000000000000000000, 0.9659258262890683122, 1.000000000000000000, 0.9659258262890683122, 1.000000000000000000, 0.9659258262890683122, 1.000000000000000000, 0.9659258262890683122, 1.000000000000000000, 0.9659258262890683122, 1.000000000000000000, 0.9659258262890683122, 1.000000000000000000, 0.9659258262890683122, 1.000000000000000000, 0.9659258262890683122, 1.000000000000000000, 0.9659258262890683122, 1.000000000000000000, 0.9659258262890683122, 1.000000000000000000, 0.9659258262890683122, 1.000000000000000000, 0.9659258262890683122, 1.000000000000000000, 0.9659258262890683122, 1.000000000000000000, 0.9659258262890683122, 1.000000000000000000, 0.9659258262890683122, 1.000000000000000000, 0.9659258262890683122, 1.000000000000000000, 0.9659258262890683122, 1.000000000000000000, 0.9659258262890683122, 1.000000000000000000, 0.9659258262890683122, 1.000000000000000000, 0.9659258262890683122, 1.000000000000000000, 0.9659258262890683122, 1.000000000000000000, 0.9659258262890683122, 1.000000000000000000, 0.9659258262890683122, 1.000000000000000000, 0.9659258262890683122, 1.000000000000000000, 0.9659258262890683122, 1.000000000000000000, 0.9659258262890683122, 1.000000000000000000, 0.9659258262890683122, 1.000000000000000000, 0.9659258262890683122, 1.000000000000000000, 0.9659258262890683122, 1.000000000000000000, 0.9659258262890683122, 1.000000000000000000, 0.9659258262890683122, 1.000000000000000000, 0.9659258262890683122, 1.000000000000000000, 0.9659258262890683122, 1.000000000000000000, 0.9659258262890683122, 1.000000000000000000, 0.9659258262890683122, 1.000000000000000000, 0.9659258262890683122, 1.000000000000000000, 0.9659258262890683122, 1.000000000000000000, 0.9659258262890683122, 1.000000000000000000, 0.9659258262890683122, 1.000000000000000000, 0.9659258262890683122, 1.000000000000000000, 0.9659258262890683122, 1.000000000000000000, 0.9659258262890683122, 1.000000000000000000, 0.9659258262890683122, 1.000000000000000000, 0.9659258262890683122, 1.000000000000000000, 0.9659258262890683122, 1.000000000000000000, 0.9659258262890683122, 1.000000000000000000, 0.9659258262890683122, 1.000000000000000000, 0.9659258262890683122, 1.000000000000000000, 0.9659258262890683122, 1.000000000000000000, 0.9659258262890683122, 1.000000000000000000, 0.9659258262890683122, 1.000000000000000000, 0.9659258262890683122, 1.000000000000000000, 0.9659258262890683122, 1.000000000000000000, 0.9659258262890683122, 1.000000000000000000, 0.9659258262890683122, 1.000000000000000000, 0.9659258262890683122, 1.000000000000000000, 0.9659258262890683122, 1.000000000000000000, 0.9659258262890683122, 1.000000000000000000, 0.9659258262890683122, 1.000000000000000000, 0.9659258262890683122, 1.000000000000000000, 0.9659258262890683122, 1.000000000000000000, 0.9659258262890683122, 1.000000000000000000, 0.9659258262890683122, 1.000000000000000000, 0.9659258262890683122, 1.000000000000000000, 0.9659258262890683122, 1.000000000000000000, 0.9659258262890683122, 1.000000000000000000, 0.9659258262890683122, 1.000000000000000000, 0.9659258262890683122, 1.000000000000000000, 0.9659258262890683122, 1.000000000000000000, 0.9659258262890683122, 1.000000000000000000, 0.9659258262890683122, 1.000000000000000000, 0.9659258262890683122, 1.000000000000000000, 0.9659258262890683122, 1.000000000000000000, 0.9659258262890683122, 1.000000000000000000, 0.9659258262890683122, 1.000000000000000000, 0.9659258262890683122, 1.000000000000000000, 0.9659258262890683122, 1.000000000000000000, 0.9659258262890683122, 1.000000000000000000, 0.9659258262890683122, 1.000000000000000000, 0.9659258262890683122, 1.000000000000000000, 0.9659258262890683122, 1.000000000000000000, 0.9659258262890683122, 1.000000000000000000, 0.9659258262890683122, 1.000000000000000000, 0.9659258262890683122, 1.000000000000000000, 0.9659258262890683122, 1.000000000000000000, 0.9659258262890683122, 1.000000000000000000, 0.9659258262890683122, 1.000000000000000000, 0.9659258262890683122, 1.000000000000000000, 0.9659258262890683122, 1.000000000000000000, 0.9659258262890683122, 1.000000000000000000, 0.9659258262890683122, 1.000000000000000000, 0.9659258262890683122, 1.000000000000000000, 0.9659258262890683122, 1.000000000000000000, 0.9659258262890683122, 1.000000000000000000, 0.9659258262890683122, 1.000000000000000000, 0.9659258262890683122, 1.000000000000000000, 0.9659258262890683122, 1.000000000000000000, 0.9659258262890683122, 1.000000000000000000, 0.9659258262890683122, 1.000000000000000000, 0.9659258262890683122, 1.000000000000000000, 0.9659258262890683122, 1.000000000000000000, 0.9659258262890683122, 1.000000000000000000, 0.9659258262890683122, 1.000000000000000000, 0.9659258262890683122, 1.000000000000000000, 0.9659258262890683122, 1.000000000000000000, 0.9659258262890683122, 1.000000000000000000, 0.9659258262890683122, 1.000000000000000000, 0.9659258262890683122, 1.000000000000000000, 0.9659258262890683122, 1.000000000000000000, 0.9659258262890683122, 1.000000000000000000, 0.9659258262890683122, 1.000000000000000000, 0.9659258262890683122, 1.000000000000000000, 0.9659258262890683122, 1.000000000000000000, 0.9659258262890683122, 1.000000000000000000, 0.9659258262890683122, 1.000000000000000000, 0.9659258262890683122, 1.000000000000000000, 0.9659258262890683122, 1.000000000000000000, 0.9659258262890683122, 1.000000000000000000, 0.9659258262890683122, 1.000000000000000000, 0.9659258262890683122, 1.000000000000000000, 0.9659258262890683122, 1.000000000000000000, 0.9659258262890683122, 1.000000000000000000, 0.9659258262890683122, 1.000000000000000000, 0.9659258262890683122, 1.000000000000000000, 0.9659258262890683122, 1.000000000000000000, 0.9659258262890683122, 1.000000000000000000, 0.9659258262890683122, 1.000000000000000000, 0.9659258262890683122, 1.000000000000000000, 0.9659258262890683122, 1.000000000000000000, 0.9659258262890683122, 1.000000000000000000, 0.9659258262890683122, 1.000000000000000000, 0.9659258262890683122, 1.000000000000000000, 0.9659258262890683122, 1.000000000000000000, 0.9659258262890683122, 1.000000000000000000, 0.9659258262890683122, 1.000000000000000000, 0.9659258262890683122, 1.000000000000000000, 0.9659258262890683122, 1.000000000000000000, 0.9659258262890683122, 1.000000000000000000, 0.9659258262890683122, 1.000000000000000000, 0.9659258262890683122, 1.000000000000000000, 0.9659258262890683122, 1.000000000000000000, 0.9659258262890683122, 1.000000000000000000, 0.9659258262890683122, 1.000000000000000000, 0.9659258262890683122, 1.000000000000000000, 0.9659258262890683122, 1.000000000000000000, 0.9659258262890683122, 1.000000000000000000, 0.9659258262890683122, 1.000000000000000000, 0.9659258262890683122, 1.000000000000000000, 0.9659258262890683122, 1.000000000000000000, 0.9659258262890683122, 1.000000000000000000, 0.9659258262890683122, 1.000000000000000000, 0.9659258262890683122, 1.000000000000000000, 0.9659258262890683122, 1.000000000000000000, 0.9659258262890683122, 1.000000000000000000, 0.9659258262890683122, 1.000000000000000000, 0.9659258262890683122, 1.000000000000000000, 0.9659258262890683122, 1.000000000000000000),
 ( 1.000000000000000000, 0.9659258262890683122, 1.000000000000000000, 0.9659258262890683122, 1.000000000000000000, 0.9659258262890683122, 1.000000000000000000, 0.9659258262890683122, 1.000000000000000000, 0.9659258262890683122, 1.000000000000000000, 0.9659258262890683122, 1.000000000000000000, 0.9659258262890683122, 1.000000000000000000, 0.9659258262890683122, 1.000000000000000000, 0.9659258262890683122, 1.000000000000000000, 0.9659258262890683122, 1.000000000000000000, 0.9659258262890683122, 1.000000000000000000, 0.9659258262890683122, 1.000000000000000000, 0.9659258262890683122, 1.000000000000000000, 0.9659258262890683122, 1.000000000000000000, 0.9659258262890683122, 1.000000000000000000, 0.9659258262890683122, 1.000000000000000000, 0.9659258262890683122, 1.000000000000000000, 0.9659258262890683122, 1.000000000000000000, 0.9659258262890683122, 1.000000000000000000, 0.9659258262890683122, 1.000000000000000000, 0.9659258262890683122, 1.000000000000000000, 0.9659258262890683122, 1.000000000000000000, 0.9659258262890683122, 1.000000000000000000, 0.9659258262890683122, 1.000000000000000000, 0.9659258262890683122, 1.000000000000000000, 0.9659258262890683122, 1.000000000000000000, 0.9659258262890683122, 1.000000000000000000, 0.9659258262890683122, 1.000000000000000000, 0.9659258262890683122, 1.000000000000000000, 0.9659258262890683122, 1.000000000000000000, 0.9659258262890683122, 1.000000000000000000, 0.9659258262890683122, 1.000000000000000000, 0.9659258262890683122, 1.000000000000000000, 0.9659258262890683122, 1.000000000000000000, 0.9659258262890683122, 1.000000000000000000, 0.9659258262890683122, 1.000000000000000000, 0.9659258262890683122, 1.000000000000000000, 0.9659258262890683122, 1.000000000000000000, 0.9659258262890683122, 1.000000000000000000, 0.9659258262890683122, 1.000000000000000000, 0.9659258262890683122, 1.000000000000000000, 0.9659258262890683122, 1.000000000000000000, 0.9659258262890683122, 1.000000000000000000, 0.9659258262890683122, 1.000000000000000000, 0.9659258262890683122, 1.000000000000000000, 0.9659258262890683122, 1.000000000000000000, 0.9659258262890683122, 1.000000000000000000, 0.9659258262890683122, 1.000000000000000000, 0.9659258262890683122, 1.000000000000000000, 0.9659258262890683122, 1.000000000000000000, 0.9659258262890683122, 1.000000000000000000, 0.9659258262890683122, 1.000000000000000000, 0.9659258262890683122, 1.000000000000000000, 0.9659258262890683122, 1.000000000000000000, 0.9659258262890683122, 1.000000000000000000, 0.9659258262890683122, 1.000000000000000000, 0.9659258262890683122, 1.000000000000000000, 0.9659258262890683122, 1.000000000000000000, 0.9659258262890683122, 1.000000000000000000, 0.9659258262890683122, 1.000000000000000000, 0.9659258262890683122, 1.000000000000000000, 0.9659258262890683122, 1.000000000000000000, 0.9659258262890683122, 1.000000000000000000, 0.9659258262890683122, 1.000000000000000000, 0.9659258262890683122, 1.000000000000000000, 0.9659258262890683122, 1.000000000000000000, 0.9659258262890683122, 1.000000000000000000, 0.9659258262890683122, 1.000000000000000000, 0.9659258262890683122, 1.000000000000000000, 0.9659258262890683122, 1.000000000000000000, 0.9659258262890683122, 1.000000000000000000, 0.9659258262890683122, 1.000000000000000000, 0.9659258262890683122, 1.000000000000000000, 0.9659258262890683122, 1.000000000000000000, 0.9659258262890683122, 1.000000000000000000, 0.9659258262890683122, 1.000000000000000000, 0.9659258262890683122, 1.000000000000000000, 0.9659258262890683122, 1.000000000000000000, 0.9659258262890683122, 1.000000000000000000, 0.9659258262890683122, 1.000000000000000000, 0.9659258262890683122, 1.000000000000000000, 0.9659258262890683122, 1.000000000000000000, 0.9659258262890683122, 1.000000000000000000, 0.9659258262890683122, 1.000000000000000000, 0.9659258262890683122, 1.000000000000000000, 0.9659258262890683122, 1.000000000000000000, 0.9659258262890683122, 1.000000000000000000, 0.9659258262890683122, 1.000000000000000000, 0.9659258262890683122, 1.000000000000000000, 0.9659258262890683122, 1.000000000000000000, 0.9659258262890683122, 1.000000000000000000, 0.9659258262890683122, 1.000000000000000000, 0.9659258262890683122, 1.000000000000000000, 0.9659258262890683122, 1.000000000000000000, 0.9659258262890683122, 1.000000000000000000, 0.9659258262890683122, 1.000000000000000000, 0.9659258262890683122, 1.000000000000000000, 0.9659258262890683122, 1.000000000000000000, 0.9659258262890683122, 1.000000000000000000, 0.9659258262890683122, 1.000000000000000000, 0.9659258262890683122, 1.000000000000000000, 0.9659258262890683122, 1.000000000000000000, 0.9659258262890683122, 1.000000000000000000, 0.9659258262890683122, 1.000000000000000000, 0.9659258262890683122, 1.000000000000000000, 0.9659258262890683122, 1.000000000000000000, 0.9659258262890683122, 1.000000000000000000, 0.9659258262890683122, 1.000000000000000000, 0.9659258262890683122, 1.000000000000000000, 0.9659258262890683122, 1.000000000000000000, 0.9659258262890683122, 1.000000000000000000, 0.9659258262890683122, 1.000000000000000000, 0.9659258262890683122, 1.000000000000000000, 0.9659258262890683122, 1.000000000000000000, 0.9659258262890683122, 1.000000000000000000, 0.9659258262890683122, 1.000000000000000000, 0.9659258262890683122, 1.000000000000000000, 0.9659258262890683122, 1.000000000000000000, 0.9659258262890683122, 1.000000000000000000, 0.9659258262890683122, 1.000000000000000000, 0.9659258262890683122, 1.000000000000000000, 0.9659258262890683122, 1.000000000000000000, 0.9659258262890683122, 1.000000000000000000, 0.9659258262890683122, 1.000000000000000000, 0.9659258262890683122, 1.000000000000000000, 0.9659258262890683122, 1.000000000000000000, 0.9659258262890683122, 1.000000000000000000, 0.9659258262890683122, 1.000000000000000000, 0.9659258262890683122, 1.000000000000000000, 0.9659258262890683122, 1.000000000000000000, 0.9659258262890683122, 1.000000000000000000, 0.9659258262890683122, 1.000000000000000000, 0.9659258262890683122, 1.000000000000000000, 0.9659258262890683122, 1.000000000000000000, 0.9659258262890683122, 1.000000000000000000, 0.9659258262890683122, 1.000000000000000000, 0.9659258262890683122, 1.000000000000000000, 0.9659258262890683122, 1.000000000000000000, 0.9659258262890683122, 1.000000000000000000, 0.9659258262890683122, 1.000000000000000000, 0.9659258262890683122, 1.000000000000000000, 0.9659258262890683122, 1.000000000000000000, 0.9659258262890683122, 1.000000000000000000, 0.9659258262890683122, 1.000000000000000000, 0.9659258262890683122, 1.000000000000000000, 0.9659258262890683122, 1.000000000000000000, 0.9659258262890683122, 1.000000000000000000, 0.9659258262890683122, 1.000000000000000000, 0.9659258262890683122, 1.000000000000000000, 0.9659258262890683122, 1.000000000000000000, 0.9659258262890683122, 1.000000000000000000, 0.9659258262890683122, 1.000000000000000000, 0.9659258262890683122, 1.000000000000000000, 0.9659258262890683122, 1.000000000000000000, 0.9659258262890683122, 1.000000000000000000, 0.9659258262890683122, 1.000000000000000000, 0.9659258262890683122, 1.000000000000000000, 0.9659258262890683122, 1.000000000000000000, 0.9659258262890683122, 1.000000000000000000, 0.9659258262890683122, 1.000000000000000000, 0.9659258262890683122, 1.000000000000000000, 0.9659258262890683122, 1.000000000000000000) ) ) 
 REPRESENTATION_ITEM ( '' )  SURFACE ( )  );
#5567 = ORIENTED_EDGE ( 'NONE', *, *, #85560, .F. ) ;
#5568 = ORIENTED_EDGE ( 'NONE', *, *, #25107, .T. ) ;
#5569 = CARTESIAN_POINT ( 'NONE',  ( -4.164238869374099039, 56.80374883491397497, 8.674139862899312516E-16 ) ) ;
#5571 = EDGE_CURVE ( 'NONE', #83513, #20604, #50436, .T. ) ;
#5570 = CARTESIAN_POINT ( 'NONE',  ( -0.8801773607111009756, 3.063685344154838397, 1.068504757029289695E-15 ) ) ;
#5572 = CARTESIAN_POINT ( 'NONE',  ( 14.92337183194729988, 29.34226448433411960, -8.527530157486177487 ) ) ;
#5573 = AXIS2_PLACEMENT_3D ( 'NONE', #5287, #6262, #36765 ) ;
#5574 = CARTESIAN_POINT ( 'NONE',  ( -2.816281873526473856, 29.12363466993041783, 9.499525473075851096E-16 ) ) ;
#5575 = DIRECTION ( 'NONE',  ( 0.000000000000000000, 1.000000000000000000, 0.000000000000000000 ) ) ;
#5576 = CARTESIAN_POINT ( 'NONE',  ( 17.74999999999999645, 78.80384757729336798, 4.000000000000000000 ) ) ;
#5577 = CARTESIAN_POINT ( 'NONE',  ( 20.88017736071110519, 15.56368534415483751, 2.639326808657452039E-16 ) ) ;
#5578 = CARTESIAN_POINT ( 'NONE',  ( -4.164238869374099927, 62.01208216824728936, 3.795296366450308767 ) ) ;
#5579 = CARTESIAN_POINT ( 'NONE',  ( 17.20831665107776587, 22.88393115100078745, 7.208316651077764980 ) ) ;
#5580 = EDGE_CURVE ( 'NONE', #36801, #21688, #34438, .T. ) ;
#5581 = CARTESIAN_POINT ( 'NONE',  ( -14.26139399674459263, 4.837279266207889341E-16, 2.619664342929711509 ) ) ;
#5582 = CARTESIAN_POINT ( 'NONE',  ( 0.1532563361054083140, 11.00893115100078568, 1.131784320476157264E-15 ) ) ;
#5583 = CARTESIAN_POINT ( 'NONE',  ( 18.61655166652078108, 59.87718327197428181, 6.499999999999962697 ) ) ;
#5584 = CARTESIAN_POINT ( 'NONE',  ( 9.846743663894590881, 18.30059781766744820, 2.638427012816828565 ) ) ;
#5585 = ORIENTED_EDGE ( 'NONE', *, *, #97321, .F. ) ;
#5586 = VERTEX_POINT ( 'NONE', #77194 ) ;
#5587 =( NAMED_UNIT ( * ) SI_UNIT ( $, .STERADIAN. ) SOLID_ANGLE_UNIT ( ) );
#5588 = EDGE_LOOP ( 'NONE', ( #76678, #1432, #7593, #62145 ) ) ;
#5590 = CARTESIAN_POINT ( 'NONE',  ( 4.559911319644449179, 18.89701867748817321, 9.422509992056141925 ) ) ;
#5589 = CARTESIAN_POINT ( 'NONE',  ( 10.00000000000000178, 14.31368534415483929, 10.88017736071110342 ) ) ;
#5592 = CARTESIAN_POINT ( 'NONE',  ( 6.565887622018943937, 20.16530133659708213, 12.81628187352647430 ) ) ;
#5591 = CARTESIAN_POINT ( 'NONE',  ( 19.84674366389459266, 58.30059781766745886, 2.638427012816836559 ) ) ;
#5593 = CARTESIAN_POINT ( 'NONE',  ( -2.266590686148945544, 11.38708216824730179, -7.082119434687050408 ) ) ;
#5594 = CARTESIAN_POINT ( 'NONE',  ( 22.81628187352647785, 36.41530133659707502, 3.434112377981063169 ) ) ;
#5595 = ORIENTED_EDGE ( 'NONE', *, *, #20390, .T. ) ;
#5596 = CARTESIAN_POINT ( 'NONE',  ( 12.63842701281683922, 29.55059781766745175, -9.846743663894590881 ) ) ;
#5597 = CARTESIAN_POINT ( 'NONE',  ( 12.91533473730992121, 4.522018677488170546, 10.88017736071110164 ) ) ;
#5598 = ORIENTED_EDGE ( 'NONE', *, *, #25141, .F. ) ;
#5599 = CARTESIAN_POINT ( 'NONE',  ( 2.035157376598822676, 7.438685344154837509, -7.964842623401177768 ) ) ;
#5600 = VERTEX_POINT ( 'NONE', #3178 ) ;
#5601 = CARTESIAN_POINT ( 'NONE',  ( 15.44008868035555260, 49.73035201082150536, 9.422509992056143702 ) ) ;
#5602 = CARTESIAN_POINT ( 'NONE',  ( 17.96484262340118221, 61.18868534415482685, -7.964842623401177768 ) ) ;
#5603 = CARTESIAN_POINT ( 'NONE',  ( 2.035157376598822676, 47.43868534415484817, -7.964842623401177768 ) ) ;
#5604 = AXIS2_PLACEMENT_3D ( 'NONE', #70959, #55455, #38981 ) ;
#5605 = DIRECTION ( 'NONE',  ( -0.000000000000000000, -1.000000000000000000, -0.000000000000000000 ) ) ;
#5606 = CARTESIAN_POINT ( 'NONE',  ( 19.42250999205614548, 40.98035201082150536, -5.440088680355545492 ) ) ;
#5607 = CARTESIAN_POINT ( 'NONE',  ( 1.492507162822263256, 47.19955587570481725, -6.500000000000077272 ) ) ;
#5608 = ORIENTED_EDGE ( 'NONE', *, *, #17531, .T. ) ;
#5609 = CARTESIAN_POINT ( 'NONE',  ( 10.00000000000000000, 34.75893115100078745, -9.846743663894594434 ) ) ;
#5610 = ORIENTED_EDGE ( 'NONE', *, *, #17730, .F. ) ;
#5611 = CARTESIAN_POINT ( 'NONE',  ( 0.1532563361054100626, 55.80059781766745175, -2.638427012816831230 ) ) ;
#5612 =( GEOMETRIC_REPRESENTATION_CONTEXT ( 3 ) GLOBAL_UNCERTAINTY_ASSIGNED_CONTEXT ( ( #79519 ) ) GLOBAL_UNIT_ASSIGNED_CONTEXT ( ( #29817, #24318, #835 ) ) REPRESENTATION_CONTEXT ( 'NONE', 'WORKASPACE' ) );
#5613 = DIRECTION ( 'NONE',  ( 0.000000000000000000, 1.000000000000000000, 0.000000000000000000 ) ) ;
#5614 = CARTESIAN_POINT ( 'NONE',  ( 24.16423886937410614, 4.512082168247300906, -3.795296366450302550 ) ) ;
#5615 = ORIENTED_EDGE ( 'NONE', *, *, #37205, .F. ) ;
#5616 = CARTESIAN_POINT ( 'NONE',  ( 12.80781515976314822, 15.00000000000000000, -6.246788841744324472 ) ) ;
#5617 = CARTESIAN_POINT ( 'NONE',  ( -4.536330790005646207, -17.54398820868007647, 3.750000000000000000 ) ) ;
#5618 = DIRECTION ( 'NONE',  ( 0.000000000000000000, 0.000000000000000000, -1.000000000000000000 ) ) ;
#5619 = CARTESIAN_POINT ( 'NONE',  ( 17.08211943468705840, 55.13708216824731068, -12.26659068614894466 ) ) ;
#5620 = CARTESIAN_POINT ( 'NONE',  ( -9.065164099344370285, 0.5000000000000004441, -11.95084933600779564 ) ) ;
#5621 = ORIENTED_EDGE ( 'NONE', *, *, #24086, .F. ) ;
#5622 = DIRECTION ( 'NONE',  ( 0.000000000000000000, 1.000000000000000000, 0.000000000000000000 ) ) ;
#5623 = CARTESIAN_POINT ( 'NONE',  ( 0.1532563361054100626, 45.80059781766745886, -2.638427012816831230 ) ) ;
#5624 = DIRECTION ( 'NONE',  ( -0.000000000000000000, -1.000000000000000000, 0.000000000000000000 ) ) ;
#5625 = CARTESIAN_POINT ( 'NONE',  ( 6.565887622018943937, 23.08196800326375708, -12.81628187352647608 ) ) ;
#5626 = CARTESIAN_POINT ( 'NONE',  ( 0.1532563361054082862, 16.21726448433411960, 2.638427012816831674 ) ) ;
#5627 = DIRECTION ( 'NONE',  ( 0.000000000000000000, 1.000000000000000000, 0.000000000000000000 ) ) ;
#5628 = CARTESIAN_POINT ( 'NONE',  ( 18.52753015748618282, 3.925597817667451306, -4.923371831947291888 ) ) ;
#5629 = CARTESIAN_POINT ( 'NONE',  ( 0.6178305044545838731, -0.2513653300695798953, 9.382169495545420901 ) ) ;
#5630 = CARTESIAN_POINT ( 'NONE',  ( 0.000000000000000000, 0.5000000000000004441, 0.000000000000000000 ) ) ;
#5631 = CIRCLE ( 'NONE', #50358, 14.49999999999999822 ) ;
#5632 = ORIENTED_EDGE ( 'NONE', *, *, #30715, .T. ) ;
#5633 = CARTESIAN_POINT ( 'NONE',  ( 17.96484262340118221, 16.18868534415483396, -7.964842623401177768 ) ) ;
#5634 = CARTESIAN_POINT ( 'NONE',  ( 6.204703633549690345, 7.845415501580634832, 14.16423886937410082 ) ) ;
#5635 = CARTESIAN_POINT ( 'NONE',  ( 10.00000000000000178, 22.25893115100078745, 9.846743663894594434 ) ) ;
#5636 = CARTESIAN_POINT ( 'NONE',  ( 20.88017736071110875, 50.77201867748817676, -2.915334737309920765 ) ) ;
#5638 = CARTESIAN_POINT ( 'NONE',  ( -4.084234479374258875, 0.000000000000000000, -3.613425430272983352 ) ) ;
#5637 = CARTESIAN_POINT ( 'NONE',  ( 21.09922568453595559, 32.04030133659708923, -6.408140936763230044 ) ) ;
#5639 = CARTESIAN_POINT ( 'NONE',  ( 7.084665262690076126, 7.022018677488169658, -10.88017736071110164 ) ) ;
#5640 = LINE ( 'NONE', #36117, #86845 ) ;
#5641 =( LENGTH_UNIT ( ) NAMED_UNIT ( * ) SI_UNIT ( .MILLI., .METRE. ) );
#5642 = CARTESIAN_POINT ( 'NONE',  ( -2.816281873526473856, 4.123634669930420493, 9.499525473075851096E-16 ) ) ;
#5643 = CARTESIAN_POINT ( 'NONE',  ( 19.84674366389459266, 63.30059781766745886, 2.638427012816836559 ) ) ;
#5644 = CARTESIAN_POINT ( 'NONE',  ( 18.52753015748618282, 18.92559781766745175, -4.923371831947291888 ) ) ;
#5645 = CARTESIAN_POINT ( 'NONE',  ( -7.964842623401179544, -22.56131465584515894, -7.964842623401174215 ) ) ;
#5646 = CARTESIAN_POINT ( 'NONE',  ( 13.43411237798106583, 22.66530133659708923, -12.81628187352647252 ) ) ;
#5647 = CARTESIAN_POINT ( 'NONE',  ( 2.603489959281613420, 50.43575266056826933, -6.500000000000031086 ) ) ;
#5649 = CYLINDRICAL_SURFACE ( 'NONE', #86302, 0.2500000000000002220 ) ;
#5648 = CARTESIAN_POINT ( 'NONE',  ( 19.42250999205614193, 45.14701867748817676, 5.440088680355555262 ) ) ;
#5650 = CARTESIAN_POINT ( 'NONE',  ( 0.000000000000000000, 0.5000000000000004441, 0.000000000000000000 ) ) ;
#5651 = VECTOR ( 'NONE', #850, 1000.000000000000000 ) ;
#5652 = EDGE_CURVE ( 'NONE', #97107, #57318, #38453, .T. ) ;
#5653 = DIRECTION ( 'NONE',  ( -0.9890158633619177131, 0.000000000000000000, 0.1478094111296046342 ) ) ;
#5654 = CARTESIAN_POINT ( 'NONE',  ( 0.5774900079438607392, 33.48035201082150536, 5.440088680355550821 ) ) ;
#5655 = CARTESIAN_POINT ( 'NONE',  ( 12.91533473730993009, 26.60535201082150536, -10.88017736071109987 ) ) ;
#5656 = CARTESIAN_POINT ( 'NONE',  ( 0.1532563361054100626, 50.80059781766745175, -2.638427012816831230 ) ) ;
#5657 = CARTESIAN_POINT ( 'NONE',  ( 19.42250999205614548, 50.98035201082151247, -5.440088680355545492 ) ) ;
#5658 = VECTOR ( 'NONE', #2728, 1000.000000000000000 ) ;
#5659 = CARTESIAN_POINT ( 'NONE',  ( 24.16423886937410614, 29.30374883491396787, 8.672049930838204340E-16 ) ) ;
#5660 = CARTESIAN_POINT ( 'NONE',  ( 0.1532563361054083140, 36.00893115100078745, 1.131784320476157264E-15 ) ) ;
#5661 = CARTESIAN_POINT ( 'NONE',  ( 19.38216949554541202, 60.99863466993042493, 9.382169495545424454 ) ) ;
#5662 = CARTESIAN_POINT ( 'NONE',  ( 22.81628187352648496, 1.831968003263753753, -3.434112377981050290 ) ) ;
#5663 = ORIENTED_EDGE ( 'NONE', *, *, #59717, .T. ) ;
#5664 = CARTESIAN_POINT ( 'NONE',  ( 17.96484262340118221, 19.93868534415484106, 7.964842623401181321 ) ) ;
#5665 = CARTESIAN_POINT ( 'NONE',  ( 10.00000000000000000, 6.813685344154838397, -10.88017736071110342 ) ) ;
#5666 = CARTESIAN_POINT ( 'NONE',  ( 19.42250999205614193, 10.14701867748816966, 5.440088680355555262 ) ) ;
#5667 = CARTESIAN_POINT ( 'NONE',  ( 12.91533473730993009, 66.60535201082150536, -10.88017736071109987 ) ) ;
#5668 = CARTESIAN_POINT ( 'NONE',  ( -2.266590686148945544, 27.22041550158063572, 7.082119434687048631 ) ) ;
#5669 = CARTESIAN_POINT ( 'NONE',  ( 1.472469842513823179, 20.59226448433411960, -4.923371831947296329 ) ) ;
#5670 = CARTESIAN_POINT ( 'NONE',  ( 19.84674366389459266, 63.30059781766745886, 2.638427012816836559 ) ) ;
#5671 = CARTESIAN_POINT ( 'NONE',  ( 7.084665262690076126, 29.10535201082150181, 10.88017736071109987 ) ) ;
#5672 = CARTESIAN_POINT ( 'NONE',  ( -7.551349515323269479, 15.00000000000000000, 12.08468537022900868 ) ) ;
#5673 = DIRECTION ( 'NONE',  ( -0.000000000000000000, 0.000000000000000000, 1.000000000000000000 ) ) ;
#5674 = ORIENTED_EDGE ( 'NONE', *, *, #84120, .T. ) ;
#5675 = CARTESIAN_POINT ( 'NONE',  ( 3.558677480090427281, 70.40124509038875544, 5.000000000000000000 ) ) ;
#5676 = CARTESIAN_POINT ( 'NONE',  ( 19.84674366389459621, 43.50893115100078745, 7.409399052514197653E-17 ) ) ;
#5677 = ORIENTED_EDGE ( 'NONE', *, *, #22946, .F. ) ;
#5678 = ORIENTED_EDGE ( 'NONE', *, *, #87817, .T. ) ;
#5679 = CARTESIAN_POINT ( 'NONE',  ( -14.88232117145529365, 0.3640475087720984049, -1.875237731503342609 ) ) ;
#5680 = CARTESIAN_POINT ( 'NONE',  ( -4.164238869374099927, 27.01208216824730357, 3.795296366450308767 ) ) ;
#5682 = EDGE_CURVE ( 'NONE', #507, #90918, #33633, .T. ) ;
#5681 = CARTESIAN_POINT ( 'NONE',  ( 13.79529636645030344, 13.26208216824729824, 14.16423886937410614 ) ) ;
#5683 = CARTESIAN_POINT ( 'NONE',  ( 20.88017736071110519, 60.56368534415484106, 2.639326808657452039E-16 ) ) ;
#5684 = CARTESIAN_POINT ( 'NONE',  ( 6.204703633549690345, 57.84541550158063927, 14.16423886937410082 ) ) ;
#5685 = CARTESIAN_POINT ( 'NONE',  ( 0.6178305044545818747, -1.501365330069579951, -9.382169495545419124 ) ) ;
#5686 = CARTESIAN_POINT ( 'NONE',  ( 19.84674366389459621, 48.50893115100078745, 7.409399052514197653E-17 ) ) ;
#5688 = CARTESIAN_POINT ( 'NONE',  ( 0.6178305044545838731, -0.2513653300695798953, 9.382169495545420901 ) ) ;
#5687 = CARTESIAN_POINT ( 'NONE',  ( 19.42250999205614548, 40.98035201082150536, -5.440088680355545492 ) ) ;
#5689 = CARTESIAN_POINT ( 'NONE',  ( 10.00000000000000000, 15.55374883491396787, -14.16423886937410082 ) ) ;
#5690 = VECTOR ( 'NONE', #51015, 1000.000000000000000 ) ;
#5691 = CARTESIAN_POINT ( 'NONE',  ( 20.88017736071110519, 15.56368534415483751, 2.639326808657452039E-16 ) ) ;
#5692 = CARTESIAN_POINT ( 'NONE',  ( 20.04068437667225666, 14.71974360917720226, 6.396802510829714628 ) ) ;
#5693 = DIRECTION ( 'NONE',  ( 1.000000000000000000, 0.000000000000000000, 0.000000000000000000 ) ) ;
#5694 = CARTESIAN_POINT ( 'NONE',  ( -0.8801773607110991993, 47.85535201082150536, -2.915334737309923874 ) ) ;
#5695 = CARTESIAN_POINT ( 'NONE',  ( 7.208316651077762316, -35.86606884899921255, -7.208316651077764980 ) ) ;
#5696 = EDGE_LOOP ( 'NONE', ( #72256, #44786, #30246, #34006 ) ) ;
#5697 = LINE ( 'NONE', #15176, #55510 ) ;
#5698 = ORIENTED_EDGE ( 'NONE', *, *, #88507, .F. ) ;
#5699 = ORIENTED_EDGE ( 'NONE', *, *, #5339, .T. ) ;
#5700 = CARTESIAN_POINT ( 'NONE',  ( 17.08211943468705130, 43.47041550158063927, 12.26659068614894998 ) ) ;
#5701 = CARTESIAN_POINT ( 'NONE',  ( 0.1532563361054083140, 46.00893115100079456, 1.131784320476157264E-15 ) ) ;
#5702 = CARTESIAN_POINT ( 'NONE',  ( 12.91533473730992121, 64.52201867748817676, 10.88017736071110164 ) ) ;
#5703 = CARTESIAN_POINT ( 'NONE',  ( 10.64017930668205736, 15.00000000000000000, -10.57291749337215592 ) ) ;
#5704 = CARTESIAN_POINT ( 'NONE',  ( 19.42250999205614193, 60.14701867748817676, 5.440088680355555262 ) ) ;
#5705 = COLOUR_RGB ( '', 0.08235294, 0.09019608, 0.10196078) ;
#5706 = CARTESIAN_POINT ( 'NONE',  ( -1.099225684535947600, 54.54030133659708923, 6.408140936763237150 ) ) ;
#5707 = CARTESIAN_POINT ( 'NONE',  ( 3.434112377981054287, 12.66530133659709101, -12.81628187352647608 ) ) ;
#5708 = ORIENTED_EDGE ( 'NONE', *, *, #7546, .T. ) ;
#5709 = CARTESIAN_POINT ( 'NONE',  ( 2.917880565312948704, 22.63708216824730002, 12.26659068614894643 ) ) ;
#5710 = CARTESIAN_POINT ( 'NONE',  ( 3.591859063236763294, 18.29030133659708568, -11.09922568453595026 ) ) ;
#5711 = VERTEX_POINT ( 'NONE', #40186 ) ;
#5712 = CARTESIAN_POINT ( 'NONE',  ( 6.565887622018943937, 45.16530133659708923, 12.81628187352647430 ) ) ;
#5713 = ADVANCED_FACE ( 'NONE', ( #24702 ), #9690, .F. ) ;
#5714 = CARTESIAN_POINT ( 'NONE',  ( 2.791683348922240793, 31.63393115100078745, 7.208316651077764092 ) ) ;
#5715 = CARTESIAN_POINT ( 'NONE',  ( 7.084665262690076126, 9.105352010821503583, 10.88017736071109987 ) ) ;
#5716 = CARTESIAN_POINT ( 'NONE',  ( 0.6178305044545818747, 53.49863466993041072, -9.382169495545419124 ) ) ;
#5717 = DIRECTION ( 'NONE',  ( -0.3826834323650877279, 0.000000000000000000, -0.9238795325112876267 ) ) ;
#5718 = CARTESIAN_POINT ( 'NONE',  ( 18.52753015748617571, 48.09226448433412315, 4.923371831947298993 ) ) ;
#5719 = COLOUR_RGB ( '', 0.40784314, 0.44705882, 0.49803922) ;
#5720 = EDGE_CURVE ( 'NONE', #4379, #97455, #15796, .T. ) ;
#5722 = EDGE_LOOP ( 'NONE', ( #23565, #73701, #81169, #13580 ) ) ;
#5721 = CARTESIAN_POINT ( 'NONE',  ( 18.72515096720568550, 20.05509018479935790, 6.500000000000015099 ) ) ;
#5723 = PRESENTATION_LAYER_ASSIGNMENT (  '', '', ( #66149 ) ) ;
#5724 = FACE_OUTER_BOUND ( 'NONE', #13078, .T. ) ;
#5725 = CARTESIAN_POINT ( 'NONE',  ( 14.49999999999999822, 60.50000000000000000, 6.000000000000000000 ) ) ;
#5726 = DIRECTION ( 'NONE',  ( 0.000000000000000000, 0.000000000000000000, 1.000000000000000000 ) ) ;
#5727 = DIRECTION ( 'NONE',  ( 1.000000000000000000, 0.000000000000000000, 0.000000000000000000 ) ) ;
#5728 = CARTESIAN_POINT ( 'NONE',  ( 19.84674366389459266, 13.71726448433411782, -2.638427012816827677 ) ) ;
#5729 = CARTESIAN_POINT ( 'NONE',  ( -2.816281873526473856, 19.33196800326375708, 3.434112377981055619 ) ) ;
#5730 = CYLINDRICAL_SURFACE ( 'NONE', #81897, 0.5000000000000004441 ) ;
#5731 = ADVANCED_FACE ( 'NONE', ( #84709 ), #70693, .T. ) ;
#5732 = ORIENTED_EDGE ( 'NONE', *, *, #57354, .F. ) ;
#5733 = CARTESIAN_POINT ( 'NONE',  ( 18.52753015748617571, 58.09226448433411605, 4.923371831947298993 ) ) ;
#5734 = CARTESIAN_POINT ( 'NONE',  ( 18.72515096720570327, 6.072280503510315341, -6.499999999999985789 ) ) ;
#5735 = CARTESIAN_POINT ( 'NONE',  ( 20.36894250292379738, 24.92874883491396787, -10.36894250292379027 ) ) ;
#5736 = CARTESIAN_POINT ( 'NONE',  ( 17.20831665107776587, 47.88393115100078745, 7.208316651077764980 ) ) ;
#5737 = CARTESIAN_POINT ( 'NONE',  ( 16.40814093676324603, 42.45696800326375353, -11.09922568453594671 ) ) ;
#5738 = CARTESIAN_POINT ( 'NONE',  ( -14.42571047809455642, 0.2306972965111904750, -3.890621016588054815 ) ) ;
#5739 = CARTESIAN_POINT ( 'NONE',  ( 7.361572987183169658, 9.967264484334119601, -9.846743663894592657 ) ) ;
#5740 = CARTESIAN_POINT ( 'NONE',  ( 14.92337183194729633, 37.67559781766745175, 8.527530157486181039 ) ) ;
#5741 = CARTESIAN_POINT ( 'NONE',  ( 20.88017736071110519, 40.56368534415484106, 2.639326808657452039E-16 ) ) ;
#5742 = TOROIDAL_SURFACE ( 'NONE', #87158, 14.49999999999999822, 0.5000000000000000000 ) ;
#5743 = CARTESIAN_POINT ( 'NONE',  ( 14.92337183194729988, 34.34226448433411605, -8.527530157486177487 ) ) ;
#5744 = PRODUCT_CONTEXT ( 'NONE', #6554, 'mechanical' ) ;
#5745 = FACE_OUTER_BOUND ( 'NONE', #26438, .T. ) ;
#5746 = AXIS2_PLACEMENT_3D ( 'NONE', #95832, #27314, #58297 ) ;
#5747 = CARTESIAN_POINT ( 'NONE',  ( 7.084665262690076126, 52.02201867748816255, -10.88017736071110164 ) ) ;
#5748 = STYLED_ITEM ( 'NONE', ( #82397 ), #86608 ) ;
#5749 = ORIENTED_EDGE ( 'NONE', *, *, #4333, .F. ) ;
#5750 = CARTESIAN_POINT ( 'NONE',  ( 3.897244926436219892, 4.401207273199346175E-16, -13.96644127841330807 ) ) ;
#5751 = CARTESIAN_POINT ( 'NONE',  ( 19.42250999205614548, 10.98035201082150358, -5.440088680355545492 ) ) ;
#5753 = CARTESIAN_POINT ( 'NONE',  ( 17.96484262340118221, 44.93868534415483396, 7.964842623401181321 ) ) ;
#5752 = CARTESIAN_POINT ( 'NONE',  ( 19.84674366389459266, 58.71726448433411605, -2.638427012816827677 ) ) ;
#5754 = DIRECTION ( 'NONE',  ( 0.000000000000000000, 0.000000000000000000, 1.000000000000000000 ) ) ;
#5755 = CARTESIAN_POINT ( 'NONE',  ( 15.44008868035555793, 56.39701867748817676, -9.422509992056140149 ) ) ;
#5757 = CARTESIAN_POINT ( 'NONE',  ( 0.000000000000000000, 0.5000000000000004441, 0.000000000000000000 ) ) ;
#5756 = CARTESIAN_POINT ( 'NONE',  ( 20.88017736071110519, 20.56368534415484106, 2.639326808657452039E-16 ) ) ;
#5758 = CARTESIAN_POINT ( 'NONE',  ( 18.72515096720571037, 50.05509018479936856, 6.499999999999982236 ) ) ;
#5759 = CARTESIAN_POINT ( 'NONE',  ( 18.52753015748618282, 18.92559781766745175, -4.923371831947291888 ) ) ;
#5760 = CARTESIAN_POINT ( 'NONE',  ( -46.68456736488007408, 103.6675473310227034, 5.000000000000000000 ) ) ;
#5761 = CARTESIAN_POINT ( 'NONE',  ( -12.26659068614895354, 11.38708216824730535, -7.082119434687038861 ) ) ;
#5762 = CARTESIAN_POINT ( 'NONE',  ( 17.20831665107776587, 49.13393115100078745, -7.208316651077762316 ) ) ;
#5763 = CARTESIAN_POINT ( 'NONE',  ( -4.164238869374099927, 62.01208216824728936, 3.795296366450308767 ) ) ;
#5764 = CARTESIAN_POINT ( 'NONE',  ( 2.153642693323417845, 61.13791097397316321, -6.499999999999922728 ) ) ;
#5765 = CARTESIAN_POINT ( 'NONE',  ( 20.36894250292379382, 13.67874883491396965, 10.36894250292379205 ) ) ;
#5766 = EDGE_CURVE ( 'NONE', #28519, #35759, #54679, .T. ) ;
#5767 = CARTESIAN_POINT ( 'NONE',  ( 22.26659068614894466, 33.88708216824730357, 7.082119434687054849 ) ) ;
#5768 = CARTESIAN_POINT ( 'NONE',  ( 0.6178305044545838731, 9.748634669930416052, 9.382169495545420901 ) ) ;
#5769 = EDGE_LOOP ( 'NONE', ( #94368, #14118, #42047, #79944 ) ) ;
#5770 = CARTESIAN_POINT ( 'NONE',  ( 20.88017736071110875, 15.77201867748817143, -2.915334737309920765 ) ) ;
#5771 = EDGE_CURVE ( 'NONE', #59748, #53014, #17034, .T. ) ;
#5772 = CARTESIAN_POINT ( 'NONE',  ( 10.00000000000000178, 52.25893115100078745, 9.846743663894594434 ) ) ;
#5774 = CARTESIAN_POINT ( 'NONE',  ( -11.26637474388419591, 89.93360374965293147, -6.408881440111466432 ) ) ;
#5773 = FACE_OUTER_BOUND ( 'NONE', #62963, .T. ) ;
#5775 = FACE_OUTER_BOUND ( 'NONE', #45800, .T. ) ;
#5776 = CARTESIAN_POINT ( 'NONE',  ( 14.92337183194729988, 4.342264484334117824, -8.527530157486177487 ) ) ;
#5777 = CARTESIAN_POINT ( 'NONE',  ( 0.6178305044545838731, 29.74863466993042138, 9.382169495545420901 ) ) ;
#5778 = CARTESIAN_POINT ( 'NONE',  ( 5.076628168052703671, 26.84226448433411960, 8.527530157486179263 ) ) ;
#5779 = EDGE_LOOP ( 'NONE', ( #78866, #86254, #22881, #76246 ) ) ;
#5780 = CARTESIAN_POINT ( 'NONE',  ( 18.52753015748617571, 3.092264484334118269, 4.923371831947298993 ) ) ;
#5781 = FACE_OUTER_BOUND ( 'NONE', #20887, .T. ) ;
#5782 = CARTESIAN_POINT ( 'NONE',  ( -53.17073170731706711, 42.53658536585359684, -8.000000000000000000 ) ) ;
#5783 = CARTESIAN_POINT ( 'NONE',  ( 7.084665262690076126, 17.02201867748817676, -10.88017736071110164 ) ) ;
#5784 = CARTESIAN_POINT ( 'NONE',  ( -2.266590686148945544, 42.22041550158063217, 7.082119434687048631 ) ) ;
#5785 = CARTESIAN_POINT ( 'NONE',  ( 10.00000000000000178, 59.31368534415484106, 10.88017736071110342 ) ) ;
#5786 = CARTESIAN_POINT ( 'NONE',  ( 14.92337183194729988, 19.34226448433411960, -8.527530157486177487 ) ) ;
#5787 = CARTESIAN_POINT ( 'NONE',  ( 17.20831665107776587, 9.133931151000787452, -7.208316651077762316 ) ) ;
#5788 = CARTESIAN_POINT ( 'NONE',  ( -1.468748247964608566, 5.397528278722328812E-15, 2.247705202101426103 ) ) ;
#5789 = CARTESIAN_POINT ( 'NONE',  ( 7.361572987183169658, 34.96726448433411605, -9.846743663894592657 ) ) ;
#5790 = CARTESIAN_POINT ( 'NONE',  ( 12.63842701281683034, 57.46726448433411605, 9.846743663894596210 ) ) ;
#5791 = EDGE_CURVE ( 'NONE', #16659, #47034, #62178, .T. ) ;
#5792 = CIRCLE ( 'NONE', #21789, 6.999999999999995559 ) ;
#5793 = CARTESIAN_POINT ( 'NONE',  ( 12.91533473730993009, 36.60535201082151247, -10.88017736071109987 ) ) ;
#5794 = ORIENTED_EDGE ( 'NONE', *, *, #82294, .T. ) ;
#5795 = CARTESIAN_POINT ( 'NONE',  ( -2.816281873526471635, 63.91530133659708923, -3.434112377981056508 ) ) ;
#5797 = ADVANCED_FACE ( 'NONE', ( #63165 ), #53575, .T. ) ;
#5796 = CARTESIAN_POINT ( 'NONE',  ( -7.750000000000000000, 79.82179676972448590, -6.250000000000000000 ) ) ;
#5798 = CARTESIAN_POINT ( 'NONE',  ( 17.96484262340118221, 66.18868534415483396, -7.964842623401177768 ) ) ;
#5799 = CARTESIAN_POINT ( 'NONE',  ( 21.09922568453594849, 46.20696800326376064, 6.408140936763242479 ) ) ;
#5801 = CARTESIAN_POINT ( 'NONE',  ( 2.791683348922240793, 36.63393115100078035, 7.208316651077764092 ) ) ;
#5800 = CARTESIAN_POINT ( 'NONE',  ( 24.16423886937410614, 64.51208216824728936, -3.795296366450302550 ) ) ;
#5802 = CARTESIAN_POINT ( 'NONE',  ( 2.917880565312948704, 42.63708216824729647, 12.26659068614894643 ) ) ;
#5803 = CARTESIAN_POINT ( 'NONE',  ( 18.52753015748617571, 48.09226448433412315, 4.923371831947298993 ) ) ;
#5804 = FILL_AREA_STYLE ('',( #74276 ) ) ;
#5805 = CARTESIAN_POINT ( 'NONE',  ( -0.8801773607111008646, 43.27201867748817676, 2.915334737309923430 ) ) ;
#5806 = ADVANCED_FACE ( 'NONE', ( #1717 ), #32873, .T. ) ;
#5807 = CARTESIAN_POINT ( 'NONE',  ( 2.791683348922237240, 0.3839311510007847872, -7.208316651077763204 ) ) ;
#5808 = CARTESIAN_POINT ( 'NONE',  ( 1.959929470562272291, 55.51528370094808906, -5.767676674365837641 ) ) ;
#5809 = ORIENTED_EDGE ( 'NONE', *, *, #98463, .T. ) ;
#5810 = CARTESIAN_POINT ( 'NONE',  ( 19.38216949554541202, 60.99863466993042493, 9.382169495545424454 ) ) ;
#5811 = EDGE_LOOP ( 'NONE', ( #23535, #58184, #19969, #31551 ) ) ;
#5812 = CARTESIAN_POINT ( 'NONE',  ( 19.84674366389459621, 3.508931151000785231, 7.409399052514197653E-17 ) ) ;
#5813 = VERTEX_POINT ( 'NONE', #17208 ) ;
#5814 = CARTESIAN_POINT ( 'NONE',  ( 0.1532563361054083140, 1.008931151000784787, 1.131784320476157264E-15 ) ) ;
#5815 = CARTESIAN_POINT ( 'NONE',  ( 1.361758211743682168, 0.02824709245459683729, -6.170260303628292142 ) ) ;
#5816 = COLOUR_RGB ( '', 0.08235294, 0.09019608, 0.10196078) ;
#5817 = ORIENTED_EDGE ( 'NONE', *, *, #32860, .F. ) ;
#5818 = PRESENTATION_LAYER_ASSIGNMENT (  '', '', ( #28140 ) ) ;
#5819 = CARTESIAN_POINT ( 'NONE',  ( 7.084665262690076126, 14.10535201082150358, 10.88017736071109987 ) ) ;
#5820 = PLANE ( 'NONE',  #35601 ) ;
#5821 = EDGE_LOOP ( 'NONE', ( #8582, #74835, #91753, #14856 ) ) ;
#5822 = CARTESIAN_POINT ( 'NONE',  ( 10.00000000000000000, 21.81368534415484106, -10.88017736071110342 ) ) ;
#5823 = CARTESIAN_POINT ( 'NONE',  ( 7.361572987183170547, 62.05059781766745886, 9.846743663894590881 ) ) ;
#5824 = ORIENTED_EDGE ( 'NONE', *, *, #68460, .T. ) ;
#5825 = CARTESIAN_POINT ( 'NONE',  ( 1.472469842513823179, 65.59226448433412315, -4.923371831947296329 ) ) ;
#5826 = ORIENTED_EDGE ( 'NONE', *, *, #43014, .T. ) ;
#5827 = CARTESIAN_POINT ( 'NONE',  ( 20.88017736071110519, 60.56368534415484106, 2.639326808657452039E-16 ) ) ;
#5828 = CARTESIAN_POINT ( 'NONE',  ( 5.076628168052704559, 65.17559781766745175, -8.527530157486179263 ) ) ;
#5829 = CARTESIAN_POINT ( 'NONE',  ( 3.591859063236761518, 39.95696800326375353, 11.09922568453594849 ) ) ;
#5831 = CARTESIAN_POINT ( 'NONE',  ( 14.24131928502211686, -0.03417435944610275333, -0.4973178280105898241 ) ) ;
#5830 = CARTESIAN_POINT ( 'NONE',  ( 20.88017736071110164, 5.355352010821502695, 2.915334737309930979 ) ) ;
#5832 = CARTESIAN_POINT ( 'NONE',  ( 0.1532563361054083140, 1.008931151000784787, 1.131784320476157264E-15 ) ) ;
#5833 = CARTESIAN_POINT ( 'NONE',  ( 15.44008868035555260, 24.73035201082150891, 9.422509992056143702 ) ) ;
#5834 = EDGE_CURVE ( 'NONE', #92561, #38139, #98147, .T. ) ;
#5835 = AXIS2_PLACEMENT_3D ( 'NONE', #47170, #64133, #94155 ) ;
#5836 = ORIENTED_EDGE ( 'NONE', *, *, #96583, .F. ) ;
#5837 = AXIS2_PLACEMENT_3D ( 'NONE', #95124, #50121, #80631 ) ;
#5838 = CARTESIAN_POINT ( 'NONE',  ( -2.816281873526471635, 53.91530133659709634, -3.434112377981056508 ) ) ;
#5839 = CARTESIAN_POINT ( 'NONE',  ( -0.8801773607111008646, 43.27201867748817676, 2.915334737309923430 ) ) ;
#5840 = CARTESIAN_POINT ( 'NONE',  ( 3.969999999999999751, 10.25000000000000000, 2.750000000000000000 ) ) ;
#5841 = CARTESIAN_POINT ( 'NONE',  ( 10.00000000000000178, 60.37363466993041783, 12.81628187352647608 ) ) ;
#5842 = CARTESIAN_POINT ( 'NONE',  ( 19.42250999205614193, 50.14701867748817676, 5.440088680355555262 ) ) ;
#5843 = CARTESIAN_POINT ( 'NONE',  ( 1.472469842513823179, 60.59226448433412315, -4.923371831947296329 ) ) ;
#5844 = CARTESIAN_POINT ( 'NONE',  ( 0.1129803114748853671, 49.29427333184091964, -6.480634945678684922 ) ) ;
#5845 = B_SPLINE_CURVE_WITH_KNOTS ( 'NONE', 3,
 ( #87370, #63385, #86398, #63862, #9409, #55405 ),
 .UNSPECIFIED., .F., .F.,
 ( 4, 2, 4 ),
 ( 0.000000000000000000, 0.0002605067024380848333, 0.0005210134048761696666 ),
 .UNSPECIFIED. ) ;
#5846 = CARTESIAN_POINT ( 'NONE',  ( 12.63842701281683922, 19.55059781766745175, -9.846743663894590881 ) ) ;
#5847 = CARTESIAN_POINT ( 'NONE',  ( 6.565887622018943937, 3.081968003263753531, -12.81628187352647608 ) ) ;
#5849 = CARTESIAN_POINT ( 'NONE',  ( 19.50000000000000711, 105.0000000000000000, 4.500000000000000888 ) ) ;
#5848 = FACE_OUTER_BOUND ( 'NONE', #62243, .T. ) ;
#5850 = CARTESIAN_POINT ( 'NONE',  ( 20.88017736071110519, 25.56368534415483751, 2.639326808657452039E-16 ) ) ;
#5851 = CARTESIAN_POINT ( 'NONE',  ( 0.1532563361054083140, 56.00893115100078745, 1.131784320476157264E-15 ) ) ;
#5852 = CARTESIAN_POINT ( 'NONE',  ( 17.20831665107776587, 4.133931151000785675, -7.208316651077762316 ) ) ;
#5853 = FACE_OUTER_BOUND ( 'NONE', #69431, .T. ) ;
#5855 = ORIENTED_EDGE ( 'NONE', *, *, #56361, .T. ) ;
#5854 = CARTESIAN_POINT ( 'NONE',  ( 3.591859063236763294, 3.290301336597087012, -11.09922568453595026 ) ) ;
#5856 = CARTESIAN_POINT ( 'NONE',  ( -10.70613742633263321, 15.00000000000000000, 9.778988772285140740 ) ) ;
#5857 = DIRECTION ( 'NONE',  ( 0.000000000000000000, 0.000000000000000000, -1.000000000000000000 ) ) ;
#5858 = CARTESIAN_POINT ( 'NONE',  ( -2.816281873526473856, 44.33196800326375353, 3.434112377981055619 ) ) ;
#5859 = CARTESIAN_POINT ( 'NONE',  ( 7.361572987183170547, 32.05059781766745175, 9.846743663894590881 ) ) ;
#5860 = CARTESIAN_POINT ( 'NONE',  ( 5.624999999999999112, 8.451366962315987053, -9.742785792574936821 ) ) ;
#5861 = CARTESIAN_POINT ( 'NONE',  ( 4.559911319644449179, 12.23035201082150714, -9.422509992056141925 ) ) ;
#5862 = CARTESIAN_POINT ( 'NONE',  ( 5.076628168052703671, 36.84226448433412315, 8.527530157486179263 ) ) ;
#5863 = VECTOR ( 'NONE', #21053, 1000.000000000000000 ) ;
#5864 = ORIENTED_EDGE ( 'NONE', *, *, #69035, .F. ) ;
#5865 = EDGE_CURVE ( 'NONE', #34058, #91342, #57562, .T. ) ;
#5866 = LINE ( 'NONE', #22849, #40869 ) ;
#5867 = CARTESIAN_POINT ( 'NONE',  ( 22.26659068614894466, 63.88708216824730357, 7.082119434687054849 ) ) ;
#5868 = DIRECTION ( 'NONE',  ( 0.000000000000000000, 0.000000000000000000, -1.000000000000000000 ) ) ;
#5869 = CARTESIAN_POINT ( 'NONE',  ( 4.559911319644449179, 13.89701867748817321, 9.422509992056141925 ) ) ;
#5870 = CARTESIAN_POINT ( 'NONE',  ( 13.79529636645030344, 43.26208216824730357, 14.16423886937410614 ) ) ;
#5872 = CARTESIAN_POINT ( 'NONE',  ( -10.93781366033354097, 0.5000000000000004441, 10.26470809774057713 ) ) ;
#5871 = CARTESIAN_POINT ( 'NONE',  ( 6.204703633549690345, 50.76208216824730357, -14.16423886937410259 ) ) ;
#5873 = CARTESIAN_POINT ( 'NONE',  ( 18.52753015748618282, 13.92559781766745175, -4.923371831947291888 ) ) ;
#5874 = CARTESIAN_POINT ( 'NONE',  ( 6.565887622018943937, -1.918031996736246692, -12.81628187352647608 ) ) ;
#5875 = CARTESIAN_POINT ( 'NONE',  ( 19.42250999205614193, 45.14701867748817676, 5.440088680355555262 ) ) ;
#5876 = LINE ( 'NONE', #60835, #64089 ) ;
#5877 = DIRECTION ( 'NONE',  ( 0.000000000000000000, 0.000000000000000000, 1.000000000000000000 ) ) ;
#5878 = CARTESIAN_POINT ( 'NONE',  ( 1.472469842513823179, 66.42559781766745175, 4.923371831947296329 ) ) ;
#5879 = CARTESIAN_POINT ( 'NONE',  ( -4.164238869374099039, 1.803748834913967647, 8.674139862899312516E-16 ) ) ;
#5880 = ORIENTED_EDGE ( 'NONE', *, *, #27317, .T. ) ;
#5881 = CARTESIAN_POINT ( 'NONE',  ( 10.00000000000000000, 29.75893115100078745, -9.846743663894594434 ) ) ;
#5882 = DIRECTION ( 'NONE',  ( 1.000000000000000000, 1.636349903325072848E-16, 0.000000000000000000 ) ) ;
#5883 = VERTEX_POINT ( 'NONE', #96647 ) ;
#5884 = CARTESIAN_POINT ( 'NONE',  ( 22.26659068614894466, 43.88708216824729647, 7.082119434687054849 ) ) ;
#5885 = ADVANCED_FACE ( 'NONE', ( #35633 ), #8897, .T. ) ;
#5886 = AXIS2_PLACEMENT_3D ( 'NONE', #23709, #8679, #62155 ) ;
#5887 = EDGE_CURVE ( 'NONE', #31069, #43200, #20133, .T. ) ;
#5888 = CARTESIAN_POINT ( 'NONE',  ( 7.361572987183169658, 14.96726448433411960, -9.846743663894592657 ) ) ;
#5889 = FILL_AREA_STYLE_COLOUR ( '', #83789 ) ;
#5890 = CARTESIAN_POINT ( 'NONE',  ( 10.00000000000000178, 34.31368534415484106, 10.88017736071110342 ) ) ;
#5891 = CARTESIAN_POINT ( 'NONE',  ( 16.40814093676323893, 35.79030133659708923, 11.09922568453595026 ) ) ;
#5892 =( BOUNDED_CURVE ( )  B_SPLINE_CURVE ( 2, ( #7354, #20868, #54304, #15842, #46807, #91828, #54791, #93293, #45842 ),
 .UNSPECIFIED., .F., .F. ) 
 B_SPLINE_CURVE_WITH_KNOTS ( ( 3, 2, 2, 2, 3 ),
 ( 0.2258552226545170460, 0.2261904761904761640, 0.2321428571428572063, 0.2380952380952381375, 0.2384304916311972555 ),
 .UNSPECIFIED. ) 
 CURVE ( )  GEOMETRIC_REPRESENTATION_ITEM ( )  RATIONAL_B_SPLINE_CURVE ( ( 0.9963778908391762723, 0.9980808541467921513, 1.000000000000000000, 0.9659258262890683122, 1.000000000000000000, 0.9659258262890683122, 1.000000000000000000, 0.9980808541467921513, 0.9963778908391762723 ) ) 
 REPRESENTATION_ITEM ( '' )  );
#5893 = CARTESIAN_POINT ( 'NONE',  ( -0.8801773607111009756, 3.063685344154837509, 1.068504757029289695E-15 ) ) ;
#5894 = CARTESIAN_POINT ( 'NONE',  ( 6.565887622018943937, 35.16530133659708923, 12.81628187352647430 ) ) ;
#5895 = CARTESIAN_POINT ( 'NONE',  ( 10.00000000000000000, 57.87363466993042493, -12.81628187352647608 ) ) ;
#5896 = ORIENTED_EDGE ( 'NONE', *, *, #74548, .T. ) ;
#5897 = CARTESIAN_POINT ( 'NONE',  ( -4.164238869374099039, 46.80374883491397497, 8.674139862899312516E-16 ) ) ;
#5898 =( NAMED_UNIT ( * ) PLANE_ANGLE_UNIT ( ) SI_UNIT ( $, .RADIAN. ) );
#5899 = CARTESIAN_POINT ( 'NONE',  ( 17.96484262340118221, 9.938685344154837509, 7.964842623401181321 ) ) ;
#5900 = CARTESIAN_POINT ( 'NONE',  ( -0.8801773607111008646, 18.27201867748817321, 2.915334737309923430 ) ) ;
#5901 = DIRECTION ( 'NONE',  ( 0.000000000000000000, 1.000000000000000000, 0.000000000000000000 ) ) ;
#5902 = FILL_AREA_STYLE ('',( #75873 ) ) ;
#5903 = CARTESIAN_POINT ( 'NONE',  ( 12.91533473730992121, 54.52201867748816255, 10.88017736071110164 ) ) ;
#5904 = CARTESIAN_POINT ( 'NONE',  ( 15.44008868035555260, 49.73035201082150536, 9.422509992056143702 ) ) ;
#5905 = CARTESIAN_POINT ( 'NONE',  ( 16.40814093676324603, 17.45696800326375353, -11.09922568453594671 ) ) ;
#5906 = FACE_OUTER_BOUND ( 'NONE', #48931, .T. ) ;
#5907 = CARTESIAN_POINT ( 'NONE',  ( 32.56412365047463453, 26.99999999999998224, 10.00000000000000000 ) ) ;
#5908 = CARTESIAN_POINT ( 'NONE',  ( 1.472469842513823179, 25.59226448433412315, -4.923371831947296329 ) ) ;
#5909 = CARTESIAN_POINT ( 'NONE',  ( -0.8801773607111009756, 58.06368534415484106, 1.068504757029289695E-15 ) ) ;
#5910 = STYLED_ITEM ( 'NONE', ( #81472 ), #56452 ) ;
#5911 = AXIS2_PLACEMENT_3D ( 'NONE', #24622, #2132, #91629 ) ;
#5912 = AXIS2_PLACEMENT_3D ( 'NONE', #17568, #11518, #18051 ) ;
#5913 = CARTESIAN_POINT ( 'NONE',  ( 22.81628187352647785, 21.41530133659708923, 3.434112377981063169 ) ) ;
#5914 = CARTESIAN_POINT ( 'NONE',  ( 0.1532563361054083140, 1.008931151000784787, 1.131784320476157264E-15 ) ) ;
#5915 = CARTESIAN_POINT ( 'NONE',  ( 14.92337183194729988, 44.34226448433412315, -8.527530157486177487 ) ) ;
#5916 = CARTESIAN_POINT ( 'NONE',  ( -2.816281873526471635, 43.91530133659708923, -3.434112377981056508 ) ) ;
#5917 = CARTESIAN_POINT ( 'NONE',  ( 10.00000000000000000, 24.75893115100078745, -9.846743663894594434 ) ) ;
#5918 = CARTESIAN_POINT ( 'NONE',  ( 6.204703633549690345, 0.7620821682473009062, -14.16423886937410259 ) ) ;
#5919 = CARTESIAN_POINT ( 'NONE',  ( -8.000000000000000000, 80.99999999999994316, 0.000000000000000000 ) ) ;
#5920 = CARTESIAN_POINT ( 'NONE',  ( 12.91533473730993009, 16.60535201082150891, -10.88017736071109987 ) ) ;
#5922 = CARTESIAN_POINT ( 'NONE',  ( 22.26659068614895176, 29.72041550158063572, -7.082119434687042414 ) ) ;
#5921 = CYLINDRICAL_SURFACE ( 'NONE', #48845, 0.1000000000000000333 ) ;
#5923 = EDGE_CURVE ( 'NONE', #19871, #84722, #88762, .T. ) ;
#5924 = CARTESIAN_POINT ( 'NONE',  ( 7.361572987183170547, 32.05059781766745175, 9.846743663894590881 ) ) ;
#5925 = CARTESIAN_POINT ( 'NONE',  ( 15.44008868035555260, 19.73035201082150536, 9.422509992056143702 ) ) ;
#5927 = CARTESIAN_POINT ( 'NONE',  ( -0.8801773607111008646, 23.27201867748817676, 2.915334737309923430 ) ) ;
#5926 = PRODUCT ( '1.3 Adjustment Nut', '1.3 Adjustment Nut', '', ( #13731 ) ) ;
#5928 = VERTEX_POINT ( 'NONE', #88132 ) ;
#5929 = VECTOR ( 'NONE', #2249, 1000.000000000000000 ) ;
#5930 = CARTESIAN_POINT ( 'NONE',  ( 17.96484262340118221, 26.18868534415483396, -7.964842623401177768 ) ) ;
#5931 = CARTESIAN_POINT ( 'NONE',  ( -1.099225684535947600, 43.70696800326375353, -6.408140936763238038 ) ) ;
#5932 = CARTESIAN_POINT ( 'NONE',  ( 4.559911319644449179, 38.89701867748817676, 9.422509992056141925 ) ) ;
#5934 = CARTESIAN_POINT ( 'NONE',  ( 0.5774900079438607392, 38.48035201082150536, 5.440088680355550821 ) ) ;
#5933 = DIRECTION ( 'NONE',  ( -0.000000000000000000, -0.000000000000000000, 1.000000000000000000 ) ) ;
#5935 = ORIENTED_EDGE ( 'NONE', *, *, #46190, .T. ) ;
#5936 = MECHANICAL_DESIGN_GEOMETRIC_PRESENTATION_REPRESENTATION (  '', ( #49032 ), #61800 ) ;
#5937 = CARTESIAN_POINT ( 'NONE',  ( 18.52753015748618282, 58.92559781766745886, -4.923371831947291888 ) ) ;
#5938 = CARTESIAN_POINT ( 'NONE',  ( 20.88017736071110519, 35.56368534415484106, 2.639326808657452039E-16 ) ) ;
#5939 = CARTESIAN_POINT ( 'NONE',  ( -6.599999999999995204, -97.00000000000000000, -3.750000000000000000 ) ) ;
#5940 = CARTESIAN_POINT ( 'NONE',  ( -10.53011945866294852, -98.59345040283277228, -4.000000000000000000 ) ) ;
#5941 = CARTESIAN_POINT ( 'NONE',  ( -2.816281873526473856, 59.33196800326374643, 3.434112377981055619 ) ) ;
#5942 = CARTESIAN_POINT ( 'NONE',  ( 1.377727649040772586E-15, 2.500000000000005773, 11.25000000000000178 ) ) ;
#5943 = CARTESIAN_POINT ( 'NONE',  ( -2.266590686148945544, 52.22041550158064638, 7.082119434687048631 ) ) ;
#5944 = CARTESIAN_POINT ( 'NONE',  ( 4.559911319644449179, 53.89701867748817676, 9.422509992056141925 ) ) ;
#5945 = CARTESIAN_POINT ( 'NONE',  ( 1.472469842513823179, 66.42559781766745175, 4.923371831947296329 ) ) ;
#5946 = AXIS2_PLACEMENT_3D ( 'NONE', #16920, #55902, #47396 ) ;
#5947 = CARTESIAN_POINT ( 'NONE',  ( -10.91752705534077705, -97.59869434427200474, -3.749999999999999112 ) ) ;
#5948 = CARTESIAN_POINT ( 'NONE',  ( 18.52753015748618282, 53.92559781766745175, -4.923371831947291888 ) ) ;
#5949 = CARTESIAN_POINT ( 'NONE',  ( 7.361572987183169658, 14.96726448433411960, -9.846743663894592657 ) ) ;
#5950 = ORIENTED_EDGE ( 'NONE', *, *, #29158, .T. ) ;
#5951 = CARTESIAN_POINT ( 'NONE',  ( 0.1532563361054082862, 26.21726448433411605, 2.638427012816831674 ) ) ;
#5952 = CARTESIAN_POINT ( 'NONE',  ( 3.469446951953614189E-15, -24.62636533006957507, 12.81628187352647608 ) ) ;
#5953 = CARTESIAN_POINT ( 'NONE',  ( 2.035157376598824452, 28.68868534415484106, 7.964842623401179544 ) ) ;
#5954 = CARTESIAN_POINT ( 'NONE',  ( 5.076628168052703671, 26.84226448433411960, 8.527530157486179263 ) ) ;
#5956 = CARTESIAN_POINT ( 'NONE',  ( 2.035157376598822676, 52.43868534415483396, -7.964842623401177768 ) ) ;
#5955 = CARTESIAN_POINT ( 'NONE',  ( 12.91533473730992121, 64.52201867748817676, 10.88017736071110164 ) ) ;
#5958 = CARTESIAN_POINT ( 'NONE',  ( 19.38216949554541557, 57.24863466993042493, -9.382169495545420901 ) ) ;
#5957 = CARTESIAN_POINT ( 'NONE',  ( -0.8801773607110991993, 37.85535201082151247, -2.915334737309923874 ) ) ;
#5959 = CARTESIAN_POINT ( 'NONE',  ( 13.79529636645031943, 50.34541550158064638, -14.16423886937409904 ) ) ;
#5960 = CARTESIAN_POINT ( 'NONE',  ( -13.34343830728408697, 0.5000000000000004441, 6.852200678592504701 ) ) ;
#5961 = ORIENTED_EDGE ( 'NONE', *, *, #60392, .T. ) ;
#5962 = CARTESIAN_POINT ( 'NONE',  ( 3.591859063236761518, 4.956968003263753531, 11.09922568453594849 ) ) ;
#5963 = CARTESIAN_POINT ( 'NONE',  ( 0.5774900079438590739, 2.647018677488170990, -5.440088680355550821 ) ) ;
#5964 = CARTESIAN_POINT ( 'NONE',  ( 7.084665262690076126, 52.02201867748816255, -10.88017736071110164 ) ) ;
#5965 =( NAMED_UNIT ( * ) SI_UNIT ( $, .STERADIAN. ) SOLID_ANGLE_UNIT ( ) );
#5966 = ORIENTED_EDGE ( 'NONE', *, *, #11212, .T. ) ;
#5967 = CARTESIAN_POINT ( 'NONE',  ( 1.472469842513823179, 16.42559781766745175, 4.923371831947296329 ) ) ;
#5968 = TOROIDAL_SURFACE ( 'NONE', #18749, 14.49999999999999822, 0.5000000000000000000 ) ;
#5969 = CARTESIAN_POINT ( 'NONE',  ( 10.00000000000000000, 56.81368534415484106, -10.88017736071110342 ) ) ;
#5970 = CARTESIAN_POINT ( 'NONE',  ( 19.84674366389459266, 33.30059781766744464, 2.638427012816836559 ) ) ;
#5971 = CARTESIAN_POINT ( 'NONE',  ( 17.20831665107776587, 27.88393115100078390, 7.208316651077764980 ) ) ;
#5972 = CARTESIAN_POINT ( 'NONE',  ( 1.472469842513823179, 16.42559781766745175, 4.923371831947296329 ) ) ;
#5973 = EDGE_CURVE ( 'NONE', #14667, #61835, #64761, .T. ) ;
#5975 = CARTESIAN_POINT ( 'NONE',  ( 22.81628187352647785, 36.62363466993041783, 6.195893100308588602E-16 ) ) ;
#5974 = CARTESIAN_POINT ( 'NONE',  ( -6.617417514236028531, -58.37570470593282579, 2.500000000000000000 ) ) ;
#5978 = CARTESIAN_POINT ( 'NONE',  ( 12.15129255554608534, 15.00000000000000000, 10.40305174771247998 ) ) ;
#5977 = VECTOR ( 'NONE', #25179, 1000.000000000000000 ) ;
#5976 = CARTESIAN_POINT ( 'NONE',  ( 12.91533473730992121, 64.52201867748817676, 10.88017736071110164 ) ) ;
#5979 = CARTESIAN_POINT ( 'NONE',  ( 9.261744320155163024, -15.50732398184953276, 4.000000000000000000 ) ) ;
#5981 = ORIENTED_EDGE ( 'NONE', *, *, #47684, .F. ) ;
#5980 = CARTESIAN_POINT ( 'NONE',  ( 17.20831665107776587, 37.88393115100078745, 7.208316651077764980 ) ) ;
#5982 = AXIS2_PLACEMENT_3D ( 'NONE', #7788, #21803, #82782 ) ;
#5983 = CARTESIAN_POINT ( 'NONE',  ( 16.40814093676323893, 55.79030133659708923, 11.09922568453595026 ) ) ;
#5984 = CARTESIAN_POINT ( 'NONE',  ( 17.39651004071838969, 54.08210964143329846, -6.500000000000027534 ) ) ;
#5985 = CARTESIAN_POINT ( 'NONE',  ( 17.20831665107776587, 64.13393115100079456, -7.208316651077762316 ) ) ;
#5986 = CARTESIAN_POINT ( 'NONE',  ( 0.5774900079438607392, 3.480352010821504027, 5.440088680355550821 ) ) ;
#5987 = CARTESIAN_POINT ( 'NONE',  ( 22.26659068614894466, 13.88708216824730179, 7.082119434687054849 ) ) ;
#5988 = CARTESIAN_POINT ( 'NONE',  ( 24.50000000000000000, 35.99999999999997158, -10.00000000000000000 ) ) ;
#5989 = CARTESIAN_POINT ( 'NONE',  ( 2.917880565312950480, 30.97041550158063572, -12.26659068614894821 ) ) ;
#5990 = CARTESIAN_POINT ( 'NONE',  ( 6.204703633549690345, 42.84541550158063217, 14.16423886937410082 ) ) ;
#5991 = CARTESIAN_POINT ( 'NONE',  ( 6.204703633549690345, 15.76208216824730179, -14.16423886937410259 ) ) ;
#5993 = CARTESIAN_POINT ( 'NONE',  ( 19.42250999205614548, 65.98035201082151957, -5.440088680355545492 ) ) ;
#5992 = CARTESIAN_POINT ( 'NONE',  ( -2.266590686148945544, 16.38708216824730357, -7.082119434687050408 ) ) ;
#5994 = CARTESIAN_POINT ( 'NONE',  ( 20.88017736071110519, 50.56368534415484106, 2.639326808657452039E-16 ) ) ;
#5995 = CARTESIAN_POINT ( 'NONE',  ( 0.4400000000000020006, 1.019547802438468986, -2.500000000000000000 ) ) ;
#5996 = CARTESIAN_POINT ( 'NONE',  ( 5.076628168052703671, 31.84226448433412315, 8.527530157486179263 ) ) ;
#5997 = ADVANCED_FACE ( 'NONE', ( #49157 ), #57637, .T. ) ;
#5999 = CARTESIAN_POINT ( 'NONE',  ( 0.1532563361054100626, 25.80059781766744820, -2.638427012816831230 ) ) ;
#5998 = CARTESIAN_POINT ( 'NONE',  ( 17.96484262340118221, 64.93868534415483396, 7.964842623401181321 ) ) ;
#6000 = CARTESIAN_POINT ( 'NONE',  ( -0.8801773607110991993, 7.855352010821506248, -2.915334737309923874 ) ) ;
#6001 = CARTESIAN_POINT ( 'NONE',  ( -2.816281873526473856, 64.33196800326376774, 3.434112377981055619 ) ) ;
#6002 = CARTESIAN_POINT ( 'NONE',  ( 2.791683348922240793, 51.63393115100078745, 7.208316651077764092 ) ) ;
#6003 = CARTESIAN_POINT ( 'NONE',  ( 0.1532563361054082862, 26.21726448433411605, 2.638427012816831674 ) ) ;
#6004 = CARTESIAN_POINT ( 'NONE',  ( -2.816281873526473856, 44.12363466993042493, 9.499525473075851096E-16 ) ) ;
#6005 = CARTESIAN_POINT ( 'NONE',  ( 12.26659068614894466, -20.27958449841936073, -7.082119434687053960 ) ) ;
#6006 = CARTESIAN_POINT ( 'NONE',  ( 15.44008868035555260, 39.73035201082150536, 9.422509992056143702 ) ) ;
#6007 = CARTESIAN_POINT ( 'NONE',  ( 12.63842701281683034, 42.46726448433412315, 9.846743663894596210 ) ) ;
#6008 = EDGE_CURVE ( 'NONE', #65472, #14954, #19310, .T. ) ;
#6009 = CARTESIAN_POINT ( 'NONE',  ( 10.00000000000000178, 28.05374883491396787, 14.16423886937410082 ) ) ;
#6010 = ORIENTED_EDGE ( 'NONE', *, *, #68078, .T. ) ;
#6011 = CARTESIAN_POINT ( 'NONE',  ( 22.26659068614894466, 3.887082168247300906, 7.082119434687054849 ) ) ;
#6012 = EDGE_CURVE ( 'NONE', #55863, #70171, #56003, .T. ) ;
#6013 = AXIS2_PLACEMENT_3D ( 'NONE', #63863, #34354, #33853 ) ;
#6014 = CARTESIAN_POINT ( 'NONE',  ( 20.88017736071110519, 50.56368534415484106, 2.639326808657452039E-16 ) ) ;
#6015 = CARTESIAN_POINT ( 'NONE',  ( 19.42250999205614193, 60.14701867748817676, 5.440088680355555262 ) ) ;
#6016 = CARTESIAN_POINT ( 'NONE',  ( 6.204703633549690345, 60.76208216824730357, -14.16423886937410259 ) ) ;
#6017 = CARTESIAN_POINT ( 'NONE',  ( 6.565887622018943937, 3.081968003263753531, -12.81628187352647608 ) ) ;
#6018 = CARTESIAN_POINT ( 'NONE',  ( -0.1042174387088606741, 53.10736173766203905, 6.337391062633418670 ) ) ;
#6019 = CARTESIAN_POINT ( 'NONE',  ( 19.42250999205614548, 60.98035201082151247, -5.440088680355545492 ) ) ;
#6020 = CARTESIAN_POINT ( 'NONE',  ( 21.09922568453594849, 1.206968003263753531, 6.408140936763242479 ) ) ;
#6021 = CARTESIAN_POINT ( 'NONE',  ( -7.964842623401179544, 27.43868534415484461, -7.964842623401174215 ) ) ;
#6022 = CARTESIAN_POINT ( 'NONE',  ( 17.96484262340118221, 9.938685344154837509, 7.964842623401181321 ) ) ;
#6023 = CARTESIAN_POINT ( 'NONE',  ( 19.42250999205614193, 10.14701867748816966, 5.440088680355555262 ) ) ;
#6024 = CARTESIAN_POINT ( 'NONE',  ( 12.63842701281683034, 47.46726448433412315, 9.846743663894596210 ) ) ;
#6025 = LINE ( 'NONE', #59992, #61549 ) ;
#6026 = ORIENTED_EDGE ( 'NONE', *, *, #28276, .F. ) ;
#6027 = SURFACE_SIDE_STYLE ('',( #49531 ) ) ;
#6028 = CARTESIAN_POINT ( 'NONE',  ( 21.09922568453595559, 7.040301336597086568, -6.408140936763230044 ) ) ;
#6029 = CARTESIAN_POINT ( 'NONE',  ( 0.5600000000000083800, 105.0000000000000000, 5.000000000000000000 ) ) ;
#6030 = CARTESIAN_POINT ( 'NONE',  ( 5.076628168052704559, 5.175597817667451750, -8.527530157486179263 ) ) ;
#6031 = CARTESIAN_POINT ( 'NONE',  ( 0.1532563361054083140, 41.00893115100078745, 1.131784320476157264E-15 ) ) ;
#6032 = CARTESIAN_POINT ( 'NONE',  ( 20.88017736071110519, 40.56368534415484106, 2.639326808657452039E-16 ) ) ;
#6033 = B_SPLINE_CURVE_WITH_KNOTS ( 'NONE', 3,
 ( #39635, #18113, #34066, #71607 ),
 .UNSPECIFIED., .F., .F.,
 ( 4, 4 ),
 ( 2.168404344971008868E-18, 0.001060528352562004149 ),
 .UNSPECIFIED. ) ;
#6034 = CARTESIAN_POINT ( 'NONE',  ( 3.591859063236763294, 3.290301336597087012, -11.09922568453595026 ) ) ;
#6036 = LINE ( 'NONE', #44513, #17694 ) ;
#6035 = CARTESIAN_POINT ( 'NONE',  ( 19.42250999205614193, 50.14701867748817676, 5.440088680355555262 ) ) ;
#6037 = CARTESIAN_POINT ( 'NONE',  ( 19.38216949554541557, 47.24863466993041783, -9.382169495545420901 ) ) ;
#6038 = VERTEX_POINT ( 'NONE', #81127 ) ;
#6039 = CARTESIAN_POINT ( 'NONE',  ( 7.084665262690076126, 69.10535201082151957, 10.88017736071109987 ) ) ;
#6040 = CARTESIAN_POINT ( 'NONE',  ( 16.40814093676324603, 37.45696800326376064, -11.09922568453594671 ) ) ;
#6041 = ADVANCED_FACE ( 'NONE', ( #43128 ), #98366, .T. ) ;
#6042 = CARTESIAN_POINT ( 'NONE',  ( 7.361572987183170547, 2.050597817667451750, 9.846743663894590881 ) ) ;
#6043 = CARTESIAN_POINT ( 'NONE',  ( 7.084665262690076126, 39.10535201082150536, 10.88017736071109987 ) ) ;
#6044 = CARTESIAN_POINT ( 'NONE',  ( 7.361572987183169658, 64.96726448433412315, -9.846743663894592657 ) ) ;
#6045 = CIRCLE ( 'NONE', #33134, 0.5000000000000000000 ) ;
#6046 = CARTESIAN_POINT ( 'NONE',  ( 18.52753015748618282, 58.92559781766745886, -4.923371831947291888 ) ) ;
#6047 = CARTESIAN_POINT ( 'NONE',  ( 1.472469842513823179, 21.42559781766745175, 4.923371831947296329 ) ) ;
#6048 = CARTESIAN_POINT ( 'NONE',  ( 1.472469842513823179, 1.425597817667451528, 4.923371831947296329 ) ) ;
#6049 = CARTESIAN_POINT ( 'NONE',  ( 13.07751017357383994, 4.340377266345630487E-16, -6.263284095430506682 ) ) ;
#6050 = CARTESIAN_POINT ( 'NONE',  ( 13.79529636645030344, 48.26208216824728936, 14.16423886937410614 ) ) ;
#6051 = CARTESIAN_POINT ( 'NONE',  ( -14.29730467490344736, 15.00000000000000000, 2.416004766801328696 ) ) ;
#6052 = CARTESIAN_POINT ( 'NONE',  ( 11.43652560662874507, -81.64049707262192612, -3.749999999999999112 ) ) ;
#6053 = AXIS2_PLACEMENT_3D ( 'NONE', #16267, #78731, #15780 ) ;
#6054 = ORIENTED_EDGE ( 'NONE', *, *, #17895, .T. ) ;
#6055 = CARTESIAN_POINT ( 'NONE',  ( 6.204703633549690345, 55.76208216824730357, -14.16423886937410259 ) ) ;
#6056 = CARTESIAN_POINT ( 'NONE',  ( 2.917880565312950480, 65.97041550158063217, -12.26659068614894821 ) ) ;
#6057 = CARTESIAN_POINT ( 'NONE',  ( 7.361572987183170547, 32.05059781766745175, 9.846743663894590881 ) ) ;
#6058 = CARTESIAN_POINT ( 'NONE',  ( -13.69999999999999751, 99.99999999999998579, -8.525133428036873795 ) ) ;
#6060 = CARTESIAN_POINT ( 'NONE',  ( -4.164238869374098151, 11.59541550158063217, -3.795296366450310543 ) ) ;
#6059 =( NAMED_UNIT ( * ) PLANE_ANGLE_UNIT ( ) SI_UNIT ( $, .RADIAN. ) );
#6061 = CARTESIAN_POINT ( 'NONE',  ( 12.91533473730992121, 9.522018677488171434, 10.88017736071110164 ) ) ;
#6062 = CARTESIAN_POINT ( 'NONE',  ( 22.26659068614895176, 54.72041550158063217, -7.082119434687042414 ) ) ;
#6063 = CARTESIAN_POINT ( 'NONE',  ( 1.472469842513823179, 30.59226448433411960, -4.923371831947296329 ) ) ;
#6064 = PLANE ( 'NONE',  #71575 ) ;
#6065 = CARTESIAN_POINT ( 'NONE',  ( 18.52753015748618282, 8.925597817667451750, -4.923371831947291888 ) ) ;
#6066 = CARTESIAN_POINT ( 'NONE',  ( 18.72515096720571037, 55.05509018479936145, 6.499999999999982236 ) ) ;
#6067 = CARTESIAN_POINT ( 'NONE',  ( -2.638427012816824124, 17.05059781766745530, 9.846743663894596210 ) ) ;
#6068 = VERTEX_POINT ( 'NONE', #72145 ) ;
#6069 = EDGE_LOOP ( 'NONE', ( #37105, #93758, #9070, #87712 ) ) ;
#6070 = CARTESIAN_POINT ( 'NONE',  ( 1.236355250167371800, 14.95037107271117982, -14.70131747622448515 ) ) ;
#6071 = EDGE_LOOP ( 'NONE', ( #98466, #96969, #7617, #47754 ) ) ;
#6072 = CARTESIAN_POINT ( 'NONE',  ( 17.20831665107776587, 42.88393115100077324, 7.208316651077764980 ) ) ;
#6074 = CARTESIAN_POINT ( 'NONE',  ( 17.96484262340118221, 24.93868534415484461, 7.964842623401181321 ) ) ;
#6073 = CARTESIAN_POINT ( 'NONE',  ( 4.559911319644449179, 23.89701867748817321, 9.422509992056141925 ) ) ;
#6076 = CARTESIAN_POINT ( 'NONE',  ( 10.00000000000000000, 12.87363466993042138, -12.81628187352647608 ) ) ;
#6075 = CARTESIAN_POINT ( 'NONE',  ( 0.1532563361054100626, 60.80059781766744464, -2.638427012816831230 ) ) ;
#6077 = CARTESIAN_POINT ( 'NONE',  ( -2.266590686148945544, 6.387082168247300906, -7.082119434687050408 ) ) ;
#6078 = B_SPLINE_CURVE_WITH_KNOTS ( 'NONE', 3,
 ( #59617, #98649, #36641, #67124, #51639, #15131 ),
 .UNSPECIFIED., .F., .F.,
 ( 4, 2, 4 ),
 ( 3.409110551496073092E-05, 0.0004400426677367845658, 0.0008459942299586083398 ),
 .UNSPECIFIED. ) ;
#6079 = CARTESIAN_POINT ( 'NONE',  ( 3.591859063236761518, 29.95696800326375708, 11.09922568453594849 ) ) ;
#6080 = EDGE_LOOP ( 'NONE', ( #21462, #10142, #42837, #199 ) ) ;
#6081 = CARTESIAN_POINT ( 'NONE',  ( 17.20831665107776587, 34.13393115100078745, -7.208316651077762316 ) ) ;
#6082 = CARTESIAN_POINT ( 'NONE',  ( 20.88017736071110519, 10.56368534415483929, 2.639326808657452039E-16 ) ) ;
#6083 = ORIENTED_EDGE ( 'NONE', *, *, #26901, .T. ) ;
#6084 = CARTESIAN_POINT ( 'NONE',  ( 20.88017736071110164, 5.355352010821503583, 2.915334737309930979 ) ) ;
#6085 = ORIENTED_EDGE ( 'NONE', *, *, #65380, .F. ) ;
#6086 = CARTESIAN_POINT ( 'NONE',  ( -0.8801773607110991993, 47.85535201082150536, -2.915334737309923874 ) ) ;
#6087 = CARTESIAN_POINT ( 'NONE',  ( 4.559911319644449179, 62.23035201082150536, -9.422509992056141925 ) ) ;
#6089 = EDGE_CURVE ( 'NONE', #72594, #61531, #72629, .T. ) ;
#6088 = CARTESIAN_POINT ( 'NONE',  ( -0.8801773607111009756, 48.06368534415484817, 1.068504757029289695E-15 ) ) ;
#6090 = FACE_OUTER_BOUND ( 'NONE', #59272, .T. ) ;
#6091 = CARTESIAN_POINT ( 'NONE',  ( 4.559911319644449179, 58.89701867748817676, 9.422509992056141925 ) ) ;
#6092 = CARTESIAN_POINT ( 'NONE',  ( -0.3289641300568005855, 30.10497603579417714, 5.963430220938281678 ) ) ;
#6093 = EDGE_CURVE ( 'NONE', #37275, #74987, #90320, .T. ) ;
#6094 = AXIS2_PLACEMENT_3D ( 'NONE', #88938, #89430, #29899 ) ;
#6095 = CARTESIAN_POINT ( 'NONE',  ( 1.472469842513823179, 31.42559781766745530, 4.923371831947296329 ) ) ;
#6096 = ORIENTED_EDGE ( 'NONE', *, *, #42064, .T. ) ;
#6097 = CARTESIAN_POINT ( 'NONE',  ( 10.00000000000000000, 59.75893115100078745, -9.846743663894594434 ) ) ;
#6098 = DIRECTION ( 'NONE',  ( 0.000000000000000000, -1.000000000000000000, 0.000000000000000000 ) ) ;
#6099 = CARTESIAN_POINT ( 'NONE',  ( 2.917880565312948704, 12.63708216824730179, 12.26659068614894643 ) ) ;
#6100 = AXIS2_PLACEMENT_3D ( 'NONE', #3155, #41652, #40164 ) ;
#6101 = VERTEX_POINT ( 'NONE', #23973 ) ;
#6102 = SURFACE_STYLE_USAGE ( .BOTH. , #6588 ) ;
#6103 = CARTESIAN_POINT ( 'NONE',  ( -6.030800153576633349, -39.80424705863364920, 3.750000000000001332 ) ) ;
#6104 = CARTESIAN_POINT ( 'NONE',  ( -7.595945211628411187, 15.00000000000000000, 12.35117874301633734 ) ) ;
#6105 = CARTESIAN_POINT ( 'NONE',  ( 4.559911319644449179, 2.230352010821504916, -9.422509992056141925 ) ) ;
#6106 = LINE ( 'NONE', #21611, #17970 ) ;
#6107 = VERTEX_POINT ( 'NONE', #8466 ) ;
#6108 = DIRECTION ( 'NONE',  ( -4.606671024408299627E-17, -2.115048048893883575E-15, -1.000000000000000000 ) ) ;
#6109 = CARTESIAN_POINT ( 'NONE',  ( 7.361572987183169658, 39.96726448433411605, -9.846743663894592657 ) ) ;
#6110 = DIRECTION ( 'NONE',  ( 0.8870108331782213806, 0.000000000000000000, -0.4617486132350345773 ) ) ;
#6111 = CARTESIAN_POINT ( 'NONE',  ( 21.09922568453594849, 16.20696800326375353, 6.408140936763242479 ) ) ;
#6112 = CARTESIAN_POINT ( 'NONE',  ( 2.791683348922240793, 16.63393115100078745, 7.208316651077764092 ) ) ;
#6113 = AXIS2_PLACEMENT_3D ( 'NONE', #45266, #91755, #10715 ) ;
#6114 = DIRECTION ( 'NONE',  ( 0.000000000000000000, 0.000000000000000000, -1.000000000000000000 ) ) ;
#6115 = CARTESIAN_POINT ( 'NONE',  ( -2.816281873526473856, 4.123634669930420493, 9.499525473075851096E-16 ) ) ;
#6116 = EDGE_CURVE ( 'NONE', #84655, #12575, #23277, .T. ) ;
#6117 = ORIENTED_EDGE ( 'NONE', *, *, #3759, .F. ) ;
#6118 = EDGE_CURVE ( 'NONE', #66530, #50127, #36633, .T. ) ;
#6119 = CARTESIAN_POINT ( 'NONE',  ( 0.5774900079438590739, 12.64701867748817321, -5.440088680355550821 ) ) ;
#6120 = CARTESIAN_POINT ( 'NONE',  ( -0.3689425029237898834, 6.178748834913968757, -10.36894250292378850 ) ) ;
#6121 = CARTESIAN_POINT ( 'NONE',  ( 1.472469842513823179, 21.42559781766745175, 4.923371831947296329 ) ) ;
#6122 = CARTESIAN_POINT ( 'NONE',  ( 19.42250999205614193, 55.14701867748817676, 5.440088680355555262 ) ) ;
#6124 = SURFACE_STYLE_FILL_AREA ( #51122 ) ;
#6123 = CARTESIAN_POINT ( 'NONE',  ( 22.81628187352647785, 41.62363466993042493, 6.195893100308588602E-16 ) ) ;
#6125 = CARTESIAN_POINT ( 'NONE',  ( 7.084665262690076126, 9.105352010821503583, 10.88017736071109987 ) ) ;
#6126 = DIRECTION ( 'NONE',  ( -1.000000000000000000, -0.000000000000000000, -0.000000000000000000 ) ) ;
#6127 = DIRECTION ( 'NONE',  ( 0.9723699203976789995, 0.000000000000000000, -0.2334453638558957045 ) ) ;
#6128 = PRODUCT ( '1.1 Cage', '1.1 Cage', '', ( #23222 ) ) ;
#6129 = CARTESIAN_POINT ( 'NONE',  ( 0.6178305044545818747, 3.498634669930420049, -9.382169495545419124 ) ) ;
#6130 = CARTESIAN_POINT ( 'NONE',  ( 5.076628168052704559, 65.17559781766745175, -8.527530157486179263 ) ) ;
#6131 = CARTESIAN_POINT ( 'NONE',  ( 12.63842701281683034, 27.46726448433411250, 9.846743663894596210 ) ) ;
#6132 = CARTESIAN_POINT ( 'NONE',  ( 5.440088680355556150, -5.269647989178491088, 9.422509992056138373 ) ) ;
#6133 = CARTESIAN_POINT ( 'NONE',  ( 16.40814093676323893, 30.79030133659708923, 11.09922568453595026 ) ) ;
#6134 =( NAMED_UNIT ( * ) SI_UNIT ( $, .STERADIAN. ) SOLID_ANGLE_UNIT ( ) );
#6136 = CARTESIAN_POINT ( 'NONE',  ( 4.862001128006773421, 4.807100664002271835E-16, -13.66056166602460031 ) ) ;
#6135 = CARTESIAN_POINT ( 'NONE',  ( 20.88017736071110519, 45.56368534415484106, 2.639326808657452039E-16 ) ) ;
#6137 = DIRECTION ( 'NONE',  ( 0.000000000000000000, -1.000000000000000000, 0.000000000000000000 ) ) ;
#6138 =( BOUNDED_CURVE ( )  B_SPLINE_CURVE ( 2, ( #34182, #57188, #80186, #42208, #89171 ),
 .UNSPECIFIED., .F., .F. ) 
 B_SPLINE_CURVE_WITH_KNOTS ( ( 3, 2, 3 ),
 ( 0.9401409369402312644, 0.9404761904761904656, 0.9419949716883659896 ),
 .UNSPECIFIED. ) 
 CURVE ( )  GEOMETRIC_REPRESENTATION_ITEM ( )  RATIONAL_B_SPLINE_CURVE ( ( 0.9963778908391753841, 0.9980808541467917072, 1.000000000000000000, 0.9913057959047685275, 0.9870483353379817526 ) ) 
 REPRESENTATION_ITEM ( '' )  );
#6139 = CARTESIAN_POINT ( 'NONE',  ( 20.88017736071110519, 45.56368534415484106, 2.639326808657452039E-16 ) ) ;
#6140 = CARTESIAN_POINT ( 'NONE',  ( 2.035157376598822676, 32.43868534415483396, -7.964842623401177768 ) ) ;
#6141 = CARTESIAN_POINT ( 'NONE',  ( 1.472469842513823179, 61.42559781766745175, 4.923371831947296329 ) ) ;
#6142 = CARTESIAN_POINT ( 'NONE',  ( 17.96484262340118221, 59.93868534415484106, 7.964842623401181321 ) ) ;
#6143 = EDGE_CURVE ( 'NONE', #10324, #49672, #16466, .T. ) ;
#6144 = CARTESIAN_POINT ( 'NONE',  ( 19.84674366389459266, 33.30059781766744464, 2.638427012816836559 ) ) ;
#6145 = CARTESIAN_POINT ( 'NONE',  ( -40.17076923076924544, 96.15384615384614619, -9.500000000000000000 ) ) ;
#6146 = CARTESIAN_POINT ( 'NONE',  ( 22.81628187352647785, 16.41530133659708923, 3.434112377981063169 ) ) ;
#6147 = ORIENTED_EDGE ( 'NONE', *, *, #58991, .T. ) ;
#6148 = CARTESIAN_POINT ( 'NONE',  ( 20.88017736071110519, 20.56368534415484106, 2.639326808657452039E-16 ) ) ;
#6149 = CARTESIAN_POINT ( 'NONE',  ( 4.559911319644449179, 12.23035201082150714, -9.422509992056141925 ) ) ;
#6150 = CARTESIAN_POINT ( 'NONE',  ( 14.92337183194729988, 4.342264484334117824, -8.527530157486177487 ) ) ;
#6151 = CARTESIAN_POINT ( 'NONE',  ( -4.164238869374098151, 26.59541550158063217, -3.795296366450310543 ) ) ;
#6152 = CARTESIAN_POINT ( 'NONE',  ( 7.361572987183170547, 12.05059781766744997, 9.846743663894590881 ) ) ;
#6153 = CARTESIAN_POINT ( 'NONE',  ( 17.20831665107776587, 62.88393115100078745, 7.208316651077764980 ) ) ;
#6154 = CARTESIAN_POINT ( 'NONE',  ( 2.035157376598822676, 47.43868534415484817, -7.964842623401177768 ) ) ;
#6155 = LINE ( 'NONE', #21160, #74563 ) ;
#6156 = FACE_OUTER_BOUND ( 'NONE', #93578, .T. ) ;
#6157 = ORIENTED_EDGE ( 'NONE', *, *, #94629, .T. ) ;
#6158 = MECHANICAL_DESIGN_GEOMETRIC_PRESENTATION_REPRESENTATION (  '', ( #54048 ), #79609 ) ;
#6159 = CARTESIAN_POINT ( 'NONE',  ( 5.429172911446037197, -28.64165983034504137, 2.499999999999999556 ) ) ;
#6160 = CARTESIAN_POINT ( 'NONE',  ( 19.84674366389459266, 48.30059781766745175, 2.638427012816836559 ) ) ;
#6161 = ORIENTED_EDGE ( 'NONE', *, *, #86978, .F. ) ;
#6162 = ORIENTED_EDGE ( 'NONE', *, *, #19398, .F. ) ;
#6163 = CARTESIAN_POINT ( 'NONE',  ( 0.000000000000000000, -97.00000000000000000, -3.750000000000000000 ) ) ;
#6164 = CARTESIAN_POINT ( 'NONE',  ( 6.204703633549690345, 20.76208216824730357, -14.16423886937410259 ) ) ;
#6165 = CARTESIAN_POINT ( 'NONE',  ( -4.164238869374099039, 21.80374883491396787, 8.674139862899312516E-16 ) ) ;
#6166 = CARTESIAN_POINT ( 'NONE',  ( 7.084665262690076126, 59.10535201082150536, 10.88017736071109987 ) ) ;
#6167 = CARTESIAN_POINT ( 'NONE',  ( -0.8801773607111009756, 3.063685344154838397, 1.068504757029289695E-15 ) ) ;
#6168 = CARTESIAN_POINT ( 'NONE',  ( -2.816281873526473856, 4.331968003263754419, 3.434112377981055619 ) ) ;
#6169 = CARTESIAN_POINT ( 'NONE',  ( 7.361572987183169658, 49.96726448433410894, -9.846743663894592657 ) ) ;
#6170 = CARTESIAN_POINT ( 'NONE',  ( -7.750000000000000000, 40.74999999999999289, -4.250000000000000000 ) ) ;
#6172 = CARTESIAN_POINT ( 'NONE',  ( 21.09922568453595559, 2.040301336597086568, -6.408140936763230044 ) ) ;
#6171 = CARTESIAN_POINT ( 'NONE',  ( -0.8801773607110991993, 47.85535201082150536, -2.915334737309923874 ) ) ;
#6173 = CARTESIAN_POINT ( 'NONE',  ( -4.164238869374099039, 16.80374883491396787, 8.674139862899312516E-16 ) ) ;
#6174 = CARTESIAN_POINT ( 'NONE',  ( 17.96484262340118221, 19.93868534415484106, 7.964842623401181321 ) ) ;
#6175 = CARTESIAN_POINT ( 'NONE',  ( 2.035157376598822676, 12.43868534415483751, -7.964842623401177768 ) ) ;
#6176 = CARTESIAN_POINT ( 'NONE',  ( 4.380000000000002558, 1.019547802438462547, -2.500000000000000000 ) ) ;
#6177 = CARTESIAN_POINT ( 'NONE',  ( 2.035157376598824452, 43.68868534415484106, 7.964842623401179544 ) ) ;
#6178 =( GEOMETRIC_REPRESENTATION_CONTEXT ( 3 ) GLOBAL_UNCERTAINTY_ASSIGNED_CONTEXT ( ( #39237 ) ) GLOBAL_UNIT_ASSIGNED_CONTEXT ( ( #47414, #69936, #55418 ) ) REPRESENTATION_CONTEXT ( 'NONE', 'WORKASPACE' ) );
#6179 = CARTESIAN_POINT ( 'NONE',  ( 13.43411237798105340, 45.58196800326374643, 12.81628187352647963 ) ) ;
#6180 = CARTESIAN_POINT ( 'NONE',  ( 7.208316651077764980, -22.11606884899921610, 7.208316651077762316 ) ) ;
#6181 = VERTEX_POINT ( 'NONE', #60094 ) ;
#6182 = CARTESIAN_POINT ( 'NONE',  ( 20.10493008474208665, 4.716974130838791801, 6.336235997365754713 ) ) ;
#6183 = ORIENTED_EDGE ( 'NONE', *, *, #71947, .F. ) ;
#6184 = CARTESIAN_POINT ( 'NONE',  ( 1.472469842513823179, 30.59226448433411960, -4.923371831947296329 ) ) ;
#6185 = ORIENTED_EDGE ( 'NONE', *, *, #74797, .F. ) ;
#6186 = DIRECTION ( 'NONE',  ( 0.000000000000000000, 0.000000000000000000, 1.000000000000000000 ) ) ;
#6188 = CARTESIAN_POINT ( 'NONE',  ( 10.00000000000000178, 4.313685344154837509, 10.88017736071110342 ) ) ;
#6187 = CARTESIAN_POINT ( 'NONE',  ( -2.266590686148945544, 47.22041550158063927, 7.082119434687048631 ) ) ;
#6190 = CARTESIAN_POINT ( 'NONE',  ( 5.076628168052704559, 50.17559781766745886, -8.527530157486179263 ) ) ;
#6189 = CARTESIAN_POINT ( 'NONE',  ( 17.20831665107776587, 27.88393115100078390, 7.208316651077764980 ) ) ;
#6191 = LINE ( 'NONE', #82675, #29461 ) ;
#6192 = TOROIDAL_SURFACE ( 'NONE', #62051, 14.49999999999999822, 0.5000000000000000000 ) ;
#6193 = CARTESIAN_POINT ( 'NONE',  ( 24.35999999999999233, 37.99999999999997868, -10.00000000000000000 ) ) ;
#6194 = TOROIDAL_SURFACE ( 'NONE', #28522, 3.250000000000001332, 0.2500000000000000000 ) ;
#6195 = CARTESIAN_POINT ( 'NONE',  ( 1.472469842513823179, 0.5922644843341181575, -4.923371831947296329 ) ) ;
#6196 = CARTESIAN_POINT ( 'NONE',  ( 3.434112377981054287, 27.66530133659709279, -12.81628187352647608 ) ) ;
#6197 = ORIENTED_EDGE ( 'NONE', *, *, #11929, .F. ) ;
#6198 = CARTESIAN_POINT ( 'NONE',  ( -0.3689425029237881626, 32.42874883491395366, 10.36894250292379027 ) ) ;
#6199 = CARTESIAN_POINT ( 'NONE',  ( 6.565887622018943937, 28.08196800326375353, -12.81628187352647608 ) ) ;
#6200 = ORIENTED_EDGE ( 'NONE', *, *, #28772, .T. ) ;
#6201 = CARTESIAN_POINT ( 'NONE',  ( 10.00000000000000000, 47.87363466993042493, -12.81628187352647608 ) ) ;
#6202 = CARTESIAN_POINT ( 'NONE',  ( 17.96484262340118221, 14.93868534415484106, 7.964842623401181321 ) ) ;
#6203 = CARTESIAN_POINT ( 'NONE',  ( 7.361572987183170547, 32.05059781766745175, 9.846743663894590881 ) ) ;
#6204 = CARTESIAN_POINT ( 'NONE',  ( -0.8801773607110991993, 17.85535201082150536, -2.915334737309923874 ) ) ;
#6205 = CARTESIAN_POINT ( 'NONE',  ( 11.49999999999999645, 75.00000000000000000, 6.500000000000000888 ) ) ;
#6206 = PLANE ( 'NONE',  #46385 ) ;
#6207 = CARTESIAN_POINT ( 'NONE',  ( 5.076628168052703671, 46.84226448433412315, 8.527530157486179263 ) ) ;
#6208 = CARTESIAN_POINT ( 'NONE',  ( 1.472469842513823179, 50.59226448433411605, -4.923371831947296329 ) ) ;
#6209 = ADVANCED_FACE ( 'NONE', ( #67117 ), #90107, .F. ) ;
#6211 = ORIENTED_EDGE ( 'NONE', *, *, #22377, .F. ) ;
#6210 = CARTESIAN_POINT ( 'NONE',  ( -1.087200977609927843, 0.000000000000000000, -5.343763529286924552 ) ) ;
#6212 = CARTESIAN_POINT ( 'NONE',  ( -13.55255535720589322, 0.000000000000000000, -4.403492169843143067 ) ) ;
#6213 = DIRECTION ( 'NONE',  ( -0.9238795325112876267, 0.000000000000000000, -0.3826834323650877279 ) ) ;
#6214 = CARTESIAN_POINT ( 'NONE',  ( -4.000000000000000000, 37.00000000000000000, -3.750000000000000000 ) ) ;
#6215 = SURFACE_SIDE_STYLE ('',( #38203 ) ) ;
#6216 = CARTESIAN_POINT ( 'NONE',  ( 14.92337183194729988, 19.34226448433411960, -8.527530157486177487 ) ) ;
#6217 = CARTESIAN_POINT ( 'NONE',  ( 13.43411237798105340, 40.58196800326375353, 12.81628187352647963 ) ) ;
#6218 = CARTESIAN_POINT ( 'NONE',  ( 3.897244926435189161, 15.00000000000000000, 13.96644127842154148 ) ) ;
#6219 = ORIENTED_EDGE ( 'NONE', *, *, #72351, .T. ) ;
#6220 = CIRCLE ( 'NONE', #74881, 1.249999999999987121 ) ;
#6221 = CARTESIAN_POINT ( 'NONE',  ( 0.1532563361054083140, 56.00893115100078745, 1.131784320476157264E-15 ) ) ;
#6222 = CARTESIAN_POINT ( 'NONE',  ( 17.39651004071841811, 4.082109641433293135, -6.499999999999999112 ) ) ;
#6223 = CARTESIAN_POINT ( 'NONE',  ( 22.26659068614895176, 29.72041550158063572, -7.082119434687042414 ) ) ;
#6224 = CARTESIAN_POINT ( 'NONE',  ( 2.791683348922240793, 41.63393115100078745, 7.208316651077764092 ) ) ;
#6225 = CARTESIAN_POINT ( 'NONE',  ( 22.81628187352647785, 46.41530133659708213, 3.434112377981063169 ) ) ;
#6226 = B_SPLINE_CURVE_WITH_KNOTS ( 'NONE', 3,
 ( #38452, #38943, #7956, #31414, #83943, #23946 ),
 .UNSPECIFIED., .F., .F.,
 ( 4, 2, 4 ),
 ( 3.409110551495695654E-05, 0.0004400426677367964921, 0.0008459942299586360953 ),
 .UNSPECIFIED. ) ;
#6228 = CARTESIAN_POINT ( 'NONE',  ( 8.721827932831768493, -3.224654430197120208E-15, 11.74045266257181375 ) ) ;
#6227 = PLANE ( 'NONE',  #43194 ) ;
#6229 = CARTESIAN_POINT ( 'NONE',  ( 17.20831665107776587, 2.883931151000785231, 7.208316651077764980 ) ) ;
#6230 = CARTESIAN_POINT ( 'NONE',  ( -10.93781366033333136, 0.5000000000000004441, -10.26470809774080628 ) ) ;
#6231 = CARTESIAN_POINT ( 'NONE',  ( 12.63842701281683034, 47.46726448433412315, 9.846743663894596210 ) ) ;
#6232 = CARTESIAN_POINT ( 'NONE',  ( -0.8801773607111009756, 38.06368534415484106, 1.068504757029289695E-15 ) ) ;
#6233 = CARTESIAN_POINT ( 'NONE',  ( 19.50000000000000711, 105.0000000000000000, 5.000000000000000000 ) ) ;
#6234 = EDGE_CURVE ( 'NONE', #86532, #77069, #8953, .T. ) ;
#6235 = CARTESIAN_POINT ( 'NONE',  ( 2.035157376598824452, 43.68868534415484106, 7.964842623401179544 ) ) ;
#6236 = EDGE_LOOP ( 'NONE', ( #68174, #77554, #41484, #96842 ) ) ;
#6237 = EDGE_CURVE ( 'NONE', #43424, #85655, #91911, .T. ) ;
#6238 = DIRECTION ( 'NONE',  ( -1.000000000000000000, -2.799047438454523236E-16, 0.000000000000000000 ) ) ;
#6239 = CARTESIAN_POINT ( 'NONE',  ( 20.88017736071110164, 10.35535201082150714, 2.915334737309930979 ) ) ;
#6241 = CARTESIAN_POINT ( 'NONE',  ( 10.00000000000000178, 44.31368534415484106, 10.88017736071110342 ) ) ;
#6240 = CARTESIAN_POINT ( 'NONE',  ( 1.472469842513823179, 61.42559781766745175, 4.923371831947296329 ) ) ;
#6242 = CARTESIAN_POINT ( 'NONE',  ( 4.559911319644449179, 63.89701867748817676, 9.422509992056141925 ) ) ;
#6243 = CARTESIAN_POINT ( 'NONE',  ( -8.000000000000000000, 83.99999999999994316, 3.000000000000000000 ) ) ;
#6245 = CARTESIAN_POINT ( 'NONE',  ( 8.879999999999991900, 76.07179676972447169, -6.250000000000000000 ) ) ;
#6244 = CARTESIAN_POINT ( 'NONE',  ( 4.559911319644449179, 22.23035201082150536, -9.422509992056141925 ) ) ;
#6246 = CARTESIAN_POINT ( 'NONE',  ( 19.84674366389459621, 13.50893115100078568, 7.409399052514197653E-17 ) ) ;
#6247 = CARTESIAN_POINT ( 'NONE',  ( 17.20831665107776587, 19.13393115100078035, -7.208316651077762316 ) ) ;
#6248 = CARTESIAN_POINT ( 'NONE',  ( 1.796645268984623511, 0.2306972965111892537, 14.83273813124059615 ) ) ;
#6249 = CARTESIAN_POINT ( 'NONE',  ( -5.204170427930421283E-15, 15.55374883491396965, -14.16423886937410082 ) ) ;
#6250 = CARTESIAN_POINT ( 'NONE',  ( 2.791683348922237240, 65.38393115100078035, -7.208316651077763204 ) ) ;
#6251 = CARTESIAN_POINT ( 'NONE',  ( -0.8801773607111009756, 3.063685344154838397, 1.068504757029289695E-15 ) ) ;
#6252 = CARTESIAN_POINT ( 'NONE',  ( -3.749999999999988010, -5.564482262735336175E-16, -4.250000000000000000 ) ) ;
#6253 = CARTESIAN_POINT ( 'NONE',  ( 24.16423886937410614, 9.512082168247301794, -3.795296366450302550 ) ) ;
#6254 =( GEOMETRIC_REPRESENTATION_CONTEXT ( 3 ) GLOBAL_UNCERTAINTY_ASSIGNED_CONTEXT ( ( #78215 ) ) GLOBAL_UNIT_ASSIGNED_CONTEXT ( ( #91181, #20726, #21721 ) ) REPRESENTATION_CONTEXT ( 'NONE', 'WORKASPACE' ) );
#6255 = CARTESIAN_POINT ( 'NONE',  ( -2.266590686148945544, 51.38708216824730357, -7.082119434687050408 ) ) ;
#6256 = CARTESIAN_POINT ( 'NONE',  ( 13.43411237798106583, 7.665301336597086568, -12.81628187352647252 ) ) ;
#6257 = ORIENTED_EDGE ( 'NONE', *, *, #4996, .T. ) ;
#6258 = CARTESIAN_POINT ( 'NONE',  ( 19.84674366389459266, 8.717264484334116048, -2.638427012816827677 ) ) ;
#6259 = CARTESIAN_POINT ( 'NONE',  ( 10.00000000000000000, 11.81368534415483751, -10.88017736071110342 ) ) ;
#6260 = CARTESIAN_POINT ( 'NONE',  ( 14.92337183194729633, 42.67559781766745886, 8.527530157486181039 ) ) ;
#6262 = DIRECTION ( 'NONE',  ( 0.000000000000000000, 1.000000000000000000, 0.000000000000000000 ) ) ;
#6261 = DIRECTION ( 'NONE',  ( -0.000000000000000000, -0.000000000000000000, 1.000000000000000000 ) ) ;
#6263 = CARTESIAN_POINT ( 'NONE',  ( 22.81628187352647785, 21.62363466993041783, 6.195893100308588602E-16 ) ) ;
#6264 = CARTESIAN_POINT ( 'NONE',  ( 19.84674366389459621, 23.50893115100078390, 7.409399052514197653E-17 ) ) ;
#6265 = VERTEX_POINT ( 'NONE', #16962 ) ;
#6266 = CARTESIAN_POINT ( 'NONE',  ( 12.63842701281683922, 4.550597817667451750, -9.846743663894590881 ) ) ;
#6267 = CARTESIAN_POINT ( 'NONE',  ( 9.729335482455997663, -19.62342160288553217, -4.000000000000000000 ) ) ;
#6268 = CARTESIAN_POINT ( 'NONE',  ( -46.70132286185116044, 101.0484326958216599, -8.835676566301254198 ) ) ;
#6269 = CARTESIAN_POINT ( 'NONE',  ( 7.084665262690076126, 14.10535201082150358, 10.88017736071109987 ) ) ;
#6270 = CARTESIAN_POINT ( 'NONE',  ( -2.266590686148945544, 46.38708216824730357, -7.082119434687050408 ) ) ;
#6271 = CARTESIAN_POINT ( 'NONE',  ( 7.084665262690076126, 57.02201867748817676, -10.88017736071110164 ) ) ;
#6272 = ADVANCED_FACE ( 'NONE', ( #46463 ), #46946, .F. ) ;
#6273 = DIRECTION ( 'NONE',  ( -5.818595309480553908E-17, -1.000000000000000000, -0.000000000000000000 ) ) ;
#6274 = CARTESIAN_POINT ( 'NONE',  ( 10.00000000000000000, 24.75893115100078745, -9.846743663894594434 ) ) ;
#6275 = CARTESIAN_POINT ( 'NONE',  ( 17.96484262340118221, 6.188685344154836621, -7.964842623401177768 ) ) ;
#6276 = CARTESIAN_POINT ( 'NONE',  ( 2.791683348922240793, 11.63393115100078568, 7.208316651077764092 ) ) ;
#6277 = CYLINDRICAL_SURFACE ( 'NONE', #67127, 0.2500000000000002220 ) ;
#6278 = CARTESIAN_POINT ( 'NONE',  ( 18.52753015748617571, 38.09226448433412315, 4.923371831947298993 ) ) ;
#6279 = EDGE_CURVE ( 'NONE', #21503, #3919, #24908, .T. ) ;
#6280 = STYLED_ITEM ( 'NONE', ( #76066 ), #26594 ) ;
#6281 = CARTESIAN_POINT ( 'NONE',  ( 2.035157376598822676, 37.43868534415484106, -7.964842623401177768 ) ) ;
#6282 = UNCERTAINTY_MEASURE_WITH_UNIT (LENGTH_MEASURE( 1.000000000000000082E-05 ), #74854, 'distance_accuracy_value', 'NONE');
#6283 = EDGE_LOOP ( 'NONE', ( #73638, #58172, #10041, #97104 ) ) ;
#6284 = CARTESIAN_POINT ( 'NONE',  ( 21.09922568453595559, 62.04030133659709634, -6.408140936763230044 ) ) ;
#6285 = DIRECTION ( 'NONE',  ( -0.9238795325112876267, 0.000000000000000000, 0.3826834323650877279 ) ) ;
#6286 = CARTESIAN_POINT ( 'NONE',  ( 19.84674366389459266, 8.300597817667451750, 2.638427012816836559 ) ) ;
#6287 = CARTESIAN_POINT ( 'NONE',  ( -2.816281873526473856, 39.33196800326374643, 3.434112377981055619 ) ) ;
#6289 = CARTESIAN_POINT ( 'NONE',  ( 0.1532563361054083140, 31.00893115100078390, 1.131784320476157264E-15 ) ) ;
#6288 = CARTESIAN_POINT ( 'NONE',  ( -0.8801773607111008646, 8.272018677488171434, 2.915334737309923430 ) ) ;
#6290 = LINE ( 'NONE', #67287, #48607 ) ;
#6291 = SURFACE_SIDE_STYLE ('',( #59773 ) ) ;
#6292 = CARTESIAN_POINT ( 'NONE',  ( 6.204703633549690345, 22.84541550158062861, 14.16423886937410082 ) ) ;
#6293 = CARTESIAN_POINT ( 'NONE',  ( -2.266590686148945544, 47.22041550158063927, 7.082119434687048631 ) ) ;
#6294 = CARTESIAN_POINT ( 'NONE',  ( 10.00000000000000178, 47.25893115100078745, 9.846743663894594434 ) ) ;
#6295 = CARTESIAN_POINT ( 'NONE',  ( 5.429172911440337757, -28.64165983023028517, -2.499999999999999556 ) ) ;
#6296 = CARTESIAN_POINT ( 'NONE',  ( 0.5774900079438590739, 32.64701867748816966, -5.440088680355550821 ) ) ;
#6297 = CARTESIAN_POINT ( 'NONE',  ( 20.88017736071110519, 65.56368534415483396, 2.639326808657452039E-16 ) ) ;
#6298 = VECTOR ( 'NONE', #51862, 1000.000000000000227 ) ;
#6299 = VERTEX_POINT ( 'NONE', #21632 ) ;
#6300 = CARTESIAN_POINT ( 'NONE',  ( 19.38216949554541557, 57.24863466993042493, -9.382169495545420901 ) ) ;
#6301 = CARTESIAN_POINT ( 'NONE',  ( 4.559911319644449179, 68.89701867748817676, 9.422509992056141925 ) ) ;
#6302 = ORIENTED_EDGE ( 'NONE', *, *, #34725, .T. ) ;
#6303 = CARTESIAN_POINT ( 'NONE',  ( -4.164238869374099927, 7.012082168247302683, 3.795296366450308767 ) ) ;
#6304 = CARTESIAN_POINT ( 'NONE',  ( 2.791683348922237240, 10.38393115100078390, -7.208316651077763204 ) ) ;
#6305 = DIRECTION ( 'NONE',  ( 0.7372773368101297464, 0.000000000000000000, -0.6755902076156540259 ) ) ;
#6306 = VERTEX_POINT ( 'NONE', #52118 ) ;
#6307 = CARTESIAN_POINT ( 'NONE',  ( 17.96484262340118221, 16.18868534415483396, -7.964842623401177768 ) ) ;
#6308 = EDGE_LOOP ( 'NONE', ( #89162, #17279, #694, #84296 ) ) ;
#6309 = CARTESIAN_POINT ( 'NONE',  ( 20.88017736071110875, 40.77201867748818387, -2.915334737309920765 ) ) ;
#6310 = ORIENTED_EDGE ( 'NONE', *, *, #31051, .T. ) ;
#6311 = CARTESIAN_POINT ( 'NONE',  ( 22.81628187352647785, 11.62363466993042138, 6.195893100308588602E-16 ) ) ;
#6312 = ORIENTED_EDGE ( 'NONE', *, *, #62855, .F. ) ;
#6313 = CARTESIAN_POINT ( 'NONE',  ( 2.791683348922237240, 0.3839311510007847872, -7.208316651077763204 ) ) ;
#6314 = CARTESIAN_POINT ( 'NONE',  ( 19.84674366389459266, 58.30059781766745886, 2.638427012816836559 ) ) ;
#6316 = DIRECTION ( 'NONE',  ( -0.4146932426562339180, 0.000000000000000000, -0.9099612708765455471 ) ) ;
#6315 = CARTESIAN_POINT ( 'NONE',  ( 2.035157376598824452, 18.68868534415484106, 7.964842623401179544 ) ) ;
#6317 = CARTESIAN_POINT ( 'NONE',  ( 0.1532563361054083140, 6.008931151000784787, 1.131784320476157264E-15 ) ) ;
#6318 = CARTESIAN_POINT ( 'NONE',  ( 15.44008868035555260, 14.73035201082150536, 9.422509992056143702 ) ) ;
#6319 = EDGE_CURVE ( 'NONE', #45246, #51268, #6614, .T. ) ;
#6320 = CARTESIAN_POINT ( 'NONE',  ( -2.816281873526471635, 58.91530133659707502, -3.434112377981056508 ) ) ;
#6321 = CARTESIAN_POINT ( 'NONE',  ( 0.5774900079438590739, 42.64701867748816966, -5.440088680355550821 ) ) ;
#6322 = CARTESIAN_POINT ( 'NONE',  ( 0.2751277870542909731, 47.28217586085238366, -6.499999999999992006 ) ) ;
#6323 = CARTESIAN_POINT ( 'NONE',  ( 22.81628187352647785, 51.62363466993042493, 6.195893100308588602E-16 ) ) ;
#6324 = CARTESIAN_POINT ( 'NONE',  ( 17.96484262340118221, 41.18868534415484106, -7.964842623401177768 ) ) ;
#6325 = DIRECTION ( 'NONE',  ( -0.7132504491541751257, 0.000000000000000000, -0.7009092642998574485 ) ) ;
#6326 = VECTOR ( 'NONE', #51893, 1000.000000000000000 ) ;
#6327 = CARTESIAN_POINT ( 'NONE',  ( 14.92337183194729988, 19.34226448433411960, -8.527530157486177487 ) ) ;
#6328 = CARTESIAN_POINT ( 'NONE',  ( 21.09922568453595559, 7.040301336597086568, -6.408140936763230044 ) ) ;
#6330 = CARTESIAN_POINT ( 'NONE',  ( 5.076628168052704559, 65.17559781766745175, -8.527530157486179263 ) ) ;
#6329 = FILL_AREA_STYLE ('',( #46794 ) ) ;
#6331 = CARTESIAN_POINT ( 'NONE',  ( 20.88017736071110875, 40.77201867748818387, -2.915334737309920765 ) ) ;
#6332 = AXIS2_PLACEMENT_3D ( 'NONE', #5831, #6316, #36823 ) ;
#6333 = CARTESIAN_POINT ( 'NONE',  ( 14.92337183194729988, 44.34226448433412315, -8.527530157486177487 ) ) ;
#6334 = LINE ( 'NONE', #19856, #69491 ) ;
#6335 = CARTESIAN_POINT ( 'NONE',  ( 0.1532563361054083140, 21.00893115100078745, 1.131784320476157264E-15 ) ) ;
#6336 = CARTESIAN_POINT ( 'NONE',  ( 7.361572987183170547, 12.05059781766744997, 9.846743663894590881 ) ) ;
#6338 = EDGE_LOOP ( 'NONE', ( #83126, #95982, #84054, #41437 ) ) ;
#6337 = CARTESIAN_POINT ( 'NONE',  ( 10.00000000000000178, 5.373634669930420493, 12.81628187352647608 ) ) ;
#6339 = CARTESIAN_POINT ( 'NONE',  ( 0.1532563361054082862, 66.21726448433413736, 2.638427012816831674 ) ) ;
#6340 = CARTESIAN_POINT ( 'NONE',  ( 10.00000000000000178, 50.37363466993042493, 12.81628187352647608 ) ) ;
#6341 = EDGE_CURVE ( 'NONE', #87452, #91690, #83919, .T. ) ;
#6342 = CARTESIAN_POINT ( 'NONE',  ( 14.92337183194729988, 29.34226448433411960, -8.527530157486177487 ) ) ;
#6343 = CARTESIAN_POINT ( 'NONE',  ( 6.757497259943707313, -58.30388498733396574, -2.750000000000000000 ) ) ;
#6344 = CARTESIAN_POINT ( 'NONE',  ( 2.035157376598822676, 2.438685344154838397, -7.964842623401177768 ) ) ;
#6345 = CARTESIAN_POINT ( 'NONE',  ( 2.791683348922237240, 30.38393115100078390, -7.208316651077763204 ) ) ;
#6346 = ORIENTED_EDGE ( 'NONE', *, *, #23931, .F. ) ;
#6347 = DIRECTION ( 'NONE',  ( -1.000000000000000000, 0.000000000000000000, 0.000000000000000000 ) ) ;
#6348 = EDGE_CURVE ( 'NONE', #29544, #97832, #39949, .T. ) ;
#6349 = CARTESIAN_POINT ( 'NONE',  ( 12.91533473730993009, 6.605352010821504471, -10.88017736071109987 ) ) ;
#6350 = CARTESIAN_POINT ( 'NONE',  ( -13.77612262535527954, 90.93158326518027934, -7.883772450803742338 ) ) ;
#6351 = CARTESIAN_POINT ( 'NONE',  ( 7.084665262690076126, 24.10535201082150181, 10.88017736071109987 ) ) ;
#6352 = CARTESIAN_POINT ( 'NONE',  ( 10.00000000000000000, 50.55374883491396787, -14.16423886937410082 ) ) ;
#6353 = CARTESIAN_POINT ( 'NONE',  ( 17.08211943468705840, 55.13708216824731068, -12.26659068614894466 ) ) ;
#6354 = DIRECTION ( 'NONE',  ( 0.000000000000000000, 0.000000000000000000, -1.000000000000000000 ) ) ;
#6355 = AXIS2_PLACEMENT_3D ( 'NONE', #21367, #27867, #43363 ) ;
#6356 = CARTESIAN_POINT ( 'NONE',  ( 2.791683348922237240, 15.38393115100078212, -7.208316651077763204 ) ) ;
#6357 = CARTESIAN_POINT ( 'NONE',  ( -1.099225684535947600, -0.4596986634029132657, 6.408140936763237150 ) ) ;
#6358 = ORIENTED_EDGE ( 'NONE', *, *, #24550, .F. ) ;
#6359 = DIRECTION ( 'NONE',  ( 1.000000000000000000, 0.000000000000000000, -0.000000000000000000 ) ) ;
#6360 = CARTESIAN_POINT ( 'NONE',  ( 0.5600000000000083800, 105.0000000000000000, -4.500000000000001776 ) ) ;
#6361 = CARTESIAN_POINT ( 'NONE',  ( -0.3689425029237881626, 12.42874883491396609, 10.36894250292379027 ) ) ;
#6362 = CARTESIAN_POINT ( 'NONE',  ( 1.472469842513823179, 26.42559781766745175, 4.923371831947296329 ) ) ;
#6363 = DIRECTION ( 'NONE',  ( -0.000000000000000000, -0.000000000000000000, 1.000000000000000000 ) ) ;
#6364 = CARTESIAN_POINT ( 'NONE',  ( -2.266590686148945544, 46.38708216824730357, -7.082119434687050408 ) ) ;
#6365 = CARTESIAN_POINT ( 'NONE',  ( 19.84674366389459266, 3.300597817667451750, 2.638427012816836559 ) ) ;
#6367 = DIRECTION ( 'NONE',  ( -0.5664062369248259454, 0.000000000000000000, -0.8241261886220204724 ) ) ;
#6366 = CARTESIAN_POINT ( 'NONE',  ( 1.274849032794131976, 13.57228050351029403, 6.499999999999760192 ) ) ;
#6368 = CARTESIAN_POINT ( 'NONE',  ( -0.8801773607111008646, 28.27201867748817321, 2.915334737309923430 ) ) ;
#6369 = CARTESIAN_POINT ( 'NONE',  ( 16.40814093676324603, 32.45696800326375353, -11.09922568453594671 ) ) ;
#6370 =( NAMED_UNIT ( * ) SI_UNIT ( $, .STERADIAN. ) SOLID_ANGLE_UNIT ( ) );
#6371 = CARTESIAN_POINT ( 'NONE',  ( 10.00000000000000178, 30.37363466993042138, 12.81628187352647608 ) ) ;
#6372 = CARTESIAN_POINT ( 'NONE',  ( 6.565887622018943937, 63.08196800326376064, -12.81628187352647608 ) ) ;
#6373 = VERTEX_POINT ( 'NONE', #59109 ) ;
#6374 = CARTESIAN_POINT ( 'NONE',  ( 2.603489959281591659, 10.43575266056827644, -6.500000000000006217 ) ) ;
#6375 = DIRECTION ( 'NONE',  ( 0.000000000000000000, 0.000000000000000000, -1.000000000000000000 ) ) ;
#6376 = CARTESIAN_POINT ( 'NONE',  ( 17.08211943468705840, 35.13708216824730357, -12.26659068614894466 ) ) ;
#6377 = CARTESIAN_POINT ( 'NONE',  ( 10.00000000000000000, 0.5537488349139675359, -14.16423886937410082 ) ) ;
#6378 = CARTESIAN_POINT ( 'NONE',  ( 12.91533473730992121, 9.522018677488171434, 10.88017736071110164 ) ) ;
#6379 = CARTESIAN_POINT ( 'NONE',  ( 0.5774900079438590739, 27.64701867748817676, -5.440088680355550821 ) ) ;
#6380 = DIRECTION ( 'NONE',  ( 0.000000000000000000, 0.000000000000000000, 1.000000000000000000 ) ) ;
#6381 = CARTESIAN_POINT ( 'NONE',  ( 20.88017736071110875, 50.77201867748817676, -2.915334737309920765 ) ) ;
#6382 = CARTESIAN_POINT ( 'NONE',  ( 19.42250999205614548, 45.98035201082150536, -5.440088680355545492 ) ) ;
#6383 = CARTESIAN_POINT ( 'NONE',  ( 10.00000000000000000, 22.87363466993042138, -12.81628187352647608 ) ) ;
#6384 = CARTESIAN_POINT ( 'NONE',  ( 20.15039907845753220, 26.74884699246889141, 6.262539305110078836 ) ) ;
#6385 = CARTESIAN_POINT ( 'NONE',  ( 1.472469842513823179, 21.42559781766745175, 4.923371831947296329 ) ) ;
#6386 = CARTESIAN_POINT ( 'NONE',  ( 7.084665262690076126, 52.02201867748816255, -10.88017736071110164 ) ) ;
#6387 = ADVANCED_FACE ( 'NONE', ( #98132 ), #54933, .F. ) ;
#6388 = CARTESIAN_POINT ( 'NONE',  ( 22.81628187352648496, 21.83196800326374643, -3.434112377981050290 ) ) ;
#6389 = FILL_AREA_STYLE ('',( #97419 ) ) ;
#6390 = CARTESIAN_POINT ( 'NONE',  ( 10.00000000000000000, 6.813685344154838397, -10.88017736071110342 ) ) ;
#6391 = CARTESIAN_POINT ( 'NONE',  ( 19.84674366389459621, 33.50893115100078745, 7.409399052514197653E-17 ) ) ;
#6392 = CARTESIAN_POINT ( 'NONE',  ( -2.816281873526471635, 63.91530133659708923, -3.434112377981056508 ) ) ;
#6393 = CARTESIAN_POINT ( 'NONE',  ( 12.63842701281683922, 14.55059781766744997, -9.846743663894590881 ) ) ;
#6394 = CARTESIAN_POINT ( 'NONE',  ( 10.00000000000000178, 8.053748834913967869, 14.16423886937410082 ) ) ;
#6395 = CARTESIAN_POINT ( 'NONE',  ( 2.550000000000003819, 99.99999999999998579, 8.000000000000000000 ) ) ;
#6396 = CARTESIAN_POINT ( 'NONE',  ( -0.8801773607111008646, 38.27201867748816255, 2.915334737309923430 ) ) ;
#6398 = CARTESIAN_POINT ( 'NONE',  ( 24.16423886937410614, 29.51208216824729647, -3.795296366450302550 ) ) ;
#6397 = CARTESIAN_POINT ( 'NONE',  ( 0.5774900079438590739, 2.647018677488170990, -5.440088680355550821 ) ) ;
#6399 = CARTESIAN_POINT ( 'NONE',  ( 10.00000000000000178, 42.25893115100078745, 9.846743663894594434 ) ) ;
#6400 = EDGE_CURVE ( 'NONE', #86598, #91147, #58421, .T. ) ;
#6401 = AXIS2_PLACEMENT_3D ( 'NONE', #35278, #28275, #49788 ) ;
#6402 = B_SPLINE_CURVE_WITH_KNOTS ( 'NONE', 3,
 ( #57336, #17880, #3369, #64338 ),
 .UNSPECIFIED., .F., .F.,
 ( 4, 4 ),
 ( 2.146014906638809613E-16, 0.002392975128318425206 ),
 .UNSPECIFIED. ) ;
#6403 = CARTESIAN_POINT ( 'NONE',  ( -0.8801773607111009756, 38.06368534415484106, 1.068504757029289695E-15 ) ) ;
#6404 = CARTESIAN_POINT ( 'NONE',  ( 10.00000000000000178, 14.31368534415483929, 10.88017736071110342 ) ) ;
#6405 = ORIENTED_EDGE ( 'NONE', *, *, #65569, .F. ) ;
#6406 = CIRCLE ( 'NONE', #52726, 0.2500000000000002220 ) ;
#6407 = CARTESIAN_POINT ( 'NONE',  ( 12.91533473730992121, 29.52201867748817321, 10.88017736071110164 ) ) ;
#6408 = AXIS2_PLACEMENT_3D ( 'NONE', #52884, #30143, #188 ) ;
#6409 = CARTESIAN_POINT ( 'NONE',  ( -1.099225684535947600, 39.54030133659708923, 6.408140936763237150 ) ) ;
#6410 = CARTESIAN_POINT ( 'NONE',  ( 7.084665262690076126, 37.02201867748817676, -10.88017736071110164 ) ) ;
#6412 = CARTESIAN_POINT ( 'NONE',  ( 15.44008868035555260, 34.73035201082151247, 9.422509992056143702 ) ) ;
#6411 = CARTESIAN_POINT ( 'NONE',  ( 0.1532563361054082862, 46.21726448433411605, 2.638427012816831674 ) ) ;
#6413 = ORIENTED_EDGE ( 'NONE', *, *, #44925, .F. ) ;
#6414 = CARTESIAN_POINT ( 'NONE',  ( 17.20831665107776587, 59.13393115100078745, -7.208316651077762316 ) ) ;
#6415 = CARTESIAN_POINT ( 'NONE',  ( 7.084665262690076126, 34.10535201082151247, 10.88017736071109987 ) ) ;
#6416 = CARTESIAN_POINT ( 'NONE',  ( 4.721518086276724979, -3.620742741961517019, 4.000000000000000000 ) ) ;
#6417 = DIRECTION ( 'NONE',  ( -0.000000000000000000, -1.000000000000000000, -0.000000000000000000 ) ) ;
#6418 = CARTESIAN_POINT ( 'NONE',  ( -2.266590686148945544, 46.38708216824730357, -7.082119434687050408 ) ) ;
#6419 = CARTESIAN_POINT ( 'NONE',  ( -0.8801773607111009756, 48.06368534415484817, 1.068504757029289695E-15 ) ) ;
#6420 = CARTESIAN_POINT ( 'NONE',  ( 17.20831665107776587, 62.88393115100078745, 7.208316651077764980 ) ) ;
#6421 = CARTESIAN_POINT ( 'NONE',  ( 8.470640952597488393, 15.00000000000000711, 11.92295067084773130 ) ) ;
#6422 = CARTESIAN_POINT ( 'NONE',  ( 14.92337183194729633, 62.67559781766745886, 8.527530157486181039 ) ) ;
#6423 = SURFACE_STYLE_USAGE ( .BOTH. , #45916 ) ;
#6424 = CARTESIAN_POINT ( 'NONE',  ( 14.92337183194729633, 2.675597817667451750, 8.527530157486181039 ) ) ;
#6425 = CARTESIAN_POINT ( 'NONE',  ( 5.076628168052704559, 20.17559781766745175, -8.527530157486179263 ) ) ;
#6426 = ORIENTED_EDGE ( 'NONE', *, *, #39741, .T. ) ;
#6427 = CARTESIAN_POINT ( 'NONE',  ( 12.63842701281683034, 27.46726448433411250, 9.846743663894596210 ) ) ;
#6428 = CARTESIAN_POINT ( 'NONE',  ( 9.382169495545419124, -24.00136533006957507, 9.382169495545417348 ) ) ;
#6429 = CARTESIAN_POINT ( 'NONE',  ( 4.559911319644449179, 23.89701867748817321, 9.422509992056141925 ) ) ;
#6430 = CARTESIAN_POINT ( 'NONE',  ( 12.63842701281683034, 22.46726448433411605, 9.846743663894596210 ) ) ;
#6431 = CARTESIAN_POINT ( 'NONE',  ( -4.838527690343710219, 14.49999999999999112, 14.19819177887730355 ) ) ;
#6432 = CARTESIAN_POINT ( 'NONE',  ( 0.6178305044545818747, 13.49863466993041783, -9.382169495545419124 ) ) ;
#6434 = CARTESIAN_POINT ( 'NONE',  ( 10.00000000000000000, 56.81368534415484106, -10.88017736071110342 ) ) ;
#6433 = CARTESIAN_POINT ( 'NONE',  ( 18.72515096720568195, 26.07228050351032778, -6.500000000000018652 ) ) ;
#6436 = CARTESIAN_POINT ( 'NONE',  ( 7.084665262690076126, 4.105352010821503583, 10.88017736071109987 ) ) ;
#6435 = CARTESIAN_POINT ( 'NONE',  ( 12.91533473730992121, 34.52201867748817676, 10.88017736071110164 ) ) ;
#6437 = CARTESIAN_POINT ( 'NONE',  ( 22.26659068614894466, 48.88708216824730357, 7.082119434687054849 ) ) ;
#6438 = EDGE_CURVE ( 'NONE', #87330, #86977, #58613, .T. ) ;
#6439 = B_SPLINE_CURVE_WITH_KNOTS ( 'NONE', 3,
 ( #36105, #36619, #75591, #20119, #60081, #98115 ),
 .UNSPECIFIED., .F., .F.,
 ( 4, 2, 4 ),
 ( 0.000000000000000000, 0.0004042018129159926330, 0.0008084036258319852661 ),
 .UNSPECIFIED. ) ;
#6440 = EDGE_CURVE ( 'NONE', #43121, #57214, #76516, .T. ) ;
#6441 = DIRECTION ( 'NONE',  ( -1.000000000000000000, -6.938893903907221278E-15, -0.000000000000000000 ) ) ;
#6442 = EDGE_CURVE ( 'NONE', #89305, #57072, #69420, .T. ) ;
#6443 = ORIENTED_EDGE ( 'NONE', *, *, #20709, .F. ) ;
#6444 = CARTESIAN_POINT ( 'NONE',  ( -1.099225684535947600, 18.70696800326375353, -6.408140936763238038 ) ) ;
#6445 = CARTESIAN_POINT ( 'NONE',  ( 12.91533473730992121, 49.52201867748817676, 10.88017736071110164 ) ) ;
#6446 = FILL_AREA_STYLE ('',( #67946 ) ) ;
#6447 = ORIENTED_EDGE ( 'NONE', *, *, #70155, .F. ) ;
#6448 = CARTESIAN_POINT ( 'NONE',  ( 0.5774900079438607392, 53.48035201082151247, 5.440088680355550821 ) ) ;
#6449 = CARTESIAN_POINT ( 'NONE',  ( 19.84674366389459621, 38.50893115100078745, 7.409399052514197653E-17 ) ) ;
#6450 = EDGE_CURVE ( 'NONE', #70139, #94698, #18080, .T. ) ;
#6451 = CARTESIAN_POINT ( 'NONE',  ( 7.361572987183169658, 19.96726448433411960, -9.846743663894592657 ) ) ;
#6452 = CARTESIAN_POINT ( 'NONE',  ( 17.20831665107776587, 12.88393115100078390, 7.208316651077764980 ) ) ;
#6454 = CARTESIAN_POINT ( 'NONE',  ( -1.099225684535947600, 39.54030133659708923, 6.408140936763237150 ) ) ;
#6453 = DIRECTION ( 'NONE',  ( 0.000000000000000000, -1.000000000000000000, 0.000000000000000000 ) ) ;
#6456 = CARTESIAN_POINT ( 'NONE',  ( -3.749999999999994671, 43.00000000000000711, 4.250000000000000000 ) ) ;
#6455 = CARTESIAN_POINT ( 'NONE',  ( -0.8801773607111009756, 68.06368534415484817, 1.068504757029289695E-15 ) ) ;
#6457 = CARTESIAN_POINT ( 'NONE',  ( 9.511407825589754950, -15.49433182431968170, 3.750000000000000000 ) ) ;
#6459 = VERTEX_POINT ( 'NONE', #94908 ) ;
#6458 = CARTESIAN_POINT ( 'NONE',  ( 0.1532563361054083140, 31.00893115100078390, 1.131784320476157264E-15 ) ) ;
#6460 = AXIS2_PLACEMENT_3D ( 'NONE', #14285, #44758, #22771 ) ;
#6461 = CARTESIAN_POINT ( 'NONE',  ( 10.00000000000000178, 55.37363466993042493, 12.81628187352647608 ) ) ;
#6462 = LINE ( 'NONE', #21474, #34205 ) ;
#6464 = EDGE_CURVE ( 'NONE', #73005, #90157, #41933, .T. ) ;
#6463 = CARTESIAN_POINT ( 'NONE',  ( 14.92337183194729633, 62.67559781766745886, 8.527530157486181039 ) ) ;
#6465 = CARTESIAN_POINT ( 'NONE',  ( 13.79529636645031943, 30.34541550158063927, -14.16423886937409904 ) ) ;
#6466 = VECTOR ( 'NONE', #21900, 1000.000000000000000 ) ;
#6467 = UNCERTAINTY_MEASURE_WITH_UNIT (LENGTH_MEASURE( 1.000000000000000082E-05 ), #63702, 'distance_accuracy_value', 'NONE');
#6468 = CARTESIAN_POINT ( 'NONE',  ( -14.82629065241270716, 0.2301504708693010715, 1.844815641835153563 ) ) ;
#6469 = ADVANCED_FACE ( 'NONE', ( #87890 ), #11412, .T. ) ;
#6470 = CARTESIAN_POINT ( 'NONE',  ( 13.79529636645031943, 30.34541550158063927, -14.16423886937409904 ) ) ;
#6471 = CARTESIAN_POINT ( 'NONE',  ( 17.08211943468705130, 48.47041550158063927, 12.26659068614894998 ) ) ;
#6472 = CARTESIAN_POINT ( 'NONE',  ( 2.917880565312948704, 12.63708216824730179, 12.26659068614894643 ) ) ;
#6474 = CARTESIAN_POINT ( 'NONE',  ( -13.65756908232610378, 90.97036336906094789, -7.949095025303489770 ) ) ;
#6473 = CARTESIAN_POINT ( 'NONE',  ( 17.08211943468705130, 18.47041550158063572, 12.26659068614894998 ) ) ;
#6475 = CARTESIAN_POINT ( 'NONE',  ( 15.44008868035555260, 44.73035201082151247, 9.422509992056143702 ) ) ;
#6476 = CARTESIAN_POINT ( 'NONE',  ( -11.36220558718868290, 15.00000000000000000, 9.008345252845137097 ) ) ;
#6477 = CARTESIAN_POINT ( 'NONE',  ( 19.84674366389459266, 28.30059781766745886, 2.638427012816836559 ) ) ;
#6480 = AXIS2_PLACEMENT_3D ( 'NONE', #53177, #45680, #76178 ) ;
#6479 = CARTESIAN_POINT ( 'NONE',  ( 17.20831665107776587, 29.13393115100078390, -7.208316651077762316 ) ) ;
#6478 = CARTESIAN_POINT ( 'NONE',  ( 12.91533473730993009, 66.60535201082150536, -10.88017736071109987 ) ) ;
#6481 = CARTESIAN_POINT ( 'NONE',  ( 12.91533473730992121, 19.52201867748816611, 10.88017736071110164 ) ) ;
#6482 = CARTESIAN_POINT ( 'NONE',  ( 0.6178305044545818747, 53.49863466993041072, -9.382169495545419124 ) ) ;
#6483 = CARTESIAN_POINT ( 'NONE',  ( 0.1532563361054082862, 61.21726448433412315, 2.638427012816831674 ) ) ;
#6484 = CARTESIAN_POINT ( 'NONE',  ( 2.791683348922237240, 30.38393115100078390, -7.208316651077763204 ) ) ;
#6485 = CARTESIAN_POINT ( 'NONE',  ( 22.81628187352648496, 36.83196800326376064, -3.434112377981050290 ) ) ;
#6486 = CARTESIAN_POINT ( 'NONE',  ( 7.082119434687054849, -21.52958449841935717, 12.26659068614894288 ) ) ;
#6487 = CARTESIAN_POINT ( 'NONE',  ( 2.035157376598824452, 38.68868534415483396, 7.964842623401179544 ) ) ;
#6488 = CARTESIAN_POINT ( 'NONE',  ( 1.472469842513823179, 45.59226448433412315, -4.923371831947296329 ) ) ;
#6489 = CARTESIAN_POINT ( 'NONE',  ( 2.917880565312950480, 30.97041550158063572, -12.26659068614894821 ) ) ;
#6490 = EDGE_LOOP ( 'NONE', ( #733, #24227, #78705, #12836, #93610, #35062, #85868, #41735 ) ) ;
#6491 = SURFACE_STYLE_USAGE ( .BOTH. , #98016 ) ;
#6492 = CARTESIAN_POINT ( 'NONE',  ( 10.00000000000000178, 69.31368534415484817, 10.88017736071110342 ) ) ;
#6493 = CARTESIAN_POINT ( 'NONE',  ( 12.91533473730993009, 61.60535201082150536, -10.88017736071109987 ) ) ;
#6494 = CARTESIAN_POINT ( 'NONE',  ( 6.204703633549690345, 57.84541550158063927, 14.16423886937410082 ) ) ;
#6495 = CARTESIAN_POINT ( 'NONE',  ( 19.84674366389459266, 63.30059781766745886, 2.638427012816836559 ) ) ;
#6496 = CARTESIAN_POINT ( 'NONE',  ( -4.249999999999999112, 78.07179676972445748, 6.250000000000000000 ) ) ;
#6497 = CARTESIAN_POINT ( 'NONE',  ( 12.91533473730992121, 54.52201867748816255, 10.88017736071110164 ) ) ;
#6498 = CARTESIAN_POINT ( 'NONE',  ( -6.761389522993706436, 0.2306972965111901419, -13.32372569557309028 ) ) ;
#6499 = VECTOR ( 'NONE', #7123, 1000.000000000000000 ) ;
#6500 = CARTESIAN_POINT ( 'NONE',  ( -9.422509992056145478, 22.64701867748818032, -5.440088680355541939 ) ) ;
#6501 = CARTESIAN_POINT ( 'NONE',  ( 17.96484262340118221, 11.18868534415483929, -7.964842623401177768 ) ) ;
#6502 = CARTESIAN_POINT ( 'NONE',  ( 4.559911319644449179, 17.23035201082150536, -9.422509992056141925 ) ) ;
#6503 = CARTESIAN_POINT ( 'NONE',  ( 12.63842701281683034, 37.46726448433411605, 9.846743663894596210 ) ) ;
#6504 = CARTESIAN_POINT ( 'NONE',  ( 13.43411237798105340, 45.58196800326374643, 12.81628187352647963 ) ) ;
#6505 = DIRECTION ( 'NONE',  ( 1.000000000000000000, 0.000000000000000000, 0.000000000000000000 ) ) ;
#6506 = VERTEX_POINT ( 'NONE', #3923 ) ;
#6507 = STYLED_ITEM ( 'NONE', ( #53339 ), #34314 ) ;
#6508 = CARTESIAN_POINT ( 'NONE',  ( -0.8801773607111008646, 23.27201867748817676, 2.915334737309923430 ) ) ;
#6509 = EDGE_CURVE ( 'NONE', #74408, #84772, #45669, .T. ) ;
#6510 = CARTESIAN_POINT ( 'NONE',  ( 13.43411237798105340, 25.58196800326374998, 12.81628187352647963 ) ) ;
#6511 = CARTESIAN_POINT ( 'NONE',  ( 19.89220837332773684, 39.74062864464239908, 6.478736007406005193 ) ) ;
#6512 = CARTESIAN_POINT ( 'NONE',  ( 1.472469842513823179, 5.592264484334118713, -4.923371831947296329 ) ) ;
#6513 = CARTESIAN_POINT ( 'NONE',  ( 18.52753015748618282, 43.92559781766745175, -4.923371831947291888 ) ) ;
#6514 = CARTESIAN_POINT ( 'NONE',  ( 17.96484262340118221, 36.18868534415484106, -7.964842623401177768 ) ) ;
#6515 = CARTESIAN_POINT ( 'NONE',  ( -1.099225684535947600, 14.54030133659708568, 6.408140936763237150 ) ) ;
#6517 = DIRECTION ( 'NONE',  ( 0.000000000000000000, -1.000000000000000000, 0.000000000000000000 ) ) ;
#6516 = CARTESIAN_POINT ( 'NONE',  ( 17.96484262340118221, 54.93868534415484106, 7.964842623401181321 ) ) ;
#6518 = DIRECTION ( 'NONE',  ( 0.000000000000000000, 0.000000000000000000, 1.000000000000000000 ) ) ;
#6519 = CARTESIAN_POINT ( 'NONE',  ( 21.09922568453594849, 51.20696800326375353, 6.408140936763242479 ) ) ;
#6520 = ORIENTED_EDGE ( 'NONE', *, *, #79035, .T. ) ;
#6521 = CARTESIAN_POINT ( 'NONE',  ( 20.88017736071110875, 65.77201867748817676, -2.915334737309920765 ) ) ;
#6523 = CARTESIAN_POINT ( 'NONE',  ( 24.16423886937410614, 4.512082168247300906, -3.795296366450302550 ) ) ;
#6522 = CARTESIAN_POINT ( 'NONE',  ( 13.43411237798105340, 30.58196800326374998, 12.81628187352647963 ) ) ;
#6524 = CARTESIAN_POINT ( 'NONE',  ( 18.52753015748618282, 3.925597817667451306, -4.923371831947291888 ) ) ;
#6525 = CARTESIAN_POINT ( 'NONE',  ( 20.88017736071110164, 35.35535201082150536, 2.915334737309930979 ) ) ;
#6526 = DIRECTION ( 'NONE',  ( -1.000000000000000000, -0.000000000000000000, -0.000000000000000000 ) ) ;
#6527 = CARTESIAN_POINT ( 'NONE',  ( 0.1532563361054100626, 65.80059781766745175, -2.638427012816831230 ) ) ;
#6528 = CARTESIAN_POINT ( 'NONE',  ( 18.52753015748617571, 18.09226448433411960, 4.923371831947298993 ) ) ;
#6529 = CARTESIAN_POINT ( 'NONE',  ( 12.63842701281683034, 7.467264484334118713, 9.846743663894596210 ) ) ;
#6530 = CARTESIAN_POINT ( 'NONE',  ( 0.000000000000000000, 0.5000000000000004441, 0.000000000000000000 ) ) ;
#6531 = CARTESIAN_POINT ( 'NONE',  ( 22.26659068614895176, 44.72041550158063927, -7.082119434687042414 ) ) ;
#6532 = CARTESIAN_POINT ( 'NONE',  ( 0.2751277870542911397, 55.30223176428831522, 6.499999999999992006 ) ) ;
#6533 =( NAMED_UNIT ( * ) PLANE_ANGLE_UNIT ( ) SI_UNIT ( $, .RADIAN. ) );
#6534 = CARTESIAN_POINT ( 'NONE',  ( 0.1077916266722467875, 7.240628644642391087, -6.478736007405949238 ) ) ;
#6535 = AXIS2_PLACEMENT_3D ( 'NONE', #7124, #53598, #90608 ) ;
#6536 = EDGE_LOOP ( 'NONE', ( #11013, #6809, #53650, #28064 ) ) ;
#6537 = EDGE_LOOP ( 'NONE', ( #7707, #54007, #79650, #25763 ) ) ;
#6538 = CARTESIAN_POINT ( 'NONE',  ( 22.26659068614895176, 64.72041550158064638, -7.082119434687042414 ) ) ;
#6539 = CARTESIAN_POINT ( 'NONE',  ( 20.36894250292379382, 63.67874883491396787, 10.36894250292379205 ) ) ;
#6540 = CARTESIAN_POINT ( 'NONE',  ( 1.472469842513823179, 26.42559781766745175, 4.923371831947296329 ) ) ;
#6541 = CARTESIAN_POINT ( 'NONE',  ( 0.6178305044545838731, 24.74863466993042493, 9.382169495545420901 ) ) ;
#6543 = CARTESIAN_POINT ( 'NONE',  ( 10.00000000000000000, 5.553748834913967869, -14.16423886937410082 ) ) ;
#6542 = CARTESIAN_POINT ( 'NONE',  ( 3.881909499399555319, 14.99999999999807976, 14.10103859408278915 ) ) ;
#6544 = CARTESIAN_POINT ( 'NONE',  ( 10.00000000000000000, 16.81368534415483751, -10.88017736071110342 ) ) ;
#6545 = CARTESIAN_POINT ( 'NONE',  ( 24.16423886937410614, 59.30374883491397497, 8.672049930838204340E-16 ) ) ;
#6546 = CARTESIAN_POINT ( 'NONE',  ( 17.20831665107776587, 27.88393115100078390, 7.208316651077764980 ) ) ;
#6547 = CARTESIAN_POINT ( 'NONE',  ( -7.750000000000000000, 40.74999999999999289, 4.000000000000000000 ) ) ;
#6548 = CARTESIAN_POINT ( 'NONE',  ( 14.92337183194729988, 24.34226448433411960, -8.527530157486177487 ) ) ;
#6549 = AXIS2_PLACEMENT_3D ( 'NONE', #70594, #83753, #18574 ) ;
#6550 = CARTESIAN_POINT ( 'NONE',  ( 19.84674366389459266, 3.300597817667451750, 2.638427012816836559 ) ) ;
#6551 = CARTESIAN_POINT ( 'NONE',  ( 2.638427012816829897, 9.550597817667449974, -9.846743663894592657 ) ) ;
#6552 = VERTEX_POINT ( 'NONE', #49898 ) ;
#6553 = ORIENTED_EDGE ( 'NONE', *, *, #6116, .T. ) ;
#6554 = APPLICATION_CONTEXT ( 'automotive_design' ) ;
#6555 = ADVANCED_FACE ( 'NONE', ( #78433 ), #80407, .T. ) ;
#6556 = VERTEX_POINT ( 'NONE', #93438 ) ;
#6557 = CARTESIAN_POINT ( 'NONE',  ( 17.20831665107776587, 49.13393115100078745, -7.208316651077762316 ) ) ;
#6558 = CARTESIAN_POINT ( 'NONE',  ( 13.79529636645031943, 20.34541550158063572, -14.16423886937409904 ) ) ;
#6560 = CARTESIAN_POINT ( 'NONE',  ( 12.91533473730992121, 44.52201867748816966, 10.88017736071110164 ) ) ;
#6559 = CARTESIAN_POINT ( 'NONE',  ( 7.084665262690076126, 24.10535201082150181, 10.88017736071109987 ) ) ;
#6562 = CARTESIAN_POINT ( 'NONE',  ( 3.591859063236761518, 14.95696800326375531, 11.09922568453594849 ) ) ;
#6561 = CARTESIAN_POINT ( 'NONE',  ( 5.076628168052703671, 66.84226448433412315, 8.527530157486179263 ) ) ;
#6563 = ADVANCED_FACE ( 'NONE', ( #24963 ), #55448, .T. ) ;
#6564 = CARTESIAN_POINT ( 'NONE',  ( 19.38216949554541202, 25.99863466993042138, 9.382169495545424454 ) ) ;
#6565 = EDGE_CURVE ( 'NONE', #89076, #37577, #24771, .T. ) ;
#6566 = ORIENTED_EDGE ( 'NONE', *, *, #79404, .F. ) ;
#6567 = CARTESIAN_POINT ( 'NONE',  ( 0.1532563361054083140, 46.00893115100079456, 1.131784320476157264E-15 ) ) ;
#6568 = CARTESIAN_POINT ( 'NONE',  ( 4.559911319644449179, 2.230352010821504916, -9.422509992056141925 ) ) ;
#6569 = ORIENTED_EDGE ( 'NONE', *, *, #88215, .F. ) ;
#6570 = CARTESIAN_POINT ( 'NONE',  ( -0.8801773607110991993, 2.855352010821504471, -2.915334737309923874 ) ) ;
#6571 = EDGE_LOOP ( 'NONE', ( #73157, #22574, #58174, #50847 ) ) ;
#6572 = CARTESIAN_POINT ( 'NONE',  ( 15.44008868035555793, 46.39701867748817676, -9.422509992056140149 ) ) ;
#6573 = CARTESIAN_POINT ( 'NONE',  ( -0.8801773607110991993, 62.85535201082150536, -2.915334737309923874 ) ) ;
#6574 = FILL_AREA_STYLE ('',( #44068 ) ) ;
#6575 = CARTESIAN_POINT ( 'NONE',  ( -0.8801773607110991993, 57.85535201082149825, -2.915334737309923874 ) ) ;
#6576 = AXIS2_PLACEMENT_3D ( 'NONE', #39343, #77314, #8828 ) ;
#6577 = EDGE_CURVE ( 'NONE', #43285, #68868, #65601, .T. ) ;
#6578 = AXIS2_PLACEMENT_3D ( 'NONE', #11279, #54801, #72270 ) ;
#6579 = LINE ( 'NONE', #92529, #65035 ) ;
#6580 = ORIENTED_EDGE ( 'NONE', *, *, #85472, .F. ) ;
#6581 = AXIS2_PLACEMENT_3D ( 'NONE', #81999, #75488, #29975 ) ;
#6582 = CARTESIAN_POINT ( 'NONE',  ( 19.84674366389459266, 33.30059781766744464, 2.638427012816836559 ) ) ;
#6583 = ORIENTED_EDGE ( 'NONE', *, *, #75639, .T. ) ;
#6584 = DIRECTION ( 'NONE',  ( 0.000000000000000000, 1.000000000000000000, 0.000000000000000000 ) ) ;
#6585 = CARTESIAN_POINT ( 'NONE',  ( 20.30776406404415724, 70.00000000000000000, -6.000000000000001776 ) ) ;
#6586 = EDGE_CURVE ( 'NONE', #12985, #90692, #50887, .T. ) ;
#6587 = CARTESIAN_POINT ( 'NONE',  ( 13.79529636645030344, 3.262082168247301350, 14.16423886937410614 ) ) ;
#6588 = SURFACE_SIDE_STYLE ('',( #75082 ) ) ;
#6589 = DIRECTION ( 'NONE',  ( -0.5905099943842175847, -0.8070303256584298035, 0.000000000000000000 ) ) ;
#6590 = DIRECTION ( 'NONE',  ( 0.000000000000000000, 0.000000000000000000, 1.000000000000000000 ) ) ;
#6591 = CARTESIAN_POINT ( 'NONE',  ( 0.5774900079438590739, 12.64701867748817321, -5.440088680355550821 ) ) ;
#6592 = CARTESIAN_POINT ( 'NONE',  ( 18.39792806157253224, 64.52224192338641728, 6.499999999999917399 ) ) ;
#6593 = ORIENTED_EDGE ( 'NONE', *, *, #40925, .T. ) ;
#6594 = SURFACE_STYLE_FILL_AREA ( #14106 ) ;
#6595 = CARTESIAN_POINT ( 'NONE',  ( 17.20831665107776587, 44.13393115100078745, -7.208316651077762316 ) ) ;
#6596 = FACE_OUTER_BOUND ( 'NONE', #91739, .T. ) ;
#6597 = CARTESIAN_POINT ( 'NONE',  ( 21.09922568453595559, 22.04030133659708923, -6.408140936763230044 ) ) ;
#6598 = CARTESIAN_POINT ( 'NONE',  ( 1.472469842513823179, 5.592264484334118713, -4.923371831947296329 ) ) ;
#6599 = CARTESIAN_POINT ( 'NONE',  ( 2.897438467171757030E-16, 23.03999999999999915, 0.000000000000000000 ) ) ;
#6600 = CARTESIAN_POINT ( 'NONE',  ( 7.361572987183169658, 19.96726448433411960, -9.846743663894592657 ) ) ;
#6601 = CARTESIAN_POINT ( 'NONE',  ( 6.565887622018943937, 8.081968003263751754, -12.81628187352647608 ) ) ;
#6602 = CARTESIAN_POINT ( 'NONE',  ( 0.1532563361054100626, 25.80059781766744820, -2.638427012816831230 ) ) ;
#6603 = AXIS2_PLACEMENT_3D ( 'NONE', #4673, #6137, #27144 ) ;
#6604 = ORIENTED_EDGE ( 'NONE', *, *, #19988, .F. ) ;
#6605 = ORIENTED_EDGE ( 'NONE', *, *, #39008, .F. ) ;
#6606 = CARTESIAN_POINT ( 'NONE',  ( -0.8801773607111008646, 18.27201867748817321, 2.915334737309923430 ) ) ;
#6607 = CARTESIAN_POINT ( 'NONE',  ( -2.266590686148945544, 17.22041550158063572, 7.082119434687048631 ) ) ;
#6608 = CARTESIAN_POINT ( 'NONE',  ( 19.84674366389459621, 33.50893115100078745, 7.409399052514197653E-17 ) ) ;
#6609 = CARTESIAN_POINT ( 'NONE',  ( 4.559911319644449179, 58.89701867748817676, 9.422509992056141925 ) ) ;
#6611 = DIRECTION ( 'NONE',  ( -0.3338068592337842810, -0.000000000000000000, 0.9426414910921737667 ) ) ;
#6610 = CARTESIAN_POINT ( 'NONE',  ( 3.591859063236761518, 39.95696800326375353, 11.09922568453594849 ) ) ;
#6612 = CARTESIAN_POINT ( 'NONE',  ( 4.559911319644449179, 12.23035201082150536, -9.422509992056141925 ) ) ;
#6613 = LINE ( 'NONE', #37620, #91767 ) ;
#6614 = LINE ( 'NONE', #89620, #28022 ) ;
#6615 = CARTESIAN_POINT ( 'NONE',  ( 0.6178305044545838731, 9.748634669930416052, 9.382169495545420901 ) ) ;
#6616 = CARTESIAN_POINT ( 'NONE',  ( 0.1532563361054100626, 65.80059781766745175, -2.638427012816831230 ) ) ;
#6617 = CARTESIAN_POINT ( 'NONE',  ( 5.076628168052704559, 30.17559781766745175, -8.527530157486179263 ) ) ;
#6618 = CARTESIAN_POINT ( 'NONE',  ( -9.422509992056145478, -12.35298132251182146, -5.440088680355541939 ) ) ;
#6619 = CARTESIAN_POINT ( 'NONE',  ( 21.09922568453595559, 42.04030133659708213, -6.408140936763230044 ) ) ;
#6620 = CARTESIAN_POINT ( 'NONE',  ( -9.024359497401759356, 75.07164295747612925, 3.000000000000000000 ) ) ;
#6621 =( GEOMETRIC_REPRESENTATION_CONTEXT ( 3 ) GLOBAL_UNCERTAINTY_ASSIGNED_CONTEXT ( ( #69131 ) ) GLOBAL_UNIT_ASSIGNED_CONTEXT ( ( #47099, #83640, #40107 ) ) REPRESENTATION_CONTEXT ( 'NONE', 'WORKASPACE' ) );
#6623 = CARTESIAN_POINT ( 'NONE',  ( 70.00000000000000000, -4.073016716636387686E-15, 9.500000000000000000 ) ) ;
#6622 = CARTESIAN_POINT ( 'NONE',  ( 20.88017736071110875, 35.77201867748816966, -2.915334737309920765 ) ) ;
#6624 = DIRECTION ( 'NONE',  ( -0.1736481776669272503, 0.9848077530122086864, -0.000000000000000000 ) ) ;
#6625 = CARTESIAN_POINT ( 'NONE',  ( 0.5774900079438590739, 67.64701867748817676, -5.440088680355550821 ) ) ;
#6626 = CARTESIAN_POINT ( 'NONE',  ( 12.91533473730993009, 46.60535201082150536, -10.88017736071109987 ) ) ;
#6627 = B_SPLINE_CURVE_WITH_KNOTS ( 'NONE', 3,
 ( #82035, #74531, #5065, #57556, #36042, #50064 ),
 .UNSPECIFIED., .F., .F.,
 ( 4, 2, 4 ),
 ( 3.409110551496108329E-05, 0.0004400426677367861921, 0.0008459942299586113755 ),
 .UNSPECIFIED. ) ;
#6628 = CARTESIAN_POINT ( 'NONE',  ( -0.8801773607111009756, 43.06368534415484106, 1.068504757029289695E-15 ) ) ;
#6629 = CARTESIAN_POINT ( 'NONE',  ( 19.84674366389459266, 63.71726448433412315, -2.638427012816827677 ) ) ;
#6630 = CARTESIAN_POINT ( 'NONE',  ( 7.084665262690076126, 67.02201867748817676, -10.88017736071110164 ) ) ;
#6631 = CARTESIAN_POINT ( 'NONE',  ( 10.00000000000000178, 37.25893115100078745, 9.846743663894594434 ) ) ;
#6632 = CARTESIAN_POINT ( 'NONE',  ( 4.559911319644449179, 2.230352010821504471, -9.422509992056141925 ) ) ;
#6633 = CARTESIAN_POINT ( 'NONE',  ( 21.09922568453594849, 6.206968003263753531, 6.408140936763242479 ) ) ;
#6634 = ORIENTED_EDGE ( 'NONE', *, *, #41779, .F. ) ;
#6635 = CARTESIAN_POINT ( 'NONE',  ( 7.084665262690076126, 29.10535201082150181, 10.88017736071109987 ) ) ;
#6636 = CARTESIAN_POINT ( 'NONE',  ( 2.035157376598824452, 33.68868534415484106, 7.964842623401179544 ) ) ;
#6637 = CARTESIAN_POINT ( 'NONE',  ( 7.084665262690076126, 69.10535201082151957, 10.88017736071109987 ) ) ;
#6638 = CARTESIAN_POINT ( 'NONE',  ( 13.79529636645030344, 43.26208216824730357, 14.16423886937410614 ) ) ;
#6639 = EDGE_CURVE ( 'NONE', #981, #82789, #88557, .T. ) ;
#6640 = CARTESIAN_POINT ( 'NONE',  ( 2.791683348922240793, 11.63393115100078568, 7.208316651077764092 ) ) ;
#6641 = CARTESIAN_POINT ( 'NONE',  ( -0.8801773607111008646, 53.27201867748816966, 2.915334737309923430 ) ) ;
#6642 = CARTESIAN_POINT ( 'NONE',  ( 0.000000000000000000, 15.00000000000000000, 0.000000000000000000 ) ) ;
#6643 = CARTESIAN_POINT ( 'NONE',  ( 22.26659068614895176, 4.720415501580633943, -7.082119434687042414 ) ) ;
#6644 = VECTOR ( 'NONE', #42771, 1000.000000000000000 ) ;
#6645 = ADVANCED_FACE ( 'NONE', ( #28862 ), #65385, .F. ) ;
#6646 = ORIENTED_EDGE ( 'NONE', *, *, #5230, .F. ) ;
#6647 = CARTESIAN_POINT ( 'NONE',  ( 4.669717816210469330, -13.81568353613706535, 2.499999999999999556 ) ) ;
#6648 = CARTESIAN_POINT ( 'NONE',  ( 5.076628168052704559, 65.17559781766745175, -8.527530157486179263 ) ) ;
#6649 =( BOUNDED_SURFACE ( )  B_SPLINE_SURFACE ( 1, 2, ( 
 ( #97964, #59925, #75428, #76416, #29420, #52917, #68433, #30411, #454, #14948, #44920, #6436, #67445, #6942, #37943, #98460, #91416, #8413, #83917, #15446, #45927, #23434, #68925, #84422, #15919, #52434, #74935, #90413, #59256, #13770, #59753, #96297, #43271, #21780, #67266, #27774, #36272, #89270, #73276, #73766, #82754, #44750, #12774, #5295, #36774, #97794, #58259, #74761, #57776, #88282, #4798, #44257, #35773, #14277, #90248, #66261, #96796, #58766, #43762, #6269, #89757, #28271, #21274, #52259, #82254, #75253, #74251, #20781, #81758, #29256, #88774, #51272, #13270, #5783, #6766, #66767, #50783, #65269, #95797, #19782, #97290, #28764, #51770, #27278, #50270, #80787, #12284, #42791, #35274, #65769, #20285, #81274, #93636, #33606, #77154, #18147, #56143, #71633, #69665, #26133, #41148, #85649, #2178, #78144, #70656, #94620, #63134, #48130, #54643, #25170, #55646, #9654, #40151, #47142, #33123, #32636, #87113, #86146, #39175, #25650, #56624, #10151, #63617, #1191, #40646, #85160, #17659, #55135, #78645, #16668, #32134, #10636, #77639, #9156, #48619, #94124, #17169, #71144, #39674, #18628, #2672, #86638, #8663, #79123, #31650, #3144, #24665, #64102, #62140, #92648, #70165, #24172, #1682, #62634, #93138, #47649, #87601, #11610, #58584, #58083, #95606, #59075, #51087, #12592, #34101, #42607, #50599, #43091, #27594, #28585, #20600, #49120, #4621, #42126, #81091, #20095, #88587, #66081, #19112, #81578, #12104, #73085, #73577, #65084, #88093, #5101, #49592, #65582, #5606, #79622, #89086, #28086, #43582, #41642, #97114, #13084, #57596, #35083, #50101, #96109, #66587, #27093, #4126, #74073, #36084, #80104, #35594, #19606, #89580, #11123, #72592, #72106, #64592, #34590, #80607, #96609, #3635, #95100, #26607, #57105, #60061, #46062, #91054, #59576, #75569, #38563, #82075, #597, #22090, #30546, #7081, #90562, #22581, #37583, #31039, #67587, #29556, #91562, #23079, #14090, #61048, #13586, #44069, #90069, #100, #52566, #69059, #76548, #98096, #83071, #14590, #98604, #68569, #45562, #45059, #76058, #8067, #38080, #61539, #30054, #68076, #60563, #53548, #82576, #53054, #83571, #15090, #84061, #7588, #6575, #15580, #21091, #74575, #51591, #6091, #36594, #67080, #97607, #29068, #21593, #52083, #44573, #75071, #37088, #24558, #46542, #54044, #62028, #24056, #16554, #77043, #92528, #54525, #48503, #8556, #84554, #94011, #79006, #1068, #69552, #55017, #17047, #10031, #31532, #47527, #85534, #25045, #77520, #85041, #25534, #86028, #56025, #10509, #41025, #78029, #78517, #71527, #33010, #47028, #70535, #9037, #39057, #39554, #70043, #40532 ),
 ( #1565, #40033, #9531, #2057, #32519, #32014, #48009, #63017, #3037, #93518, #16054, #71030, #33487, #55531, #2553, #62517, #17542, #93022, #63509, #86523, #18021, #92047, #23575, #96491, #33975, #3517, #4987, #49482, #64478, #65964, #57967, #27962, #81460, #12963, #95492, #50471, #43458, #35468, #94985, #42490, #26491, #18507, #11008, #56985, #80976, #48997, #26985, #72972, #4503, #58456, #34473, #87492, #94496, #56510, #19006, #4011, #79990, #57483, #73960, #11492, #87978, #64966, #88971, #42013, #19489, #20480, #72478, #34968, #26015, #88471, #12475, #50966, #49982, #80490, #5489, #63986, #11987, #65465, #95992, #71992, #27474, #87001, #79506, #19974, #42979, #41524, #73459, #28944, #45433, #28468, #58965, #74444, #14963, #44446, #53423, #60925, #13971, #6451, #29433, #14462, #83442, #60434, #74948, #90927, #22958, #52931, #15459, #44937, #36961, #52447, #75935, #97478, #67456, #97977, #59937, #7458, #75443, #21465, #37956, #91430, #89461, #6955, #90427, #21968, #67950, #82947, #29928, #37463, #45940, #20979, #82447, #22456, #98474, #51462, #96991, #5971, #66960, #59446, #81952, #36465, #89947, #83930, #13465, #43946, #68449, #76430, #51963, #98970, #30424, #35960, #66455, #46423, #62390, #69919, #39910, #8426, #63384, #61416, #68938, #9911, #93888, #15932, #84435, #1440, #31892, #24919, #76916, #92898, #24429, #70413, #92411, #38933, #40413, #1933, #70908, #25416, #55900, #39426, #93394, #86397, #47888, #69422, #85408, #943, #91923, #53925, #31404, #55404, #23448, #54893, #16918, #47394, #78390, #77396, #61905, #38441, #468, #23935, #46903, #54404, #77896, #17900, #84916, #9408, #8909, #2428, #16427, #32390, #32885, #62895, #85905, #30916, #17419, #48383, #7945, #10886, #56868, #35347, #80856, #41410, #49856, #3885, #86880, #87369, #96370, #58331, #26369, #18884, #50345, #12353, #71874, #88356, #71401, #2917, #18390, #57846, #49365, #27843, #4870, #79867, #11371, #72353, #57359, #27353, #4382, #41893, #34847, #65841, #95871, #88848, #87853, #34352, #95362, #19852, #3386, #64843, #26862, #19371, #42860, #80365, #64359, #73343, #20356, #33367, #11865, #42372, #72846, #65343, #78885, #10396, #40900, #63861, #94375, #25894, #56393, #48869, #79381, #33851, #94868, #81827, #74323, #5366, #20851, #97356, #59325, #22342, #52815, #43827, #60323, #43341, #73838, #89341, #29814, #89828, #68331, #75818, #28825, #21345, #44325, #29319, #98356, #75320, #51836, #6833, #37840, #67838, #30305, #59816, #82323, #67330, #90813, #13343, #13843, #74826, #6330, #83323, #90311, #36340, #14849, #7339, #35845, #21847, #36842, #97856, #82821 ) ),
 .UNSPECIFIED., .F., .F., .T. ) 
 B_SPLINE_SURFACE_WITH_KNOTS ( ( 2, 2 ),
 ( 3, 2, 2, 2, 2, 2, 2, 2, 2, 2, 2, 2, 2, 2, 2, 2, 2, 2, 2, 2, 2, 2, 2, 2, 2, 2, 2, 2, 2, 2, 2, 2, 2, 2, 2, 2, 2, 2, 2, 2, 2, 2, 2, 2, 2, 2, 2, 2, 2, 2, 2, 2, 2, 2, 2, 2, 2, 2, 2, 2, 2, 2, 2, 2, 2, 2, 2, 2, 2, 2, 2, 2, 2, 2, 2, 2, 2, 2, 2, 2, 2, 2, 2, 2, 2, 2, 2, 2, 2, 2, 2, 2, 2, 2, 2, 2, 2, 2, 2, 2, 2, 2, 2, 2, 2, 2, 2, 2, 2, 2, 2, 2, 2, 2, 2, 2, 2, 2, 2, 2, 2, 2, 2, 2, 2, 2, 2, 2, 2, 2, 2, 2, 2, 2, 2, 2, 2, 2, 2, 2, 2, 2, 2, 2, 2, 2, 2, 2, 2, 2, 2, 2, 2, 2, 2, 2, 2, 2, 2, 2, 2, 2, 3 ),
 ( 0.000000000000000000, 1.000000000000000000 ),
 ( 0.000000000000000000, 0.005952380952380952051, 0.01190476190476190410, 0.01785714285714285615, 0.02380952380952380820, 0.02976190476190476025, 0.03571428571428571230, 0.04166666666666666435, 0.04761904761904761640, 0.05357142857142856845, 0.05952380952380952051, 0.06547619047619047949, 0.07142857142857142461, 0.07738095238095238360, 0.08333333333333332871, 0.08928571428571428770, 0.09523809523809523281, 0.1011904761904761918, 0.1071428571428571369, 0.1130952380952380959, 0.1190476190476190410, 0.1250000000000000000, 0.1309523809523809590, 0.1369047619047619180, 0.1428571428571428492, 0.1488095238095238082, 0.1547619047619047672, 0.1607142857142857262, 0.1666666666666666574, 0.1726190476190476164, 0.1785714285714285754, 0.1845238095238095344, 0.1904761904761904656, 0.1964285714285714246, 0.2023809523809523836, 0.2083333333333333426, 0.2142857142857142738, 0.2202380952380952328, 0.2261904761904761918, 0.2321428571428571508, 0.2380952380952380820, 0.2440476190476190410, 0.2500000000000000000, 0.2559523809523809312, 0.2619047619047619180, 0.2678571428571428492, 0.2738095238095238360, 0.2797619047619047672, 0.2857142857142856984, 0.2916666666666666852, 0.2976190476190476164, 0.3035714285714285476, 0.3095238095238095344, 0.3154761904761904656, 0.3214285714285714524, 0.3273809523809523836, 0.3333333333333333148, 0.3392857142857143016, 0.3452380952380952328, 0.3511904761904761640, 0.3571428571428571508, 0.3630952380952380820, 0.3690476190476190688, 0.3750000000000000000, 0.3809523809523809312, 0.3869047619047619180, 0.3928571428571428492, 0.3988095238095238360, 0.4047619047619047672, 0.4107142857142856984, 0.4166666666666666852, 0.4226190476190476164, 0.4285714285714285476, 0.4345238095238095344, 0.4404761904761904656, 0.4464285714285714524, 0.4523809523809523836, 0.4583333333333333148, 0.4642857142857143016, 0.4702380952380952328, 0.4761904761904761640, 0.4821428571428571508, 0.4880952380952380820, 0.4940476190476190688, 0.5000000000000000000, 0.5059523809523809312, 0.5119047619047618625, 0.5178571428571429047, 0.5238095238095238360, 0.5297619047619047672, 0.5357142857142856984, 0.5416666666666666297, 0.5476190476190476719, 0.5535714285714286031, 0.5595238095238095344, 0.5654761904761904656, 0.5714285714285713969, 0.5773809523809523281, 0.5833333333333333703, 0.5892857142857143016, 0.5952380952380952328, 0.6011904761904761640, 0.6071428571428570953, 0.6130952380952381375, 0.6190476190476190688, 0.6250000000000000000, 0.6309523809523809312, 0.6369047619047618625, 0.6428571428571429047, 0.6488095238095238360, 0.6547619047619047672, 0.6607142857142856984, 0.6666666666666666297, 0.6726190476190476719, 0.6785714285714286031, 0.6845238095238095344, 0.6904761904761904656, 0.6964285714285713969, 0.7023809523809523281, 0.7083333333333333703, 0.7142857142857143016, 0.7202380952380952328, 0.7261904761904761640, 0.7321428571428570953, 0.7380952380952381375, 0.7440476190476190688, 0.7500000000000000000, 0.7559523809523809312, 0.7619047619047618625, 0.7678571428571429047, 0.7738095238095238360, 0.7797619047619047672, 0.7857142857142856984, 0.7916666666666666297, 0.7976190476190476719, 0.8035714285714286031, 0.8095238095238095344, 0.8154761904761904656, 0.8214285714285713969, 0.8273809523809523281, 0.8333333333333333703, 0.8392857142857143016, 0.8452380952380952328, 0.8511904761904761640, 0.8571428571428570953, 0.8630952380952381375, 0.8690476190476190688, 0.8750000000000000000, 0.8809523809523809312, 0.8869047619047618625, 0.8928571428571429047, 0.8988095238095238360, 0.9047619047619047672, 0.9107142857142856984, 0.9166666666666666297, 0.9226190476190476719, 0.9285714285714286031, 0.9345238095238095344, 0.9404761904761904656, 0.9464285714285713969, 0.9523809523809523281, 0.9583333333333333703, 0.9642857142857143016 ),
 .UNSPECIFIED. ) 
 GEOMETRIC_REPRESENTATION_ITEM ( )  RATIONAL_B_SPLINE_SURFACE ( (
 ( 1.000000000000000000, 0.9659258262890683122, 1.000000000000000000, 0.9659258262890683122, 1.000000000000000000, 0.9659258262890683122, 1.000000000000000000, 0.9659258262890683122, 1.000000000000000000, 0.9659258262890683122, 1.000000000000000000, 0.9659258262890683122, 1.000000000000000000, 0.9659258262890683122, 1.000000000000000000, 0.9659258262890683122, 1.000000000000000000, 0.9659258262890683122, 1.000000000000000000, 0.9659258262890683122, 1.000000000000000000, 0.9659258262890683122, 1.000000000000000000, 0.9659258262890683122, 1.000000000000000000, 0.9659258262890683122, 1.000000000000000000, 0.9659258262890683122, 1.000000000000000000, 0.9659258262890683122, 1.000000000000000000, 0.9659258262890683122, 1.000000000000000000, 0.9659258262890683122, 1.000000000000000000, 0.9659258262890683122, 1.000000000000000000, 0.9659258262890683122, 1.000000000000000000, 0.9659258262890683122, 1.000000000000000000, 0.9659258262890683122, 1.000000000000000000, 0.9659258262890683122, 1.000000000000000000, 0.9659258262890683122, 1.000000000000000000, 0.9659258262890683122, 1.000000000000000000, 0.9659258262890683122, 1.000000000000000000, 0.9659258262890683122, 1.000000000000000000, 0.9659258262890683122, 1.000000000000000000, 0.9659258262890683122, 1.000000000000000000, 0.9659258262890683122, 1.000000000000000000, 0.9659258262890683122, 1.000000000000000000, 0.9659258262890683122, 1.000000000000000000, 0.9659258262890683122, 1.000000000000000000, 0.9659258262890683122, 1.000000000000000000, 0.9659258262890683122, 1.000000000000000000, 0.9659258262890683122, 1.000000000000000000, 0.9659258262890683122, 1.000000000000000000, 0.9659258262890683122, 1.000000000000000000, 0.9659258262890683122, 1.000000000000000000, 0.9659258262890683122, 1.000000000000000000, 0.9659258262890683122, 1.000000000000000000, 0.9659258262890683122, 1.000000000000000000, 0.9659258262890683122, 1.000000000000000000, 0.9659258262890683122, 1.000000000000000000, 0.9659258262890683122, 1.000000000000000000, 0.9659258262890683122, 1.000000000000000000, 0.9659258262890683122, 1.000000000000000000, 0.9659258262890683122, 1.000000000000000000, 0.9659258262890683122, 1.000000000000000000, 0.9659258262890683122, 1.000000000000000000, 0.9659258262890683122, 1.000000000000000000, 0.9659258262890683122, 1.000000000000000000, 0.9659258262890683122, 1.000000000000000000, 0.9659258262890683122, 1.000000000000000000, 0.9659258262890683122, 1.000000000000000000, 0.9659258262890683122, 1.000000000000000000, 0.9659258262890683122, 1.000000000000000000, 0.9659258262890683122, 1.000000000000000000, 0.9659258262890683122, 1.000000000000000000, 0.9659258262890683122, 1.000000000000000000, 0.9659258262890683122, 1.000000000000000000, 0.9659258262890683122, 1.000000000000000000, 0.9659258262890683122, 1.000000000000000000, 0.9659258262890683122, 1.000000000000000000, 0.9659258262890683122, 1.000000000000000000, 0.9659258262890683122, 1.000000000000000000, 0.9659258262890683122, 1.000000000000000000, 0.9659258262890683122, 1.000000000000000000, 0.9659258262890683122, 1.000000000000000000, 0.9659258262890683122, 1.000000000000000000, 0.9659258262890683122, 1.000000000000000000, 0.9659258262890683122, 1.000000000000000000, 0.9659258262890683122, 1.000000000000000000, 0.9659258262890683122, 1.000000000000000000, 0.9659258262890683122, 1.000000000000000000, 0.9659258262890683122, 1.000000000000000000, 0.9659258262890683122, 1.000000000000000000, 0.9659258262890683122, 1.000000000000000000, 0.9659258262890683122, 1.000000000000000000, 0.9659258262890683122, 1.000000000000000000, 0.9659258262890683122, 1.000000000000000000, 0.9659258262890683122, 1.000000000000000000, 0.9659258262890683122, 1.000000000000000000, 0.9659258262890683122, 1.000000000000000000, 0.9659258262890683122, 1.000000000000000000, 0.9659258262890683122, 1.000000000000000000, 0.9659258262890683122, 1.000000000000000000, 0.9659258262890683122, 1.000000000000000000, 0.9659258262890683122, 1.000000000000000000, 0.9659258262890683122, 1.000000000000000000, 0.9659258262890683122, 1.000000000000000000, 0.9659258262890683122, 1.000000000000000000, 0.9659258262890683122, 1.000000000000000000, 0.9659258262890683122, 1.000000000000000000, 0.9659258262890683122, 1.000000000000000000, 0.9659258262890683122, 1.000000000000000000, 0.9659258262890683122, 1.000000000000000000, 0.9659258262890683122, 1.000000000000000000, 0.9659258262890683122, 1.000000000000000000, 0.9659258262890683122, 1.000000000000000000, 0.9659258262890683122, 1.000000000000000000, 0.9659258262890683122, 1.000000000000000000, 0.9659258262890683122, 1.000000000000000000, 0.9659258262890683122, 1.000000000000000000, 0.9659258262890683122, 1.000000000000000000, 0.9659258262890683122, 1.000000000000000000, 0.9659258262890683122, 1.000000000000000000, 0.9659258262890683122, 1.000000000000000000, 0.9659258262890683122, 1.000000000000000000, 0.9659258262890683122, 1.000000000000000000, 0.9659258262890683122, 1.000000000000000000, 0.9659258262890683122, 1.000000000000000000, 0.9659258262890683122, 1.000000000000000000, 0.9659258262890683122, 1.000000000000000000, 0.9659258262890683122, 1.000000000000000000, 0.9659258262890683122, 1.000000000000000000, 0.9659258262890683122, 1.000000000000000000, 0.9659258262890683122, 1.000000000000000000, 0.9659258262890683122, 1.000000000000000000, 0.9659258262890683122, 1.000000000000000000, 0.9659258262890683122, 1.000000000000000000, 0.9659258262890683122, 1.000000000000000000, 0.9659258262890683122, 1.000000000000000000, 0.9659258262890683122, 1.000000000000000000, 0.9659258262890683122, 1.000000000000000000, 0.9659258262890683122, 1.000000000000000000, 0.9659258262890683122, 1.000000000000000000, 0.9659258262890683122, 1.000000000000000000, 0.9659258262890683122, 1.000000000000000000, 0.9659258262890683122, 1.000000000000000000, 0.9659258262890683122, 1.000000000000000000, 0.9659258262890683122, 1.000000000000000000, 0.9659258262890683122, 1.000000000000000000, 0.9659258262890683122, 1.000000000000000000, 0.9659258262890683122, 1.000000000000000000, 0.9659258262890683122, 1.000000000000000000, 0.9659258262890683122, 1.000000000000000000, 0.9659258262890683122, 1.000000000000000000, 0.9659258262890683122, 1.000000000000000000, 0.9659258262890683122, 1.000000000000000000, 0.9659258262890683122, 1.000000000000000000, 0.9659258262890683122, 1.000000000000000000, 0.9659258262890683122, 1.000000000000000000, 0.9659258262890683122, 1.000000000000000000, 0.9659258262890683122, 1.000000000000000000, 0.9659258262890683122, 1.000000000000000000, 0.9659258262890683122, 1.000000000000000000, 0.9659258262890683122, 1.000000000000000000, 0.9659258262890683122, 1.000000000000000000, 0.9659258262890683122, 1.000000000000000000, 0.9659258262890683122, 1.000000000000000000, 0.9659258262890683122, 1.000000000000000000, 0.9659258262890683122, 1.000000000000000000, 0.9659258262890683122, 1.000000000000000000, 0.9659258262890683122, 1.000000000000000000, 0.9659258262890683122, 1.000000000000000000, 0.9659258262890683122, 1.000000000000000000, 0.9659258262890683122, 1.000000000000000000, 0.9659258262890683122, 1.000000000000000000, 0.9659258262890683122, 1.000000000000000000, 0.9659258262890683122, 1.000000000000000000, 0.9659258262890683122, 1.000000000000000000, 0.9659258262890683122, 1.000000000000000000),
 ( 1.000000000000000000, 0.9659258262890683122, 1.000000000000000000, 0.9659258262890683122, 1.000000000000000000, 0.9659258262890683122, 1.000000000000000000, 0.9659258262890683122, 1.000000000000000000, 0.9659258262890683122, 1.000000000000000000, 0.9659258262890683122, 1.000000000000000000, 0.9659258262890683122, 1.000000000000000000, 0.9659258262890683122, 1.000000000000000000, 0.9659258262890683122, 1.000000000000000000, 0.9659258262890683122, 1.000000000000000000, 0.9659258262890683122, 1.000000000000000000, 0.9659258262890683122, 1.000000000000000000, 0.9659258262890683122, 1.000000000000000000, 0.9659258262890683122, 1.000000000000000000, 0.9659258262890683122, 1.000000000000000000, 0.9659258262890683122, 1.000000000000000000, 0.9659258262890683122, 1.000000000000000000, 0.9659258262890683122, 1.000000000000000000, 0.9659258262890683122, 1.000000000000000000, 0.9659258262890683122, 1.000000000000000000, 0.9659258262890683122, 1.000000000000000000, 0.9659258262890683122, 1.000000000000000000, 0.9659258262890683122, 1.000000000000000000, 0.9659258262890683122, 1.000000000000000000, 0.9659258262890683122, 1.000000000000000000, 0.9659258262890683122, 1.000000000000000000, 0.9659258262890683122, 1.000000000000000000, 0.9659258262890683122, 1.000000000000000000, 0.9659258262890683122, 1.000000000000000000, 0.9659258262890683122, 1.000000000000000000, 0.9659258262890683122, 1.000000000000000000, 0.9659258262890683122, 1.000000000000000000, 0.9659258262890683122, 1.000000000000000000, 0.9659258262890683122, 1.000000000000000000, 0.9659258262890683122, 1.000000000000000000, 0.9659258262890683122, 1.000000000000000000, 0.9659258262890683122, 1.000000000000000000, 0.9659258262890683122, 1.000000000000000000, 0.9659258262890683122, 1.000000000000000000, 0.9659258262890683122, 1.000000000000000000, 0.9659258262890683122, 1.000000000000000000, 0.9659258262890683122, 1.000000000000000000, 0.9659258262890683122, 1.000000000000000000, 0.9659258262890683122, 1.000000000000000000, 0.9659258262890683122, 1.000000000000000000, 0.9659258262890683122, 1.000000000000000000, 0.9659258262890683122, 1.000000000000000000, 0.9659258262890683122, 1.000000000000000000, 0.9659258262890683122, 1.000000000000000000, 0.9659258262890683122, 1.000000000000000000, 0.9659258262890683122, 1.000000000000000000, 0.9659258262890683122, 1.000000000000000000, 0.9659258262890683122, 1.000000000000000000, 0.9659258262890683122, 1.000000000000000000, 0.9659258262890683122, 1.000000000000000000, 0.9659258262890683122, 1.000000000000000000, 0.9659258262890683122, 1.000000000000000000, 0.9659258262890683122, 1.000000000000000000, 0.9659258262890683122, 1.000000000000000000, 0.9659258262890683122, 1.000000000000000000, 0.9659258262890683122, 1.000000000000000000, 0.9659258262890683122, 1.000000000000000000, 0.9659258262890683122, 1.000000000000000000, 0.9659258262890683122, 1.000000000000000000, 0.9659258262890683122, 1.000000000000000000, 0.9659258262890683122, 1.000000000000000000, 0.9659258262890683122, 1.000000000000000000, 0.9659258262890683122, 1.000000000000000000, 0.9659258262890683122, 1.000000000000000000, 0.9659258262890683122, 1.000000000000000000, 0.9659258262890683122, 1.000000000000000000, 0.9659258262890683122, 1.000000000000000000, 0.9659258262890683122, 1.000000000000000000, 0.9659258262890683122, 1.000000000000000000, 0.9659258262890683122, 1.000000000000000000, 0.9659258262890683122, 1.000000000000000000, 0.9659258262890683122, 1.000000000000000000, 0.9659258262890683122, 1.000000000000000000, 0.9659258262890683122, 1.000000000000000000, 0.9659258262890683122, 1.000000000000000000, 0.9659258262890683122, 1.000000000000000000, 0.9659258262890683122, 1.000000000000000000, 0.9659258262890683122, 1.000000000000000000, 0.9659258262890683122, 1.000000000000000000, 0.9659258262890683122, 1.000000000000000000, 0.9659258262890683122, 1.000000000000000000, 0.9659258262890683122, 1.000000000000000000, 0.9659258262890683122, 1.000000000000000000, 0.9659258262890683122, 1.000000000000000000, 0.9659258262890683122, 1.000000000000000000, 0.9659258262890683122, 1.000000000000000000, 0.9659258262890683122, 1.000000000000000000, 0.9659258262890683122, 1.000000000000000000, 0.9659258262890683122, 1.000000000000000000, 0.9659258262890683122, 1.000000000000000000, 0.9659258262890683122, 1.000000000000000000, 0.9659258262890683122, 1.000000000000000000, 0.9659258262890683122, 1.000000000000000000, 0.9659258262890683122, 1.000000000000000000, 0.9659258262890683122, 1.000000000000000000, 0.9659258262890683122, 1.000000000000000000, 0.9659258262890683122, 1.000000000000000000, 0.9659258262890683122, 1.000000000000000000, 0.9659258262890683122, 1.000000000000000000, 0.9659258262890683122, 1.000000000000000000, 0.9659258262890683122, 1.000000000000000000, 0.9659258262890683122, 1.000000000000000000, 0.9659258262890683122, 1.000000000000000000, 0.9659258262890683122, 1.000000000000000000, 0.9659258262890683122, 1.000000000000000000, 0.9659258262890683122, 1.000000000000000000, 0.9659258262890683122, 1.000000000000000000, 0.9659258262890683122, 1.000000000000000000, 0.9659258262890683122, 1.000000000000000000, 0.9659258262890683122, 1.000000000000000000, 0.9659258262890683122, 1.000000000000000000, 0.9659258262890683122, 1.000000000000000000, 0.9659258262890683122, 1.000000000000000000, 0.9659258262890683122, 1.000000000000000000, 0.9659258262890683122, 1.000000000000000000, 0.9659258262890683122, 1.000000000000000000, 0.9659258262890683122, 1.000000000000000000, 0.9659258262890683122, 1.000000000000000000, 0.9659258262890683122, 1.000000000000000000, 0.9659258262890683122, 1.000000000000000000, 0.9659258262890683122, 1.000000000000000000, 0.9659258262890683122, 1.000000000000000000, 0.9659258262890683122, 1.000000000000000000, 0.9659258262890683122, 1.000000000000000000, 0.9659258262890683122, 1.000000000000000000, 0.9659258262890683122, 1.000000000000000000, 0.9659258262890683122, 1.000000000000000000, 0.9659258262890683122, 1.000000000000000000, 0.9659258262890683122, 1.000000000000000000, 0.9659258262890683122, 1.000000000000000000, 0.9659258262890683122, 1.000000000000000000, 0.9659258262890683122, 1.000000000000000000, 0.9659258262890683122, 1.000000000000000000, 0.9659258262890683122, 1.000000000000000000, 0.9659258262890683122, 1.000000000000000000, 0.9659258262890683122, 1.000000000000000000, 0.9659258262890683122, 1.000000000000000000, 0.9659258262890683122, 1.000000000000000000, 0.9659258262890683122, 1.000000000000000000, 0.9659258262890683122, 1.000000000000000000, 0.9659258262890683122, 1.000000000000000000, 0.9659258262890683122, 1.000000000000000000, 0.9659258262890683122, 1.000000000000000000, 0.9659258262890683122, 1.000000000000000000, 0.9659258262890683122, 1.000000000000000000, 0.9659258262890683122, 1.000000000000000000, 0.9659258262890683122, 1.000000000000000000, 0.9659258262890683122, 1.000000000000000000, 0.9659258262890683122, 1.000000000000000000, 0.9659258262890683122, 1.000000000000000000, 0.9659258262890683122, 1.000000000000000000, 0.9659258262890683122, 1.000000000000000000, 0.9659258262890683122, 1.000000000000000000, 0.9659258262890683122, 1.000000000000000000, 0.9659258262890683122, 1.000000000000000000, 0.9659258262890683122, 1.000000000000000000, 0.9659258262890683122, 1.000000000000000000) ) ) 
 REPRESENTATION_ITEM ( '' )  SURFACE ( )  );
#6650 = EDGE_LOOP ( 'NONE', ( #51499, #60296, #62086, #64666 ) ) ;
#6651 = ORIENTED_EDGE ( 'NONE', *, *, #48371, .F. ) ;
#6652 = AXIS2_PLACEMENT_3D ( 'NONE', #63315, #69860, #62832 ) ;
#6653 = CARTESIAN_POINT ( 'NONE',  ( -14.40939250469963895, 4.354406223596783273E-16, -1.618458416365949226 ) ) ;
#6654 = CARTESIAN_POINT ( 'NONE',  ( 10.00000000000000178, 18.05374883491396787, 14.16423886937410082 ) ) ;
#6655 = CARTESIAN_POINT ( 'NONE',  ( 24.16423886937409904, 19.09541550158063927, 3.795296366450317205 ) ) ;
#6656 = CARTESIAN_POINT ( 'NONE',  ( 17.96484262340118221, 59.93868534415484106, 7.964842623401181321 ) ) ;
#6657 = CARTESIAN_POINT ( 'NONE',  ( 10.00000000000000000, 1.813685344154838175, -10.88017736071110342 ) ) ;
#6658 = CARTESIAN_POINT ( 'NONE',  ( -1.099225684535947600, -0.4596986634029132657, 6.408140936763237150 ) ) ;
#6659 = CARTESIAN_POINT ( 'NONE',  ( 17.20831665107776587, 42.88393115100077324, 7.208316651077764980 ) ) ;
#6660 = CARTESIAN_POINT ( 'NONE',  ( -11.58433430580200607, -69.52997016218412796, 4.000000000003603340 ) ) ;
#6662 = CARTESIAN_POINT ( 'NONE',  ( 21.09922568453594849, 1.206968003263753531, 6.408140936763242479 ) ) ;
#6661 = CARTESIAN_POINT ( 'NONE',  ( 0.5774900079438590739, 52.64701867748817676, -5.440088680355550821 ) ) ;
#6663 = CARTESIAN_POINT ( 'NONE',  ( 24.16423886937409904, 14.09541550158063217, 3.795296366450317205 ) ) ;
#6664 = CARTESIAN_POINT ( 'NONE',  ( -0.8801773607110991993, 12.85535201082150358, -2.915334737309923874 ) ) ;
#6665 = CARTESIAN_POINT ( 'NONE',  ( 7.084665262690076126, 12.02201867748817321, -10.88017736071110164 ) ) ;
#6666 = CARTESIAN_POINT ( 'NONE',  ( -0.3289641300568009741, 2.245456701841137548, -5.963430220938281678 ) ) ;
#6667 = CARTESIAN_POINT ( 'NONE',  ( 10.00000000000000178, 54.31368534415484106, 10.88017736071110342 ) ) ;
#6668 = CARTESIAN_POINT ( 'NONE',  ( 19.38216949554541557, 47.24863466993041783, -9.382169495545420901 ) ) ;
#6669 = CARTESIAN_POINT ( 'NONE',  ( -3.469446951953614189E-15, -25.24106884899920900, -9.846743663894594434 ) ) ;
#6670 = ORIENTED_EDGE ( 'NONE', *, *, #86362, .F. ) ;
#6671 = CARTESIAN_POINT ( 'NONE',  ( -46.20903833114419967, 103.7402771300235855, -6.114030023718171059 ) ) ;
#6672 = ORIENTED_EDGE ( 'NONE', *, *, #25922, .T. ) ;
#6673 = ORIENTED_EDGE ( 'NONE', *, *, #69829, .F. ) ;
#6674 = CARTESIAN_POINT ( 'NONE',  ( -0.1503990784575242878, 19.24884699246888786, -6.262539305110083276 ) ) ;
#6676 = CARTESIAN_POINT ( 'NONE',  ( 24.16423886937410614, 64.51208216824728936, -3.795296366450302550 ) ) ;
#6675 = CARTESIAN_POINT ( 'NONE',  ( 20.36894250292379738, 49.92874883491396787, -10.36894250292379027 ) ) ;
#6678 = CARTESIAN_POINT ( 'NONE',  ( 19.84674366389459266, 48.71726448433413026, -2.638427012816827677 ) ) ;
#6677 = CARTESIAN_POINT ( 'NONE',  ( 14.92337183194729988, 29.34226448433411960, -8.527530157486177487 ) ) ;
#6679 = DIRECTION ( 'NONE',  ( 0.000000000000000000, 0.000000000000000000, -1.000000000000000000 ) ) ;
#6680 = CIRCLE ( 'NONE', #54551, 8.250000000000007105 ) ;
#6681 = CARTESIAN_POINT ( 'NONE',  ( 19.84674366389459266, 3.300597817667451750, 2.638427012816836559 ) ) ;
#6682 = EDGE_CURVE ( 'NONE', #66913, #69767, #42313, .T. ) ;
#6683 = CARTESIAN_POINT ( 'NONE',  ( 11.09922568453594671, 22.04030133659709634, -6.408140936763241591 ) ) ;
#6684 = EDGE_CURVE ( 'NONE', #42806, #68457, #93409, .T. ) ;
#6685 = ORIENTED_EDGE ( 'NONE', *, *, #23632, .F. ) ;
#6686 = AXIS2_PLACEMENT_3D ( 'NONE', #65324, #88338, #52796 ) ;
#6687 = CARTESIAN_POINT ( 'NONE',  ( 6.204703633549690345, 32.84541550158063927, 14.16423886937410082 ) ) ;
#6688 = CARTESIAN_POINT ( 'NONE',  ( -1.099225684535947600, 29.54030133659708923, 6.408140936763237150 ) ) ;
#6689 = ORIENTED_EDGE ( 'NONE', *, *, #1534, .T. ) ;
#6690 = CARTESIAN_POINT ( 'NONE',  ( -2.816281873526473856, 64.12363466993042493, 9.499525473075851096E-16 ) ) ;
#6691 = CARTESIAN_POINT ( 'NONE',  ( 7.084665262690076126, 29.10535201082150181, 10.88017736071109987 ) ) ;
#6692 = CARTESIAN_POINT ( 'NONE',  ( 19.84674366389459266, 33.71726448433410894, -2.638427012816827677 ) ) ;
#6693 = CARTESIAN_POINT ( 'NONE',  ( -0.8801773607111009756, 33.06368534415484106, 1.068504757029289695E-15 ) ) ;
#6694 = MECHANICAL_DESIGN_GEOMETRIC_PRESENTATION_REPRESENTATION (  '', ( #22697 ), #80123 ) ;
#6695 = CARTESIAN_POINT ( 'NONE',  ( 19.38216949554541557, 62.24863466993041072, -9.382169495545420901 ) ) ;
#6696 = CARTESIAN_POINT ( 'NONE',  ( -3.715841784917612856, -0.03417435944610275333, -15.55859621770273193 ) ) ;
#6697 = CARTESIAN_POINT ( 'NONE',  ( 10.00000000000000000, 44.75893115100078745, -9.846743663894594434 ) ) ;
#6698 = CARTESIAN_POINT ( 'NONE',  ( 0.1532563361054082862, 56.21726448433411605, 2.638427012816831674 ) ) ;
#6699 = DIRECTION ( 'NONE',  ( -0.000000000000000000, -1.000000000000000000, -0.000000000000000000 ) ) ;
#6700 = ORIENTED_EDGE ( 'NONE', *, *, #93124, .T. ) ;
#6701 = FACE_OUTER_BOUND ( 'NONE', #42927, .T. ) ;
#6702 = CARTESIAN_POINT ( 'NONE',  ( 0.000000000000000000, 14.49999999999999822, 0.000000000000000000 ) ) ;
#6703 = CARTESIAN_POINT ( 'NONE',  ( 14.35000000000000142, 98.50000000000001421, -8.000000000000000000 ) ) ;
#6704 = CARTESIAN_POINT ( 'NONE',  ( -12.50534872682736065, 15.00000000000000000, 7.339363270777414350 ) ) ;
#6705 = CARTESIAN_POINT ( 'NONE',  ( 18.52753015748618282, 13.92559781766745175, -4.923371831947291888 ) ) ;
#6706 = CARTESIAN_POINT ( 'NONE',  ( 0.6178305044545838731, 34.74863466993042493, 9.382169495545420901 ) ) ;
#6707 = CARTESIAN_POINT ( 'NONE',  ( -3.999999999999999112, 23.03999999999999915, 0.000000000000000000 ) ) ;
#6708 = EDGE_CURVE ( 'NONE', #22423, #28167, #51881, .T. ) ;
#6709 = ORIENTED_EDGE ( 'NONE', *, *, #20199, .T. ) ;
#6710 = CARTESIAN_POINT ( 'NONE',  ( 7.361572987183169658, 54.96726448433413026, -9.846743663894592657 ) ) ;
#6711 = DIRECTION ( 'NONE',  ( 0.000000000000000000, 0.000000000000000000, 1.000000000000000000 ) ) ;
#6712 = CARTESIAN_POINT ( 'NONE',  ( 19.84674366389459266, 43.71726448433410894, -2.638427012816827677 ) ) ;
#6713 = CARTESIAN_POINT ( 'NONE',  ( 24.16423886937409904, 29.09541550158063572, 3.795296366450317205 ) ) ;
#6714 = CARTESIAN_POINT ( 'NONE',  ( 14.92337183194729988, 49.34226448433411605, -8.527530157486177487 ) ) ;
#6715 = CARTESIAN_POINT ( 'NONE',  ( 22.81628187352648496, 46.83196800326376064, -3.434112377981050290 ) ) ;
#6717 = CARTESIAN_POINT ( 'NONE',  ( 1.816707512666851709, 10.10290668512023338, -6.499999999999988454 ) ) ;
#6716 = DIRECTION ( 'NONE',  ( -1.000000000000000000, 0.000000000000000000, -0.000000000000000000 ) ) ;
#6718 = CARTESIAN_POINT ( 'NONE',  ( 18.52753015748617571, 3.092264484334118269, 4.923371831947298993 ) ) ;
#6719 = CARTESIAN_POINT ( 'NONE',  ( 24.16423886937410614, 4.512082168247300906, -3.795296366450302550 ) ) ;
#6720 = CARTESIAN_POINT ( 'NONE',  ( 10.00000000000000000, 54.75893115100078745, -9.846743663894594434 ) ) ;
#6721 = CARTESIAN_POINT ( 'NONE',  ( 17.96484262340118221, 34.93868534415482685, 7.964842623401181321 ) ) ;
#6722 = CARTESIAN_POINT ( 'NONE',  ( 1.472469842513823179, 45.59226448433412315, -4.923371831947296329 ) ) ;
#6723 = SHAPE_DEFINITION_REPRESENTATION ( #13299, #53719 ) ;
#6724 = FACE_OUTER_BOUND ( 'NONE', #70596, .T. ) ;
#6725 = AXIS2_PLACEMENT_3D ( 'NONE', #87202, #18230, #1770 ) ;
#6726 = CARTESIAN_POINT ( 'NONE',  ( 20.88017736071110519, 50.56368534415484106, 2.639326808657452039E-16 ) ) ;
#6727 = ORIENTED_EDGE ( 'NONE', *, *, #91334, .F. ) ;
#6728 = DIRECTION ( 'NONE',  ( 0.000000000000000000, 0.000000000000000000, 1.000000000000000000 ) ) ;
#6729 = CARTESIAN_POINT ( 'NONE',  ( 12.91533473730993009, 21.60535201082150536, -10.88017736071109987 ) ) ;
#6731 = CARTESIAN_POINT ( 'NONE',  ( 2.035157376598824452, 38.68868534415483396, 7.964842623401179544 ) ) ;
#6730 = CARTESIAN_POINT ( 'NONE',  ( 5.076628168052704559, 65.17559781766745175, -8.527530157486179263 ) ) ;
#6732 = CARTESIAN_POINT ( 'NONE',  ( -14.62617646268082972, 0.5000000000000004441, -3.327906561567078647 ) ) ;
#6733 = DIRECTION ( 'NONE',  ( -0.3007057995042635157, 0.000000000000000000, -0.9537169507482300412 ) ) ;
#6734 = CARTESIAN_POINT ( 'NONE',  ( 42.87872917473848844, 58.60092987214253668, -8.000000000000000000 ) ) ;
#6736 = CARTESIAN_POINT ( 'NONE',  ( 20.00000000000000711, 92.18909449965150316, -4.886738312308601451 ) ) ;
#6735 = CARTESIAN_POINT ( 'NONE',  ( 20.88017736071110875, 35.77201867748816966, -2.915334737309920765 ) ) ;
#6737 = CARTESIAN_POINT ( 'NONE',  ( 17.20831665107776587, 14.13393115100078568, -7.208316651077762316 ) ) ;
#6738 = PRODUCT_DEFINITION_SHAPE ( 'NONE', 'NONE',  #4342 ) ;
#6739 = CARTESIAN_POINT ( 'NONE',  ( 7.361572987183170547, 27.05059781766745175, 9.846743663894590881 ) ) ;
#6740 = FACE_OUTER_BOUND ( 'NONE', #43969, .T. ) ;
#6741 = CARTESIAN_POINT ( 'NONE',  ( 10.36894250292378850, 19.92874883491397497, -10.36894250292379027 ) ) ;
#6742 = CARTESIAN_POINT ( 'NONE',  ( 6.565887622018943937, 0.1653013365970866511, 12.81628187352647430 ) ) ;
#6743 = CARTESIAN_POINT ( 'NONE',  ( 10.00000000000000178, 68.05374883491397497, 14.16423886937410082 ) ) ;
#6744 = DIRECTION ( 'NONE',  ( -0.000000000000000000, -0.000000000000000000, -1.000000000000000000 ) ) ;
#6745 = CARTESIAN_POINT ( 'NONE',  ( 10.00000000000000178, 23.05374883491397142, 14.16423886937410082 ) ) ;
#6746 = CARTESIAN_POINT ( 'NONE',  ( -4.164238869374099927, 57.01208216824731068, 3.795296366450308767 ) ) ;
#6747 = CIRCLE ( 'NONE', #67415, 0.2500000000000002220 ) ;
#6748 = DIRECTION ( 'NONE',  ( 0.000000000000000000, 0.000000000000000000, 1.000000000000000000 ) ) ;
#6749 = VERTEX_POINT ( 'NONE', #57884 ) ;
#6750 = CARTESIAN_POINT ( 'NONE',  ( 19.84674366389459266, 28.30059781766745886, 2.638427012816836559 ) ) ;
#6751 = CARTESIAN_POINT ( 'NONE',  ( 12.91533473730992121, 14.52201867748817143, 10.88017736071110164 ) ) ;
#6752 = CARTESIAN_POINT ( 'NONE',  ( 19.84674366389459621, 53.50893115100078745, 7.409399052514197653E-17 ) ) ;
#6754 = LINE ( 'NONE', #70713, #24832 ) ;
#6753 = CARTESIAN_POINT ( 'NONE',  ( -4.164238869374099039, 11.80374883491396965, 8.674139862899312516E-16 ) ) ;
#6755 = CARTESIAN_POINT ( 'NONE',  ( 14.49999999999999822, 60.50000000000000000, 5.000000000000000000 ) ) ;
#6756 = CIRCLE ( 'NONE', #35510, 0.2499999999999978351 ) ;
#6757 = CIRCLE ( 'NONE', #30722, 6.599999999999995204 ) ;
#6758 = CARTESIAN_POINT ( 'NONE',  ( 2.791683348922237240, 0.3839311510007847872, -7.208316651077763204 ) ) ;
#6759 = CARTESIAN_POINT ( 'NONE',  ( 22.81628187352647785, 36.41530133659707502, 3.434112377981063169 ) ) ;
#6760 = CARTESIAN_POINT ( 'NONE',  ( 19.84674366389459266, 38.71726448433412315, -2.638427012816827677 ) ) ;
#6761 = ORIENTED_EDGE ( 'NONE', *, *, #32079, .F. ) ;
#6762 = CARTESIAN_POINT ( 'NONE',  ( 19.84674366389459266, 13.30059781766745353, 2.638427012816836559 ) ) ;
#6763 = AXIS2_PLACEMENT_3D ( 'NONE', #6170, #73664, #67162 ) ;
#6764 = CARTESIAN_POINT ( 'NONE',  ( 11.08992015845062262, -87.81706477660959820, -4.000000000000000000 ) ) ;
#6765 = CARTESIAN_POINT ( 'NONE',  ( 20.15039907845753575, 16.74884699246888431, 6.262539305110077059 ) ) ;
#6766 = CARTESIAN_POINT ( 'NONE',  ( 4.559911319644449179, 17.23035201082150536, -9.422509992056141925 ) ) ;
#6767 = CARTESIAN_POINT ( 'NONE',  ( 10.00000000000000000, 60.55374883491397497, -14.16423886937410082 ) ) ;
#6768 = CARTESIAN_POINT ( 'NONE',  ( 4.559911319644449179, 68.89701867748817676, 9.422509992056141925 ) ) ;
#6769 = CARTESIAN_POINT ( 'NONE',  ( 20.15039907845753220, 40.60158574516643171, -6.262539305110077947 ) ) ;
#6770 = CARTESIAN_POINT ( 'NONE',  ( 18.52753015748617571, 18.09226448433411960, 4.923371831947298993 ) ) ;
#6771 = CARTESIAN_POINT ( 'NONE',  ( 19.42250999205614193, 10.14701867748816966, 5.440088680355555262 ) ) ;
#6772 = CARTESIAN_POINT ( 'NONE',  ( 2.791683348922237240, 0.3839311510007847872, -7.208316651077763204 ) ) ;
#6773 = AXIS2_PLACEMENT_3D ( 'NONE', #92335, #68370, #8347 ) ;
#6774 =( LENGTH_UNIT ( ) NAMED_UNIT ( * ) SI_UNIT ( .MILLI., .METRE. ) );
#6775 = CARTESIAN_POINT ( 'NONE',  ( 7.361572987183169658, 44.96726448433412315, -9.846743663894592657 ) ) ;
#6776 = EDGE_CURVE ( 'NONE', #4994, #23295, #36530, .T. ) ;
#6777 = CARTESIAN_POINT ( 'NONE',  ( 15.44008868035555260, 39.73035201082150536, 9.422509992056143702 ) ) ;
#6778 = ORIENTED_EDGE ( 'NONE', *, *, #35765, .T. ) ;
#6779 = CARTESIAN_POINT ( 'NONE',  ( 10.00000000000000178, 55.37363466993042493, 12.81628187352647608 ) ) ;
#6780 = CARTESIAN_POINT ( 'NONE',  ( 2.791683348922240793, 6.633931151000785675, 7.208316651077764092 ) ) ;
#6781 = CARTESIAN_POINT ( 'NONE',  ( 16.40814093676323893, 40.79030133659708923, 11.09922568453595026 ) ) ;
#6783 = CARTESIAN_POINT ( 'NONE',  ( 17.20831665107776587, 37.88393115100078745, 7.208316651077764980 ) ) ;
#6782 = CARTESIAN_POINT ( 'NONE',  ( -0.8801773607110991993, 12.85535201082150358, -2.915334737309923874 ) ) ;
#6784 =( LENGTH_UNIT ( ) NAMED_UNIT ( * ) SI_UNIT ( .MILLI., .METRE. ) );
#6785 = FILL_AREA_STYLE ('',( #98807 ) ) ;
#6786 = CARTESIAN_POINT ( 'NONE',  ( 24.16423886937410614, 34.51208216824731068, -3.795296366450302550 ) ) ;
#6787 = CARTESIAN_POINT ( 'NONE',  ( 13.79529636645031943, 45.34541550158062506, -14.16423886937409904 ) ) ;
#6788 = CARTESIAN_POINT ( 'NONE',  ( 5.076628168052704559, 55.17559781766745175, -8.527530157486179263 ) ) ;
#6789 = CARTESIAN_POINT ( 'NONE',  ( 17.35999999999999943, 33.99999999999997158, 9.500000000000000000 ) ) ;
#6790 = CARTESIAN_POINT ( 'NONE',  ( 2.035157376598822676, 42.43868534415483396, -7.964842623401177768 ) ) ;
#6791 = CARTESIAN_POINT ( 'NONE',  ( 7.361572987183169658, 4.967264484334119601, -9.846743663894592657 ) ) ;
#6792 = CIRCLE ( 'NONE', #57867, 0.2500000000000002220 ) ;
#6793 = PRESENTATION_STYLE_ASSIGNMENT (( #14808 ) ) ;
#6794 = ORIENTED_EDGE ( 'NONE', *, *, #69233, .F. ) ;
#6795 = CARTESIAN_POINT ( 'NONE',  ( 3.591859063236761518, 64.95696800326376774, 11.09922568453594849 ) ) ;
#6796 = CARTESIAN_POINT ( 'NONE',  ( 20.88017736071110519, 60.56368534415484106, 2.639326808657452039E-16 ) ) ;
#6797 = ORIENTED_EDGE ( 'NONE', *, *, #50588, .T. ) ;
#6798 = CARTESIAN_POINT ( 'NONE',  ( -4.164238869374099927, 12.01208216824730357, 3.795296366450308767 ) ) ;
#6799 = CARTESIAN_POINT ( 'NONE',  ( 10.00000000000000000, 4.758931151000784787, -9.846743663894594434 ) ) ;
#6800 = CARTESIAN_POINT ( 'NONE',  ( 20.88017736071110164, 25.35535201082150891, 2.915334737309930979 ) ) ;
#6801 = ORIENTED_EDGE ( 'NONE', *, *, #18314, .F. ) ;
#6802 = CARTESIAN_POINT ( 'NONE',  ( 7.084665262690076126, 24.10535201082150181, 10.88017736071109987 ) ) ;
#6803 = CIRCLE ( 'NONE', #62663, 14.49999999999999822 ) ;
#6804 = EDGE_CURVE ( 'NONE', #97117, #46057, #21886, .T. ) ;
#6805 = EDGE_CURVE ( 'NONE', #48230, #25555, #61427, .T. ) ;
#6806 = ORIENTED_EDGE ( 'NONE', *, *, #49225, .F. ) ;
#6807 = CARTESIAN_POINT ( 'NONE',  ( 17.96484262340118221, 36.18868534415484106, -7.964842623401177768 ) ) ;
#6808 = DIRECTION ( 'NONE',  ( 0.000000000000000000, 0.000000000000000000, 1.000000000000000000 ) ) ;
#6809 = ORIENTED_EDGE ( 'NONE', *, *, #79708, .T. ) ;
#6810 = ORIENTED_EDGE ( 'NONE', *, *, #86183, .T. ) ;
#6811 = CARTESIAN_POINT ( 'NONE',  ( 2.035157376598822676, 62.43868534415483396, -7.964842623401177768 ) ) ;
#6812 = DIRECTION ( 'NONE',  ( 0.000000000000000000, 1.000000000000000000, 0.000000000000000000 ) ) ;
#6814 = CARTESIAN_POINT ( 'NONE',  ( 11.24699797944280100, 54.09857164847241506, -3.000000000000000000 ) ) ;
#6813 = CARTESIAN_POINT ( 'NONE',  ( 0.5774900079438607392, 18.48035201082150536, 5.440088680355550821 ) ) ;
#6815 = CARTESIAN_POINT ( 'NONE',  ( 0.1532563361054082862, 1.217264484334117824, 2.638427012816831674 ) ) ;
#6816 = CARTESIAN_POINT ( 'NONE',  ( 12.91533473730992121, 14.52201867748817143, 10.88017736071110164 ) ) ;
#6817 = COLOUR_RGB ( '', 0.40784314, 0.44705882, 0.49803922) ;
#6818 = ORIENTED_EDGE ( 'NONE', *, *, #66898, .F. ) ;
#6819 = CARTESIAN_POINT ( 'NONE',  ( 19.38216949554541557, 57.24863466993042493, -9.382169495545420901 ) ) ;
#6820 = CARTESIAN_POINT ( 'NONE',  ( 0.5774900079438607392, 38.48035201082150536, 5.440088680355550821 ) ) ;
#6821 = CARTESIAN_POINT ( 'NONE',  ( -0.3289641300568009741, 22.24545670184114243, -5.963430220938281678 ) ) ;
#6822 = CARTESIAN_POINT ( 'NONE',  ( 22.81628187352647785, 56.41530133659708213, 3.434112377981063169 ) ) ;
#6823 = CARTESIAN_POINT ( 'NONE',  ( 12.91533473730993009, 41.60535201082149825, -10.88017736071109987 ) ) ;
#6824 = VECTOR ( 'NONE', #27721, 1000.000000000000000 ) ;
#6825 = AXIS2_PLACEMENT_3D ( 'NONE', #66981, #50987, #81481 ) ;
#6826 = CARTESIAN_POINT ( 'NONE',  ( 1.472469842513823179, 65.59226448433412315, -4.923371831947296329 ) ) ;
#6827 = CARTESIAN_POINT ( 'NONE',  ( -14.54804176595373555, -0.03417435944610275333, -6.650705016170777917 ) ) ;
#6828 = CARTESIAN_POINT ( 'NONE',  ( 19.84674366389459266, 18.30059781766745175, 2.638427012816836559 ) ) ;
#6829 = CARTESIAN_POINT ( 'NONE',  ( -2.816281873526473856, 59.12363466993042493, 9.499525473075851096E-16 ) ) ;
#6830 = CARTESIAN_POINT ( 'NONE',  ( 1.383448333479235348, 37.37718327197428181, -6.499999999999977796 ) ) ;
#6831 = CARTESIAN_POINT ( 'NONE',  ( 13.43411237798105340, 5.581968003263753531, 12.81628187352647963 ) ) ;
#6833 = CARTESIAN_POINT ( 'NONE',  ( 17.20831665107776587, 62.88393115100078745, 7.208316651077764980 ) ) ;
#6832 =( LENGTH_UNIT ( ) NAMED_UNIT ( * ) SI_UNIT ( .MILLI., .METRE. ) );
#6834 = CARTESIAN_POINT ( 'NONE',  ( -0.8801773607111009756, 33.06368534415484106, 1.068504757029289695E-15 ) ) ;
#6835 = CARTESIAN_POINT ( 'NONE',  ( 0.1532563361054083140, 51.00893115100078745, 1.131784320476157264E-15 ) ) ;
#6836 = CYLINDRICAL_SURFACE ( 'NONE', #34342, 0.2500000000000002220 ) ;
#6837 = EDGE_CURVE ( 'NONE', #69558, #40424, #80612, .T. ) ;
#6838 = CARTESIAN_POINT ( 'NONE',  ( 1.472469842513823179, 10.59226448433411782, -4.923371831947296329 ) ) ;
#6840 = ORIENTED_EDGE ( 'NONE', *, *, #33985, .T. ) ;
#6839 = CARTESIAN_POINT ( 'NONE',  ( -2.816281873526471635, -1.084698663402913210, -3.434112377981056508 ) ) ;
#6841 = CARTESIAN_POINT ( 'NONE',  ( 20.88017736071110519, 5.563685344154837509, 2.639326808657452039E-16 ) ) ;
#6842 =( NAMED_UNIT ( * ) SI_UNIT ( $, .STERADIAN. ) SOLID_ANGLE_UNIT ( ) );
#6843 = CARTESIAN_POINT ( 'NONE',  ( 19.84674366389459266, 63.30059781766745886, 2.638427012816836559 ) ) ;
#6844 = CARTESIAN_POINT ( 'NONE',  ( 4.441081520557000673, -2.684960557620042376, -2.500000000000000888 ) ) ;
#6845 = CARTESIAN_POINT ( 'NONE',  ( 7.084665262690076126, 7.022018677488170546, -10.88017736071110164 ) ) ;
#6846 = CARTESIAN_POINT ( 'NONE',  ( 12.63842701281683922, 39.55059781766744464, -9.846743663894590881 ) ) ;
#6847 = VERTEX_POINT ( 'NONE', #68860 ) ;
#6848 = LINE ( 'NONE', #66348, #15402 ) ;
#6849 = CARTESIAN_POINT ( 'NONE',  ( 0.5774900079438607392, 3.480352010821504916, 5.440088680355550821 ) ) ;
#6850 = CARTESIAN_POINT ( 'NONE',  ( 0.1532563361054082862, 6.217264484334118713, 2.638427012816831674 ) ) ;
#6851 = CARTESIAN_POINT ( 'NONE',  ( 12.91533473730993009, 21.60535201082150536, -10.88017736071109987 ) ) ;
#6852 = VECTOR ( 'NONE', #20822, 1000.000000000000000 ) ;
#6853 = CARTESIAN_POINT ( 'NONE',  ( -0.3689425029237898834, 51.17874883491397497, -10.36894250292378850 ) ) ;
#6855 = CARTESIAN_POINT ( 'NONE',  ( -27.43587634952537968, 29.50000000000000000, -9.500000000000000000 ) ) ;
#6854 = CARTESIAN_POINT ( 'NONE',  ( 2.917880565312948704, 67.63708216824730357, 12.26659068614894643 ) ) ;
#6856 = CARTESIAN_POINT ( 'NONE',  ( 0.1532563361054100626, 5.800597817667452638, -2.638427012816831230 ) ) ;
#6857 = CARTESIAN_POINT ( 'NONE',  ( 2.791683348922240793, 21.63393115100078745, 7.208316651077764092 ) ) ;
#6858 = CARTESIAN_POINT ( 'NONE',  ( 3.591859063236763294, 13.29030133659708746, -11.09922568453595026 ) ) ;
#6859 = EDGE_LOOP ( 'NONE', ( #14580, #4614, #64215, #56215 ) ) ;
#6860 = CARTESIAN_POINT ( 'NONE',  ( 6.728851239469101131, -3.114116630580434013E-15, -12.98580270086200628 ) ) ;
#6861 = TOROIDAL_SURFACE ( 'NONE', #91518, 1.000000000000000000, 0.5000000000000000000 ) ;
#6862 = DIRECTION ( 'NONE',  ( 0.000000000000000000, 0.000000000000000000, 1.000000000000000000 ) ) ;
#6863 = B_SPLINE_CURVE_WITH_KNOTS ( 'NONE', 3,
 ( #88681, #88184, #42214, #26698, #13176, #35685 ),
 .UNSPECIFIED., .F., .F.,
 ( 4, 2, 4 ),
 ( 3.409110551495928758E-05, 0.0004400426677367854332, 0.0008459942299586115924 ),
 .UNSPECIFIED. ) ;
#6864 = CARTESIAN_POINT ( 'NONE',  ( 5.076628168052704559, 65.17559781766745175, -8.527530157486179263 ) ) ;
#6865 = CARTESIAN_POINT ( 'NONE',  ( 20.36894250292379738, 4.928748834913967869, -10.36894250292379027 ) ) ;
#6866 = VECTOR ( 'NONE', #78764, 1000.000000000000000 ) ;
#6867 = CARTESIAN_POINT ( 'NONE',  ( 12.63842701281683922, 29.55059781766745175, -9.846743663894590881 ) ) ;
#6868 = SURFACE_STYLE_FILL_AREA ( #15374 ) ;
#6869 = EDGE_LOOP ( 'NONE', ( #67732, #17552, #6553, #46287 ) ) ;
#6870 = CARTESIAN_POINT ( 'NONE',  ( 20.36894250292379738, 34.92874883491396076, -10.36894250292379027 ) ) ;
#6871 = CARTESIAN_POINT ( 'NONE',  ( 19.84674366389459621, 13.50893115100078568, 7.409399052514197653E-17 ) ) ;
#6873 = CARTESIAN_POINT ( 'NONE',  ( -12.98685442714190508, 15.00000000000000000, -6.449155920601135072 ) ) ;
#6872 = FACE_OUTER_BOUND ( 'NONE', #76542, .T. ) ;
#6874 = CARTESIAN_POINT ( 'NONE',  ( 20.88017736071110164, 35.35535201082150536, 2.915334737309930979 ) ) ;
#6875 = CARTESIAN_POINT ( 'NONE',  ( -2.816281873526471635, 53.91530133659709634, -3.434112377981056508 ) ) ;
#6876 = CARTESIAN_POINT ( 'NONE',  ( 2.035157376598824452, 3.688685344154837953, 7.964842623401179544 ) ) ;
#6877 = CARTESIAN_POINT ( 'NONE',  ( 0.6178305044545838731, 39.74863466993041072, 9.382169495545420901 ) ) ;
#6878 = CARTESIAN_POINT ( 'NONE',  ( 5.076628168052703671, 1.842264484334118047, 8.527530157486179263 ) ) ;
#6879 = ORIENTED_EDGE ( 'NONE', *, *, #53053, .F. ) ;
#6880 = PRESENTATION_STYLE_ASSIGNMENT (( #83861 ) ) ;
#6881 = CARTESIAN_POINT ( 'NONE',  ( 1.274849032793998305, 2.555090184799397424, -6.499999999999581668 ) ) ;
#6882 = CARTESIAN_POINT ( 'NONE',  ( 13.79529636645031943, 40.34541550158063217, -14.16423886937409904 ) ) ;
#6883 = CARTESIAN_POINT ( 'NONE',  ( 2.035157376598824452, 8.688685344154839285, 7.964842623401179544 ) ) ;
#6884 = CARTESIAN_POINT ( 'NONE',  ( 19.42250999205614548, 20.98035201082150891, -5.440088680355545492 ) ) ;
#6885 = DIRECTION ( 'NONE',  ( -0.000000000000000000, -1.000000000000000000, -0.000000000000000000 ) ) ;
#6886 = LINE ( 'NONE', #12897, #3265 ) ;
#6887 = CARTESIAN_POINT ( 'NONE',  ( 4.559911319644449179, 58.89701867748817676, 9.422509992056141925 ) ) ;
#6888 = CARTESIAN_POINT ( 'NONE',  ( 4.559911319644449179, 67.23035201082150536, -9.422509992056141925 ) ) ;
#6889 = CARTESIAN_POINT ( 'NONE',  ( 6.565887622018943937, 20.16530133659708213, 12.81628187352647430 ) ) ;
#6890 = CARTESIAN_POINT ( 'NONE',  ( 0.2751277870542876980, 48.21833443783936701, 6.499999999999984901 ) ) ;
#6891 = CARTESIAN_POINT ( 'NONE',  ( -8.731067818237040257, 2.037123368507817389, -8.731067818237033151 ) ) ;
#6892 = CARTESIAN_POINT ( 'NONE',  ( 5.076628168052704559, 20.17559781766745175, -8.527530157486179263 ) ) ;
#6893 = CARTESIAN_POINT ( 'NONE',  ( 10.00000000000000000, 56.81368534415484106, -10.88017736071110342 ) ) ;
#6894 = EDGE_CURVE ( 'NONE', #9920, #69773, #55072, .T. ) ;
#6895 = AXIS2_PLACEMENT_3D ( 'NONE', #70355, #76855, #8368 ) ;
#6896 = CARTESIAN_POINT ( 'NONE',  ( 21.09922568453595559, 17.04030133659708923, -6.408140936763230044 ) ) ;
#6897 = CARTESIAN_POINT ( 'NONE',  ( 2.035157376598824452, 8.688685344154839285, 7.964842623401179544 ) ) ;
#6898 = CARTESIAN_POINT ( 'NONE',  ( 12.63842701281683034, 42.46726448433412315, 9.846743663894596210 ) ) ;
#6899 = CARTESIAN_POINT ( 'NONE',  ( 22.81628187352647785, 61.41530133659709634, 3.434112377981063169 ) ) ;
#6900 = CIRCLE ( 'NONE', #49997, 15.00000000000000000 ) ;
#6901 = CARTESIAN_POINT ( 'NONE',  ( 12.63842701281683034, 17.46726448433411250, 9.846743663894596210 ) ) ;
#6902 = VECTOR ( 'NONE', #42884, 1000.000000000000000 ) ;
#6903 = CARTESIAN_POINT ( 'NONE',  ( -4.164238869374098151, 1.595415501580634388, -3.795296366450310543 ) ) ;
#6904 = CARTESIAN_POINT ( 'NONE',  ( 5.803070148808322948, 15.00000000000000000, -13.28812917035385510 ) ) ;
#6905 = CARTESIAN_POINT ( 'NONE',  ( 20.88017736071110875, 30.77201867748816966, -2.915334737309920765 ) ) ;
#6907 = CARTESIAN_POINT ( 'NONE',  ( 10.00000000000000000, 35.55374883491396787, -14.16423886937410082 ) ) ;
#6906 = CARTESIAN_POINT ( 'NONE',  ( 4.559911319644449179, 3.897018677488170990, 9.422509992056141925 ) ) ;
#6908 = CARTESIAN_POINT ( 'NONE',  ( 19.84674366389459266, 48.71726448433413026, -2.638427012816827677 ) ) ;
#6909 = STYLED_ITEM ( 'NONE', ( #54805 ), #92469 ) ;
#6910 = CARTESIAN_POINT ( 'NONE',  ( 4.559911319644449179, 27.23035201082150536, -9.422509992056141925 ) ) ;
#6911 = CARTESIAN_POINT ( 'NONE',  ( -0.8801773607111008646, 13.27201867748817321, 2.915334737309923430 ) ) ;
#6912 = ORIENTED_EDGE ( 'NONE', *, *, #88945, .F. ) ;
#6913 = VECTOR ( 'NONE', #30304, 1000.000000000000000 ) ;
#6914 = CARTESIAN_POINT ( 'NONE',  ( 2.035157376598822676, 22.43868534415483396, -7.964842623401177768 ) ) ;
#6915 = CARTESIAN_POINT ( 'NONE',  ( 21.09922568453594849, 51.20696800326375353, 6.408140936763242479 ) ) ;
#6916 = CARTESIAN_POINT ( 'NONE',  ( 2.035157376598824452, 48.68868534415483396, 7.964842623401179544 ) ) ;
#6918 = CARTESIAN_POINT ( 'NONE',  ( 20.88017736071110519, 40.56368534415484106, 2.639326808657452039E-16 ) ) ;
#6917 = CARTESIAN_POINT ( 'NONE',  ( -12.25993886608597094, 14.49999999999999112, -8.642563219313844414 ) ) ;
#6919 = ORIENTED_EDGE ( 'NONE', *, *, #76963, .T. ) ;
#6920 = CARTESIAN_POINT ( 'NONE',  ( 12.63842701281683034, 57.46726448433411605, 9.846743663894596210 ) ) ;
#6921 = CARTESIAN_POINT ( 'NONE',  ( -0.8801773607111008646, 43.27201867748817676, 2.915334737309923430 ) ) ;
#6922 = CARTESIAN_POINT ( 'NONE',  ( 6.825238882348372726, -50.90120388559804354, 4.000000000000000000 ) ) ;
#6923 = SURFACE_SIDE_STYLE ('',( #98442 ) ) ;
#6924 = ADVANCED_FACE ( 'NONE', ( #8348 ), #7128, .T. ) ;
#6925 = CYLINDRICAL_SURFACE ( 'NONE', #61969, 0.5000000000000004441 ) ;
#6926 = CARTESIAN_POINT ( 'NONE',  ( 2.917880565312948704, 42.63708216824729647, 12.26659068614894643 ) ) ;
#6927 = CARTESIAN_POINT ( 'NONE',  ( 2.035157376598822676, 52.43868534415483396, -7.964842623401177768 ) ) ;
#6928 = CARTESIAN_POINT ( 'NONE',  ( 8.134956207566084174, -0.03417435944610275333, -13.77315809598639085 ) ) ;
#6929 = CARTESIAN_POINT ( 'NONE',  ( 10.00000000000000000, 64.75893115100078035, -9.846743663894594434 ) ) ;
#6930 = CARTESIAN_POINT ( 'NONE',  ( -0.8801773607111008646, 3.272018677488171434, 2.915334737309923430 ) ) ;
#6931 = CARTESIAN_POINT ( 'NONE',  ( 0.1532563361054083140, 36.00893115100078745, 1.131784320476157264E-15 ) ) ;
#6932 = EDGE_CURVE ( 'NONE', #96670, #30525, #91347, .T. ) ;
#6933 = ORIENTED_EDGE ( 'NONE', *, *, #25432, .F. ) ;
#6934 = CARTESIAN_POINT ( 'NONE',  ( 19.84674366389459621, 28.50893115100078745, 7.409399052514197653E-17 ) ) ;
#6935 = CARTESIAN_POINT ( 'NONE',  ( -12.81628187352647252, -15.66803199673624114, 3.434112377981066722 ) ) ;
#6936 = CARTESIAN_POINT ( 'NONE',  ( 15.44008868035555260, 24.73035201082150891, 9.422509992056143702 ) ) ;
#6937 = CARTESIAN_POINT ( 'NONE',  ( 19.84674366389459621, 28.50893115100078745, 7.409399052514197653E-17 ) ) ;
#6938 = CARTESIAN_POINT ( 'NONE',  ( -2.816281873526471635, 18.91530133659708213, -3.434112377981056508 ) ) ;
#6940 = CARTESIAN_POINT ( 'NONE',  ( -0.8801773607111008646, 58.27201867748816966, 2.915334737309923430 ) ) ;
#6939 = CARTESIAN_POINT ( 'NONE',  ( 2.148416515056620124, 37.23726573380441351, 6.499999999999959144 ) ) ;
#6942 = CARTESIAN_POINT ( 'NONE',  ( 12.91533473730992121, 4.522018677488169658, 10.88017736071110164 ) ) ;
#6941 = CARTESIAN_POINT ( 'NONE',  ( 0.5774900079438590739, 37.64701867748817676, -5.440088680355550821 ) ) ;
#6943 = CARTESIAN_POINT ( 'NONE',  ( 24.16423886937409904, 44.09541550158063927, 3.795296366450317205 ) ) ;
#6944 = AXIS2_PLACEMENT_3D ( 'NONE', #55454, #18933, #72405 ) ;
#6945 = VECTOR ( 'NONE', #38937, 1000.000000000000000 ) ;
#6946 = DIRECTION ( 'NONE',  ( -1.000000000000000000, 0.000000000000000000, -0.000000000000000000 ) ) ;
#6947 = ORIENTED_EDGE ( 'NONE', *, *, #35382, .F. ) ;
#6948 = CARTESIAN_POINT ( 'NONE',  ( 0.6178305044545818747, 13.49863466993041783, -9.382169495545419124 ) ) ;
#6949 = CARTESIAN_POINT ( 'NONE',  ( 15.44008868035555260, 4.730352010821504471, 9.422509992056143702 ) ) ;
#6950 = CARTESIAN_POINT ( 'NONE',  ( 12.91533473730993009, 46.60535201082150536, -10.88017736071109987 ) ) ;
#6951 = VERTEX_POINT ( 'NONE', #92336 ) ;
#6952 = EDGE_CURVE ( 'NONE', #49408, #717, #77320, .T. ) ;
#6953 = CARTESIAN_POINT ( 'NONE',  ( 17.96484262340118221, 54.93868534415484106, 7.964842623401181321 ) ) ;
#6954 = CARTESIAN_POINT ( 'NONE',  ( 12.63842701281683922, 39.55059781766744464, -9.846743663894590881 ) ) ;
#6955 = CARTESIAN_POINT ( 'NONE',  ( 7.361572987183169658, 24.96726448433412315, -9.846743663894592657 ) ) ;
#6956 = CARTESIAN_POINT ( 'NONE',  ( 12.63842701281683922, 9.550597817667449974, -9.846743663894590881 ) ) ;
#6957 = CARTESIAN_POINT ( 'NONE',  ( 8.879999999999991900, 76.07179676972447169, 6.500000000000000888 ) ) ;
#6958 = EDGE_CURVE ( 'NONE', #49583, #50673, #45861, .T. ) ;
#6960 = DIRECTION ( 'NONE',  ( 1.000000000000000000, 0.000000000000000000, 0.000000000000000000 ) ) ;
#6959 = CARTESIAN_POINT ( 'NONE',  ( 7.361572987183170547, 17.05059781766745530, 9.846743663894590881 ) ) ;
#6961 = LINE ( 'NONE', #36966, #60133 ) ;
#6963 = VERTEX_POINT ( 'NONE', #83362 ) ;
#6962 = CARTESIAN_POINT ( 'NONE',  ( 2.791683348922240793, 36.63393115100078035, 7.208316651077764092 ) ) ;
#6964 = CARTESIAN_POINT ( 'NONE',  ( 19.38216949554541202, 55.99863466993041072, 9.382169495545424454 ) ) ;
#6965 = CARTESIAN_POINT ( 'NONE',  ( 19.72487221294570858, 5.718334437839381224, -6.500000000000000888 ) ) ;
#6966 = CARTESIAN_POINT ( 'NONE',  ( 3.591859063236763294, 8.290301336597087456, -11.09922568453595026 ) ) ;
#6967 = PRESENTATION_LAYER_ASSIGNMENT (  '', '', ( #93165 ) ) ;
#6968 = CARTESIAN_POINT ( 'NONE',  ( 2.035157376598824452, 58.68868534415482685, 7.964842623401179544 ) ) ;
#6969 = CARTESIAN_POINT ( 'NONE',  ( 24.16423886937410614, 34.30374883491396787, 8.672049930838204340E-16 ) ) ;
#6970 = VECTOR ( 'NONE', #74583, 1000.000000000000000 ) ;
#6971 = CARTESIAN_POINT ( 'NONE',  ( -8.004782461319718934, 84.51756810411845322, 3.750000000000000000 ) ) ;
#6972 = VECTOR ( 'NONE', #59473, 1000.000000000000000 ) ;
#6973 = CARTESIAN_POINT ( 'NONE',  ( 22.26659068614895176, 24.72041550158063572, -7.082119434687042414 ) ) ;
#6974 = ADVANCED_FACE ( 'NONE', ( #30842 ), #98218, .T. ) ;
#6975 = CARTESIAN_POINT ( 'NONE',  ( 2.917880565312950480, 50.97041550158064638, -12.26659068614894821 ) ) ;
#6976 = CARTESIAN_POINT ( 'NONE',  ( 24.16423886937410614, 9.512082168247301794, -3.795296366450302550 ) ) ;
#6978 = CARTESIAN_POINT ( 'NONE',  ( -1.926860441876562247, 37.45379003517448524, -3.195792623639530650 ) ) ;
#6977 = CARTESIAN_POINT ( 'NONE',  ( 22.26659068614895176, 9.720415501580633943, -7.082119434687042414 ) ) ;
#6979 = CARTESIAN_POINT ( 'NONE',  ( 2.035157376598824452, 43.68868534415484106, 7.964842623401179544 ) ) ;
#6980 = CARTESIAN_POINT ( 'NONE',  ( -3.836325488035984499, 14.63606917487569703, -14.50112432709431864 ) ) ;
#6981 = CARTESIAN_POINT ( 'NONE',  ( 14.92337183194729988, 24.34226448433411960, -8.527530157486177487 ) ) ;
#6983 = CARTESIAN_POINT ( 'NONE',  ( 1.472469842513823179, 41.42559781766745886, 4.923371831947296329 ) ) ;
#6982 = LINE ( 'NONE', #29956, #62853 ) ;
#6984 = B_SPLINE_CURVE_WITH_KNOTS ( 'NONE', 3,
 ( #45132, #44138, #29139, #30122, #67151, #52150 ),
 .UNSPECIFIED., .F., .F.,
 ( 4, 2, 4 ),
 ( 3.409110551494650755E-05, 0.0004400426677367923721, 0.0008459942299586382638 ),
 .UNSPECIFIED. ) ;
#6985 = CARTESIAN_POINT ( 'NONE',  ( 20.88017736071110519, 25.56368534415483751, 2.639326808657452039E-16 ) ) ;
#6986 = CARTESIAN_POINT ( 'NONE',  ( 21.09922568453595559, 62.04030133659709634, -6.408140936763230044 ) ) ;
#6987 = CARTESIAN_POINT ( 'NONE',  ( 14.92337183194729988, 64.34226448433412315, -8.527530157486177487 ) ) ;
#6988 = DIRECTION ( 'NONE',  ( -1.776356839400250780E-14, 0.000000000000000000, 1.000000000000000000 ) ) ;
#6989 = CARTESIAN_POINT ( 'NONE',  ( 1.472469842513823179, 30.59226448433411960, -4.923371831947296329 ) ) ;
#6990 = CARTESIAN_POINT ( 'NONE',  ( -2.816281873526471635, 38.91530133659708213, -3.434112377981056508 ) ) ;
#6991 = CARTESIAN_POINT ( 'NONE',  ( -14.16423886937409726, -22.98791783175269643, 3.795296366450320757 ) ) ;
#6992 = CARTESIAN_POINT ( 'NONE',  ( 2.035157376598824452, 43.68868534415484106, 7.964842623401179544 ) ) ;
#6993 = CARTESIAN_POINT ( 'NONE',  ( 14.92337183194729988, 49.34226448433411605, -8.527530157486177487 ) ) ;
#6994 = CARTESIAN_POINT ( 'NONE',  ( -4.164238869374099927, 22.01208216824730357, 3.795296366450308767 ) ) ;
#6995 = ORIENTED_EDGE ( 'NONE', *, *, #64077, .F. ) ;
#6996 = CARTESIAN_POINT ( 'NONE',  ( -0.8801773607111008646, 58.27201867748816966, 2.915334737309923430 ) ) ;
#6997 = CARTESIAN_POINT ( 'NONE',  ( 17.96484262340118221, 64.93868534415483396, 7.964842623401181321 ) ) ;
#6998 = CARTESIAN_POINT ( 'NONE',  ( 20.36894250292379738, 64.92874883491397497, -10.36894250292379027 ) ) ;
#6999 = CARTESIAN_POINT ( 'NONE',  ( 2.791683348922240793, 61.63393115100079456, 7.208316651077764092 ) ) ;
#7000 = DIRECTION ( 'NONE',  ( -1.000000000000000000, 0.000000000000000000, 0.000000000000000000 ) ) ;
#7001 = CARTESIAN_POINT ( 'NONE',  ( 2.035157376598824452, 53.68868534415484817, 7.964842623401179544 ) ) ;
#7002 = CARTESIAN_POINT ( 'NONE',  ( 1.354709868695545216, 14.49999999999999112, 14.93870011653158336 ) ) ;
#7003 = CARTESIAN_POINT ( 'NONE',  ( -0.3689425029237898834, 46.17874883491397497, -10.36894250292378850 ) ) ;
#7004 = CARTESIAN_POINT ( 'NONE',  ( 7.964842623401181321, 24.93868534415484461, 7.964842623401174215 ) ) ;
#7005 = CARTESIAN_POINT ( 'NONE',  ( 12.91533473730992121, 9.522018677488171434, 10.88017736071110164 ) ) ;
#7006 = CARTESIAN_POINT ( 'NONE',  ( 10.00000000000000178, 24.31368534415484106, 10.88017736071110342 ) ) ;
#7007 = CARTESIAN_POINT ( 'NONE',  ( 7.361572987183170547, 52.05059781766745175, 9.846743663894590881 ) ) ;
#7008 = CARTESIAN_POINT ( 'NONE',  ( 16.40814093676324603, 57.45696800326375353, -11.09922568453594671 ) ) ;
#7009 = DIRECTION ( 'NONE',  ( 0.000000000000000000, 0.000000000000000000, 1.000000000000000000 ) ) ;
#7010 = ORIENTED_EDGE ( 'NONE', *, *, #19227, .F. ) ;
#7011 = CARTESIAN_POINT ( 'NONE',  ( 12.91533473730993009, 11.60535201082150536, -10.88017736071109987 ) ) ;
#7012 = EDGE_CURVE ( 'NONE', #92653, #97221, #25730, .T. ) ;
#7013 = CARTESIAN_POINT ( 'NONE',  ( -2.816281873526471635, 18.91530133659708213, -3.434112377981056508 ) ) ;
#7014 = PLANE ( 'NONE',  #20966 ) ;
#7016 = B_SPLINE_CURVE_WITH_KNOTS ( 'NONE', 3,
 ( #85392, #38918, #56380, #93873, #23919, #25399 ),
 .UNSPECIFIED., .F., .F.,
 ( 4, 2, 4 ),
 ( 0.000000000000000000, 0.0002626113303184793800, 0.0005252226606369587601 ),
 .UNSPECIFIED. ) ;
#7015 = CARTESIAN_POINT ( 'NONE',  ( 19.84674366389459266, 48.71726448433413026, -2.638427012816827677 ) ) ;
#7017 = EDGE_CURVE ( 'NONE', #12064, #61160, #19891, .T. ) ;
#7018 = CARTESIAN_POINT ( 'NONE',  ( 2.035157376598824452, 33.68868534415484106, 7.964842623401179544 ) ) ;
#7019 = CARTESIAN_POINT ( 'NONE',  ( 16.40814093676324603, 27.45696800326375708, -11.09922568453594671 ) ) ;
#7021 = CARTESIAN_POINT ( 'NONE',  ( 0.000000000000000000, 80.32179676972448590, 4.000000000000000000 ) ) ;
#7020 = CARTESIAN_POINT ( 'NONE',  ( -0.8801773607110991993, 47.85535201082150536, -2.915334737309923874 ) ) ;
#7022 = DIRECTION ( 'NONE',  ( -0.000000000000000000, -1.000000000000000000, -0.000000000000000000 ) ) ;
#7023 = CARTESIAN_POINT ( 'NONE',  ( -2.816281873526473856, 49.12363466993042493, 9.499525473075851096E-16 ) ) ;
#7024 = ORIENTED_EDGE ( 'NONE', *, *, #64473, .F. ) ;
#7025 = CARTESIAN_POINT ( 'NONE',  ( -6.000000000000000000, 78.07179676972447169, -6.250000000000000000 ) ) ;
#7026 = CARTESIAN_POINT ( 'NONE',  ( 4.559911319644449179, 53.89701867748817676, 9.422509992056141925 ) ) ;
#7027 = CARTESIAN_POINT ( 'NONE',  ( 6.565887622018943937, 40.16530133659708923, 12.81628187352647430 ) ) ;
#7028 = CARTESIAN_POINT ( 'NONE',  ( 5.076628168052703671, 6.842264484334118713, 8.527530157486179263 ) ) ;
#7029 = CARTESIAN_POINT ( 'NONE',  ( 19.42250999205614548, 45.98035201082150536, -5.440088680355545492 ) ) ;
#7030 = CARTESIAN_POINT ( 'NONE',  ( -0.03447792253739143109, 15.15514106990689847, 6.401564815979740253 ) ) ;
#7031 = SURFACE_STYLE_FILL_AREA ( #69503 ) ;
#7032 = CARTESIAN_POINT ( 'NONE',  ( 0.1532563361054083140, 21.00893115100078745, 1.131784320476157264E-15 ) ) ;
#7033 = CARTESIAN_POINT ( 'NONE',  ( 1.472469842513823179, 0.5922644843341181575, -4.923371831947296329 ) ) ;
#7034 = CARTESIAN_POINT ( 'NONE',  ( -0.03447792253739536544, 5.155141069906901130, 6.401564815979722489 ) ) ;
#7035 = CARTESIAN_POINT ( 'NONE',  ( 6.204703633549690345, 37.84541550158063927, 14.16423886937410082 ) ) ;
#7036 = ADVANCED_FACE ( 'NONE', ( #30341 ), #38856, .T. ) ;
#7037 = FACE_OUTER_BOUND ( 'NONE', #13198, .T. ) ;
#7038 = CARTESIAN_POINT ( 'NONE',  ( 2.035157376598822676, 12.43868534415483751, -7.964842623401177768 ) ) ;
#7039 = CARTESIAN_POINT ( 'NONE',  ( -7.322357042924514836, -84.41015717759208314, -4.000000000000000000 ) ) ;
#7040 = ORIENTED_EDGE ( 'NONE', *, *, #44146, .F. ) ;
#7041 = CARTESIAN_POINT ( 'NONE',  ( 17.08211943468705840, 60.13708216824729647, -12.26659068614894466 ) ) ;
#7042 = CARTESIAN_POINT ( 'NONE',  ( 6.204703633549690345, 62.84541550158063927, 14.16423886937410082 ) ) ;
#7043 = CARTESIAN_POINT ( 'NONE',  ( 2.791683348922240793, 36.63393115100078035, 7.208316651077764092 ) ) ;
#7044 = EDGE_CURVE ( 'NONE', #9285, #27759, #54393, .T. ) ;
#7045 = CARTESIAN_POINT ( 'NONE',  ( -1.099225684535947600, 39.54030133659708923, 6.408140936763237150 ) ) ;
#7046 = CARTESIAN_POINT ( 'NONE',  ( -8.000000000000000000, 41.24999999999999289, -6.250000000000000000 ) ) ;
#7049 = CARTESIAN_POINT ( 'NONE',  ( -0.3689425029237898834, 1.178748834913967869, -10.36894250292378850 ) ) ;
#7048 = CARTESIAN_POINT ( 'NONE',  ( -12.23643000159860250, 90.44368800334666503, -7.046674173440611533 ) ) ;
#7047 = AXIS2_PLACEMENT_3D ( 'NONE', #88666, #49196, #19193 ) ;
#7050 = CARTESIAN_POINT ( 'NONE',  ( 12.91533473730992121, 19.52201867748816611, 10.88017736071110164 ) ) ;
#7051 = CARTESIAN_POINT ( 'NONE',  ( 10.00000000000000178, 63.05374883491396076, 14.16423886937410082 ) ) ;
#7052 = CARTESIAN_POINT ( 'NONE',  ( 12.63842701281683034, 37.46726448433411605, 9.846743663894596210 ) ) ;
#7053 = CARTESIAN_POINT ( 'NONE',  ( -14.66148682522524993, 0.2301506158824424275, 2.874551585517085783 ) ) ;
#7054 = CARTESIAN_POINT ( 'NONE',  ( 19.84674366389459266, 28.30059781766745886, 2.638427012816836559 ) ) ;
#7055 = EDGE_CURVE ( 'NONE', #96379, #91469, #53345, .T. ) ;
#7056 = CIRCLE ( 'NONE', #59697, 2.500000000000002220 ) ;
#7057 = CARTESIAN_POINT ( 'NONE',  ( 9.065164099344466209, 14.63595249122789177, 11.95084933600773880 ) ) ;
#7058 = CARTESIAN_POINT ( 'NONE',  ( -8.527530157486173934, 11.42559781766745708, 4.923371831947302546 ) ) ;
#7059 = EDGE_LOOP ( 'NONE', ( #67714, #6646, #43305, #98960, #52308, #26480 ) ) ;
#7060 = EDGE_LOOP ( 'NONE', ( #17501, #96359, #87481, #19133 ) ) ;
#7061 = DIRECTION ( 'NONE',  ( 0.9999619230641713097, -0.000000000000000000, 0.008726535498374266009 ) ) ;
#7062 = ORIENTED_EDGE ( 'NONE', *, *, #18281, .T. ) ;
#7063 = CARTESIAN_POINT ( 'NONE',  ( 17.20831665107776587, 57.88393115100078745, 7.208316651077764980 ) ) ;
#7064 = CARTESIAN_POINT ( 'NONE',  ( -4.164238869374098151, 21.59541550158063217, -3.795296366450310543 ) ) ;
#7066 = CARTESIAN_POINT ( 'NONE',  ( 4.559911319644449179, 33.89701867748817676, 9.422509992056141925 ) ) ;
#7065 = CARTESIAN_POINT ( 'NONE',  ( 17.96484262340118221, 31.18868534415483751, -7.964842623401177768 ) ) ;
#7068 = CARTESIAN_POINT ( 'NONE',  ( 19.38216949554541202, 35.99863466993041072, 9.382169495545424454 ) ) ;
#7067 = CARTESIAN_POINT ( 'NONE',  ( 5.076628168052703671, 56.84226448433412315, 8.527530157486179263 ) ) ;
#7069 = CARTESIAN_POINT ( 'NONE',  ( 10.00000000000000000, 5.553748834913967869, -14.16423886937410082 ) ) ;
#7070 = CARTESIAN_POINT ( 'NONE',  ( 4.559911319644449179, 68.89701867748817676, 9.422509992056141925 ) ) ;
#7071 = CARTESIAN_POINT ( 'NONE',  ( 10.00000000000000178, 25.37363466993041783, 12.81628187352647608 ) ) ;
#7072 = ORIENTED_EDGE ( 'NONE', *, *, #21856, .F. ) ;
#7073 = CARTESIAN_POINT ( 'NONE',  ( 18.52753015748617571, 43.09226448433412315, 4.923371831947298993 ) ) ;
#7074 = CARTESIAN_POINT ( 'NONE',  ( -0.8801773607111009756, 3.063685344154838397, 1.068504757029289695E-15 ) ) ;
#7075 = ORIENTED_EDGE ( 'NONE', *, *, #77438, .T. ) ;
#7076 = CARTESIAN_POINT ( 'NONE',  ( 20.88017736071110519, 15.56368534415483751, 2.639326808657452039E-16 ) ) ;
#7077 = ORIENTED_EDGE ( 'NONE', *, *, #6577, .F. ) ;
#7078 = CARTESIAN_POINT ( 'NONE',  ( 17.96484262340118221, 66.18868534415483396, -7.964842623401177768 ) ) ;
#7079 = CARTESIAN_POINT ( 'NONE',  ( 2.035157376598822676, 52.43868534415483396, -7.964842623401177768 ) ) ;
#7080 = CARTESIAN_POINT ( 'NONE',  ( 12.91533473730992121, 64.52201867748817676, 10.88017736071110164 ) ) ;
#7081 = CARTESIAN_POINT ( 'NONE',  ( 15.44008868035555260, 49.73035201082150536, 9.422509992056143702 ) ) ;
#7082 = DIRECTION ( 'NONE',  ( -0.000000000000000000, 0.000000000000000000, -1.000000000000000000 ) ) ;
#7083 = ADVANCED_FACE ( 'NONE', ( #29852 ), #45445, .T. ) ;
#7084 = CARTESIAN_POINT ( 'NONE',  ( 20.15039907845753930, 70.00000000000000000, -6.262539305110068177 ) ) ;
#7086 = EDGE_LOOP ( 'NONE', ( #64096, #44288, #39872, #83251 ) ) ;
#7085 = CARTESIAN_POINT ( 'NONE',  ( 8.630000000000000782, 1.019547802438458550, 4.000000000000000000 ) ) ;
#7087 = CARTESIAN_POINT ( 'NONE',  ( 12.63842701281683034, 47.46726448433412315, 9.846743663894596210 ) ) ;
#7088 = ORIENTED_EDGE ( 'NONE', *, *, #50943, .T. ) ;
#7089 = DIRECTION ( 'NONE',  ( 0.000000000000000000, -1.000000000000000000, 0.000000000000000000 ) ) ;
#7090 = CARTESIAN_POINT ( 'NONE',  ( 20.36894250292379382, 8.678748834913967869, 10.36894250292379205 ) ) ;
#7091 = VERTEX_POINT ( 'NONE', #61340 ) ;
#7092 = CARTESIAN_POINT ( 'NONE',  ( -1.114591949024815731, 15.00000000000000000, -14.45709807627963350 ) ) ;
#7093 = CARTESIAN_POINT ( 'NONE',  ( 17.39651004071838614, 42.93575266056826933, 6.500000000000032863 ) ) ;
#7094 = CARTESIAN_POINT ( 'NONE',  ( 0.5774900079438607392, 8.480352010821505360, 5.440088680355550821 ) ) ;
#7095 = DIRECTION ( 'NONE',  ( 0.000000000000000000, 1.000000000000000000, 0.000000000000000000 ) ) ;
#7097 = VERTEX_POINT ( 'NONE', #84360 ) ;
#7096 = CARTESIAN_POINT ( 'NONE',  ( 16.40814093676324603, 37.45696800326376064, -11.09922568453594671 ) ) ;
#7098 = CARTESIAN_POINT ( 'NONE',  ( -5.963430220938278126, 5.521642702460839658, 10.32896413005680358 ) ) ;
#7099 = CARTESIAN_POINT ( 'NONE',  ( 0.1532563361054083140, 41.00893115100078745, 1.131784320476157264E-15 ) ) ;
#7100 = CARTESIAN_POINT ( 'NONE',  ( -13.30156849913890937, 14.76930270348882068, 6.804875469487965844 ) ) ;
#7101 = CARTESIAN_POINT ( 'NONE',  ( -2.816281873526471635, 13.91530133659708746, -3.434112377981056508 ) ) ;
#7102 = CARTESIAN_POINT ( 'NONE',  ( 17.20831665107776587, 29.13393115100078390, -7.208316651077762316 ) ) ;
#7103 = CARTESIAN_POINT ( 'NONE',  ( 17.20831665107776587, 17.88393115100078745, 7.208316651077764980 ) ) ;
#7104 = CARTESIAN_POINT ( 'NONE',  ( 13.43411237798106583, 2.665301336597086568, -12.81628187352647252 ) ) ;
#7105 = AXIS2_PLACEMENT_3D ( 'NONE', #24931, #81354, #96380 ) ;
#7106 = ORIENTED_EDGE ( 'NONE', *, *, #67725, .T. ) ;
#7107 = ORIENTED_EDGE ( 'NONE', *, *, #16746, .F. ) ;
#7108 = VECTOR ( 'NONE', #50983, 1000.000000000000000 ) ;
#7109 = CARTESIAN_POINT ( 'NONE',  ( 17.96484262340118221, 24.93868534415484461, 7.964842623401181321 ) ) ;
#7110 = CARTESIAN_POINT ( 'NONE',  ( 24.16423886937410614, 14.51208216824730179, -3.795296366450302550 ) ) ;
#7111 = CARTESIAN_POINT ( 'NONE',  ( 7.361572987183170547, 32.05059781766745175, 9.846743663894590881 ) ) ;
#7112 = CARTESIAN_POINT ( 'NONE',  ( 7.084665262690076126, 69.10535201082151957, 10.88017736071109987 ) ) ;
#7113 = CARTESIAN_POINT ( 'NONE',  ( 16.40814093676323893, 40.79030133659708923, 11.09922568453595026 ) ) ;
#7114 = CARTESIAN_POINT ( 'NONE',  ( -0.8801773607110991993, 12.85535201082150358, -2.915334737309923874 ) ) ;
#7115 = AXIS2_PLACEMENT_3D ( 'NONE', #90595, #31080, #91600 ) ;
#7116 = CARTESIAN_POINT ( 'NONE',  ( -0.1503990784575328643, 70.00000000000000000, 6.262539305110068177 ) ) ;
#7117 = CARTESIAN_POINT ( 'NONE',  ( 0.6178305044545818747, 3.498634669930420049, -9.382169495545419124 ) ) ;
#7118 = CARTESIAN_POINT ( 'NONE',  ( 18.52753015748618282, 28.92559781766745175, -4.923371831947291888 ) ) ;
#7119 = CARTESIAN_POINT ( 'NONE',  ( -2.915334737309934532, -12.97798132251181968, -10.88017736071109987 ) ) ;
#7120 = CARTESIAN_POINT ( 'NONE',  ( 3.591859063236763294, 38.29030133659708923, -11.09922568453595026 ) ) ;
#7121 = CARTESIAN_POINT ( 'NONE',  ( -19.64999999999999858, 98.99999999999998579, 7.750000000000000000 ) ) ;
#7123 = DIRECTION ( 'NONE',  ( -0.8433914458128813907, 0.000000000000000000, -0.5372996083468306594 ) ) ;
#7122 = CARTESIAN_POINT ( 'NONE',  ( 15.44008868035555260, 39.73035201082150536, 9.422509992056143702 ) ) ;
#7124 = CARTESIAN_POINT ( 'NONE',  ( 64.56412365047462742, 13.99999999999999467, -10.00000000000000000 ) ) ;
#7125 = CARTESIAN_POINT ( 'NONE',  ( 15.44008868035555793, 41.39701867748817676, -9.422509992056140149 ) ) ;
#7126 = CARTESIAN_POINT ( 'NONE',  ( -0.8801773607110991993, 47.85535201082150536, -2.915334737309923874 ) ) ;
#7127 = DIRECTION ( 'NONE',  ( 1.000000000000000000, 1.790682297782510536E-15, 0.000000000000000000 ) ) ;
#7128 = TOROIDAL_SURFACE ( 'NONE', #96574, 62.00000000000000000, 0.5000000000000000000 ) ;
#7129 = CARTESIAN_POINT ( 'NONE',  ( 0.5774900079438590739, 62.64701867748817676, -5.440088680355550821 ) ) ;
#7130 = ADVANCED_FACE ( 'NONE', ( #90849 ), #72277, .F. ) ;
#7131 = EDGE_CURVE ( 'NONE', #34423, #47878, #9327, .T. ) ;
#7132 = UNCERTAINTY_MEASURE_WITH_UNIT (LENGTH_MEASURE( 1.000000000000000082E-05 ), #61334, 'distance_accuracy_value', 'NONE');
#7133 = CARTESIAN_POINT ( 'NONE',  ( 10.00000000000000000, 54.75893115100078745, -9.846743663894594434 ) ) ;
#7135 = DIRECTION ( 'NONE',  ( 0.1993679344172039347, 0.000000000000000000, -0.9799247046208282574 ) ) ;
#7134 = CARTESIAN_POINT ( 'NONE',  ( 2.035157376598822676, 7.438685344154837509, -7.964842623401177768 ) ) ;
#7136 = CARTESIAN_POINT ( 'NONE',  ( 13.43411237798105340, 10.58196800326375353, 12.81628187352647963 ) ) ;
#7137 = EDGE_LOOP ( 'NONE', ( #50573, #56976, #12048, #88462 ) ) ;
#7138 = CARTESIAN_POINT ( 'NONE',  ( 17.96484262340118221, 36.18868534415484106, -7.964842623401177768 ) ) ;
#7139 = DIRECTION ( 'NONE',  ( -0.000000000000000000, -1.000000000000000000, -0.000000000000000000 ) ) ;
#7140 = CARTESIAN_POINT ( 'NONE',  ( 10.00000000000000178, 24.31368534415484106, 10.88017736071110342 ) ) ;
#7141 = CARTESIAN_POINT ( 'NONE',  ( 14.92337183194729633, 2.675597817667451750, 8.527530157486181039 ) ) ;
#7142 = CARTESIAN_POINT ( 'NONE',  ( 13.79529636645031943, 40.34541550158063217, -14.16423886937409904 ) ) ;
#7143 = CARTESIAN_POINT ( 'NONE',  ( 1.472469842513823179, 31.42559781766745530, 4.923371831947296329 ) ) ;
#7144 = CARTESIAN_POINT ( 'NONE',  ( -0.8801773607111008646, 48.27201867748816966, 2.915334737309923430 ) ) ;
#7145 = CARTESIAN_POINT ( 'NONE',  ( 6.579634127946655475, -87.99828267815715321, -4.000000000000000000 ) ) ;
#7146 = SURFACE_STYLE_FILL_AREA ( #75634 ) ;
#7147 = VECTOR ( 'NONE', #32620, 1000.000000000000000 ) ;
#7148 = ORIENTED_EDGE ( 'NONE', *, *, #18304, .T. ) ;
#7149 = CARTESIAN_POINT ( 'NONE',  ( -11.96291822454869802, 4.725512573308054359E-16, -8.193813980849247613 ) ) ;
#7150 = CARTESIAN_POINT ( 'NONE',  ( 12.63842701281683034, 57.46726448433411605, 9.846743663894596210 ) ) ;
#7151 = ORIENTED_EDGE ( 'NONE', *, *, #42484, .T. ) ;
#7152 = VERTEX_POINT ( 'NONE', #17339 ) ;
#7153 = CARTESIAN_POINT ( 'NONE',  ( -4.164238869374099039, 16.80374883491396787, 8.674139862899312516E-16 ) ) ;
#7154 = CARTESIAN_POINT ( 'NONE',  ( 6.204703633549690345, 25.76208216824730712, -14.16423886937410259 ) ) ;
#7155 = CARTESIAN_POINT ( 'NONE',  ( -0.8801773607111008646, 63.27201867748817676, 2.915334737309923430 ) ) ;
#7156 = CARTESIAN_POINT ( 'NONE',  ( -4.164238869374099927, 67.01208216824728936, 3.795296366450308767 ) ) ;
#7157 = CARTESIAN_POINT ( 'NONE',  ( 13.43411237798106583, 7.665301336597086568, -12.81628187352647252 ) ) ;
#7158 = CARTESIAN_POINT ( 'NONE',  ( 2.791683348922240793, 46.63393115100077324, 7.208316651077764092 ) ) ;
#7159 = CARTESIAN_POINT ( 'NONE',  ( -8.468251460007511611, -9.345277391842092385, 4.000000000000000000 ) ) ;
#7161 = CARTESIAN_POINT ( 'NONE',  ( 22.81628187352647785, 16.62363466993042138, 6.195893100308588602E-16 ) ) ;
#7160 = CARTESIAN_POINT ( 'NONE',  ( 19.42250999205614548, 45.98035201082150536, -5.440088680355545492 ) ) ;
#7162 = CARTESIAN_POINT ( 'NONE',  ( 10.00000000000000178, 18.05374883491396787, 14.16423886937410082 ) ) ;
#7163 = CARTESIAN_POINT ( 'NONE',  ( 2.035157376598824452, 8.688685344154839285, 7.964842623401179544 ) ) ;
#7164 = CARTESIAN_POINT ( 'NONE',  ( 7.084665262690076126, 24.10535201082150181, 10.88017736071109987 ) ) ;
#7165 = CARTESIAN_POINT ( 'NONE',  ( -3.750000000000000000, 10.25000000000000000, -2.750000000000000000 ) ) ;
#7166 = CARTESIAN_POINT ( 'NONE',  ( 2.035157376598824452, 53.68868534415484817, 7.964842623401179544 ) ) ;
#7167 = ADVANCED_FACE ( 'NONE', ( #3807 ), #56312, .T. ) ;
#7168 = CARTESIAN_POINT ( 'NONE',  ( 7.208316651077762316, -25.86606884899920900, -7.208316651077764980 ) ) ;
#7169 = VERTEX_POINT ( 'NONE', #10809 ) ;
#7170 = CARTESIAN_POINT ( 'NONE',  ( 13.55101055326450599, 0.2301500585724599590, 6.292244619294732999 ) ) ;
#7171 = STYLED_ITEM ( 'NONE', ( #11421 ), #10384 ) ;
#7172 = ORIENTED_EDGE ( 'NONE', *, *, #91952, .T. ) ;
#7173 = PLANE ( 'NONE',  #27096 ) ;
#7174 = EDGE_LOOP ( 'NONE', ( #45175, #67917, #83781, #48638 ) ) ;
#7175 = CARTESIAN_POINT ( 'NONE',  ( -0.1491070598754174470, 61.94583914210339515, 5.000000000000000000 ) ) ;
#7177 = CARTESIAN_POINT ( 'NONE',  ( -4.164238869374098151, 66.59541550158060375, -3.795296366450310543 ) ) ;
#7176 = CARTESIAN_POINT ( 'NONE',  ( 10.00000000000000000, 65.55374883491396076, -14.16423886937410082 ) ) ;
#7179 = CARTESIAN_POINT ( 'NONE',  ( 12.63842701281683922, 54.55059781766745175, -9.846743663894590881 ) ) ;
#7178 = CARTESIAN_POINT ( 'NONE',  ( 12.63842701281683922, 29.55059781766745175, -9.846743663894590881 ) ) ;
#7180 = CARTESIAN_POINT ( 'NONE',  ( 7.084665262690076126, 67.02201867748817676, -10.88017736071110164 ) ) ;
#7181 = CARTESIAN_POINT ( 'NONE',  ( 17.96484262340118221, 64.93868534415483396, 7.964842623401181321 ) ) ;
#7182 = AXIS2_PLACEMENT_3D ( 'NONE', #66341, #97867, #5857 ) ;
#7183 = VECTOR ( 'NONE', #3225, 1000.000000000000000 ) ;
#7184 = CARTESIAN_POINT ( 'NONE',  ( 11.09922568453595026, 21.20696800326375708, 6.408140936763232709 ) ) ;
#7185 = VERTEX_POINT ( 'NONE', #18310 ) ;
#7186 = CARTESIAN_POINT ( 'NONE',  ( 20.36894250292379738, 39.92874883491396787, -10.36894250292379027 ) ) ;
#7187 = ORIENTED_EDGE ( 'NONE', *, *, #63876, .T. ) ;
#7188 = CARTESIAN_POINT ( 'NONE',  ( -4.164238869374098151, 41.59541550158061796, -3.795296366450310543 ) ) ;
#7189 = ORIENTED_EDGE ( 'NONE', *, *, #53785, .T. ) ;
#7190 = CARTESIAN_POINT ( 'NONE',  ( -2.816281873526471635, 53.91530133659709634, -3.434112377981056508 ) ) ;
#7191 = CARTESIAN_POINT ( 'NONE',  ( 0.5774900079438590739, 22.64701867748817321, -5.440088680355550821 ) ) ;
#7192 = CARTESIAN_POINT ( 'NONE',  ( 10.00000000000000000, 49.75893115100078745, -9.846743663894594434 ) ) ;
#7193 = CARTESIAN_POINT ( 'NONE',  ( 7.084665262690076126, 22.02201867748817321, -10.88017736071110164 ) ) ;
#7194 = FACE_OUTER_BOUND ( 'NONE', #61423, .T. ) ;
#7195 = CARTESIAN_POINT ( 'NONE',  ( -2.393480905992944496, 0.5000000000000004441, -14.80781041047754520 ) ) ;
#7196 = CARTESIAN_POINT ( 'NONE',  ( 2.791683348922237240, 55.38393115100078745, -7.208316651077763204 ) ) ;
#7197 = CARTESIAN_POINT ( 'NONE',  ( 19.84674366389459621, 53.50893115100078745, 7.409399052514197653E-17 ) ) ;
#7199 = ORIENTED_EDGE ( 'NONE', *, *, #13544, .T. ) ;
#7198 = CARTESIAN_POINT ( 'NONE',  ( -11.81378540890942119, 15.00000000000000000, 7.968498874458034287 ) ) ;
#7200 = AXIS2_PLACEMENT_3D ( 'NONE', #66375, #51382, #13382 ) ;
#7201 = CARTESIAN_POINT ( 'NONE',  ( 2.618367889266248100E-15, 44.99999999999999289, 7.000000000000000000 ) ) ;
#7202 = FACE_OUTER_BOUND ( 'NONE', #83288, .T. ) ;
#7203 = ORIENTED_EDGE ( 'NONE', *, *, #46528, .T. ) ;
#7204 = CARTESIAN_POINT ( 'NONE',  ( 0.6076426042653103599, 67.37576471608602446, -6.499999999999992006 ) ) ;
#7205 = CARTESIAN_POINT ( 'NONE',  ( 7.361572987183169658, 24.96726448433412315, -9.846743663894592657 ) ) ;
#7206 = CYLINDRICAL_SURFACE ( 'NONE', #61199, 0.5000000000000004441 ) ;
#7207 = CARTESIAN_POINT ( 'NONE',  ( 21.09922568453595559, 32.04030133659708923, -6.408140936763230044 ) ) ;
#7208 = DIRECTION ( 'NONE',  ( 1.000000000000000000, 0.000000000000000000, 0.000000000000000000 ) ) ;
#7209 = FACE_OUTER_BOUND ( 'NONE', #93687, .T. ) ;
#7210 = ORIENTED_EDGE ( 'NONE', *, *, #29282, .F. ) ;
#7211 = PLANE ( 'NONE',  #2913 ) ;
#7212 = CARTESIAN_POINT ( 'NONE',  ( 0.1143410931637171279, 65.21691075486303646, 6.480892540919849232 ) ) ;
#7213 = CARTESIAN_POINT ( 'NONE',  ( 18.52753015748618282, 38.92559781766745175, -4.923371831947291888 ) ) ;
#7214 = CARTESIAN_POINT ( 'NONE',  ( 2.917880565312948704, 32.63708216824730357, 12.26659068614894643 ) ) ;
#7215 = CARTESIAN_POINT ( 'NONE',  ( 0.1532563361054100626, 50.80059781766745175, -2.638427012816831230 ) ) ;
#7216 = FACE_OUTER_BOUND ( 'NONE', #89771, .T. ) ;
#7217 = DIRECTION ( 'NONE',  ( 0.000000000000000000, 0.000000000000000000, 1.000000000000000000 ) ) ;
#7218 = CARTESIAN_POINT ( 'NONE',  ( 0.1532563361054083140, 1.008931151000784787, 1.131784320476157264E-15 ) ) ;
#7219 = CARTESIAN_POINT ( 'NONE',  ( 2.917880565312950480, 5.970415501580634832, -12.26659068614894821 ) ) ;
#7221 = ADVANCED_FACE ( 'NONE', ( #40329 ), #1113, .T. ) ;
#7220 = VECTOR ( 'NONE', #80386, 1000.000000000000000 ) ;
#7222 = CARTESIAN_POINT ( 'NONE',  ( 5.076628168052703671, 46.84226448433412315, 8.527530157486179263 ) ) ;
#7223 = CARTESIAN_POINT ( 'NONE',  ( 12.91533473730993009, 51.60535201082149825, -10.88017736071109987 ) ) ;
#7224 = CARTESIAN_POINT ( 'NONE',  ( 0.1532563361054100626, 45.80059781766745886, -2.638427012816831230 ) ) ;
#7225 = FACE_OUTER_BOUND ( 'NONE', #70406, .T. ) ;
#7226 = CARTESIAN_POINT ( 'NONE',  ( 17.96484262340118221, 44.93868534415483396, 7.964842623401181321 ) ) ;
#7227 = ORIENTED_EDGE ( 'NONE', *, *, #90627, .T. ) ;
#7228 = DIRECTION ( 'NONE',  ( 0.000000000000000000, 1.000000000000000000, 0.000000000000000000 ) ) ;
#7229 = CARTESIAN_POINT ( 'NONE',  ( 4.559911319644449179, 18.89701867748817321, 9.422509992056141925 ) ) ;
#7231 = CARTESIAN_POINT ( 'NONE',  ( 10.00000000000000178, 49.31368534415484106, 10.88017736071110342 ) ) ;
#7230 = CARTESIAN_POINT ( 'NONE',  ( 6.565887622018943937, 3.081968003263753531, -12.81628187352647608 ) ) ;
#7232 = CARTESIAN_POINT ( 'NONE',  ( -1.926860441876563801, 47.66212336850780673, 1.004413902775740978E-15 ) ) ;
#7233 = CARTESIAN_POINT ( 'NONE',  ( 20.15039907845753575, 10.60158574516642460, -6.262539305110077059 ) ) ;
#7234 = CARTESIAN_POINT ( 'NONE',  ( 11.92686044187657224, 4.953790035174480799, 3.195792623639526209 ) ) ;
#7236 = DIRECTION ( 'NONE',  ( 0.7826081568524149157, 0.000000000000000000, 0.6225146366376184126 ) ) ;
#7235 = CARTESIAN_POINT ( 'NONE',  ( 20.88017736071110519, 45.56368534415484106, 2.639326808657452039E-16 ) ) ;
#7237 = CARTESIAN_POINT ( 'NONE',  ( 18.52753015748618282, 13.92559781766745175, -4.923371831947291888 ) ) ;
#7238 = AXIS2_PLACEMENT_3D ( 'NONE', #81577, #99, #36592 ) ;
#7239 = CARTESIAN_POINT ( 'NONE',  ( 5.076628168052703671, 36.84226448433412315, 8.527530157486179263 ) ) ;
#7240 = DIRECTION ( 'NONE',  ( 0.9935718556765885667, 0.000000000000000000, -0.1132032137678971873 ) ) ;
#7241 = CARTESIAN_POINT ( 'NONE',  ( 10.36894250292378850, 24.92874883491397497, -10.36894250292379027 ) ) ;
#7242 = CARTESIAN_POINT ( 'NONE',  ( 7.361572987183170547, 67.05059781766746596, 9.846743663894590881 ) ) ;
#7243 = EDGE_CURVE ( 'NONE', #13092, #94718, #71020, .T. ) ;
#7244 = CARTESIAN_POINT ( 'NONE',  ( -0.8801773607111008646, 3.272018677488171434, 2.915334737309923430 ) ) ;
#7245 = SURFACE_STYLE_FILL_AREA ( #45231 ) ;
#7246 = CARTESIAN_POINT ( 'NONE',  ( 13.79529636645031943, 25.34541550158063572, -14.16423886937409904 ) ) ;
#7247 = B_SPLINE_CURVE_WITH_KNOTS ( 'NONE', 3,
 ( #80036, #64033, #73018, #65014, #94547, #4550 ),
 .UNSPECIFIED., .F., .F.,
 ( 4, 2, 4 ),
 ( 0.000000000000000000, 0.0002605067024380935069, 0.0005210134048761870139 ),
 .UNSPECIFIED. ) ;
#7248 = CARTESIAN_POINT ( 'NONE',  ( 13.79529636645030344, 48.26208216824728936, 14.16423886937410614 ) ) ;
#7249 = FILL_AREA_STYLE ('',( #45234 ) ) ;
#7250 = EDGE_CURVE ( 'NONE', #5928, #59170, #21264, .T. ) ;
#7251 = VERTEX_POINT ( 'NONE', #27268 ) ;
#7252 = CARTESIAN_POINT ( 'NONE',  ( 18.52753015748617571, 23.09226448433411960, 4.923371831947298993 ) ) ;
#7253 = AXIS2_PLACEMENT_3D ( 'NONE', #12245, #28725, #35736 ) ;
#7254 = CARTESIAN_POINT ( 'NONE',  ( -0.8801773607111008646, 33.27201867748817676, 2.915334737309923430 ) ) ;
#7255 = CARTESIAN_POINT ( 'NONE',  ( 0.1532563361054100626, 50.80059781766745175, -2.638427012816831230 ) ) ;
#7257 = CARTESIAN_POINT ( 'NONE',  ( 34.56412365047463453, 13.99999999999999645, -9.500000000000000000 ) ) ;
#7256 = CARTESIAN_POINT ( 'NONE',  ( 20.36894250292379382, 3.678748834913967869, 10.36894250292379205 ) ) ;
#7258 = CARTESIAN_POINT ( 'NONE',  ( -9.402796353261203777, 15.00000000000000000, 11.68706210897750708 ) ) ;
#7259 = EDGE_CURVE ( 'NONE', #91314, #92036, #51761, .T. ) ;
#7260 = CARTESIAN_POINT ( 'NONE',  ( 9.779999999999990479, 20.99999999999999645, -2.899999999999999911 ) ) ;
#7261 = CARTESIAN_POINT ( 'NONE',  ( 19.38216949554541202, 40.99863466993042493, 9.382169495545424454 ) ) ;
#7262 = B_SPLINE_CURVE_WITH_KNOTS ( 'NONE', 3,
 ( #14108, #67102, #98624, #60077, #88605, #52585 ),
 .UNSPECIFIED., .F., .F.,
 ( 4, 2, 4 ),
 ( 3.409110551494646011E-05, 0.0004400426677367926974, 0.0008459942299586389143 ),
 .UNSPECIFIED. ) ;
#7263 = CARTESIAN_POINT ( 'NONE',  ( 18.52753015748618282, 38.92559781766745175, -4.923371831947291888 ) ) ;
#7264 = ORIENTED_EDGE ( 'NONE', *, *, #86712, .T. ) ;
#7265 = CARTESIAN_POINT ( 'NONE',  ( 17.20831665107776587, 12.88393115100078390, 7.208316651077764980 ) ) ;
#7266 = CARTESIAN_POINT ( 'NONE',  ( 11.01507687156111892, -96.09620168231128901, -3.750000000000000000 ) ) ;
#7267 = CARTESIAN_POINT ( 'NONE',  ( 20.10384461210892226, 16.74302437010793199, 6.337995344473751125 ) ) ;
#7268 = CARTESIAN_POINT ( 'NONE',  ( 4.559911319644449179, 8.897018677488173211, 9.422509992056141925 ) ) ;
#7269 = CARTESIAN_POINT ( 'NONE',  ( 22.26659068614894466, 48.88708216824730357, 7.082119434687054849 ) ) ;
#7270 = CARTESIAN_POINT ( 'NONE',  ( 4.559911319644449179, 43.89701867748816966, 9.422509992056141925 ) ) ;
#7271 = CARTESIAN_POINT ( 'NONE',  ( 0.2751277870542908621, 32.28217586085237656, -6.499999999999992006 ) ) ;
#7272 = LINE ( 'NONE', #47593, #83200 ) ;
#7273 = CARTESIAN_POINT ( 'NONE',  ( 17.20831665107776587, 32.88393115100078745, 7.208316651077764980 ) ) ;
#7274 = CARTESIAN_POINT ( 'NONE',  ( 19.42250999205614548, 5.980352010821504471, -5.440088680355545492 ) ) ;
#7275 = CARTESIAN_POINT ( 'NONE',  ( 5.076628168052704559, 45.17559781766745175, -8.527530157486179263 ) ) ;
#7276 = CARTESIAN_POINT ( 'NONE',  ( 17.20831665107776587, 54.13393115100079456, -7.208316651077762316 ) ) ;
#7277 = CARTESIAN_POINT ( 'NONE',  ( 17.96484262340118221, 29.93868534415484106, 7.964842623401181321 ) ) ;
#7278 = ORIENTED_EDGE ( 'NONE', *, *, #26619, .F. ) ;
#7279 = ORIENTED_EDGE ( 'NONE', *, *, #2661, .F. ) ;
#7280 = CARTESIAN_POINT ( 'NONE',  ( 22.81628187352647785, 56.41530133659708213, 3.434112377981063169 ) ) ;
#7281 = VECTOR ( 'NONE', #85220, 1000.000000000000000 ) ;
#7282 = CARTESIAN_POINT ( 'NONE',  ( 6.000000000000000000, 61.00000000000000711, -6.500000000000000888 ) ) ;
#7283 = CARTESIAN_POINT ( 'NONE',  ( 10.00000000000000000, 9.758931151000785675, -9.846743663894594434 ) ) ;
#7284 = CARTESIAN_POINT ( 'NONE',  ( 21.09922568453595559, 52.04030133659708923, -6.408140936763230044 ) ) ;
#7286 = CARTESIAN_POINT ( 'NONE',  ( 10.00000000000000178, 52.25893115100078745, 9.846743663894594434 ) ) ;
#7285 = CARTESIAN_POINT ( 'NONE',  ( 0.5774900079438590739, 7.647018677488171434, -5.440088680355550821 ) ) ;
#7287 = FILL_AREA_STYLE_COLOUR ( '', #48816 ) ;
#7288 = B_SPLINE_CURVE_WITH_KNOTS ( 'NONE', 3,
 ( #67598, #8078, #97620, #69073, #29566, #609 ),
 .UNSPECIFIED., .F., .F.,
 ( 4, 2, 4 ),
 ( 0.000000000000000000, 0.0002565770811490998300, 0.0005131541622981996599 ),
 .UNSPECIFIED. ) ;
#7289 = CARTESIAN_POINT ( 'NONE',  ( 17.08211943468705840, 25.13708216824730357, -12.26659068614894466 ) ) ;
#7290 = CARTESIAN_POINT ( 'NONE',  ( -4.164238869374098151, 51.59541550158063217, -3.795296366450310543 ) ) ;
#7291 = CARTESIAN_POINT ( 'NONE',  ( 7.361572987183169658, 59.96726448433410894, -9.846743663894592657 ) ) ;
#7292 = SURFACE_STYLE_USAGE ( .BOTH. , #59285 ) ;
#7293 = CARTESIAN_POINT ( 'NONE',  ( 15.44008868035555260, 54.73035201082150536, 9.422509992056143702 ) ) ;
#7294 = EDGE_CURVE ( 'NONE', #19902, #89066, #74751, .T. ) ;
#7295 = CARTESIAN_POINT ( 'NONE',  ( 2.791683348922237240, 5.383931151000785675, -7.208316651077763204 ) ) ;
#7296 = SURFACE_STYLE_FILL_AREA ( #91267 ) ;
#7297 = ORIENTED_EDGE ( 'NONE', *, *, #44366, .T. ) ;
#7298 = CARTESIAN_POINT ( 'NONE',  ( 0.6178305044545838731, 54.74863466993042493, 9.382169495545420901 ) ) ;
#7299 = ORIENTED_EDGE ( 'NONE', *, *, #86151, .F. ) ;
#7300 = CARTESIAN_POINT ( 'NONE',  ( 5.076628168052704559, 10.17559781766745175, -8.527530157486179263 ) ) ;
#7301 = ORIENTED_EDGE ( 'NONE', *, *, #57955, .T. ) ;
#7302 = CIRCLE ( 'NONE', #28044, 0.2500000000000002220 ) ;
#7303 = CARTESIAN_POINT ( 'NONE',  ( 6.204703633549690345, 25.76208216824730712, -14.16423886937410259 ) ) ;
#7304 = CARTESIAN_POINT ( 'NONE',  ( 19.84674366389459266, 3.300597817667451750, 2.638427012816836559 ) ) ;
#7305 = CARTESIAN_POINT ( 'NONE',  ( 0.5774900079438607392, 28.48035201082150891, 5.440088680355550821 ) ) ;
#7306 = DIRECTION ( 'NONE',  ( 0.7353630527936689809, 0.6776733583268385042, 0.000000000000000000 ) ) ;
#7307 = ORIENTED_EDGE ( 'NONE', *, *, #48449, .T. ) ;
#7308 = CARTESIAN_POINT ( 'NONE',  ( 7.084665262690076126, 32.02201867748816966, -10.88017736071110164 ) ) ;
#7309 = VECTOR ( 'NONE', #78699, 1000.000000000000000 ) ;
#7310 = ORIENTED_EDGE ( 'NONE', *, *, #81256, .T. ) ;
#7311 = ORIENTED_EDGE ( 'NONE', *, *, #27705, .T. ) ;
#7312 = VERTEX_POINT ( 'NONE', #88271 ) ;
#7313 = CARTESIAN_POINT ( 'NONE',  ( 13.43411237798106583, 12.66530133659708746, -12.81628187352647252 ) ) ;
#7314 = CARTESIAN_POINT ( 'NONE',  ( 19.42250999205614548, 60.98035201082151247, -5.440088680355545492 ) ) ;
#7315 = CARTESIAN_POINT ( 'NONE',  ( 9.879999999999990123, 20.99999999999999645, 0.000000000000000000 ) ) ;
#7316 = DIRECTION ( 'NONE',  ( 0.000000000000000000, 1.000000000000000000, 0.000000000000000000 ) ) ;
#7317 = CARTESIAN_POINT ( 'NONE',  ( 1.472469842513823179, 11.42559781766745175, 4.923371831947296329 ) ) ;
#7318 = CARTESIAN_POINT ( 'NONE',  ( -0.8801773607111008646, 38.27201867748816255, 2.915334737309923430 ) ) ;
#7319 = COLOUR_RGB ( '', 0.08235294, 0.09019608, 0.10196078) ;
#7321 = VERTEX_POINT ( 'NONE', #42781 ) ;
#7320 = VECTOR ( 'NONE', #52176, 1000.000000000000000 ) ;
#7322 = AXIS2_PLACEMENT_3D ( 'NONE', #33384, #95891, #80873 ) ;
#7323 = ORIENTED_EDGE ( 'NONE', *, *, #9855, .F. ) ;
#7324 = CARTESIAN_POINT ( 'NONE',  ( 0.000000000000000000, 0.5000000000000004441, 0.000000000000000000 ) ) ;
#7325 = CARTESIAN_POINT ( 'NONE',  ( 15.44008868035555260, 44.73035201082151247, 9.422509992056143702 ) ) ;
#7326 = CARTESIAN_POINT ( 'NONE',  ( -1.926860441876563801, 22.66212336850780673, 1.004413902775740978E-15 ) ) ;
#7327 = B_SPLINE_CURVE_WITH_KNOTS ( 'NONE', 3,
 ( #56363, #11340, #42340, #64814, #55869, #3357 ),
 .UNSPECIFIED., .F., .F.,
 ( 4, 2, 4 ),
 ( 0.0002800056097769385239, 0.0006862108940652357231, 0.001092416178353533031 ),
 .UNSPECIFIED. ) ;
#7328 = AXIS2_PLACEMENT_3D ( 'NONE', #13014, #29986, #6505 ) ;
#7329 = CARTESIAN_POINT ( 'NONE',  ( 13.43411237798106583, 52.66530133659708213, -12.81628187352647252 ) ) ;
#7330 = CARTESIAN_POINT ( 'NONE',  ( 12.91533473730993009, 56.60535201082151247, -10.88017736071109987 ) ) ;
#7331 = CARTESIAN_POINT ( 'NONE',  ( -2.816281873526471635, -1.084698663402913210, -3.434112377981056508 ) ) ;
#7332 = DIRECTION ( 'NONE',  ( 1.000000000000000000, 0.000000000000000000, 0.000000000000000000 ) ) ;
#7333 = CARTESIAN_POINT ( 'NONE',  ( 10.00000000000000000, 19.75893115100078390, -9.846743663894594434 ) ) ;
#7334 = CARTESIAN_POINT ( 'NONE',  ( 21.09922568453595559, 57.04030133659708923, -6.408140936763230044 ) ) ;
#7335 = DIRECTION ( 'NONE',  ( 0.000000000000000000, 1.000000000000000000, 0.000000000000000000 ) ) ;
#7336 = CARTESIAN_POINT ( 'NONE',  ( 10.00000000000000178, 2.258931151000784787, 9.846743663894594434 ) ) ;
#7337 = CARTESIAN_POINT ( 'NONE',  ( 6.565887622018943937, 8.081968003263751754, -12.81628187352647608 ) ) ;
#7339 = CARTESIAN_POINT ( 'NONE',  ( 0.1532563361054082862, 66.21726448433413736, 2.638427012816831674 ) ) ;
#7338 = SURFACE_STYLE_FILL_AREA ( #6329 ) ;
#7340 = CARTESIAN_POINT ( 'NONE',  ( 4.559911319644449179, 33.89701867748817676, 9.422509992056141925 ) ) ;
#7341 = CARTESIAN_POINT ( 'NONE',  ( 10.00000000000000000, 44.75893115100078745, -9.846743663894594434 ) ) ;
#7342 = CARTESIAN_POINT ( 'NONE',  ( -1.926860441876563801, 32.66212336850780673, 1.004413902775740978E-15 ) ) ;
#7343 = ADVANCED_FACE ( 'NONE', ( #36262 ), #72619, .T. ) ;
#7344 = CARTESIAN_POINT ( 'NONE',  ( 2.791683348922237240, 15.38393115100078212, -7.208316651077763204 ) ) ;
#7345 = CARTESIAN_POINT ( 'NONE',  ( 12.63842701281683034, 7.467264484334118713, 9.846743663894596210 ) ) ;
#7347 = VERTEX_POINT ( 'NONE', #28261 ) ;
#7346 = CARTESIAN_POINT ( 'NONE',  ( 3.591859063236761518, -0.04303199673624671928, 11.09922568453594849 ) ) ;
#7348 = CARTESIAN_POINT ( 'NONE',  ( 2.035157376598824452, 3.688685344154837953, 7.964842623401179544 ) ) ;
#7349 = CARTESIAN_POINT ( 'NONE',  ( 19.84674366389459266, 63.71726448433412315, -2.638427012816827677 ) ) ;
#7350 = VECTOR ( 'NONE', #70197, 1000.000000000000000 ) ;
#7351 = CARTESIAN_POINT ( 'NONE',  ( 5.678900477119734447, -28.62996443916405909, -2.499999999996779909 ) ) ;
#7352 = CARTESIAN_POINT ( 'NONE',  ( 0.5774900079438590739, 7.647018677488171434, -5.440088680355550821 ) ) ;
#7353 = CARTESIAN_POINT ( 'NONE',  ( 7.361572987183169658, 39.96726448433411605, -9.846743663894592657 ) ) ;
#7354 = CARTESIAN_POINT ( 'NONE',  ( -0.1503990784575328643, 50.12777174578613426, 6.262539305110068177 ) ) ;
#7355 = CARTESIAN_POINT ( 'NONE',  ( -0.8801773607111008646, 8.272018677488171434, 2.915334737309923430 ) ) ;
#7356 = CARTESIAN_POINT ( 'NONE',  ( -11.81378540890942119, -0.03417435944610275333, 7.968498874458034287 ) ) ;
#7357 = CARTESIAN_POINT ( 'NONE',  ( 10.00000000000000178, 39.31368534415484106, 10.88017736071110342 ) ) ;
#7358 = CARTESIAN_POINT ( 'NONE',  ( 13.79529636645031943, 45.34541550158062506, -14.16423886937409904 ) ) ;
#7360 = DIRECTION ( 'NONE',  ( 0.000000000000000000, 1.000000000000000000, 0.000000000000000000 ) ) ;
#7359 = CARTESIAN_POINT ( 'NONE',  ( 6.204703633549690345, 62.84541550158063927, 14.16423886937410082 ) ) ;
#7361 = CARTESIAN_POINT ( 'NONE',  ( 5.076628168052703671, 6.842264484334118713, 8.527530157486179263 ) ) ;
#7362 = CARTESIAN_POINT ( 'NONE',  ( 1.472469842513823179, 31.42559781766745530, 4.923371831947296329 ) ) ;
#7363 = CARTESIAN_POINT ( 'NONE',  ( 19.38216949554541202, 15.99863466993042138, 9.382169495545424454 ) ) ;
#7364 = CARTESIAN_POINT ( 'NONE',  ( -14.48718990079891888, 4.171500096121077077E-16, -0.6093675230842403590 ) ) ;
#7365 = AXIS2_PLACEMENT_3D ( 'NONE', #10225, #2740, #79197 ) ;
#7366 = ORIENTED_EDGE ( 'NONE', *, *, #85870, .T. ) ;
#7367 = LINE ( 'NONE', #8338, #96015 ) ;
#7368 = CARTESIAN_POINT ( 'NONE',  ( 12.63842701281683034, 57.46726448433411605, 9.846743663894596210 ) ) ;
#7369 = DIRECTION ( 'NONE',  ( -0.000000000000000000, -1.000000000000000000, -0.000000000000000000 ) ) ;
#7370 = CARTESIAN_POINT ( 'NONE',  ( -10.07341714983716230, -32.14978703225411039, -4.000000000000000000 ) ) ;
#7371 = CARTESIAN_POINT ( 'NONE',  ( -4.164238869374098151, 6.595415501580634832, -3.795296366450310543 ) ) ;
#7372 = CARTESIAN_POINT ( 'NONE',  ( 14.92337183194729633, 22.67559781766745175, 8.527530157486181039 ) ) ;
#7373 = EDGE_CURVE ( 'NONE', #8435, #4994, #26315, .T. ) ;
#7374 = SURFACE_STYLE_USAGE ( .BOTH. , #36876 ) ;
#7375 = VERTEX_POINT ( 'NONE', #74241 ) ;
#7376 = CARTESIAN_POINT ( 'NONE',  ( -2.266590686148945544, 52.22041550158064638, 7.082119434687048631 ) ) ;
#7377 = CARTESIAN_POINT ( 'NONE',  ( 1.472469842513823179, 11.42559781766745175, 4.923371831947296329 ) ) ;
#7379 = DIRECTION ( 'NONE',  ( 0.000000000000000000, 1.000000000000000000, 0.000000000000000000 ) ) ;
#7378 = SURFACE_STYLE_USAGE ( .BOTH. , #39347 ) ;
#7380 = CARTESIAN_POINT ( 'NONE',  ( 15.44008868035555260, 34.73035201082151247, 9.422509992056143702 ) ) ;
#7381 = CARTESIAN_POINT ( 'NONE',  ( 10.00000000000000000, 47.87363466993042493, -12.81628187352647608 ) ) ;
#7382 = EDGE_CURVE ( 'NONE', #52640, #98966, #82197, .T. ) ;
#7383 = CARTESIAN_POINT ( 'NONE',  ( 19.42250999205614193, 10.14701867748816966, 5.440088680355555262 ) ) ;
#7385 = ORIENTED_EDGE ( 'NONE', *, *, #16385, .F. ) ;
#7384 = CARTESIAN_POINT ( 'NONE',  ( 3.591859063236761518, 34.95696800326375353, 11.09922568453594849 ) ) ;
#7386 = CARTESIAN_POINT ( 'NONE',  ( 2.791683348922237240, 5.383931151000785675, -7.208316651077763204 ) ) ;
#7387 = ORIENTED_EDGE ( 'NONE', *, *, #94690, .T. ) ;
#7388 = CARTESIAN_POINT ( 'NONE',  ( -9.543993260087553665, -28.01899697271202427, -4.000000000000000000 ) ) ;
#7389 = CARTESIAN_POINT ( 'NONE',  ( -0.3689425029237881626, 42.42874883491396787, 10.36894250292379027 ) ) ;
#7390 = CARTESIAN_POINT ( 'NONE',  ( 6.204703633549690345, 12.84541550158063572, 14.16423886937410082 ) ) ;
#7391 = CARTESIAN_POINT ( 'NONE',  ( 15.44008868035555260, 4.730352010821504471, 9.422509992056143702 ) ) ;
#7392 = CARTESIAN_POINT ( 'NONE',  ( 19.42250999205614548, 40.98035201082150536, -5.440088680355545492 ) ) ;
#7393 = CARTESIAN_POINT ( 'NONE',  ( -14.74963345907814016, 14.95077488074853456, -0.3072669459662672464 ) ) ;
#7394 = SURFACE_STYLE_FILL_AREA ( #5902 ) ;
#7395 = CARTESIAN_POINT ( 'NONE',  ( 12.91533473730992121, 59.52201867748816966, 10.88017736071110164 ) ) ;
#7396 = CARTESIAN_POINT ( 'NONE',  ( 19.42250999205614193, 65.14701867748817676, 5.440088680355555262 ) ) ;
#7397 = CARTESIAN_POINT ( 'NONE',  ( 19.38216949554541202, 25.99863466993042138, 9.382169495545424454 ) ) ;
#7398 = CARTESIAN_POINT ( 'NONE',  ( 14.88232117145531319, 14.63595249122790598, -1.875237731503143879 ) ) ;
#7399 = CARTESIAN_POINT ( 'NONE',  ( -5.963430220938278126, 3.495456701841148650, 10.32896413005680358 ) ) ;
#7400 = CARTESIAN_POINT ( 'NONE',  ( 0.1532563361054100626, 30.80059781766744820, -2.638427012816831230 ) ) ;
#7401 = VECTOR ( 'NONE', #33935, 1000.000000000000000 ) ;
#7402 = VECTOR ( 'NONE', #88247, 1000.000000000000114 ) ;
#7403 = TOROIDAL_SURFACE ( 'NONE', #85612, 14.49999999999999822, 0.5000000000000000000 ) ;
#7404 = CARTESIAN_POINT ( 'NONE',  ( 19.38216949554541202, 20.99863466993042138, 9.382169495545424454 ) ) ;
#7405 = EDGE_CURVE ( 'NONE', #53047, #62035, #19287, .T. ) ;
#7406 = CARTESIAN_POINT ( 'NONE',  ( 7.361572987183169658, -0.03273551566588185635, -9.846743663894592657 ) ) ;
#7407 = CARTESIAN_POINT ( 'NONE',  ( 4.559911319644449179, 8.897018677488171434, 9.422509992056141925 ) ) ;
#7408 = AXIS2_PLACEMENT_3D ( 'NONE', #44692, #6699, #98216 ) ;
#7409 = CARTESIAN_POINT ( 'NONE',  ( 19.84674366389459266, 38.71726448433412315, -2.638427012816827677 ) ) ;
#7410 = CARTESIAN_POINT ( 'NONE',  ( -23.44000000000000838, 92.00000000000000000, -10.09898361729590199 ) ) ;
#7412 = CARTESIAN_POINT ( 'NONE',  ( 6.204703633549690345, 2.845415501580634388, 14.16423886937410082 ) ) ;
#7411 = CARTESIAN_POINT ( 'NONE',  ( 10.00000000000000178, 17.25893115100078745, 9.846743663894594434 ) ) ;
#7413 = CARTESIAN_POINT ( 'NONE',  ( 2.917880565312950480, 0.9704155015806342766, -12.26659068614894821 ) ) ;
#7414 = DIRECTION ( 'NONE',  ( -0.000000000000000000, -0.000000000000000000, -1.000000000000000000 ) ) ;
#7415 = CARTESIAN_POINT ( 'NONE',  ( 4.559911319644449179, 38.89701867748817676, 9.422509992056141925 ) ) ;
#7417 = CARTESIAN_POINT ( 'NONE',  ( 20.36894250292379738, 44.92874883491396787, -10.36894250292379027 ) ) ;
#7416 = CARTESIAN_POINT ( 'NONE',  ( 11.22915323889580463, 0.000000000000000000, -8.773176023390609757 ) ) ;
#7418 = CARTESIAN_POINT ( 'NONE',  ( 20.88017736071110519, 25.56368534415483751, 2.639326808657452039E-16 ) ) ;
#7419 = CARTESIAN_POINT ( 'NONE',  ( 4.559911319644449179, 13.89701867748817321, 9.422509992056141925 ) ) ;
#7420 = ORIENTED_EDGE ( 'NONE', *, *, #36870, .F. ) ;
#7421 = CARTESIAN_POINT ( 'NONE',  ( 12.91533473730992121, 24.52201867748816966, 10.88017736071110164 ) ) ;
#7422 = CARTESIAN_POINT ( 'NONE',  ( 22.81628187352647785, 46.41530133659708213, 3.434112377981063169 ) ) ;
#7424 = AXIS2_PLACEMENT_3D ( 'NONE', #17687, #34129, #79652 ) ;
#7423 = CARTESIAN_POINT ( 'NONE',  ( 20.88017736071110875, 45.77201867748816966, -2.915334737309920765 ) ) ;
#7425 = CARTESIAN_POINT ( 'NONE',  ( 0.5774900079438590739, 57.64701867748817676, -5.440088680355550821 ) ) ;
#7426 = ORIENTED_EDGE ( 'NONE', *, *, #54855, .T. ) ;
#7427 = MECHANICAL_DESIGN_GEOMETRIC_PRESENTATION_REPRESENTATION (  '', ( #95248 ), #79273 ) ;
#7428 = CARTESIAN_POINT ( 'NONE',  ( -0.8801773607111009756, 38.06368534415484106, 1.068504757029289695E-15 ) ) ;
#7429 = DIRECTION ( 'NONE',  ( 1.000000000000000000, 6.938893903907221278E-15, -0.000000000000000000 ) ) ;
#7430 = LINE ( 'NONE', #38410, #70046 ) ;
#7431 = CARTESIAN_POINT ( 'NONE',  ( -4.164238869374099039, 41.80374883491397497, 8.674139862899312516E-16 ) ) ;
#7432 = CARTESIAN_POINT ( 'NONE',  ( 2.035157376598822676, 67.43868534415484817, -7.964842623401177768 ) ) ;
#7433 = CARTESIAN_POINT ( 'NONE',  ( 19.80777595082616216, 25.68878173731741299, -6.499999999999960920 ) ) ;
#7434 = CARTESIAN_POINT ( 'NONE',  ( 10.00000000000000000, -0.2410688489992152128, -9.846743663894594434 ) ) ;
#7435 = CARTESIAN_POINT ( 'NONE',  ( 0.1532563361054100626, 60.80059781766744464, -2.638427012816831230 ) ) ;
#7436 = CARTESIAN_POINT ( 'NONE',  ( -14.99847009497948669, 14.63606908182952715, 0.2142307401079193430 ) ) ;
#7437 = CARTESIAN_POINT ( 'NONE',  ( 12.63842701281683034, 27.46726448433411250, 9.846743663894596210 ) ) ;
#7438 = CARTESIAN_POINT ( 'NONE',  ( 17.20831665107776587, 39.13393115100079456, -7.208316651077762316 ) ) ;
#7439 = CARTESIAN_POINT ( 'NONE',  ( 12.81628187352647608, -23.58469866340291432, 3.434112377981052511 ) ) ;
#7440 = CARTESIAN_POINT ( 'NONE',  ( 4.559911319644449179, 27.23035201082150536, -9.422509992056141925 ) ) ;
#7441 = CARTESIAN_POINT ( 'NONE',  ( 17.20831665107776587, 42.88393115100077324, 7.208316651077764980 ) ) ;
#7443 = CARTESIAN_POINT ( 'NONE',  ( 17.96484262340118221, 56.18868534415484817, -7.964842623401177768 ) ) ;
#7442 = CARTESIAN_POINT ( 'NONE',  ( 19.39188664607695500, 25.83703382326400089, -6.499999999999964473 ) ) ;
#7445 = PRESENTATION_STYLE_ASSIGNMENT (( #98955 ) ) ;
#7444 = CARTESIAN_POINT ( 'NONE',  ( 2.035157376598822676, 37.43868534415484106, -7.964842623401177768 ) ) ;
#7446 = CARTESIAN_POINT ( 'NONE',  ( 20.36894250292379382, 53.67874883491397497, 10.36894250292379205 ) ) ;
#7447 = MECHANICAL_DESIGN_GEOMETRIC_PRESENTATION_REPRESENTATION (  '', ( #1091 ), #26608 ) ;
#7448 = MECHANICAL_DESIGN_GEOMETRIC_PRESENTATION_REPRESENTATION (  '', ( #55310 ), #40777 ) ;
#7449 = CARTESIAN_POINT ( 'NONE',  ( -1.099225684535947600, 23.70696800326375708, -6.408140936763238038 ) ) ;
#7450 = DIRECTION ( 'NONE',  ( -0.000000000000000000, -1.000000000000000000, 0.000000000000000000 ) ) ;
#7451 = ORIENTED_EDGE ( 'NONE', *, *, #10767, .F. ) ;
#7452 = CARTESIAN_POINT ( 'NONE',  ( -2.816281873526473856, 14.33196800326375531, 3.434112377981055619 ) ) ;
#7453 = CARTESIAN_POINT ( 'NONE',  ( 0.5774900079438607392, 13.48035201082150358, 5.440088680355550821 ) ) ;
#7454 = CARTESIAN_POINT ( 'NONE',  ( 7.084665262690076126, 47.02201867748818387, -10.88017736071110164 ) ) ;
#7455 = VERTEX_POINT ( 'NONE', #4297 ) ;
#7456 = CARTESIAN_POINT ( 'NONE',  ( 12.91533473730992121, 54.52201867748816255, 10.88017736071110164 ) ) ;
#7457 = CARTESIAN_POINT ( 'NONE',  ( 14.92337183194729988, 39.34226448433412315, -8.527530157486177487 ) ) ;
#7458 = CARTESIAN_POINT ( 'NONE',  ( 19.84674366389459266, 23.71726448433412315, -2.638427012816827677 ) ) ;
#7459 = AXIS2_PLACEMENT_3D ( 'NONE', #53332, #37864, #37370 ) ;
#7460 = CARTESIAN_POINT ( 'NONE',  ( 19.84674366389459266, 18.71726448433411960, -2.638427012816827677 ) ) ;
#7461 =( NAMED_UNIT ( * ) SI_UNIT ( $, .STERADIAN. ) SOLID_ANGLE_UNIT ( ) );
#7463 = CARTESIAN_POINT ( 'NONE',  ( 19.38216949554541202, 35.99863466993041072, 9.382169495545424454 ) ) ;
#7462 = FACE_OUTER_BOUND ( 'NONE', #47362, .T. ) ;
#7464 = ADVANCED_FACE ( 'NONE', ( #34771 ), #31159, .T. ) ;
#7466 = CARTESIAN_POINT ( 'NONE',  ( -5.795997163830251431, -0.03417435944610275333, 13.01802277140702024 ) ) ;
#7465 = CARTESIAN_POINT ( 'NONE',  ( 0.1532563361054082862, 16.21726448433411960, 2.638427012816831674 ) ) ;
#7467 = CARTESIAN_POINT ( 'NONE',  ( 7.155629327958947350, -69.45263185074750822, -4.000000000000000000 ) ) ;
#7468 = AXIS2_PLACEMENT_3D ( 'NONE', #71794, #19282, #65254 ) ;
#7470 = ORIENTED_EDGE ( 'NONE', *, *, #63443, .T. ) ;
#7469 = CARTESIAN_POINT ( 'NONE',  ( 18.52753015748618282, 28.92559781766745175, -4.923371831947291888 ) ) ;
#7471 = DIRECTION ( 'NONE',  ( -0.09584575252021386438, 0.000000000000000000, -0.9953961983671798519 ) ) ;
#7472 = B_SPLINE_CURVE_WITH_KNOTS ( 'NONE', 3,
 ( #54194, #97762, #91715, #29718, #29227, #68723 ),
 .UNSPECIFIED., .F., .F.,
 ( 4, 2, 4 ),
 ( 2.221529986854170345E-17, 0.0002504968758227833921, 0.0005009937516455445581 ),
 .UNSPECIFIED. ) ;
#7473 = CARTESIAN_POINT ( 'NONE',  ( 10.00000000000000178, 15.37363466993042138, 12.81628187352647608 ) ) ;
#7474 = CARTESIAN_POINT ( 'NONE',  ( 4.559911319644449179, 58.89701867748817676, 9.422509992056141925 ) ) ;
#7475 = CIRCLE ( 'NONE', #44120, 0.5000000000000004441 ) ;
#7476 = CARTESIAN_POINT ( 'NONE',  ( 24.16423886937410614, 34.51208216824731068, -3.795296366450302550 ) ) ;
#7477 = UNCERTAINTY_MEASURE_WITH_UNIT (LENGTH_MEASURE( 1.000000000000000082E-05 ), #30333, 'distance_accuracy_value', 'NONE');
#7478 = CARTESIAN_POINT ( 'NONE',  ( -12.79762580178202214, 90.64749249312531276, 7.346077433007431878 ) ) ;
#7479 = CARTESIAN_POINT ( 'NONE',  ( 13.79529636645030344, 33.26208216824730357, 14.16423886937410614 ) ) ;
#7480 = CARTESIAN_POINT ( 'NONE',  ( -0.3689425029237898834, 56.17874883491396076, -10.36894250292378850 ) ) ;
#7481 = CARTESIAN_POINT ( 'NONE',  ( 22.26659068614894466, 8.887082168247300018, 7.082119434687054849 ) ) ;
#7483 = CARTESIAN_POINT ( 'NONE',  ( -0.3289641300567998083, 38.07879003517447103, 5.963430220938281678 ) ) ;
#7482 = CARTESIAN_POINT ( 'NONE',  ( 13.79529636645031943, 20.34541550158063572, -14.16423886937409904 ) ) ;
#7484 = CARTESIAN_POINT ( 'NONE',  ( 10.00000000000000178, 49.31368534415484106, 10.88017736071110342 ) ) ;
#7485 = CARTESIAN_POINT ( 'NONE',  ( 4.380000000000000782, 1.019547802438464545, -2.750000000000000000 ) ) ;
#7487 = CARTESIAN_POINT ( 'NONE',  ( 17.20831665107776587, 47.88393115100078745, 7.208316651077764980 ) ) ;
#7486 = DIRECTION ( 'NONE',  ( -1.000000000000000000, 0.000000000000000000, -0.000000000000000000 ) ) ;
#7488 = CARTESIAN_POINT ( 'NONE',  ( 2.035157376598824452, 18.68868534415484106, 7.964842623401179544 ) ) ;
#7489 = CARTESIAN_POINT ( 'NONE',  ( 13.43411237798106583, 57.66530133659708923, -12.81628187352647252 ) ) ;
#7490 = CARTESIAN_POINT ( 'NONE',  ( 12.63842701281683922, 59.55059781766744464, -9.846743663894590881 ) ) ;
#7491 = CARTESIAN_POINT ( 'NONE',  ( 20.00000000000000711, 79.40087001978915282, -4.500000000000000888 ) ) ;
#7492 = CARTESIAN_POINT ( 'NONE',  ( 7.361572987183169658, 29.96726448433411960, -9.846743663894592657 ) ) ;
#7494 = CARTESIAN_POINT ( 'NONE',  ( 0.6178305044545818747, 58.49863466993042493, -9.382169495545419124 ) ) ;
#7493 = VECTOR ( 'NONE', #31432, 1000.000000000000000 ) ;
#7495 = CARTESIAN_POINT ( 'NONE',  ( -14.16423886937410437, -18.40458449841936073, -3.795296366450299885 ) ) ;
#7496 = AXIS2_PLACEMENT_3D ( 'NONE', #84136, #7656, #70606 ) ;
#7497 = CARTESIAN_POINT ( 'NONE',  ( 7.084665262690076126, 47.02201867748818387, -10.88017736071110164 ) ) ;
#7498 = CARTESIAN_POINT ( 'NONE',  ( 1.472469842513823179, 50.59226448433411605, -4.923371831947296329 ) ) ;
#7499 = CARTESIAN_POINT ( 'NONE',  ( 2.917880565312950480, 40.97041550158063217, -12.26659068614894821 ) ) ;
#7501 = ADVANCED_FACE ( 'NONE', ( #65258 ), #63136, .T. ) ;
#7500 = VECTOR ( 'NONE', #33517, 1000.000000000000000 ) ;
#7502 = ORIENTED_EDGE ( 'NONE', *, *, #89283, .F. ) ;
#7503 = CARTESIAN_POINT ( 'NONE',  ( 24.16423886937410614, 4.512082168247300906, -3.795296366450302550 ) ) ;
#7504 = CARTESIAN_POINT ( 'NONE',  ( 12.91533473730992121, 64.52201867748817676, 10.88017736071110164 ) ) ;
#7505 = CARTESIAN_POINT ( 'NONE',  ( 0.000000000000000000, 70.25000000000000000, -6.250000000000000000 ) ) ;
#7506 = CARTESIAN_POINT ( 'NONE',  ( 24.16423886937409904, 59.09541550158063217, 3.795296366450317205 ) ) ;
#7507 = CARTESIAN_POINT ( 'NONE',  ( 19.38216949554541202, 15.99863466993042138, 9.382169495545424454 ) ) ;
#7508 = CYLINDRICAL_SURFACE ( 'NONE', #84814, 15.00000000000000000 ) ;
#7509 = CARTESIAN_POINT ( 'NONE',  ( 4.559911319644449179, 57.23035201082150536, -9.422509992056141925 ) ) ;
#7510 = CARTESIAN_POINT ( 'NONE',  ( -6.715867195167276371, 4.396228481599465503E-16, -12.85095824508335838 ) ) ;
#7511 = CARTESIAN_POINT ( 'NONE',  ( -46.69421152571126044, 101.0768001808267229, -8.798454068542781670 ) ) ;
#7512 = CARTESIAN_POINT ( 'NONE',  ( 7.084665262690076126, 2.022018677488171434, -10.88017736071110164 ) ) ;
#7513 = CARTESIAN_POINT ( 'NONE',  ( 10.88017736071110519, 30.56368534415485172, -2.602085213965210642E-15 ) ) ;
#7514 = CARTESIAN_POINT ( 'NONE',  ( 10.00000000000000000, 11.81368534415483751, -10.88017736071110342 ) ) ;
#7515 = CARTESIAN_POINT ( 'NONE',  ( 15.44008868035555793, 21.39701867748817321, -9.422509992056140149 ) ) ;
#7516 = CARTESIAN_POINT ( 'NONE',  ( 14.92337183194729988, 59.34226448433412315, -8.527530157486177487 ) ) ;
#7517 = CARTESIAN_POINT ( 'NONE',  ( 19.38216949554541557, 52.24863466993041072, -9.382169495545420901 ) ) ;
#7518 = FACE_OUTER_BOUND ( 'NONE', #65659, .T. ) ;
#7519 = ORIENTED_EDGE ( 'NONE', *, *, #30483, .F. ) ;
#7520 = CARTESIAN_POINT ( 'NONE',  ( 2.035157376598824452, 13.68868534415483751, 7.964842623401179544 ) ) ;
#7521 = CARTESIAN_POINT ( 'NONE',  ( 21.09922568453594849, 21.20696800326375353, 6.408140936763242479 ) ) ;
#7522 = DIRECTION ( 'NONE',  ( 0.4146932426562462415, 0.000000000000000000, -0.9099612708765399960 ) ) ;
#7523 = B_SPLINE_CURVE_WITH_KNOTS ( 'NONE', 3,
 ( #19032, #43976, #51993, #73489, #36989, #97020, #58990, #97511 ),
 .UNSPECIFIED., .F., .F.,
 ( 4, 2, 2, 4 ),
 ( 0.000000000000000000, 0.0004516266542298916719, 0.0009032533084597833438, 0.001806506616919566688 ),
 .UNSPECIFIED. ) ;
#7524 = CARTESIAN_POINT ( 'NONE',  ( 5.076628168052704559, 45.17559781766745175, -8.527530157486179263 ) ) ;
#7525 = CARTESIAN_POINT ( 'NONE',  ( 2.035157376598822676, 32.43868534415483396, -7.964842623401177768 ) ) ;
#7526 = CARTESIAN_POINT ( 'NONE',  ( 0.6178305044545818747, 28.49863466993041783, -9.382169495545419124 ) ) ;
#7528 = CARTESIAN_POINT ( 'NONE',  ( 19.10478245763048477, 16.02576239577082262, -5.990408912944377384 ) ) ;
#7527 = CARTESIAN_POINT ( 'NONE',  ( 4.559911319644449179, 43.89701867748816966, 9.422509992056141925 ) ) ;
#7529 = CARTESIAN_POINT ( 'NONE',  ( 17.85999999999999943, 37.99999999999997868, 9.500000000000000000 ) ) ;
#7530 = CARTESIAN_POINT ( 'NONE',  ( 10.00000000000000000, 52.87363466993041783, -12.81628187352647608 ) ) ;
#7531 = EDGE_LOOP ( 'NONE', ( #29161, #50480, #72220, #63227, #60300, #25160 ) ) ;
#7532 = CARTESIAN_POINT ( 'NONE',  ( 20.88017736071110519, 55.56368534415484817, 2.639326808657452039E-16 ) ) ;
#7534 = CARTESIAN_POINT ( 'NONE',  ( 2.917880565312948704, 7.637082168247301794, 12.26659068614894643 ) ) ;
#7533 = CARTESIAN_POINT ( 'NONE',  ( 10.00000000000000000, 27.87363466993042138, -12.81628187352647608 ) ) ;
#7535 = CARTESIAN_POINT ( 'NONE',  ( 2.791683348922237240, 5.383931151000785675, -7.208316651077763204 ) ) ;
#7536 = CARTESIAN_POINT ( 'NONE',  ( -0.8801773607111008646, 58.27201867748816966, 2.915334737309923430 ) ) ;
#7537 = CARTESIAN_POINT ( 'NONE',  ( 6.204703633549690345, 42.84541550158063217, 14.16423886937410082 ) ) ;
#7538 = CARTESIAN_POINT ( 'NONE',  ( 12.63842701281683034, 62.46726448433410894, 9.846743663894596210 ) ) ;
#7539 = CARTESIAN_POINT ( 'NONE',  ( 17.20831665107776587, 12.88393115100078390, 7.208316651077764980 ) ) ;
#7540 = EDGE_CURVE ( 'NONE', #55430, #12785, #82268, .T. ) ;
#7541 = CARTESIAN_POINT ( 'NONE',  ( 2.791683348922237240, 5.383931151000785675, -7.208316651077763204 ) ) ;
#7542 = DIRECTION ( 'NONE',  ( 0.000000000000000000, 0.000000000000000000, -1.000000000000000000 ) ) ;
#7543 = CARTESIAN_POINT ( 'NONE',  ( -2.266590686148945544, 42.22041550158063217, 7.082119434687048631 ) ) ;
#7544 =( BOUNDED_CURVE ( )  B_SPLINE_CURVE ( 2, ( #57325, #87819, #13311, #11339, #95836, #74291, #73806, #64813, #34315 ),
 .UNSPECIFIED., .F., .T. ) 
 B_SPLINE_CURVE_WITH_KNOTS ( ( 3, 2, 2, 2, 3 ),
 ( 0.009663273234349279567, 0.01190476190476190410, 0.01785714285714285615, 0.02380952380952380820, 0.02605726409658919510 ),
 .UNSPECIFIED. ) 
 CURVE ( )  GEOMETRIC_REPRESENTATION_ITEM ( )  RATIONAL_B_SPLINE_CURVE ( ( 0.9840011491998950088, 0.9871686851131101781, 1.000000000000000000, 0.9659258262890683122, 1.000000000000000000, 0.9659258262890683122, 1.000000000000000000, 0.9871328979762477029, 0.9839835555609426354 ) ) 
 REPRESENTATION_ITEM ( '' )  );
#7545 = DIRECTION ( 'NONE',  ( -0.000000000000000000, -1.000000000000000000, -0.000000000000000000 ) ) ;
#7546 = EDGE_CURVE ( 'NONE', #47538, #32615, #74267, .T. ) ;
#7547 = CARTESIAN_POINT ( 'NONE',  ( 20.88017736071110164, 10.35535201082150714, 2.915334737309930979 ) ) ;
#7548 = CARTESIAN_POINT ( 'NONE',  ( -7.232415441807423129, -88.12698951299773853, -4.000000000000000000 ) ) ;
#7549 = COLOUR_RGB ( '', 0.40784314, 0.44705882, 0.49803922) ;
#7550 = VERTEX_POINT ( 'NONE', #14266 ) ;
#7551 = CARTESIAN_POINT ( 'NONE',  ( 15.44008868035555260, 4.730352010821505360, 9.422509992056143702 ) ) ;
#7552 = CARTESIAN_POINT ( 'NONE',  ( 0.5774900079438590739, 2.647018677488171434, -5.440088680355550821 ) ) ;
#7553 = CARTESIAN_POINT ( 'NONE',  ( 12.63842701281683922, 49.55059781766744464, -9.846743663894590881 ) ) ;
#7554 = CARTESIAN_POINT ( 'NONE',  ( 22.81628187352648496, 41.83196800326375353, -3.434112377981050290 ) ) ;
#7555 = CARTESIAN_POINT ( 'NONE',  ( -4.181050312904877941, 15.00000000000000888, -14.01631781289607659 ) ) ;
#7557 = CARTESIAN_POINT ( 'NONE',  ( 13.79529636645030344, 3.262082168247301350, 14.16423886937410614 ) ) ;
#7556 = CARTESIAN_POINT ( 'NONE',  ( 2.361410439757328117, 0.2306972965111871443, -14.75336556272936228 ) ) ;
#7558 = CARTESIAN_POINT ( 'NONE',  ( -0.8801773607110991993, 12.85535201082150358, -2.915334737309923874 ) ) ;
#7559 = CARTESIAN_POINT ( 'NONE',  ( 2.917880565312948704, 67.63708216824730357, 12.26659068614894643 ) ) ;
#7560 = PRODUCT ( 'MAS-685', 'MAS-685', '', ( #5744 ) ) ;
#7561 = CIRCLE ( 'NONE', #71417, 0.2500000000000002220 ) ;
#7562 = CARTESIAN_POINT ( 'NONE',  ( 14.92337183194729633, 47.67559781766745175, 8.527530157486181039 ) ) ;
#7563 = CARTESIAN_POINT ( 'NONE',  ( 18.06765999051787119, 43.99127512925446126, 6.499999999999926281 ) ) ;
#7564 = CARTESIAN_POINT ( 'NONE',  ( 1.472469842513823179, 26.42559781766745175, 4.923371831947296329 ) ) ;
#7565 = CARTESIAN_POINT ( 'NONE',  ( 0.8952175423694952450, 33.52576239577081907, 5.990408912944338304 ) ) ;
#7566 = CARTESIAN_POINT ( 'NONE',  ( -3.469446951953614189E-15, 19.75893115100078745, -9.846743663894594434 ) ) ;
#7567 = ORIENTED_EDGE ( 'NONE', *, *, #23183, .F. ) ;
#7568 = ORIENTED_EDGE ( 'NONE', *, *, #83927, .F. ) ;
#7569 = CARTESIAN_POINT ( 'NONE',  ( -22.44000000000001194, 93.50000000000000000, -10.09898361729590199 ) ) ;
#7570 = EDGE_LOOP ( 'NONE', ( #82632, #60248, #32625, #25427, #36388, #54669 ) ) ;
#7571 = CARTESIAN_POINT ( 'NONE',  ( 14.92337183194729633, 52.67559781766745175, 8.527530157486181039 ) ) ;
#7573 = CARTESIAN_POINT ( 'NONE',  ( 20.88017736071110519, 35.56368534415484106, 2.639326808657452039E-16 ) ) ;
#7572 = CARTESIAN_POINT ( 'NONE',  ( 4.559911319644449179, 28.89701867748817321, 9.422509992056141925 ) ) ;
#7575 = CARTESIAN_POINT ( 'NONE',  ( 13.43411237798105340, 25.58196800326374998, 12.81628187352647963 ) ) ;
#7574 = CARTESIAN_POINT ( 'NONE',  ( 14.92337183194729988, 59.34226448433412315, -8.527530157486177487 ) ) ;
#7576 = AXIS2_PLACEMENT_3D ( 'NONE', #15215, #81830, #51345 ) ;
#7577 = CIRCLE ( 'NONE', #79348, 14.49999999999999822 ) ;
#7578 = CARTESIAN_POINT ( 'NONE',  ( 21.09922568453595559, 42.04030133659708213, -6.408140936763230044 ) ) ;
#7579 = ORIENTED_EDGE ( 'NONE', *, *, #88779, .F. ) ;
#7580 = CARTESIAN_POINT ( 'NONE',  ( 17.20831665107776587, 49.13393115100078745, -7.208316651077762316 ) ) ;
#7581 = CARTESIAN_POINT ( 'NONE',  ( 20.88017736071110519, 5.563685344154838397, 2.639326808657452039E-16 ) ) ;
#7582 = ORIENTED_EDGE ( 'NONE', *, *, #84272, .F. ) ;
#7583 = CARTESIAN_POINT ( 'NONE',  ( 12.91533473730993009, 21.60535201082150536, -10.88017736071109987 ) ) ;
#7584 = ORIENTED_EDGE ( 'NONE', *, *, #9982, .T. ) ;
#7585 = CARTESIAN_POINT ( 'NONE',  ( 2.035157376598824452, 63.68868534415484106, 7.964842623401179544 ) ) ;
#7586 = CARTESIAN_POINT ( 'NONE',  ( 20.88017736071110164, 60.35535201082151957, 2.915334737309930979 ) ) ;
#7587 = DIRECTION ( 'NONE',  ( 0.000000000000000000, 0.000000000000000000, 1.000000000000000000 ) ) ;
#7588 = CARTESIAN_POINT ( 'NONE',  ( 0.5774900079438590739, 57.64701867748817676, -5.440088680355550821 ) ) ;
#7589 = EDGE_CURVE ( 'NONE', #35045, #55728, #38736, .T. ) ;
#7590 = CARTESIAN_POINT ( 'NONE',  ( -46.94000000000240647, 102.7387969410439723, 6.737038697110675045 ) ) ;
#7591 = ORIENTED_EDGE ( 'NONE', *, *, #42129, .T. ) ;
#7592 = CARTESIAN_POINT ( 'NONE',  ( 12.63842701281683034, 42.46726448433412315, 9.846743663894596210 ) ) ;
#7593 = ORIENTED_EDGE ( 'NONE', *, *, #39541, .F. ) ;
#7594 = DIRECTION ( 'NONE',  ( -1.000000000000000000, 0.000000000000000000, 0.000000000000000000 ) ) ;
#7595 = AXIS2_PLACEMENT_3D ( 'NONE', #4925, #73397, #21404 ) ;
#7596 = ORIENTED_EDGE ( 'NONE', *, *, #97466, .T. ) ;
#7597 = DIRECTION ( 'NONE',  ( 0.8070303256584298035, -0.5905099943842175847, 0.000000000000000000 ) ) ;
#7599 = CARTESIAN_POINT ( 'NONE',  ( 2.035157376598824452, 58.68868534415482685, 7.964842623401179544 ) ) ;
#7598 = DIRECTION ( 'NONE',  ( -0.000000000000000000, -1.000000000000000000, -0.000000000000000000 ) ) ;
#7600 = CARTESIAN_POINT ( 'NONE',  ( 10.00000000000000178, 9.313685344154839285, 10.88017736071110342 ) ) ;
#7601 = CARTESIAN_POINT ( 'NONE',  ( -0.03743638938522109161, 59.25197528031019090, -6.399506433553975526 ) ) ;
#7603 = ORIENTED_EDGE ( 'NONE', *, *, #44754, .T. ) ;
#7602 = CARTESIAN_POINT ( 'NONE',  ( 21.09922568453594849, 41.20696800326375353, 6.408140936763242479 ) ) ;
#7604 = DIRECTION ( 'NONE',  ( 0.000000000000000000, 0.000000000000000000, 1.000000000000000000 ) ) ;
#7605 = CARTESIAN_POINT ( 'NONE',  ( 18.52753015748617571, 43.09226448433412315, 4.923371831947298993 ) ) ;
#7606 = CARTESIAN_POINT ( 'NONE',  ( 12.63842701281683922, 4.550597817667451750, -9.846743663894590881 ) ) ;
#7607 = CARTESIAN_POINT ( 'NONE',  ( 0.6178305044545838731, 24.74863466993042493, 9.382169495545420901 ) ) ;
#7608 = CARTESIAN_POINT ( 'NONE',  ( 0.1532563361054100626, 20.80059781766744464, -2.638427012816831230 ) ) ;
#7609 = SURFACE_SIDE_STYLE ('',( #16576 ) ) ;
#7610 = CARTESIAN_POINT ( 'NONE',  ( 0.1532563361054100626, 20.80059781766744464, -2.638427012816831230 ) ) ;
#7611 = CARTESIAN_POINT ( 'NONE',  ( -1.099225684535947600, 14.54030133659708568, 6.408140936763237150 ) ) ;
#7612 =( BOUNDED_CURVE ( )  B_SPLINE_CURVE ( 2, ( #90633, #22157, #73658, #96689, #58662, #48510, #33495, #63994, #56517 ),
 .UNSPECIFIED., .F., .F. ) 
 B_SPLINE_CURVE_WITH_KNOTS ( ( 3, 2, 2, 2, 3 ),
 ( 0.8677146600783226527, 0.8690476190476190688, 0.8750000000000000000, 0.8809523809523809312, 0.8822853399216774584 ),
 .UNSPECIFIED. ) 
 CURVE ( )  GEOMETRIC_REPRESENTATION_ITEM ( )  RATIONAL_B_SPLINE_CURVE ( ( 0.9881565478350733400, 0.9923695281211490915, 1.000000000000000000, 0.9659258262890683122, 1.000000000000000000, 0.9659258262890683122, 1.000000000000000000, 0.9923695281211484254, 0.9881565478350726739 ) ) 
 REPRESENTATION_ITEM ( '' )  );
#7613 = DIRECTION ( 'NONE',  ( -0.000000000000000000, -0.000000000000000000, -1.000000000000000000 ) ) ;
#7614 = CIRCLE ( 'NONE', #63474, 15.00000000000000000 ) ;
#7615 = CARTESIAN_POINT ( 'NONE',  ( 5.076628168052704559, 5.175597817667451750, -8.527530157486179263 ) ) ;
#7616 = EDGE_CURVE ( 'NONE', #45856, #9878, #63951, .T. ) ;
#7617 = ORIENTED_EDGE ( 'NONE', *, *, #48609, .T. ) ;
#7618 = ORIENTED_EDGE ( 'NONE', *, *, #70921, .F. ) ;
#7619 = CARTESIAN_POINT ( 'NONE',  ( 4.559911319644449179, 23.89701867748817321, 9.422509992056141925 ) ) ;
#7620 = CARTESIAN_POINT ( 'NONE',  ( -4.164238869374099039, 21.80374883491396787, 8.674139862899312516E-16 ) ) ;
#7621 = CARTESIAN_POINT ( 'NONE',  ( 0.1532563361054100626, 45.80059781766745886, -2.638427012816831230 ) ) ;
#7622 = CARTESIAN_POINT ( 'NONE',  ( 10.00000000000000178, 64.31368534415483396, 10.88017736071110342 ) ) ;
#7624 = DIRECTION ( 'NONE',  ( 1.000000000000000000, -0.000000000000000000, -0.000000000000000000 ) ) ;
#7623 = CARTESIAN_POINT ( 'NONE',  ( 6.565887622018943937, 40.16530133659708923, 12.81628187352647430 ) ) ;
#7625 = CARTESIAN_POINT ( 'NONE',  ( 20.88017736071110519, 15.56368534415483751, 2.639326808657452039E-16 ) ) ;
#7626 = EDGE_CURVE ( 'NONE', #46052, #62525, #95039, .T. ) ;
#7627 = CARTESIAN_POINT ( 'NONE',  ( -14.09397099617986093, 0.04962897248923128779, -4.360881834954357217 ) ) ;
#7628 = CIRCLE ( 'NONE', #10821, 4.000000000000001776 ) ;
#7629 = CARTESIAN_POINT ( 'NONE',  ( -2.816281873526473856, 9.123634669930421381, 9.499525473075851096E-16 ) ) ;
#7630 = CARTESIAN_POINT ( 'NONE',  ( 5.076628168052703671, 21.84226448433411960, 8.527530157486179263 ) ) ;
#7631 = CARTESIAN_POINT ( 'NONE',  ( -9.422509992056136596, -16.51964798917849109, 5.440088680355559703 ) ) ;
#7632 = CARTESIAN_POINT ( 'NONE',  ( 3.591859063236761518, 34.95696800326375353, 11.09922568453594849 ) ) ;
#7633 = PRESENTATION_STYLE_ASSIGNMENT (( #53104 ) ) ;
#7635 = CARTESIAN_POINT ( 'NONE',  ( -4.096035146093626622, 4.358906096699807873E-16, 13.90943910019256258 ) ) ;
#7634 = CARTESIAN_POINT ( 'NONE',  ( 19.42250999205614193, 35.14701867748816966, 5.440088680355555262 ) ) ;
#7636 = CIRCLE ( 'NONE', #92271, 99.50000000000000000 ) ;
#7637 = CARTESIAN_POINT ( 'NONE',  ( 15.00000000000000000, 77.07179676972447169, 6.500000000000000888 ) ) ;
#7638 = CARTESIAN_POINT ( 'NONE',  ( 20.03932841506543383, 20.62161441960503083, -6.397827110478934820 ) ) ;
#7639 = TOROIDAL_SURFACE ( 'NONE', #92195, 8.250000000000000000, 0.2500000000000000000 ) ;
#7640 = CARTESIAN_POINT ( 'NONE',  ( 10.00000000000000000, 41.81368534415484106, -10.88017736071110342 ) ) ;
#7641 = CARTESIAN_POINT ( 'NONE',  ( 10.00000000000000178, 39.31368534415484106, 10.88017736071110342 ) ) ;
#7642 = CARTESIAN_POINT ( 'NONE',  ( 0.1532563361054100626, 60.80059781766744464, -2.638427012816831230 ) ) ;
#7643 = CARTESIAN_POINT ( 'NONE',  ( 2.035157376598822676, 67.43868534415484817, -7.964842623401177768 ) ) ;
#7644 = CARTESIAN_POINT ( 'NONE',  ( 7.361572987183169658, 49.96726448433410894, -9.846743663894592657 ) ) ;
#7646 = CARTESIAN_POINT ( 'NONE',  ( -13.34343830728408697, 0.5000000000000004441, 6.852200678592504701 ) ) ;
#7645 = CARTESIAN_POINT ( 'NONE',  ( -0.8801773607110991993, 12.85535201082150358, -2.915334737309923874 ) ) ;
#7647 = CARTESIAN_POINT ( 'NONE',  ( -1.099225684535947600, 14.54030133659708568, 6.408140936763237150 ) ) ;
#7648 = VERTEX_POINT ( 'NONE', #30225 ) ;
#7649 = CARTESIAN_POINT ( 'NONE',  ( -0.8801773607110991993, 32.85535201082151247, -2.915334737309923874 ) ) ;
#7650 = CARTESIAN_POINT ( 'NONE',  ( 3.591859063236761518, -0.04303199673624671928, 11.09922568453594849 ) ) ;
#7651 = CARTESIAN_POINT ( 'NONE',  ( 7.084665262690076126, 19.10535201082150181, 10.88017736071109987 ) ) ;
#7652 = CARTESIAN_POINT ( 'NONE',  ( 17.96484262340118221, 31.18868534415483751, -7.964842623401177768 ) ) ;
#7653 = CARTESIAN_POINT ( 'NONE',  ( 24.16423886937410614, 39.51208216824731068, -3.795296366450302550 ) ) ;
#7654 = CARTESIAN_POINT ( 'NONE',  ( 1.472469842513823179, 25.59226448433412315, -4.923371831947296329 ) ) ;
#7655 = CARTESIAN_POINT ( 'NONE',  ( 7.084665262690076126, 49.10535201082149825, 10.88017736071109987 ) ) ;
#7656 = DIRECTION ( 'NONE',  ( 1.000000000000000000, 0.000000000000000000, 0.000000000000000000 ) ) ;
#7657 = CARTESIAN_POINT ( 'NONE',  ( 6.204703633549690345, 0.7620821682473009062, -14.16423886937410259 ) ) ;
#7658 = EDGE_CURVE ( 'NONE', #22307, #3873, #96637, .T. ) ;
#7659 = FILL_AREA_STYLE ('',( #70116 ) ) ;
#7660 = CARTESIAN_POINT ( 'NONE',  ( 14.92337183194729988, 59.34226448433412315, -8.527530157486177487 ) ) ;
#7661 = ORIENTED_EDGE ( 'NONE', *, *, #98035, .F. ) ;
#7662 = ORIENTED_EDGE ( 'NONE', *, *, #55770, .T. ) ;
#7663 = CARTESIAN_POINT ( 'NONE',  ( 13.79529636645030344, 38.26208216824729647, 14.16423886937410614 ) ) ;
#7664 = CARTESIAN_POINT ( 'NONE',  ( 2.917880565312948704, 17.63708216824730357, 12.26659068614894643 ) ) ;
#7665 = CARTESIAN_POINT ( 'NONE',  ( 18.52753015748618282, 8.925597817667451750, -4.923371831947291888 ) ) ;
#7666 = CARTESIAN_POINT ( 'NONE',  ( 3.591859063236761518, 9.956968003263753531, 11.09922568453594849 ) ) ;
#7667 = CARTESIAN_POINT ( 'NONE',  ( 19.84674366389459621, 53.50893115100078745, 7.409399052514197653E-17 ) ) ;
#7668 = CARTESIAN_POINT ( 'NONE',  ( -8.897278993079112297, -15.56326597358625108, 4.000000000000000000 ) ) ;
#7670 = CARTESIAN_POINT ( 'NONE',  ( 22.81628187352647785, 16.41530133659708923, 3.434112377981063169 ) ) ;
#7669 = CARTESIAN_POINT ( 'NONE',  ( 19.42250999205614193, 40.14701867748817676, 5.440088680355555262 ) ) ;
#7671 = CARTESIAN_POINT ( 'NONE',  ( 13.79529636645031943, 20.34541550158063572, -14.16423886937409904 ) ) ;
#7672 = CARTESIAN_POINT ( 'NONE',  ( -0.8801773607111008646, 18.27201867748817321, 2.915334737309923430 ) ) ;
#7673 = CARTESIAN_POINT ( 'NONE',  ( 7.084665262690076126, 29.10535201082150181, 10.88017736071109987 ) ) ;
#7674 = CARTESIAN_POINT ( 'NONE',  ( 17.96484262340118221, 59.93868534415484106, 7.964842623401181321 ) ) ;
#7675 = CARTESIAN_POINT ( 'NONE',  ( -4.923371831947292776, -28.15773551566587685, 8.527530157486181039 ) ) ;
#7676 = ORIENTED_EDGE ( 'NONE', *, *, #49106, .T. ) ;
#7677 = CARTESIAN_POINT ( 'NONE',  ( 1.514341385896460501, -0.03417435944610275333, 15.92432625271834112 ) ) ;
#7678 = ORIENTED_EDGE ( 'NONE', *, *, #13044, .T. ) ;
#7679 = VERTEX_POINT ( 'NONE', #84247 ) ;
#7680 = DIRECTION ( 'NONE',  ( 0.9636304532086191754, 0.000000000000000000, 0.2672383760782702788 ) ) ;
#7682 = CARTESIAN_POINT ( 'NONE',  ( -2.266590686148945544, 62.22041550158063927, 7.082119434687048631 ) ) ;
#7681 = CARTESIAN_POINT ( 'NONE',  ( 17.08211943468705840, 55.13708216824731068, -12.26659068614894466 ) ) ;
#7684 = CARTESIAN_POINT ( 'NONE',  ( 7.361572987183170547, 62.05059781766745886, 9.846743663894590881 ) ) ;
#7683 = CARTESIAN_POINT ( 'NONE',  ( 14.92337183194729633, 17.67559781766745175, 8.527530157486181039 ) ) ;
#7685 = CARTESIAN_POINT ( 'NONE',  ( 2.035157376598822676, 67.43868534415484817, -7.964842623401177768 ) ) ;
#7686 = CARTESIAN_POINT ( 'NONE',  ( 0.1532563361054082862, 11.21726448433411605, 2.638427012816831674 ) ) ;
#7687 = CARTESIAN_POINT ( 'NONE',  ( -9.382169495545422677, 18.49863466993041428, -9.382169495545417348 ) ) ;
#7688 = ORIENTED_EDGE ( 'NONE', *, *, #14714, .F. ) ;
#7689 = ADVANCED_FACE ( 'NONE', ( #59744 ), #68742, .F. ) ;
#7690 = CARTESIAN_POINT ( 'NONE',  ( -4.164238869374099927, 32.01208216824730357, 3.795296366450308767 ) ) ;
#7691 = CARTESIAN_POINT ( 'NONE',  ( 20.36894250292379382, 48.67874883491396076, 10.36894250292379205 ) ) ;
#7692 = ORIENTED_EDGE ( 'NONE', *, *, #82620, .F. ) ;
#7693 = CARTESIAN_POINT ( 'NONE',  ( 3.591859063236761518, 54.95696800326376064, 11.09922568453594849 ) ) ;
#7694 = CIRCLE ( 'NONE', #63545, 14.49999999999999822 ) ;
#7695 = CARTESIAN_POINT ( 'NONE',  ( 15.44008868035555260, 24.73035201082150891, 9.422509992056143702 ) ) ;
#7696 = CARTESIAN_POINT ( 'NONE',  ( 19.84674366389459621, 43.50893115100078745, 7.409399052514197653E-17 ) ) ;
#7697 = CARTESIAN_POINT ( 'NONE',  ( 19.42250999205614193, 20.14701867748817321, 5.440088680355555262 ) ) ;
#7698 = CARTESIAN_POINT ( 'NONE',  ( 12.98685442714194949, 4.417933709739653524E-16, 6.449155920601044478 ) ) ;
#7699 = CARTESIAN_POINT ( 'NONE',  ( 1.472469842513823179, 60.59226448433412315, -4.923371831947296329 ) ) ;
#7700 = CARTESIAN_POINT ( 'NONE',  ( 18.52753015748618282, 53.92559781766745175, -4.923371831947291888 ) ) ;
#7701 = AXIS2_PLACEMENT_3D ( 'NONE', #90716, #52718, #30206 ) ;
#7702 = EDGE_CURVE ( 'NONE', #42198, #39274, #22192, .T. ) ;
#7703 = CIRCLE ( 'NONE', #63554, 0.2499999999999980294 ) ;
#7704 = CARTESIAN_POINT ( 'NONE',  ( 19.50000000000000355, 98.59912998021083297, -5.000000000000000000 ) ) ;
#7705 = CARTESIAN_POINT ( 'NONE',  ( -14.82269085861169344, 0.3639308522293647763, -2.299529454047150701 ) ) ;
#7706 =( NAMED_UNIT ( * ) SI_UNIT ( $, .STERADIAN. ) SOLID_ANGLE_UNIT ( ) );
#7707 = ORIENTED_EDGE ( 'NONE', *, *, #44953, .F. ) ;
#7708 = CARTESIAN_POINT ( 'NONE',  ( 0.9408516040111539747, 7.466938638839759612, -6.499999999999972466 ) ) ;
#7709 = CARTESIAN_POINT ( 'NONE',  ( 5.076628168052704559, 35.17559781766745175, -8.527530157486179263 ) ) ;
#7710 = EDGE_CURVE ( 'NONE', #62689, #39764, #83849, .T. ) ;
#7711 = CARTESIAN_POINT ( 'NONE',  ( 6.715867195167361636, 15.00000000000000000, 12.85095824508331930 ) ) ;
#7712 = CARTESIAN_POINT ( 'NONE',  ( 22.81628187352647785, 31.41530133659709279, 3.434112377981063169 ) ) ;
#7713 = CARTESIAN_POINT ( 'NONE',  ( 1.274849032794231007, 38.57228050351032067, 6.499999999999895195 ) ) ;
#7714 = CARTESIAN_POINT ( 'NONE',  ( 11.10175276307590586, 0.04962894967561130161, 9.716398248524756198 ) ) ;
#7715 = ORIENTED_EDGE ( 'NONE', *, *, #83458, .T. ) ;
#7716 = CARTESIAN_POINT ( 'NONE',  ( 6.715867195167446901, 15.00000000000000000, -12.85095824508324469 ) ) ;
#7717 = CARTESIAN_POINT ( 'NONE',  ( 12.63842701281683922, 39.55059781766744464, -9.846743663894590881 ) ) ;
#7718 = CARTESIAN_POINT ( 'NONE',  ( 2.917880565312950480, 30.97041550158063572, -12.26659068614894821 ) ) ;
#7719 = CARTESIAN_POINT ( 'NONE',  ( 18.52753015748618282, 58.92559781766745886, -4.923371831947291888 ) ) ;
#7720 = DIRECTION ( 'NONE',  ( 1.000000000000000000, 3.167963975439022915E-12, 0.000000000000000000 ) ) ;
#7721 = CARTESIAN_POINT ( 'NONE',  ( 10.00000000000000178, 69.31368534415484817, 10.88017736071110342 ) ) ;
#7722 = CARTESIAN_POINT ( 'NONE',  ( 10.00000000000000000, 0.5537488349139675359, -14.16423886937410082 ) ) ;
#7723 = CARTESIAN_POINT ( 'NONE',  ( 17.20831665107776587, 47.88393115100078745, 7.208316651077764980 ) ) ;
#7724 = CARTESIAN_POINT ( 'NONE',  ( 10.00000000000000000, 56.81368534415484106, -10.88017736071110342 ) ) ;
#7725 = CARTESIAN_POINT ( 'NONE',  ( 5.076628168052703671, 46.84226448433412315, 8.527530157486179263 ) ) ;
#7726 = PLANE ( 'NONE',  #1262 ) ;
#7727 = EDGE_CURVE ( 'NONE', #89266, #28441, #6754, .T. ) ;
#7728 = CARTESIAN_POINT ( 'NONE',  ( 12.91533473730992121, 49.52201867748817676, 10.88017736071110164 ) ) ;
#7729 = ORIENTED_EDGE ( 'NONE', *, *, #11977, .T. ) ;
#7730 = CARTESIAN_POINT ( 'NONE',  ( 0.8719017118913385822, 123.9374316453451144, -4.500000000000000888 ) ) ;
#7731 = CARTESIAN_POINT ( 'NONE',  ( 20.88017736071110519, 25.56368534415483751, 2.639326808657452039E-16 ) ) ;
#7733 = CARTESIAN_POINT ( 'NONE',  ( -0.8801773607110991993, 57.85535201082149825, -2.915334737309923874 ) ) ;
#7732 = CARTESIAN_POINT ( 'NONE',  ( -1.099225684535947600, 4.540301336597087456, 6.408140936763237150 ) ) ;
#7734 = DIRECTION ( 'NONE',  ( 0.000000000000000000, 0.000000000000000000, -1.000000000000000000 ) ) ;
#7735 = EDGE_CURVE ( 'NONE', #35951, #20172, #91847, .T. ) ;
#7736 = CARTESIAN_POINT ( 'NONE',  ( 2.035157376598824452, 68.68868534415484817, 7.964842623401179544 ) ) ;
#7737 = CARTESIAN_POINT ( 'NONE',  ( -46.48928645636213730, 103.2957187381727238, -6.397878122524045530 ) ) ;
#7738 = CARTESIAN_POINT ( 'NONE',  ( 0.5774900079438590739, 42.64701867748816966, -5.440088680355550821 ) ) ;
#7739 = CARTESIAN_POINT ( 'NONE',  ( 10.00000000000000000, 14.75893115100078568, -9.846743663894594434 ) ) ;
#7740 = AXIS2_PLACEMENT_3D ( 'NONE', #9337, #56798, #55830 ) ;
#7741 = CARTESIAN_POINT ( 'NONE',  ( 18.52753015748618282, 33.92559781766745886, -4.923371831947291888 ) ) ;
#7742 = CYLINDRICAL_SURFACE ( 'NONE', #77668, 0.2500000000000002220 ) ;
#7743 = CARTESIAN_POINT ( 'NONE',  ( 7.082119434687047743, 25.13708216824731068, -12.26659068614894821 ) ) ;
#7744 = CARTESIAN_POINT ( 'NONE',  ( 1.472469842513823179, 61.42559781766745175, 4.923371831947296329 ) ) ;
#7745 = CARTESIAN_POINT ( 'NONE',  ( 24.16423886937410614, 64.51208216824728936, -3.795296366450302550 ) ) ;
#7746 = CARTESIAN_POINT ( 'NONE',  ( 3.420591144908569081, 14.63606885998601825, -14.60477854057959490 ) ) ;
#7747 = CARTESIAN_POINT ( 'NONE',  ( -2.266590686148945544, 26.38708216824730357, -7.082119434687050408 ) ) ;
#7748 = CARTESIAN_POINT ( 'NONE',  ( 17.08211943468705840, 55.13708216824731068, -12.26659068614894466 ) ) ;
#7749 = TOROIDAL_SURFACE ( 'NONE', #44410, 2.899999999999999911, 0.1000000000000000056 ) ;
#7750 = CARTESIAN_POINT ( 'NONE',  ( 12.63842701281683922, 19.55059781766745175, -9.846743663894590881 ) ) ;
#7751 = CARTESIAN_POINT ( 'NONE',  ( -0.8801773607110991993, 2.855352010821504471, -2.915334737309923874 ) ) ;
#7752 = VERTEX_POINT ( 'NONE', #85711 ) ;
#7753 = CARTESIAN_POINT ( 'NONE',  ( 17.20831665107776587, 27.88393115100078390, 7.208316651077764980 ) ) ;
#7754 = CARTESIAN_POINT ( 'NONE',  ( 7.084665262690076126, 22.02201867748817321, -10.88017736071110164 ) ) ;
#7755 = CARTESIAN_POINT ( 'NONE',  ( 7.361572987183169658, 49.96726448433410894, -9.846743663894592657 ) ) ;
#7757 = SURFACE_SIDE_STYLE ('',( #54210 ) ) ;
#7756 = CARTESIAN_POINT ( 'NONE',  ( 13.79529636645030344, 8.262082168247300018, 14.16423886937410614 ) ) ;
#7758 = DIRECTION ( 'NONE',  ( 0.000000000000000000, 0.000000000000000000, -1.000000000000000000 ) ) ;
#7759 = CARTESIAN_POINT ( 'NONE',  ( 5.076628168052704559, 5.175597817667451750, -8.527530157486179263 ) ) ;
#7760 = CARTESIAN_POINT ( 'NONE',  ( 16.40814093676324603, 37.45696800326376064, -11.09922568453594671 ) ) ;
#7761 = CARTESIAN_POINT ( 'NONE',  ( 12.63842701281683922, 44.55059781766745175, -9.846743663894590881 ) ) ;
#7762 = EDGE_LOOP ( 'NONE', ( #4949, #82036, #54167, #23373, #61872, #75045 ) ) ;
#7763 = CARTESIAN_POINT ( 'NONE',  ( 17.20831665107776587, 27.88393115100078390, 7.208316651077764980 ) ) ;
#7764 = DIRECTION ( 'NONE',  ( 0.000000000000000000, 0.000000000000000000, 1.000000000000000000 ) ) ;
#7765 = CARTESIAN_POINT ( 'NONE',  ( -0.3689425029237898834, 56.17874883491396076, -10.36894250292378850 ) ) ;
#7766 = CARTESIAN_POINT ( 'NONE',  ( 17.96484262340118221, 51.18868534415483396, -7.964842623401177768 ) ) ;
#7767 = DIRECTION ( 'NONE',  ( -0.000000000000000000, -1.000000000000000000, -0.000000000000000000 ) ) ;
#7768 = DIRECTION ( 'NONE',  ( 1.000000000000000000, 0.000000000000000000, -0.000000000000000000 ) ) ;
#7769 = CARTESIAN_POINT ( 'NONE',  ( 0.1532563361054083140, 36.00893115100078745, 1.131784320476157264E-15 ) ) ;
#7770 = CARTESIAN_POINT ( 'NONE',  ( 2.035157376598822676, 7.438685344154837509, -7.964842623401177768 ) ) ;
#7771 = CARTESIAN_POINT ( 'NONE',  ( 7.361572987183170547, 37.05059781766744464, 9.846743663894590881 ) ) ;
#7772 = FACE_OUTER_BOUND ( 'NONE', #60279, .T. ) ;
#7773 = CARTESIAN_POINT ( 'NONE',  ( 5.076628168052703671, 51.84226448433412315, 8.527530157486179263 ) ) ;
#7774 = CARTESIAN_POINT ( 'NONE',  ( 20.88017736071110164, 45.35535201082149115, 2.915334737309930979 ) ) ;
#7775 = AXIS2_PLACEMENT_3D ( 'NONE', #8913, #91926, #60436 ) ;
#7776 = VERTEX_POINT ( 'NONE', #55194 ) ;
#7777 = ORIENTED_EDGE ( 'NONE', *, *, #25585, .F. ) ;
#7778 = CARTESIAN_POINT ( 'NONE',  ( 13.43411237798105340, 60.58196800326376064, 12.81628187352647963 ) ) ;
#7779 = DIRECTION ( 'NONE',  ( 0.000000000000000000, -0.000000000000000000, -1.000000000000000000 ) ) ;
#7780 = CARTESIAN_POINT ( 'NONE',  ( 18.52753015748618282, 13.92559781766745175, -4.923371831947291888 ) ) ;
#7781 = CARTESIAN_POINT ( 'NONE',  ( 13.43411237798105340, 55.58196800326374643, 12.81628187352647963 ) ) ;
#7783 = CARTESIAN_POINT ( 'NONE',  ( 19.84674366389459266, 53.71726448433411605, -2.638427012816827677 ) ) ;
#7782 = CARTESIAN_POINT ( 'NONE',  ( 2.035157376598824452, 8.688685344154839285, 7.964842623401179544 ) ) ;
#7784 = LINE ( 'NONE', #22293, #83731 ) ;
#7785 = CARTESIAN_POINT ( 'NONE',  ( 6.204703633549690345, 25.76208216824730712, -14.16423886937410259 ) ) ;
#7786 = CARTESIAN_POINT ( 'NONE',  ( 17.08211943468705130, 58.47041550158063927, 12.26659068614894998 ) ) ;
#7787 = CARTESIAN_POINT ( 'NONE',  ( 1.472469842513823179, 61.42559781766745175, 4.923371831947296329 ) ) ;
#7788 = CARTESIAN_POINT ( 'NONE',  ( -6.000000000000000000, 78.07179676972447169, 4.000000000000000000 ) ) ;
#7789 = CARTESIAN_POINT ( 'NONE',  ( 12.91533473730992121, 54.52201867748816255, 10.88017736071110164 ) ) ;
#7790 = CARTESIAN_POINT ( 'NONE',  ( 10.00000000000000178, 69.31368534415484817, 10.88017736071110342 ) ) ;
#7791 = ORIENTED_EDGE ( 'NONE', *, *, #81606, .F. ) ;
#7792 = CARTESIAN_POINT ( 'NONE',  ( 13.43411237798106583, 52.66530133659708213, -12.81628187352647252 ) ) ;
#7793 = ORIENTED_EDGE ( 'NONE', *, *, #4245, .T. ) ;
#7794 = CARTESIAN_POINT ( 'NONE',  ( 18.52753015748618282, 3.925597817667451306, -4.923371831947291888 ) ) ;
#7795 = ORIENTED_EDGE ( 'NONE', *, *, #76361, .T. ) ;
#7796 = CARTESIAN_POINT ( 'NONE',  ( -2.266590686148945544, 16.38708216824730357, -7.082119434687050408 ) ) ;
#7797 = CARTESIAN_POINT ( 'NONE',  ( 0.1532563361054100626, 20.80059781766744464, -2.638427012816831230 ) ) ;
#7798 = CARTESIAN_POINT ( 'NONE',  ( 7.084665262690076126, 27.02201867748817676, -10.88017736071110164 ) ) ;
#7799 = DIRECTION ( 'NONE',  ( 0.6246950475544238435, 0.7808688094430307203, 0.000000000000000000 ) ) ;
#7800 = ORIENTED_EDGE ( 'NONE', *, *, #76887, .T. ) ;
#7801 = CARTESIAN_POINT ( 'NONE',  ( 12.91533473730992121, 29.52201867748817321, 10.88017736071110164 ) ) ;
#7802 = ORIENTED_EDGE ( 'NONE', *, *, #67208, .T. ) ;
#7803 = CARTESIAN_POINT ( 'NONE',  ( 15.44008868035555260, 39.73035201082150536, 9.422509992056143702 ) ) ;
#7804 = CARTESIAN_POINT ( 'NONE',  ( -5.803070148808147088, 3.900978891399319278E-16, -13.28812917035395813 ) ) ;
#7805 = EDGE_LOOP ( 'NONE', ( #30049, #60359, #7502, #60391 ) ) ;
#7806 = ORIENTED_EDGE ( 'NONE', *, *, #30838, .F. ) ;
#7807 = CARTESIAN_POINT ( 'NONE',  ( 13.43411237798105340, 20.58196800326374643, 12.81628187352647963 ) ) ;
#7808 =( NAMED_UNIT ( * ) SI_UNIT ( $, .STERADIAN. ) SOLID_ANGLE_UNIT ( ) );
#7809 =( BOUNDED_SURFACE ( )  B_SPLINE_SURFACE ( 3, 2, ( 
 ( #35201, #49714, #57221 ),
 ( #58194, #56262, #65208 ),
 ( #42241, #80224, #26726 ),
 ( #56737, #50210, #42725 ) ),
 .UNSPECIFIED., .F., .F., .F. ) 
 B_SPLINE_SURFACE_WITH_KNOTS ( ( 4, 4 ),
 ( 3, 3 ),
 ( 2.168404344971008868E-19, 0.0006068291151710755033 ),
 ( 0.000000000000000000, 1.000000000000000000 ),
 .UNSPECIFIED. ) 
 GEOMETRIC_REPRESENTATION_ITEM ( )  RATIONAL_B_SPLINE_SURFACE ( (
 ( 1.000000000000000000, 0.8188293140827536121, 1.000000000000000000),
 ( 1.000000000000000000, 0.8260591074388915489, 1.000000000000000000),
 ( 1.000000000000000000, 0.8336435218269933056, 1.000000000000000000),
 ( 1.000000000000000000, 0.8414823709351006986, 1.000000000000000000) ) ) 
 REPRESENTATION_ITEM ( '' )  SURFACE ( )  );
#7810 = CARTESIAN_POINT ( 'NONE',  ( 5.076628168052704559, 10.17559781766745175, -8.527530157486179263 ) ) ;
#7811 = PRESENTATION_STYLE_ASSIGNMENT (( #75797 ) ) ;
#7812 = EDGE_CURVE ( 'NONE', #25175, #10365, #82848, .T. ) ;
#7813 = FILL_AREA_STYLE_COLOUR ( '', #38330 ) ;
#7814 = CARTESIAN_POINT ( 'NONE',  ( 14.92337183194729988, 19.34226448433411960, -8.527530157486177487 ) ) ;
#7815 = CARTESIAN_POINT ( 'NONE',  ( 20.88017736071110875, 35.77201867748816966, -2.915334737309920765 ) ) ;
#7816 = ADVANCED_FACE ( 'NONE', ( #71688 ), #92707, .F. ) ;
#7817 = ORIENTED_EDGE ( 'NONE', *, *, #620, .F. ) ;
#7818 = DIRECTION ( 'NONE',  ( -0.000000000000000000, 0.000000000000000000, 1.000000000000000000 ) ) ;
#7819 = CARTESIAN_POINT ( 'NONE',  ( 19.42250999205614548, 50.98035201082151247, -5.440088680355545492 ) ) ;
#7820 = DIRECTION ( 'NONE',  ( 0.000000000000000000, 0.000000000000000000, 1.000000000000000000 ) ) ;
#7821 = CARTESIAN_POINT ( 'NONE',  ( -2.816281873526473856, 59.33196800326374643, 3.434112377981055619 ) ) ;
#7822 = CARTESIAN_POINT ( 'NONE',  ( 17.96484262340118221, 56.18868534415484817, -7.964842623401177768 ) ) ;
#7823 = EDGE_CURVE ( 'NONE', #88606, #11086, #5631, .T. ) ;
#7824 = CARTESIAN_POINT ( 'NONE',  ( 19.38216949554541557, 2.248634669930420049, -9.382169495545420901 ) ) ;
#7825 = DIRECTION ( 'NONE',  ( -0.000000000000000000, -1.000000000000000000, -0.000000000000000000 ) ) ;
#7826 = CARTESIAN_POINT ( 'NONE',  ( 7.361572987183170547, 37.05059781766744464, 9.846743663894590881 ) ) ;
#7827 = CARTESIAN_POINT ( 'NONE',  ( -1.099225684535947600, 53.70696800326376064, -6.408140936763238038 ) ) ;
#7828 = CARTESIAN_POINT ( 'NONE',  ( 20.15039907845753220, 37.62777174578614847, -6.262539305110077947 ) ) ;
#7829 = CARTESIAN_POINT ( 'NONE',  ( 19.84674366389459266, 3.300597817667451750, 2.638427012816836559 ) ) ;
#7830 = CARTESIAN_POINT ( 'NONE',  ( 3.591859063236763294, 18.29030133659708568, -11.09922568453595026 ) ) ;
#7832 = DIRECTION ( 'NONE',  ( 0.000000000000000000, 1.000000000000000000, 0.000000000000000000 ) ) ;
#7831 = CYLINDRICAL_SURFACE ( 'NONE', #10129, 0.2500000000000002220 ) ;
#7833 = CARTESIAN_POINT ( 'NONE',  ( 10.00000000000000000, 31.81368534415483751, -10.88017736071110342 ) ) ;
#7834 = CARTESIAN_POINT ( 'NONE',  ( 14.92337183194729633, 57.67559781766745886, 8.527530157486181039 ) ) ;
#7835 = CARTESIAN_POINT ( 'NONE',  ( 0.000000000000000000, 0.5000000000000004441, 0.000000000000000000 ) ) ;
#7836 = CARTESIAN_POINT ( 'NONE',  ( 5.076628168052703671, 6.842264484334118713, 8.527530157486179263 ) ) ;
#7837 = CARTESIAN_POINT ( 'NONE',  ( 2.035157376598824452, 18.68868534415484106, 7.964842623401179544 ) ) ;
#7838 = CARTESIAN_POINT ( 'NONE',  ( 0.6178305044545838731, 14.74863466993041783, 9.382169495545420901 ) ) ;
#7839 = STYLED_ITEM ( 'NONE', ( #31868 ), #71516 ) ;
#7840 =( NAMED_UNIT ( * ) SI_UNIT ( $, .STERADIAN. ) SOLID_ANGLE_UNIT ( ) );
#7841 = CARTESIAN_POINT ( 'NONE',  ( -0.7375392941516176748, 0.5000000000000004441, -14.98185688723471820 ) ) ;
#7842 = CARTESIAN_POINT ( 'NONE',  ( 4.130000000000000782, 1.019547802438464545, -2.500000000000000000 ) ) ;
#7843 = CARTESIAN_POINT ( 'NONE',  ( 20.88017736071110519, 10.56368534415483929, 2.639326808657452039E-16 ) ) ;
#7844 = CARTESIAN_POINT ( 'NONE',  ( 12.63842701281683922, 44.55059781766745175, -9.846743663894590881 ) ) ;
#7845 = DIRECTION ( 'NONE',  ( 0.000000000000000000, 0.000000000000000000, 1.000000000000000000 ) ) ;
#7846 = CARTESIAN_POINT ( 'NONE',  ( 15.44008868035555260, 4.730352010821505360, 9.422509992056143702 ) ) ;
#7847 = EDGE_CURVE ( 'NONE', #35983, #13186, #18198, .T. ) ;
#7848 = CARTESIAN_POINT ( 'NONE',  ( 7.084665262690076126, 34.10535201082151247, 10.88017736071109987 ) ) ;
#7850 = DIRECTION ( 'NONE',  ( 1.000000000000000000, 0.000000000000000000, 0.000000000000000000 ) ) ;
#7849 = CARTESIAN_POINT ( 'NONE',  ( 13.79529636645030344, 63.26208216824730357, 14.16423886937410614 ) ) ;
#7851 = CARTESIAN_POINT ( 'NONE',  ( 5.076628168052703671, 21.84226448433411960, 8.527530157486179263 ) ) ;
#7852 = CARTESIAN_POINT ( 'NONE',  ( 13.43411237798105340, 10.58196800326375353, 12.81628187352647963 ) ) ;
#7853 = DIRECTION ( 'NONE',  ( -0.000000000000000000, -0.000000000000000000, -1.000000000000000000 ) ) ;
#7854 = CARTESIAN_POINT ( 'NONE',  ( -3.750000000000000000, 78.07179676972445748, 4.000000000000000000 ) ) ;
#7855 = CARTESIAN_POINT ( 'NONE',  ( 17.20831665107776587, 64.13393115100079456, -7.208316651077762316 ) ) ;
#7856 = CIRCLE ( 'NONE', #25421, 15.00000000000000000 ) ;
#7857 = CARTESIAN_POINT ( 'NONE',  ( 2.241241388159942801E-47, 3.851859888774471706E-31, 7.000000000000000000 ) ) ;
#7858 = EDGE_CURVE ( 'NONE', #16435, #9403, #52194, .T. ) ;
#7859 = CARTESIAN_POINT ( 'NONE',  ( -8.330963134902997780, -7.272696214962663497, -4.000000000000000000 ) ) ;
#7860 = CARTESIAN_POINT ( 'NONE',  ( -2.266590686148945544, 16.38708216824730357, -7.082119434687050408 ) ) ;
#7861 = CARTESIAN_POINT ( 'NONE',  ( 0.1532563361054083140, 21.00893115100078745, 1.131784320476157264E-15 ) ) ;
#7862 = LINE ( 'NONE', #44848, #80011 ) ;
#7863 = ORIENTED_EDGE ( 'NONE', *, *, #77918, .F. ) ;
#7864 = CARTESIAN_POINT ( 'NONE',  ( 22.26659068614895176, 49.72041550158063927, -7.082119434687042414 ) ) ;
#7865 = CARTESIAN_POINT ( 'NONE',  ( 17.20831665107776587, 7.883931151000784787, 7.208316651077764980 ) ) ;
#7867 = CARTESIAN_POINT ( 'NONE',  ( -13.34343830728398927, 14.49999999999999112, -6.852200678592835104 ) ) ;
#7866 = FACE_OUTER_BOUND ( 'NONE', #93030, .T. ) ;
#7868 = CARTESIAN_POINT ( 'NONE',  ( 7.084665262690076126, 39.10535201082150536, 10.88017736071109987 ) ) ;
#7869 = CARTESIAN_POINT ( 'NONE',  ( 21.09922568453594849, 46.20696800326376064, 6.408140936763242479 ) ) ;
#7870 = CARTESIAN_POINT ( 'NONE',  ( -0.8801773607111008646, 13.27201867748817143, 2.915334737309923430 ) ) ;
#7871 = CARTESIAN_POINT ( 'NONE',  ( 6.565887622018943937, 45.16530133659708923, 12.81628187352647430 ) ) ;
#7872 = CARTESIAN_POINT ( 'NONE',  ( 2.791683348922237240, 65.38393115100078035, -7.208316651077763204 ) ) ;
#7873 = CARTESIAN_POINT ( 'NONE',  ( 0.1532563361054082862, 1.217264484334117824, 2.638427012816831674 ) ) ;
#7874 = ORIENTED_EDGE ( 'NONE', *, *, #63870, .F. ) ;
#7875 = DIRECTION ( 'NONE',  ( -0.000000000000000000, -0.000000000000000000, -1.000000000000000000 ) ) ;
#7876 = CARTESIAN_POINT ( 'NONE',  ( -7.909660991676054742, -4.175919252839798368, -4.000000000000000000 ) ) ;
#7877 = CARTESIAN_POINT ( 'NONE',  ( 24.16423886937410614, 44.51208216824730357, -3.795296366450302550 ) ) ;
#7878 = CARTESIAN_POINT ( 'NONE',  ( -2.266590686148945544, 11.38708216824730179, -7.082119434687050408 ) ) ;
#7879 = CARTESIAN_POINT ( 'NONE',  ( 0.5774900079438590739, 7.647018677488171434, -5.440088680355550821 ) ) ;
#7880 = CARTESIAN_POINT ( 'NONE',  ( 0.5774900079438607392, 38.48035201082150536, 5.440088680355550821 ) ) ;
#7881 = LINE ( 'NONE', #75872, #90972 ) ;
#7882 = CIRCLE ( 'NONE', #63734, 19.99999999999999289 ) ;
#7883 = CARTESIAN_POINT ( 'NONE',  ( 14.73551000134585820, 0.04962893459885754643, -0.7225335126797688412 ) ) ;
#7884 = CARTESIAN_POINT ( 'NONE',  ( -0.8801773607111008646, 63.27201867748817676, 2.915334737309923430 ) ) ;
#7885 = DIRECTION ( 'NONE',  ( 0.2334453638559024768, 0.000000000000000000, 0.9723699203976772232 ) ) ;
#7886 = CARTESIAN_POINT ( 'NONE',  ( 16.40814093676323893, 30.79030133659708923, 11.09922568453595026 ) ) ;
#7887 = PLANE ( 'NONE',  #68258 ) ;
#7888 = CARTESIAN_POINT ( 'NONE',  ( -3.195792623639463592, 3.703790035174482131, 11.92686044187660421 ) ) ;
#7889 = CARTESIAN_POINT ( 'NONE',  ( 19.84674366389459266, 38.71726448433412315, -2.638427012816827677 ) ) ;
#7890 = CARTESIAN_POINT ( 'NONE',  ( 10.00000000000000000, 16.81368534415483751, -10.88017736071110342 ) ) ;
#7891 = CARTESIAN_POINT ( 'NONE',  ( -1.099225684535947600, 14.54030133659708568, 6.408140936763237150 ) ) ;
#7892 = CARTESIAN_POINT ( 'NONE',  ( 10.00000000000000000, 4.758931151000784787, -9.846743663894594434 ) ) ;
#7893 = CARTESIAN_POINT ( 'NONE',  ( -0.8801773607110991993, 12.85535201082150358, -2.915334737309923874 ) ) ;
#7894 = CARTESIAN_POINT ( 'NONE',  ( 7.361572987183169658, 34.96726448433411605, -9.846743663894592657 ) ) ;
#7895 = CARTESIAN_POINT ( 'NONE',  ( 16.40814093676324603, 62.45696800326376064, -11.09922568453594671 ) ) ;
#7896 = CARTESIAN_POINT ( 'NONE',  ( 19.84674366389459621, 23.50893115100078390, 7.409399052514197653E-17 ) ) ;
#7897 = CARTESIAN_POINT ( 'NONE',  ( 13.79529636645030344, 8.262082168247300018, 14.16423886937410614 ) ) ;
#7898 = CARTESIAN_POINT ( 'NONE',  ( 5.806645064956531321, 15.00000000000000888, -13.42464971016994113 ) ) ;
#7899 = CARTESIAN_POINT ( 'NONE',  ( 0.5774900079438607392, 28.48035201082150891, 5.440088680355550821 ) ) ;
#7901 = CARTESIAN_POINT ( 'NONE',  ( 24.16423886937410614, 39.51208216824731068, -3.795296366450302550 ) ) ;
#7900 = CARTESIAN_POINT ( 'NONE',  ( 19.42250999205614548, 5.980352010821504471, -5.440088680355545492 ) ) ;
#7902 = CARTESIAN_POINT ( 'NONE',  ( 4.559911319644449179, 33.89701867748817676, 9.422509992056141925 ) ) ;
#7903 = ADVANCED_FACE ( 'NONE', ( #10696 ), #45523, .F. ) ;
#7904 = CARTESIAN_POINT ( 'NONE',  ( 20.88017736071110875, 10.77201867748817143, -2.915334737309920765 ) ) ;
#7905 = ORIENTED_EDGE ( 'NONE', *, *, #68674, .T. ) ;
#7906 = CARTESIAN_POINT ( 'NONE',  ( 20.88017736071110875, 45.77201867748816966, -2.915334737309920765 ) ) ;
#7907 = EDGE_CURVE ( 'NONE', #13653, #26237, #78196, .T. ) ;
#7908 = CARTESIAN_POINT ( 'NONE',  ( 0.6178305044545818747, 53.49863466993041072, -9.382169495545419124 ) ) ;
#7909 = CARTESIAN_POINT ( 'NONE',  ( 12.91533473730993009, 46.60535201082150536, -10.88017736071109987 ) ) ;
#7910 = CARTESIAN_POINT ( 'NONE',  ( 19.42250999205614548, 55.98035201082150536, -5.440088680355545492 ) ) ;
#7911 = ORIENTED_EDGE ( 'NONE', *, *, #31695, .T. ) ;
#7912 = CARTESIAN_POINT ( 'NONE',  ( 19.42250999205614193, 50.14701867748817676, 5.440088680355555262 ) ) ;
#7913 = DIRECTION ( 'NONE',  ( -0.9588197348681908316, 0.000000000000000000, -0.2840153447039300283 ) ) ;
#7914 = CARTESIAN_POINT ( 'NONE',  ( -0.1503990784575260087, 24.24884699246888786, -6.262539305110081500 ) ) ;
#7915 = CARTESIAN_POINT ( 'NONE',  ( 17.08211943468705840, 50.13708216824730357, -12.26659068614894466 ) ) ;
#7916 = CARTESIAN_POINT ( 'NONE',  ( 0.1532563361054082862, 1.217264484334117824, 2.638427012816831674 ) ) ;
#7917 = CARTESIAN_POINT ( 'NONE',  ( -13.95697193428315330, 15.00000000000000711, 4.371663894958725649 ) ) ;
#7918 = CARTESIAN_POINT ( 'NONE',  ( -7.366188783701793419, -80.69039970148938323, -4.000000000000000000 ) ) ;
#7919 = CARTESIAN_POINT ( 'NONE',  ( 12.63842701281683922, 59.55059781766744464, -9.846743663894590881 ) ) ;
#7920 =( LENGTH_UNIT ( ) NAMED_UNIT ( * ) SI_UNIT ( .MILLI., .METRE. ) );
#7921 = CARTESIAN_POINT ( 'NONE',  ( 19.84674366389459266, 33.71726448433410894, -2.638427012816827677 ) ) ;
#7922 = ORIENTED_EDGE ( 'NONE', *, *, #2450, .T. ) ;
#7923 = CARTESIAN_POINT ( 'NONE',  ( 2.791683348922237240, 35.38393115100079456, -7.208316651077763204 ) ) ;
#7924 = CARTESIAN_POINT ( 'NONE',  ( -12.81628187352647252, -10.66803199673624825, 3.434112377981066722 ) ) ;
#7925 = CARTESIAN_POINT ( 'NONE',  ( -0.8801773607111009756, 43.06368534415484106, 1.068504757029289695E-15 ) ) ;
#7926 = CARTESIAN_POINT ( 'NONE',  ( 2.791683348922240793, 31.63393115100078745, 7.208316651077764092 ) ) ;
#7927 = CARTESIAN_POINT ( 'NONE',  ( 3.591859063236761518, 24.95696800326375353, 11.09922568453594849 ) ) ;
#7929 = CARTESIAN_POINT ( 'NONE',  ( 19.42250999205614193, 55.14701867748817676, 5.440088680355555262 ) ) ;
#7928 = CARTESIAN_POINT ( 'NONE',  ( 10.00000000000000178, 70.00000000000000000, 0.000000000000000000 ) ) ;
#7931 =( LENGTH_UNIT ( ) NAMED_UNIT ( * ) SI_UNIT ( .MILLI., .METRE. ) );
#7930 = CARTESIAN_POINT ( 'NONE',  ( 17.96484262340118221, 44.93868534415483396, 7.964842623401181321 ) ) ;
#7932 = CARTESIAN_POINT ( 'NONE',  ( 20.36894250292379382, 58.67874883491396076, 10.36894250292379205 ) ) ;
#7933 = EDGE_CURVE ( 'NONE', #87224, #2388, #51928, .T. ) ;
#7934 = CARTESIAN_POINT ( 'NONE',  ( 16.40814093676324603, 17.45696800326375353, -11.09922568453594671 ) ) ;
#7935 = LINE ( 'NONE', #8417, #91441 ) ;
#7936 = EDGE_LOOP ( 'NONE', ( #14023, #18032, #5066, #7210 ) ) ;
#7937 = CARTESIAN_POINT ( 'NONE',  ( 19.38216949554541557, 12.24863466993041961, -9.382169495545420901 ) ) ;
#7938 = CARTESIAN_POINT ( 'NONE',  ( 19.42250999205614193, 15.14701867748817143, 5.440088680355555262 ) ) ;
#7939 = EDGE_CURVE ( 'NONE', #72059, #69558, #78698, .T. ) ;
#7940 = CARTESIAN_POINT ( 'NONE',  ( 7.084665262690076126, 54.10535201082151247, 10.88017736071109987 ) ) ;
#7941 = ORIENTED_EDGE ( 'NONE', *, *, #92769, .T. ) ;
#7942 = TOROIDAL_SURFACE ( 'NONE', #95802, 3.699999999999999289, 0.2999999999999999889 ) ;
#7943 = CARTESIAN_POINT ( 'NONE',  ( 0.1532563361054083140, 1.008931151000784787, 1.131784320476157264E-15 ) ) ;
#7944 = CARTESIAN_POINT ( 'NONE',  ( 1.472469842513823179, 55.59226448433412315, -4.923371831947296329 ) ) ;
#7945 = CARTESIAN_POINT ( 'NONE',  ( 14.92337183194729988, 44.34226448433412315, -8.527530157486177487 ) ) ;
#7946 = CARTESIAN_POINT ( 'NONE',  ( 0.1532563361054082862, 31.21726448433412315, 2.638427012816831674 ) ) ;
#7947 = CARTESIAN_POINT ( 'NONE',  ( -12.60589901313210071, 0.5000000000000004441, -8.129656208642224158 ) ) ;
#7948 = VECTOR ( 'NONE', #17828, 1000.000000000000114 ) ;
#7950 = CARTESIAN_POINT ( 'NONE',  ( -1.099225684535947600, 34.54030133659708923, 6.408140936763237150 ) ) ;
#7949 = CARTESIAN_POINT ( 'NONE',  ( -4.000000000000000000, 78.07179676972445748, -6.500000000000000888 ) ) ;
#7952 = DIRECTION ( 'NONE',  ( 0.000000000000000000, 1.000000000000000000, 0.000000000000000000 ) ) ;
#7951 = CARTESIAN_POINT ( 'NONE',  ( 2.791683348922237240, 20.38393115100078745, -7.208316651077763204 ) ) ;
#7953 = CARTESIAN_POINT ( 'NONE',  ( 21.92686044187657046, 45.16212336850780673, 4.562052436263912550E-16 ) ) ;
#7955 = ORIENTED_EDGE ( 'NONE', *, *, #51347, .F. ) ;
#7954 = CARTESIAN_POINT ( 'NONE',  ( 14.92337183194729988, 44.34226448433412315, -8.527530157486177487 ) ) ;
#7956 = CARTESIAN_POINT ( 'NONE',  ( 11.59608414876348448, 14.76930270348882068, -9.421724210956282874 ) ) ;
#7957 = CARTESIAN_POINT ( 'NONE',  ( 16.40814093676323893, 15.79030133659708746, 11.09922568453595026 ) ) ;
#7958 = EDGE_CURVE ( 'NONE', #85917, #14813, #98301, .T. ) ;
#7959 = CARTESIAN_POINT ( 'NONE',  ( 10.00000000000000000, 51.81368534415484106, -10.88017736071110342 ) ) ;
#7960 = CARTESIAN_POINT ( 'NONE',  ( -4.164238869374099927, 27.01208216824730357, 3.795296366450308767 ) ) ;
#7961 = CARTESIAN_POINT ( 'NONE',  ( 1.602071938427519049, 42.02224192338641018, -6.500000000000035527 ) ) ;
#7962 = CARTESIAN_POINT ( 'NONE',  ( 17.08211943468705840, 30.13708216824730357, -12.26659068614894466 ) ) ;
#7963 = ADVANCED_FACE ( 'NONE', ( #16556 ), #86656, .T. ) ;
#7964 = CARTESIAN_POINT ( 'NONE',  ( 6.204703633549690345, 55.76208216824730357, -14.16423886937410259 ) ) ;
#7965 = CARTESIAN_POINT ( 'NONE',  ( 13.79529636645030344, 8.262082168247300018, 14.16423886937410614 ) ) ;
#7967 = CARTESIAN_POINT ( 'NONE',  ( -13.34400464406060571, 90.99713512412014893, -7.995014993563001049 ) ) ;
#7966 = CARTESIAN_POINT ( 'NONE',  ( 10.00000000000000000, 30.55374883491397142, -14.16423886937410082 ) ) ;
#7968 = CARTESIAN_POINT ( 'NONE',  ( 15.44008868035555793, 56.39701867748817676, -9.422509992056140149 ) ) ;
#7969 = CARTESIAN_POINT ( 'NONE',  ( 19.89220837332776526, 24.74062864464239553, 6.478736007405958119 ) ) ;
#7971 = CARTESIAN_POINT ( 'NONE',  ( 17.20831665107776587, 49.13393115100078745, -7.208316651077762316 ) ) ;
#7970 = CARTESIAN_POINT ( 'NONE',  ( 5.678900477127609037, -28.62996443930519774, 2.500000000000000000 ) ) ;
#7972 = CARTESIAN_POINT ( 'NONE',  ( 15.44008868035555793, 21.39701867748817321, -9.422509992056140149 ) ) ;
#7973 = LINE ( 'NONE', #84942, #97806 ) ;
#7974 = CARTESIAN_POINT ( 'NONE',  ( 5.076628168052703671, 61.84226448433412315, 8.527530157486179263 ) ) ;
#7975 = CARTESIAN_POINT ( 'NONE',  ( 12.00809552683965364, 14.49999999999999112, -8.989195838243565717 ) ) ;
#7976 = CARTESIAN_POINT ( 'NONE',  ( 0.1532563361054083140, 31.00893115100078390, 1.131784320476157264E-15 ) ) ;
#7977 = CARTESIAN_POINT ( 'NONE',  ( 13.43411237798105340, 50.58196800326375353, 12.81628187352647963 ) ) ;
#7978 = CARTESIAN_POINT ( 'NONE',  ( 14.16423886937410082, -0.4879178317526934872, -3.795296366450314096 ) ) ;
#7979 = CARTESIAN_POINT ( 'NONE',  ( 14.92337183194729988, 44.34226448433412315, -8.527530157486177487 ) ) ;
#7980 = CARTESIAN_POINT ( 'NONE',  ( 0.1532563361054083140, 56.00893115100078745, 1.131784320476157264E-15 ) ) ;
#7981 = CARTESIAN_POINT ( 'NONE',  ( 20.36894250292379738, 34.92874883491396076, -10.36894250292379027 ) ) ;
#7982 = ORIENTED_EDGE ( 'NONE', *, *, #51956, .T. ) ;
#7983 = CARTESIAN_POINT ( 'NONE',  ( 17.08211943468705130, 8.470415501580635720, 12.26659068614894998 ) ) ;
#7984 = CARTESIAN_POINT ( 'NONE',  ( 7.084665262690076126, 64.10535201082150536, 10.88017736071109987 ) ) ;
#7985 = DIRECTION ( 'NONE',  ( -0.000000000000000000, 1.000000000000000000, -0.000000000000000000 ) ) ;
#7986 = CARTESIAN_POINT ( 'NONE',  ( -4.164238869374099039, 56.80374883491397497, 8.674139862899312516E-16 ) ) ;
#7987 = CARTESIAN_POINT ( 'NONE',  ( 16.40814093676324603, 17.45696800326375353, -11.09922568453594671 ) ) ;
#7988 = DIRECTION ( 'NONE',  ( -0.000000000000000000, 1.000000000000000000, -0.000000000000000000 ) ) ;
#7989 = CARTESIAN_POINT ( 'NONE',  ( 17.20831665107776587, 2.883931151000785231, 7.208316651077764980 ) ) ;
#7990 = CARTESIAN_POINT ( 'NONE',  ( -6.767445849361066301, 0.3640475087720979608, -13.38662304974506512 ) ) ;
#7991 = CARTESIAN_POINT ( 'NONE',  ( -9.990730578767623271, 46.91630561652144138, -2.899999999999999467 ) ) ;
#7992 = CARTESIAN_POINT ( 'NONE',  ( 13.79529636645031943, 60.34541550158063927, -14.16423886937409904 ) ) ;
#7993 = CARTESIAN_POINT ( 'NONE',  ( 5.000000000000002665, 44.99999999999999289, -7.000000000000000000 ) ) ;
#7994 = CARTESIAN_POINT ( 'NONE',  ( 20.88017736071110875, 25.77201867748816966, -2.915334737309920765 ) ) ;
#7995 = CARTESIAN_POINT ( 'NONE',  ( -0.8801773607111008646, 28.27201867748817321, 2.915334737309923430 ) ) ;
#7996 = CARTESIAN_POINT ( 'NONE',  ( 10.00000000000000178, 57.25893115100078745, 9.846743663894594434 ) ) ;
#7997 = CARTESIAN_POINT ( 'NONE',  ( 10.00000000000000000, 59.75893115100078745, -9.846743663894594434 ) ) ;
#7998 = CARTESIAN_POINT ( 'NONE',  ( 21.09922568453594849, 51.20696800326375353, 6.408140936763242479 ) ) ;
#8000 = ORIENTED_EDGE ( 'NONE', *, *, #13212, .F. ) ;
#7999 = VECTOR ( 'NONE', #78259, 1000.000000000000000 ) ;
#8001 = AXIS2_PLACEMENT_3D ( 'NONE', #60383, #70739, #2255 ) ;
#8002 = CARTESIAN_POINT ( 'NONE',  ( -0.8801773607111008646, 18.27201867748817321, 2.915334737309923430 ) ) ;
#8003 = CARTESIAN_POINT ( 'NONE',  ( 16.40814093676323893, 25.79030133659708923, 11.09922568453595026 ) ) ;
#8004 = CARTESIAN_POINT ( 'NONE',  ( 0.1034006766821532752, 4.444999227851523509E-16, 14.49963131600461175 ) ) ;
#8005 = CARTESIAN_POINT ( 'NONE',  ( 12.63842701281683034, 42.46726448433412315, 9.846743663894596210 ) ) ;
#8006 = CARTESIAN_POINT ( 'NONE',  ( -0.8801773607110991993, 47.85535201082150536, -2.915334737309923874 ) ) ;
#8007 = CARTESIAN_POINT ( 'NONE',  ( 10.00000000000000178, 20.37363466993042138, 12.81628187352647608 ) ) ;
#8009 = DIRECTION ( 'NONE',  ( -0.8433914458128884961, 0.000000000000000000, 0.5372996083468194461 ) ) ;
#8008 = CARTESIAN_POINT ( 'NONE',  ( 10.00000000000000000, 51.81368534415484106, -10.88017736071110342 ) ) ;
#8010 = DIRECTION ( 'NONE',  ( 0.000000000000000000, -1.000000000000000000, 0.000000000000000000 ) ) ;
#8011 = CARTESIAN_POINT ( 'NONE',  ( 10.00000000000000178, 45.37363466993041783, 12.81628187352647608 ) ) ;
#8012 = ORIENTED_EDGE ( 'NONE', *, *, #56486, .T. ) ;
#8013 = CARTESIAN_POINT ( 'NONE',  ( 7.361572987183170547, 57.05059781766744464, 9.846743663894590881 ) ) ;
#8014 = CARTESIAN_POINT ( 'NONE',  ( 0.000000000000000000, 15.00000000000000000, 0.000000000000000000 ) ) ;
#8015 = CARTESIAN_POINT ( 'NONE',  ( 10.00000000000000178, 54.31368534415484106, 10.88017736071110342 ) ) ;
#8017 = CARTESIAN_POINT ( 'NONE',  ( 24.16423886937410614, 19.51208216824729647, -3.795296366450302550 ) ) ;
#8016 = CARTESIAN_POINT ( 'NONE',  ( 10.00000000000000178, 45.37363466993041783, 12.81628187352647608 ) ) ;
#8018 = CARTESIAN_POINT ( 'NONE',  ( 1.472469842513823179, 10.59226448433411782, -4.923371831947296329 ) ) ;
#8019 = DIRECTION ( 'NONE',  ( 0.000000000000000000, -1.000000000000000000, 0.000000000000000000 ) ) ;
#8020 = CARTESIAN_POINT ( 'NONE',  ( 19.84674366389459621, 28.50893115100078745, 7.409399052514197653E-17 ) ) ;
#8021 = CARTESIAN_POINT ( 'NONE',  ( 14.92337183194729988, 9.342264484334119601, -8.527530157486177487 ) ) ;
#8022 = CARTESIAN_POINT ( 'NONE',  ( -42.16485527613927076, 107.5383484153110061, 5.000000000000000000 ) ) ;
#8023 = CARTESIAN_POINT ( 'NONE',  ( -2.266590686148945544, 46.38708216824730357, -7.082119434687050408 ) ) ;
#8024 = CARTESIAN_POINT ( 'NONE',  ( 64.56412365047462742, 26.99999999999999645, -9.500000000000000000 ) ) ;
#8025 = EDGE_CURVE ( 'NONE', #73183, #71843, #14594, .T. ) ;
#8026 = CARTESIAN_POINT ( 'NONE',  ( 20.88017736071110875, 10.77201867748817143, -2.915334737309920765 ) ) ;
#8027 = DIRECTION ( 'NONE',  ( 0.000000000000000000, 1.000000000000000000, 0.000000000000000000 ) ) ;
#8028 = ORIENTED_EDGE ( 'NONE', *, *, #13420, .T. ) ;
#8029 = CARTESIAN_POINT ( 'NONE',  ( 19.42250999205614193, 15.14701867748817143, 5.440088680355555262 ) ) ;
#8030 = CARTESIAN_POINT ( 'NONE',  ( 2.035157376598822676, 7.438685344154837509, -7.964842623401177768 ) ) ;
#8031 = CARTESIAN_POINT ( 'NONE',  ( 7.361572987183169658, 39.96726448433411605, -9.846743663894592657 ) ) ;
#8032 = CARTESIAN_POINT ( 'NONE',  ( 10.00000000000000000, 37.87363466993041783, -12.81628187352647608 ) ) ;
#8033 = DIRECTION ( 'NONE',  ( 1.000000000000000000, 0.000000000000000000, 0.000000000000000000 ) ) ;
#8035 = CARTESIAN_POINT ( 'NONE',  ( 13.79529636645031943, 5.345415501580634832, -14.16423886937409904 ) ) ;
#8034 = CARTESIAN_POINT ( 'NONE',  ( 1.274849032794199255, 23.57228050351030646, 6.499999999999850786 ) ) ;
#8036 = CARTESIAN_POINT ( 'NONE',  ( 17.96484262340118221, 29.93868534415484106, 7.964842623401181321 ) ) ;
#8037 = CARTESIAN_POINT ( 'NONE',  ( -0.3689425029237898834, 66.17874883491396076, -10.36894250292378850 ) ) ;
#8038 = CARTESIAN_POINT ( 'NONE',  ( 19.84674366389459266, 43.71726448433410894, -2.638427012816827677 ) ) ;
#8039 = DIRECTION ( 'NONE',  ( 1.000000000000000000, -0.000000000000000000, -0.000000000000000000 ) ) ;
#8040 = CARTESIAN_POINT ( 'NONE',  ( 2.791683348922240793, 26.63393115100078745, 7.208316651077764092 ) ) ;
#8041 = FILL_AREA_STYLE_COLOUR ( '', #84950 ) ;
#8042 = CARTESIAN_POINT ( 'NONE',  ( -5.204170427930421283E-15, -42.12636533006957507, -12.81628187352647608 ) ) ;
#8043 = ORIENTED_EDGE ( 'NONE', *, *, #9359, .F. ) ;
#8044 = B_SPLINE_CURVE_WITH_KNOTS ( 'NONE', 3,
 ( #73704, #43707, #65213, #81217, #65711, #12222 ),
 .UNSPECIFIED., .F., .F.,
 ( 4, 2, 4 ),
 ( 3.409110551417103194E-05, 0.0004400426677359989529, 0.0008459942299578269553 ),
 .UNSPECIFIED. ) ;
#8045 = CARTESIAN_POINT ( 'NONE',  ( 0.000000000000000000, 15.00000000000000000, 0.000000000000000000 ) ) ;
#8046 = ORIENTED_EDGE ( 'NONE', *, *, #43468, .T. ) ;
#8048 = CARTESIAN_POINT ( 'NONE',  ( 20.88017736071110519, 40.56368534415484106, 2.639326808657452039E-16 ) ) ;
#8047 = CARTESIAN_POINT ( 'NONE',  ( 10.00000000000000178, 34.31368534415484106, 10.88017736071110342 ) ) ;
#8050 = CARTESIAN_POINT ( 'NONE',  ( 21.09922568453595559, 32.04030133659708923, -6.408140936763230044 ) ) ;
#8049 = CARTESIAN_POINT ( 'NONE',  ( 7.084665262690076126, 2.022018677488170990, -10.88017736071110164 ) ) ;
#8051 = CARTESIAN_POINT ( 'NONE',  ( 24.16423886937410614, 19.51208216824729647, -3.795296366450302550 ) ) ;
#8052 = VECTOR ( 'NONE', #12171, 1000.000000000000114 ) ;
#8053 = EDGE_CURVE ( 'NONE', #68797, #97455, #34947, .T. ) ;
#8054 = CARTESIAN_POINT ( 'NONE',  ( 19.38216949554541557, 42.24863466993041783, -9.382169495545420901 ) ) ;
#8055 = VERTEX_POINT ( 'NONE', #92050 ) ;
#8056 = CARTESIAN_POINT ( 'NONE',  ( 0.1532563361054100626, 50.80059781766745175, -2.638427012816831230 ) ) ;
#8057 = EDGE_CURVE ( 'NONE', #25434, #98109, #45062, .T. ) ;
#8058 = CARTESIAN_POINT ( 'NONE',  ( 17.96484262340118221, 24.93868534415484461, 7.964842623401181321 ) ) ;
#8059 = ORIENTED_EDGE ( 'NONE', *, *, #98705, .T. ) ;
#8060 = VECTOR ( 'NONE', #31455, 1000.000000000000000 ) ;
#8061 = CARTESIAN_POINT ( 'NONE',  ( 2.035157376598822676, 22.43868534415483396, -7.964842623401177768 ) ) ;
#8062 = ORIENTED_EDGE ( 'NONE', *, *, #48567, .T. ) ;
#8063 = CARTESIAN_POINT ( 'NONE',  ( 10.00000000000000000, 56.81368534415484106, -10.88017736071110342 ) ) ;
#8064 = AXIS2_PLACEMENT_3D ( 'NONE', #73280, #91113, #12288 ) ;
#8065 = CARTESIAN_POINT ( 'NONE',  ( 12.91533473730993009, 61.60535201082150536, -10.88017736071109987 ) ) ;
#8066 = CARTESIAN_POINT ( 'NONE',  ( 1.472469842513823179, 0.5922644843341181575, -4.923371831947296329 ) ) ;
#8067 = CARTESIAN_POINT ( 'NONE',  ( 19.42250999205614193, 55.14701867748817676, 5.440088680355555262 ) ) ;
#8068 = CARTESIAN_POINT ( 'NONE',  ( -46.94000000000000483, 101.1610691152320953, 7.882642855612810528 ) ) ;
#8069 = CARTESIAN_POINT ( 'NONE',  ( 1.472469842513823179, 10.59226448433411782, -4.923371831947296329 ) ) ;
#8071 = ORIENTED_EDGE ( 'NONE', *, *, #891, .T. ) ;
#8070 = FACE_OUTER_BOUND ( 'NONE', #91251, .T. ) ;
#8072 = CARTESIAN_POINT ( 'NONE',  ( 19.84674366389459621, 43.50893115100078745, 7.409399052514197653E-17 ) ) ;
#8073 = ORIENTED_EDGE ( 'NONE', *, *, #2694, .F. ) ;
#8074 = CARTESIAN_POINT ( 'NONE',  ( 5.076628168052703671, 66.84226448433412315, 8.527530157486179263 ) ) ;
#8075 = CARTESIAN_POINT ( 'NONE',  ( 17.08211943468705840, 15.13708216824730179, -12.26659068614894466 ) ) ;
#8076 = VERTEX_POINT ( 'NONE', #63989 ) ;
#8077 = VECTOR ( 'NONE', #95656, 1000.000000000000000 ) ;
#8078 = CARTESIAN_POINT ( 'NONE',  ( 19.80832241502127289, 29.75868815902069997, 6.499999999999991118 ) ) ;
#8080 = CARTESIAN_POINT ( 'NONE',  ( 7.084665262690076126, 59.10535201082150536, 10.88017736071109987 ) ) ;
#8079 = CARTESIAN_POINT ( 'NONE',  ( 19.72487221294570858, 9.782175860852373006, 6.500000000000000000 ) ) ;
#8081 = CARTESIAN_POINT ( 'NONE',  ( -0.8801773607110991993, 7.855352010821506248, -2.915334737309923874 ) ) ;
#8082 = FACE_OUTER_BOUND ( 'NONE', #22544, .T. ) ;
#8084 = ORIENTED_EDGE ( 'NONE', *, *, #87293, .F. ) ;
#8083 = CARTESIAN_POINT ( 'NONE',  ( 6.565887622018943937, 40.16530133659708923, 12.81628187352647430 ) ) ;
#8085 = CARTESIAN_POINT ( 'NONE',  ( 14.92337183194729633, 2.675597817667451750, 8.527530157486181039 ) ) ;
#8086 =( NAMED_UNIT ( * ) PLANE_ANGLE_UNIT ( ) SI_UNIT ( $, .RADIAN. ) );
#8087 = CARTESIAN_POINT ( 'NONE',  ( 3.591859063236763294, 33.29030133659708213, -11.09922568453595026 ) ) ;
#8089 = EDGE_CURVE ( 'NONE', #5244, #52640, #47126, .T. ) ;
#8088 = CARTESIAN_POINT ( 'NONE',  ( 5.076628168052704559, 20.17559781766745175, -8.527530157486179263 ) ) ;
#8090 = SURFACE_STYLE_USAGE ( .BOTH. , #7609 ) ;
#8091 = CARTESIAN_POINT ( 'NONE',  ( -2.816281873526473856, 19.33196800326375708, 3.434112377981055619 ) ) ;
#8092 = CARTESIAN_POINT ( 'NONE',  ( 8.921421356237301481, 27.04185244743870697, -3.000000000000000888 ) ) ;
#8093 = AXIS2_PLACEMENT_3D ( 'NONE', #35104, #43601, #58604 ) ;
#8094 = CARTESIAN_POINT ( 'NONE',  ( 1.472469842513823179, 6.425597817667451750, 4.923371831947296329 ) ) ;
#8095 = ORIENTED_EDGE ( 'NONE', *, *, #82686, .T. ) ;
#8096 = ORIENTED_EDGE ( 'NONE', *, *, #54951, .F. ) ;
#8097 = CARTESIAN_POINT ( 'NONE',  ( 10.00000000000000000, 16.81368534415483751, -10.88017736071110342 ) ) ;
#8098 = CARTESIAN_POINT ( 'NONE',  ( 10.00000000000000178, 13.05374883491396787, 14.16423886937410082 ) ) ;
#8099 = CARTESIAN_POINT ( 'NONE',  ( 2.791683348922237240, 35.38393115100079456, -7.208316651077763204 ) ) ;
#8100 = CARTESIAN_POINT ( 'NONE',  ( 2.035157376598824452, 68.68868534415484817, 7.964842623401179544 ) ) ;
#8102 = CARTESIAN_POINT ( 'NONE',  ( -6.982525766139714207, -88.11956320875633253, -3.750000000000000000 ) ) ;
#8101 = CARTESIAN_POINT ( 'NONE',  ( 10.00000000000000178, 45.37363466993041783, 12.81628187352647608 ) ) ;
#8103 = CARTESIAN_POINT ( 'NONE',  ( 2.035157376598822676, 12.43868534415483751, -7.964842623401177768 ) ) ;
#8104 = CARTESIAN_POINT ( 'NONE',  ( 7.313705784284628031, 14.63606873438734901, -13.09617149020746751 ) ) ;
#8105 = CARTESIAN_POINT ( 'NONE',  ( -2.816281873526473856, 14.33196800326375531, 3.434112377981055619 ) ) ;
#8106 = CARTESIAN_POINT ( 'NONE',  ( 13.43411237798106583, 7.665301336597086568, -12.81628187352647252 ) ) ;
#8107 = CARTESIAN_POINT ( 'NONE',  ( 14.92337183194729633, 22.67559781766745175, 8.527530157486181039 ) ) ;
#8108 = CARTESIAN_POINT ( 'NONE',  ( -5.440088680355558814, -7.769647989178493752, -9.422509992056136596 ) ) ;
#8109 = CARTESIAN_POINT ( 'NONE',  ( -2.816281873526473856, 29.33196800326376064, 3.434112377981055619 ) ) ;
#8110 = CARTESIAN_POINT ( 'NONE',  ( 13.78891971893208357, 0.5000000000000004441, -5.904717858191528279 ) ) ;
#8112 = DIRECTION ( 'NONE',  ( -0.000000000000000000, -1.000000000000000000, -0.000000000000000000 ) ) ;
#8111 = CARTESIAN_POINT ( 'NONE',  ( 7.084665262690076126, 59.10535201082150536, 10.88017736071109987 ) ) ;
#8113 = FACE_OUTER_BOUND ( 'NONE', #54263, .T. ) ;
#8114 = CARTESIAN_POINT ( 'NONE',  ( 7.084665262690076126, 69.10535201082151957, 10.88017736071109987 ) ) ;
#8115 = CARTESIAN_POINT ( 'NONE',  ( 4.559911319644449179, 43.89701867748816966, 9.422509992056141925 ) ) ;
#8116 = STYLED_ITEM ( 'NONE', ( #20534 ), #62435 ) ;
#8117 = CARTESIAN_POINT ( 'NONE',  ( 20.88017736071110164, 40.35535201082150536, 2.915334737309930979 ) ) ;
#8118 = CARTESIAN_POINT ( 'NONE',  ( 20.15039907845753220, 56.74884699246889141, 6.262539305110074395 ) ) ;
#8119 = CARTESIAN_POINT ( 'NONE',  ( -7.002992508388866888, -2.668153783851045279E-15, -12.84003923133027492 ) ) ;
#8120 = CARTESIAN_POINT ( 'NONE',  ( 2.791683348922237240, 50.38393115100078035, -7.208316651077763204 ) ) ;
#8122 = CARTESIAN_POINT ( 'NONE',  ( 9.876730923139225737, 0.5000000000000004441, 11.28938378619069560 ) ) ;
#8121 = CARTESIAN_POINT ( 'NONE',  ( 7.084665262690076126, 7.022018677488169658, -10.88017736071110164 ) ) ;
#8123 = STYLED_ITEM ( 'NONE', ( #60741 ), #46435 ) ;
#8124 = CARTESIAN_POINT ( 'NONE',  ( 16.40814093676324603, 7.456968003263754419, -11.09922568453594671 ) ) ;
#8125 = ORIENTED_EDGE ( 'NONE', *, *, #27988, .F. ) ;
#8126 = CARTESIAN_POINT ( 'NONE',  ( 20.88017736071110164, 35.35535201082150536, 2.915334737309930979 ) ) ;
#8128 = CARTESIAN_POINT ( 'NONE',  ( -20.19000000000001194, 92.00000000000000000, -10.09898361729590199 ) ) ;
#8127 = CARTESIAN_POINT ( 'NONE',  ( 0.6178305044545818747, 3.498634669930420049, -9.382169495545419124 ) ) ;
#8129 = CARTESIAN_POINT ( 'NONE',  ( -0.8801773607110991993, 12.85535201082150358, -2.915334737309923874 ) ) ;
#8130 = VECTOR ( 'NONE', #76000, 1000.000000000000000 ) ;
#8131 = CARTESIAN_POINT ( 'NONE',  ( 19.42250999205614548, 30.98035201082150536, -5.440088680355545492 ) ) ;
#8132 = CARTESIAN_POINT ( 'NONE',  ( 17.08211943468705840, 35.13708216824730357, -12.26659068614894466 ) ) ;
#8133 = CARTESIAN_POINT ( 'NONE',  ( 19.84674366389459621, 33.50893115100078745, 7.409399052514197653E-17 ) ) ;
#8134 = CARTESIAN_POINT ( 'NONE',  ( 20.88017736071110164, 45.35535201082149115, 2.915334737309930979 ) ) ;
#8135 = DIRECTION ( 'NONE',  ( 0.000000000000000000, 1.000000000000000000, 0.000000000000000000 ) ) ;
#8136 = CARTESIAN_POINT ( 'NONE',  ( 2.917880565312950480, 5.970415501580634832, -12.26659068614894821 ) ) ;
#8137 = ADVANCED_FACE ( 'NONE', ( #10513 ), #13613, .T. ) ;
#8138 = UNCERTAINTY_MEASURE_WITH_UNIT (LENGTH_MEASURE( 1.000000000000000082E-05 ), #18710, 'distance_accuracy_value', 'NONE');
#8139 = CARTESIAN_POINT ( 'NONE',  ( 3.469446951953614189E-15, 5.938309369127516391, 11.92686044187656513 ) ) ;
#8140 = CARTESIAN_POINT ( 'NONE',  ( 19.84674366389459266, 63.71726448433412315, -2.638427012816827677 ) ) ;
#8141 = VERTEX_POINT ( 'NONE', #93521 ) ;
#8142 = ORIENTED_EDGE ( 'NONE', *, *, #52894, .T. ) ;
#8143 = CARTESIAN_POINT ( 'NONE',  ( 10.00000000000000178, 33.05374883491396787, 14.16423886937410082 ) ) ;
#8144 = CARTESIAN_POINT ( 'NONE',  ( 10.00000000000000178, 18.05374883491396787, 14.16423886937410082 ) ) ;
#8145 = CARTESIAN_POINT ( 'NONE',  ( 18.52753015748617571, 3.092264484334118269, 4.923371831947298993 ) ) ;
#8146 = CARTESIAN_POINT ( 'NONE',  ( 17.20831665107776587, 62.88393115100078745, 7.208316651077764980 ) ) ;
#8147 = CARTESIAN_POINT ( 'NONE',  ( -11.58433430577145273, -69.52997016218431270, 3.750000000000000000 ) ) ;
#8149 = CARTESIAN_POINT ( 'NONE',  ( 13.43411237798105340, 15.58196800326374998, 12.81628187352647963 ) ) ;
#8148 = CARTESIAN_POINT ( 'NONE',  ( 0.5774900079438607392, 63.48035201082149825, 5.440088680355550821 ) ) ;
#8150 = CARTESIAN_POINT ( 'NONE',  ( -2.266590686148945544, 27.22041550158063572, 7.082119434687048631 ) ) ;
#8151 = CARTESIAN_POINT ( 'NONE',  ( 2.035157376598822676, 17.43868534415483751, -7.964842623401177768 ) ) ;
#8152 = CARTESIAN_POINT ( 'NONE',  ( 20.88017736071110164, 35.35535201082150536, 2.915334737309930979 ) ) ;
#8153 = LINE ( 'NONE', #15665, #1303 ) ;
#8154 = CARTESIAN_POINT ( 'NONE',  ( 17.96484262340118221, 56.18868534415484817, -7.964842623401177768 ) ) ;
#8155 = CARTESIAN_POINT ( 'NONE',  ( 13.43411237798106583, 52.66530133659708213, -12.81628187352647252 ) ) ;
#8156 = CARTESIAN_POINT ( 'NONE',  ( -9.846743663894594434, -18.99106884899921255, 3.469446951953614189E-15 ) ) ;
#8157 = EDGE_LOOP ( 'NONE', ( #43861, #13677, #27585, #4220, #97678, #42682 ) ) ;
#8158 = FILL_AREA_STYLE_COLOUR ( '', #93820 ) ;
#8159 = VERTEX_POINT ( 'NONE', #72481 ) ;
#8160 = DIRECTION ( 'NONE',  ( 0.000000000000000000, 0.000000000000000000, 1.000000000000000000 ) ) ;
#8161 = VERTEX_POINT ( 'NONE', #4015 ) ;
#8162 = AXIS2_PLACEMENT_3D ( 'NONE', #83103, #73616, #88622 ) ;
#8163 = DIRECTION ( 'NONE',  ( 0.000000000000000000, 1.000000000000000000, 0.000000000000000000 ) ) ;
#8165 = CARTESIAN_POINT ( 'NONE',  ( 10.00000000000000000, 65.55374883491396076, -14.16423886937410082 ) ) ;
#8164 = CARTESIAN_POINT ( 'NONE',  ( 13.79529636645031943, 55.34541550158062506, -14.16423886937409904 ) ) ;
#8167 = CARTESIAN_POINT ( 'NONE',  ( 1.472469842513823179, 55.59226448433412315, -4.923371831947296329 ) ) ;
#8166 = CARTESIAN_POINT ( 'NONE',  ( 19.84674366389459266, 18.30059781766745175, 2.638427012816836559 ) ) ;
#8168 = DIRECTION ( 'NONE',  ( 0.9953961983671798519, 0.000000000000000000, -0.09584575252021386438 ) ) ;
#8169 = STYLED_ITEM ( 'NONE', ( #35882 ), #80046 ) ;
#8170 = ADVANCED_FACE ( 'NONE', ( #63511 ), #56728, .T. ) ;
#8171 = CARTESIAN_POINT ( 'NONE',  ( -2.816281873526473856, -0.8763653300695799508, 9.499525473075851096E-16 ) ) ;
#8172 = CARTESIAN_POINT ( 'NONE',  ( -12.81628187352647252, 24.33196800326376064, 3.434112377981066722 ) ) ;
#8173 = ORIENTED_EDGE ( 'NONE', *, *, #29529, .F. ) ;
#8174 = CARTESIAN_POINT ( 'NONE',  ( 17.08211943468705130, 28.47041550158063572, 12.26659068614894998 ) ) ;
#8175 = EDGE_CURVE ( 'NONE', #75802, #25854, #25049, .T. ) ;
#8176 = CARTESIAN_POINT ( 'NONE',  ( 22.26659068614895176, 39.72041550158063217, -7.082119434687042414 ) ) ;
#8177 = ORIENTED_EDGE ( 'NONE', *, *, #62796, .F. ) ;
#8178 = CARTESIAN_POINT ( 'NONE',  ( -1.099225684535947600, 54.54030133659708923, 6.408140936763237150 ) ) ;
#8179 = CARTESIAN_POINT ( 'NONE',  ( 19.84674366389459266, 48.30059781766745175, 2.638427012816836559 ) ) ;
#8180 = CARTESIAN_POINT ( 'NONE',  ( 2.035157376598822676, 22.43868534415483396, -7.964842623401177768 ) ) ;
#8181 = CARTESIAN_POINT ( 'NONE',  ( -6.822555938877846948, -84.39442183841865130, 2.500000000000000444 ) ) ;
#8182 = CARTESIAN_POINT ( 'NONE',  ( 12.63842701281683034, 52.46726448433413026, 9.846743663894596210 ) ) ;
#8183 = CARTESIAN_POINT ( 'NONE',  ( 7.361572987183170547, 47.05059781766745175, 9.846743663894590881 ) ) ;
#8184 = STYLED_ITEM ( 'NONE', ( #77535 ), #33405 ) ;
#8186 = AXIS2_PLACEMENT_3D ( 'NONE', #21844, #45823, #30301 ) ;
#8185 = CARTESIAN_POINT ( 'NONE',  ( 1.180296924652914470, 0.000000000000000000, -5.323975374878053834 ) ) ;
#8187 = DIRECTION ( 'NONE',  ( 0.000000000000000000, 1.000000000000000000, 0.000000000000000000 ) ) ;
#8188 = CARTESIAN_POINT ( 'NONE',  ( 12.63842701281683922, 4.550597817667451750, -9.846743663894590881 ) ) ;
#8189 = DIRECTION ( 'NONE',  ( -0.000000000000000000, -0.000000000000000000, 1.000000000000000000 ) ) ;
#8190 = VERTEX_POINT ( 'NONE', #2060 ) ;
#8191 = CARTESIAN_POINT ( 'NONE',  ( 8.880000000000000782, 1.019547802438459216, 3.750000000000000000 ) ) ;
#8192 = CARTESIAN_POINT ( 'NONE',  ( 19.84674366389459621, 33.50893115100078745, 7.409399052514197653E-17 ) ) ;
#8193 = CARTESIAN_POINT ( 'NONE',  ( 6.761335002693003027, 14.76984993307862482, 13.32315948060042743 ) ) ;
#8194 = CARTESIAN_POINT ( 'NONE',  ( 3.591859063236763294, 38.29030133659708923, -11.09922568453595026 ) ) ;
#8195 = PRESENTATION_LAYER_ASSIGNMENT (  '', '', ( #56087 ) ) ;
#8196 =( NAMED_UNIT ( * ) SI_UNIT ( $, .STERADIAN. ) SOLID_ANGLE_UNIT ( ) );
#8197 = DIRECTION ( 'NONE',  ( -0.8320502943378436100, 0.5547001962252291474, -0.000000000000000000 ) ) ;
#8198 = ORIENTED_EDGE ( 'NONE', *, *, #14233, .F. ) ;
#8199 = CARTESIAN_POINT ( 'NONE',  ( 7.361572987183170547, 67.05059781766746596, 9.846743663894590881 ) ) ;
#8200 = CARTESIAN_POINT ( 'NONE',  ( 0.000000000000000000, 15.00000000000000000, 0.000000000000000000 ) ) ;
#8201 = CARTESIAN_POINT ( 'NONE',  ( 17.20831665107776587, 59.13393115100078745, -7.208316651077762316 ) ) ;
#8202 = CARTESIAN_POINT ( 'NONE',  ( 13.79529636645030344, 28.26208216824729647, 14.16423886937410614 ) ) ;
#8203 = CARTESIAN_POINT ( 'NONE',  ( 0.1532563361054083140, 56.00893115100078745, 1.131784320476157264E-15 ) ) ;
#8204 = DIRECTION ( 'NONE',  ( -0.000000000000000000, -1.000000000000000000, -0.000000000000000000 ) ) ;
#8205 = CARTESIAN_POINT ( 'NONE',  ( 14.92337183194729988, 24.34226448433411960, -8.527530157486177487 ) ) ;
#8206 = CARTESIAN_POINT ( 'NONE',  ( 3.591859063236763294, 48.29030133659708923, -11.09922568453595026 ) ) ;
#8207 = CARTESIAN_POINT ( 'NONE',  ( 10.00000000000000178, 3.053748834913967425, 14.16423886937410082 ) ) ;
#8208 = CARTESIAN_POINT ( 'NONE',  ( 7.361572987183170547, 52.05059781766745175, 9.846743663894590881 ) ) ;
#8210 = EDGE_CURVE ( 'NONE', #67800, #37192, #74579, .T. ) ;
#8209 = CARTESIAN_POINT ( 'NONE',  ( 0.5774900079438607392, 48.48035201082150536, 5.440088680355550821 ) ) ;
#8211 = CARTESIAN_POINT ( 'NONE',  ( 10.00000000000000000, 39.75893115100078745, -9.846743663894594434 ) ) ;
#8212 = CARTESIAN_POINT ( 'NONE',  ( -0.1034006766821533585, 15.00000000000000000, -14.49963131600461175 ) ) ;
#8213 = ORIENTED_EDGE ( 'NONE', *, *, #11124, .F. ) ;
#8214 = CARTESIAN_POINT ( 'NONE',  ( 19.42250999205614548, 60.98035201082151247, -5.440088680355545492 ) ) ;
#8215 = ORIENTED_EDGE ( 'NONE', *, *, #47389, .F. ) ;
#8216 = CARTESIAN_POINT ( 'NONE',  ( -6.732636091893173358, -88.11213685669363826, 2.500000000000000000 ) ) ;
#8217 = CARTESIAN_POINT ( 'NONE',  ( 19.42250999205614548, 25.98035201082150891, -5.440088680355545492 ) ) ;
#8219 = CARTESIAN_POINT ( 'NONE',  ( 4.559911319644449179, 57.23035201082150536, -9.422509992056141925 ) ) ;
#8218 = CARTESIAN_POINT ( 'NONE',  ( 18.52753015748618282, 63.92559781766745886, -4.923371831947291888 ) ) ;
#8220 = CARTESIAN_POINT ( 'NONE',  ( 7.084665262690076126, 69.10535201082151957, 10.88017736071109987 ) ) ;
#8221 = DIRECTION ( 'NONE',  ( -1.000000000000000000, 0.000000000000000000, 0.000000000000000000 ) ) ;
#8223 = DIRECTION ( 'NONE',  ( -1.000000000000000000, 0.000000000000000000, 0.000000000000000000 ) ) ;
#8222 = CARTESIAN_POINT ( 'NONE',  ( -0.8801773607111008646, 43.27201867748817676, 2.915334737309923430 ) ) ;
#8224 = MANIFOLD_SOLID_BREP ( 'CirPattern1', #25068 ) ;
#8225 = CARTESIAN_POINT ( 'NONE',  ( 19.84674366389459621, 43.50893115100078745, 7.409399052514197653E-17 ) ) ;
#8226 = DIRECTION ( 'NONE',  ( 1.000000000000000000, 0.000000000000000000, 0.000000000000000000 ) ) ;
#8227 = CARTESIAN_POINT ( 'NONE',  ( 10.36894250292379027, 23.67874883491397142, 10.36894250292378672 ) ) ;
#8228 = CARTESIAN_POINT ( 'NONE',  ( 0.1532563361054082862, 61.21726448433412315, 2.638427012816831674 ) ) ;
#8229 = CARTESIAN_POINT ( 'NONE',  ( 12.91533473730992121, 19.52201867748816611, 10.88017736071110164 ) ) ;
#8231 =( GEOMETRIC_REPRESENTATION_CONTEXT ( 3 ) GLOBAL_UNCERTAINTY_ASSIGNED_CONTEXT ( ( #57422 ) ) GLOBAL_UNIT_ASSIGNED_CONTEXT ( ( #29839, #52842, #68359 ) ) REPRESENTATION_CONTEXT ( 'NONE', 'WORKASPACE' ) );
#8230 = CARTESIAN_POINT ( 'NONE',  ( -10.44999999999999751, 99.99999999999998579, -8.525133428036873795 ) ) ;
#8232 = CARTESIAN_POINT ( 'NONE',  ( 24.16423886937409904, 19.09541550158063927, 3.795296366450317205 ) ) ;
#8233 = CARTESIAN_POINT ( 'NONE',  ( 2.917880565312950480, 55.97041550158063217, -12.26659068614894821 ) ) ;
#8234 = CARTESIAN_POINT ( 'NONE',  ( 19.84674366389459621, 18.50893115100078745, 7.409399052514197653E-17 ) ) ;
#8235 = CARTESIAN_POINT ( 'NONE',  ( 20.15039907845753575, 32.62777174578613426, -6.262539305110076171 ) ) ;
#8236 = PRESENTATION_LAYER_ASSIGNMENT (  '', '', ( #88081 ) ) ;
#8237 = ORIENTED_EDGE ( 'NONE', *, *, #9740, .F. ) ;
#8238 = CARTESIAN_POINT ( 'NONE',  ( 5.076628168052704559, 20.17559781766745175, -8.527530157486179263 ) ) ;
#8239 = CARTESIAN_POINT ( 'NONE',  ( -0.8801773607110991993, 22.85535201082150181, -2.915334737309923874 ) ) ;
#8240 = CARTESIAN_POINT ( 'NONE',  ( 19.84674366389459266, 63.71726448433412315, -2.638427012816827677 ) ) ;
#8241 = CARTESIAN_POINT ( 'NONE',  ( -4.164238869374098151, 6.595415501580634832, -3.795296366450310543 ) ) ;
#8242 = DIRECTION ( 'NONE',  ( 1.257568779154408793E-17, 1.000000000000000000, -0.000000000000000000 ) ) ;
#8243 = CARTESIAN_POINT ( 'NONE',  ( 0.1532563361054100626, 15.80059781766745353, -2.638427012816831230 ) ) ;
#8244 = CARTESIAN_POINT ( 'NONE',  ( -2.816281873526473856, 44.12363466993042493, 9.499525473075851096E-16 ) ) ;
#8245 = CARTESIAN_POINT ( 'NONE',  ( 1.472469842513823179, 40.59226448433411605, -4.923371831947296329 ) ) ;
#8246 = VERTEX_POINT ( 'NONE', #33491 ) ;
#8247 = CARTESIAN_POINT ( 'NONE',  ( 12.63842701281683922, 19.55059781766745175, -9.846743663894590881 ) ) ;
#8248 = CARTESIAN_POINT ( 'NONE',  ( 14.56311970191028138, 14.76984991344722253, -3.337330457605880873 ) ) ;
#8249 = CARTESIAN_POINT ( 'NONE',  ( -4.164238869374099927, 57.01208216824731068, 3.795296366450308767 ) ) ;
#8250 = CARTESIAN_POINT ( 'NONE',  ( -19.89999999999999858, 92.00000000000000000, -7.750000000000000000 ) ) ;
#8251 = CARTESIAN_POINT ( 'NONE',  ( 2.791683348922237240, 35.38393115100079456, -7.208316651077763204 ) ) ;
#8252 = CARTESIAN_POINT ( 'NONE',  ( 20.88017736071110164, 5.355352010821502695, 2.915334737309930979 ) ) ;
#8253 = CARTESIAN_POINT ( 'NONE',  ( 14.92337183194729633, 52.67559781766745175, 8.527530157486181039 ) ) ;
#8254 = CARTESIAN_POINT ( 'NONE',  ( 20.88017736071110164, 55.35535201082149825, 2.915334737309930979 ) ) ;
#8255 = EDGE_CURVE ( 'NONE', #60677, #94458, #49001, .T. ) ;
#8256 = CARTESIAN_POINT ( 'NONE',  ( 10.00000000000000178, 2.258931151000784787, 9.846743663894594434 ) ) ;
#8257 = VECTOR ( 'NONE', #15038, 1000.000000000000000 ) ;
#8258 = ORIENTED_EDGE ( 'NONE', *, *, #60120, .T. ) ;
#8259 = VECTOR ( 'NONE', #47279, 1000.000000000000000 ) ;
#8260 = ORIENTED_EDGE ( 'NONE', *, *, #60753, .F. ) ;
#8261 = CARTESIAN_POINT ( 'NONE',  ( 6.767445849361160448, 14.49999999999999112, 13.38662304974508110 ) ) ;
#8262 = CARTESIAN_POINT ( 'NONE',  ( 4.629999999999995453, 43.00000000000000711, 4.250000000000000000 ) ) ;
#8263 = CARTESIAN_POINT ( 'NONE',  ( 2.791683348922237240, 25.38393115100078390, -7.208316651077763204 ) ) ;
#8264 = CARTESIAN_POINT ( 'NONE',  ( 6.565887622018943937, 63.08196800326376064, -12.81628187352647608 ) ) ;
#8266 = CARTESIAN_POINT ( 'NONE',  ( 17.20831665107776587, 42.88393115100077324, 7.208316651077764980 ) ) ;
#8265 = CARTESIAN_POINT ( 'NONE',  ( 10.00000000000000178, 68.05374883491397497, 14.16423886937410082 ) ) ;
#8267 = CARTESIAN_POINT ( 'NONE',  ( -4.249999999999994671, 43.00000000000000711, 6.500000000000000888 ) ) ;
#8268 = EDGE_CURVE ( 'NONE', #50375, #49115, #21547, .T. ) ;
#8269 = CARTESIAN_POINT ( 'NONE',  ( 24.16423886937410614, 24.30374883491396787, 8.672049930838204340E-16 ) ) ;
#8270 = CARTESIAN_POINT ( 'NONE',  ( 24.16423886937409904, 54.09541550158063217, 3.795296366450317205 ) ) ;
#8271 = CARTESIAN_POINT ( 'NONE',  ( 14.92337183194729633, 62.67559781766745886, 8.527530157486181039 ) ) ;
#8272 = CARTESIAN_POINT ( 'NONE',  ( 1.707155281725165397, 67.90189080397283306, 6.499999999999919176 ) ) ;
#8273 = CARTESIAN_POINT ( 'NONE',  ( 19.42250999205614548, 50.98035201082151247, -5.440088680355545492 ) ) ;
#8274 = CARTESIAN_POINT ( 'NONE',  ( 12.63842701281683922, 9.550597817667449974, -9.846743663894590881 ) ) ;
#8275 = CARTESIAN_POINT ( 'NONE',  ( -3.836050625226996580, -2.701282487337019145, 3.999999999999999112 ) ) ;
#8276 = ORIENTED_EDGE ( 'NONE', *, *, #58455, .T. ) ;
#8277 = DIRECTION ( 'NONE',  ( -0.6360782202777751637, -0.000000000000000000, 0.7716245833877106719 ) ) ;
#8278 = CIRCLE ( 'NONE', #35448, 9.538348415311009632 ) ;
#8279 = VERTEX_POINT ( 'NONE', #40037 ) ;
#8280 = EDGE_CURVE ( 'NONE', #62619, #94846, #34972, .T. ) ;
#8281 = CARTESIAN_POINT ( 'NONE',  ( 1.472469842513823179, 5.592264484334118713, -4.923371831947296329 ) ) ;
#8282 = ORIENTED_EDGE ( 'NONE', *, *, #19548, .T. ) ;
#8283 = CARTESIAN_POINT ( 'NONE',  ( -0.3689425029237881626, 22.42874883491397142, 10.36894250292379027 ) ) ;
#8284 = CARTESIAN_POINT ( 'NONE',  ( 0.1532563361054100626, 25.80059781766744820, -2.638427012816831230 ) ) ;
#8285 = CARTESIAN_POINT ( 'NONE',  ( -0.8801773607110991993, 32.85535201082151247, -2.915334737309923874 ) ) ;
#8286 = ORIENTED_EDGE ( 'NONE', *, *, #30815, .F. ) ;
#8287 = CARTESIAN_POINT ( 'NONE',  ( 10.00000000000000178, 24.31368534415484106, 10.88017736071110342 ) ) ;
#8288 = ORIENTED_EDGE ( 'NONE', *, *, #1056, .T. ) ;
#8289 = CARTESIAN_POINT ( 'NONE',  ( -0.8801773607111008646, 38.27201867748816255, 2.915334737309923430 ) ) ;
#8290 =( LENGTH_UNIT ( ) NAMED_UNIT ( * ) SI_UNIT ( .MILLI., .METRE. ) );
#8291 = EDGE_CURVE ( 'NONE', #8190, #31523, #34366, .T. ) ;
#8292 = FILL_AREA_STYLE ('',( #92280 ) ) ;
#8293 = ORIENTED_EDGE ( 'NONE', *, *, #60962, .T. ) ;
#8294 = CARTESIAN_POINT ( 'NONE',  ( 16.40814093676323893, 20.79030133659708923, 11.09922568453595026 ) ) ;
#8295 = CARTESIAN_POINT ( 'NONE',  ( 1.472469842513823179, 10.59226448433411782, -4.923371831947296329 ) ) ;
#8296 = DIRECTION ( 'NONE',  ( 0.000000000000000000, 0.000000000000000000, 1.000000000000000000 ) ) ;
#8297 = CARTESIAN_POINT ( 'NONE',  ( 1.472469842513823179, 15.59226448433411960, -4.923371831947296329 ) ) ;
#8298 = CARTESIAN_POINT ( 'NONE',  ( 0.5774900079438590739, 27.64701867748817676, -5.440088680355550821 ) ) ;
#8299 = VERTEX_POINT ( 'NONE', #95995 ) ;
#8300 = CIRCLE ( 'NONE', #68973, 2.250000000000000444 ) ;
#8301 = EDGE_LOOP ( 'NONE', ( #15157, #94152, #5535, #44717, #58647, #34551 ) ) ;
#8302 = CARTESIAN_POINT ( 'NONE',  ( 19.38216949554541557, 62.24863466993041072, -9.382169495545420901 ) ) ;
#8303 = CARTESIAN_POINT ( 'NONE',  ( 20.88017736071110519, 60.56368534415484106, 2.639326808657452039E-16 ) ) ;
#8304 = DIRECTION ( 'NONE',  ( 0.8070303256584299145, -0.5905099943842175847, 0.000000000000000000 ) ) ;
#8305 = SURFACE_STYLE_USAGE ( .BOTH. , #93762 ) ;
#8306 = CARTESIAN_POINT ( 'NONE',  ( 20.88017736071110519, 55.56368534415484817, 2.639326808657452039E-16 ) ) ;
#8307 = CARTESIAN_POINT ( 'NONE',  ( 3.591859063236761518, 4.956968003263753531, 11.09922568453594849 ) ) ;
#8308 = CARTESIAN_POINT ( 'NONE',  ( 56.78206182523731371, 44.99999999999999289, 0.000000000000000000 ) ) ;
#8309 = CARTESIAN_POINT ( 'NONE',  ( 0.1532563361054083140, 36.00893115100078745, 1.131784320476157264E-15 ) ) ;
#8310 = CARTESIAN_POINT ( 'NONE',  ( 21.09922568453595559, 52.04030133659708923, -6.408140936763230044 ) ) ;
#8311 = CARTESIAN_POINT ( 'NONE',  ( 3.699999999999999289, -3.175805879500891925E-16, 0.000000000000000000 ) ) ;
#8312 = CARTESIAN_POINT ( 'NONE',  ( 18.52753015748617571, 18.09226448433411960, 4.923371831947298993 ) ) ;
#8313 = CARTESIAN_POINT ( 'NONE',  ( 21.09922568453594849, 21.20696800326375353, 6.408140936763242479 ) ) ;
#8315 = CARTESIAN_POINT ( 'NONE',  ( 14.49999999999999822, 11.00000000000000000, 5.000000000000000000 ) ) ;
#8314 = CARTESIAN_POINT ( 'NONE',  ( 8.630000000000000782, 1.085138116723527427E-15, -3.750000000000000000 ) ) ;
#8316 = CARTESIAN_POINT ( 'NONE',  ( 20.88017736071110875, 30.77201867748816966, -2.915334737309920765 ) ) ;
#8317 = CARTESIAN_POINT ( 'NONE',  ( 10.00000000000000178, 67.25893115100079456, 9.846743663894594434 ) ) ;
#8318 = CARTESIAN_POINT ( 'NONE',  ( -10.84451454131299997, 15.00000000000000000, 9.625305416633544553 ) ) ;
#8319 = CARTESIAN_POINT ( 'NONE',  ( 0.1532563361054100626, 25.80059781766744820, -2.638427012816831230 ) ) ;
#8320 = CARTESIAN_POINT ( 'NONE',  ( 19.84674366389459266, 3.717264484334118713, -2.638427012816827677 ) ) ;
#8322 = EDGE_CURVE ( 'NONE', #8299, #93646, #58274, .T. ) ;
#8321 = CARTESIAN_POINT ( 'NONE',  ( 15.44008868035555260, 19.73035201082150536, 9.422509992056143702 ) ) ;
#8323 = CARTESIAN_POINT ( 'NONE',  ( 6.565887622018943937, 20.16530133659708213, 12.81628187352647430 ) ) ;
#8324 = CARTESIAN_POINT ( 'NONE',  ( 10.00000000000000178, 67.25893115100079456, 9.846743663894594434 ) ) ;
#8325 = CARTESIAN_POINT ( 'NONE',  ( 6.905507196108331414, -69.44000359822085500, -2.750000000000000000 ) ) ;
#8326 = CARTESIAN_POINT ( 'NONE',  ( 20.88017736071110519, 20.56368534415484106, 2.639326808657452039E-16 ) ) ;
#8327 = CARTESIAN_POINT ( 'NONE',  ( 10.00000000000000000, 49.75893115100078745, -9.846743663894594434 ) ) ;
#8328 = MECHANICAL_DESIGN_GEOMETRIC_PRESENTATION_REPRESENTATION (  '', ( #19531 ), #29079 ) ;
#8329 = CARTESIAN_POINT ( 'NONE',  ( 15.44008868035555793, 21.39701867748817321, -9.422509992056140149 ) ) ;
#8330 = CARTESIAN_POINT ( 'NONE',  ( 0.1532563361054100626, 5.800597817667451750, -2.638427012816831230 ) ) ;
#8331 = AXIS2_PLACEMENT_3D ( 'NONE', #40117, #17136, #87574 ) ;
#8332 = CARTESIAN_POINT ( 'NONE',  ( 10.00000000000000000, 31.81368534415483751, -10.88017736071110342 ) ) ;
#8334 = CARTESIAN_POINT ( 'NONE',  ( 9.876730923139286134, 14.49999999999999112, 11.28938378619072935 ) ) ;
#8333 = CARTESIAN_POINT ( 'NONE',  ( 19.42250999205614193, 5.147018677488171434, 5.440088680355555262 ) ) ;
#8335 =( NAMED_UNIT ( * ) SI_UNIT ( $, .STERADIAN. ) SOLID_ANGLE_UNIT ( ) );
#8336 = CARTESIAN_POINT ( 'NONE',  ( 19.84674366389459266, 28.71726448433411960, -2.638427012816827677 ) ) ;
#8337 = CARTESIAN_POINT ( 'NONE',  ( 16.40814093676323893, 10.79030133659708923, 11.09922568453595026 ) ) ;
#8338 = CARTESIAN_POINT ( 'NONE',  ( -10.19513985507817821, 15.00000000000000000, -11.00268709613231088 ) ) ;
#8339 = CARTESIAN_POINT ( 'NONE',  ( -8.922167142635602843, 75.09950301435408448, 2.900000000000000355 ) ) ;
#8340 = CARTESIAN_POINT ( 'NONE',  ( -9.543993260040148030, -28.01899697272886769, -4.000000000000000000 ) ) ;
#8341 = CARTESIAN_POINT ( 'NONE',  ( 6.204703633549690345, 12.84541550158063572, 14.16423886937410082 ) ) ;
#8342 = CARTESIAN_POINT ( 'NONE',  ( 18.52753015748618282, 33.92559781766745886, -4.923371831947291888 ) ) ;
#8343 = DIRECTION ( 'NONE',  ( 0.000000000000000000, 0.000000000000000000, 1.000000000000000000 ) ) ;
#8344 = EDGE_LOOP ( 'NONE', ( #17428, #66577, #67027, #73596 ) ) ;
#8345 = CARTESIAN_POINT ( 'NONE',  ( 10.00000000000000178, 48.05374883491396787, 14.16423886937410082 ) ) ;
#8346 = CARTESIAN_POINT ( 'NONE',  ( 12.63842701281683034, 22.46726448433411605, 9.846743663894596210 ) ) ;
#8348 = FACE_OUTER_BOUND ( 'NONE', #30508, .T. ) ;
#8347 = DIRECTION ( 'NONE',  ( 0.000000000000000000, 0.000000000000000000, 1.000000000000000000 ) ) ;
#8349 = CARTESIAN_POINT ( 'NONE',  ( -0.8801773607110991993, 47.85535201082150536, -2.915334737309923874 ) ) ;
#8350 = CARTESIAN_POINT ( 'NONE',  ( 0.6178305044545818747, 48.49863466993042493, -9.382169495545419124 ) ) ;
#8351 = CARTESIAN_POINT ( 'NONE',  ( -0.8801773607111009756, 18.06368534415484106, 1.068504757029289695E-15 ) ) ;
#8352 = CARTESIAN_POINT ( 'NONE',  ( 10.00000000000000178, 50.37363466993042493, 12.81628187352647608 ) ) ;
#8353 = CARTESIAN_POINT ( 'NONE',  ( -2.816281873526471635, -1.084698663402913210, -3.434112377981056508 ) ) ;
#8354 = CARTESIAN_POINT ( 'NONE',  ( 0.1532563361054100626, 5.800597817667452638, -2.638427012816831230 ) ) ;
#8355 = ORIENTED_EDGE ( 'NONE', *, *, #29891, .T. ) ;
#8356 = DIRECTION ( 'NONE',  ( 1.000000000000000000, -1.257568779154408793E-17, 0.000000000000000000 ) ) ;
#8357 = CARTESIAN_POINT ( 'NONE',  ( 0.000000000000000000, 10.49999999999999822, -6.500000000000000888 ) ) ;
#8358 = CARTESIAN_POINT ( 'NONE',  ( 20.36894250292379738, 59.92874883491397497, -10.36894250292379027 ) ) ;
#8359 = CARTESIAN_POINT ( 'NONE',  ( 24.16423886937410614, 14.51208216824730179, -3.795296366450302550 ) ) ;
#8360 = CARTESIAN_POINT ( 'NONE',  ( 10.00000000000000178, 24.31368534415484106, 10.88017736071110342 ) ) ;
#8361 = CARTESIAN_POINT ( 'NONE',  ( 4.559911319644449179, 38.89701867748817676, 9.422509992056141925 ) ) ;
#8362 = CARTESIAN_POINT ( 'NONE',  ( 8.879999999999995453, 40.74999999999999289, -4.250000000000000000 ) ) ;
#8363 = CARTESIAN_POINT ( 'NONE',  ( -0.5000000000000073275, 80.99999999999994316, 0.000000000000000000 ) ) ;
#8364 = CARTESIAN_POINT ( 'NONE',  ( 20.88017736071110875, 65.77201867748817676, -2.915334737309920765 ) ) ;
#8365 = CARTESIAN_POINT ( 'NONE',  ( 20.88017736071110875, 60.77201867748817676, -2.915334737309920765 ) ) ;
#8366 = CARTESIAN_POINT ( 'NONE',  ( 6.565887622018943937, 25.16530133659708213, 12.81628187352647430 ) ) ;
#8367 = CYLINDRICAL_SURFACE ( 'NONE', #74584, 0.5000000000000004441 ) ;
#8368 = DIRECTION ( 'NONE',  ( 0.000000000000000000, 0.000000000000000000, 1.000000000000000000 ) ) ;
#8369 = CARTESIAN_POINT ( 'NONE',  ( 14.92337183194729633, 7.675597817667451750, 8.527530157486181039 ) ) ;
#8370 = CARTESIAN_POINT ( 'NONE',  ( 14.92337183194729633, 42.67559781766745886, 8.527530157486181039 ) ) ;
#8371 = CARTESIAN_POINT ( 'NONE',  ( 19.42250999205614548, 10.98035201082150358, -5.440088680355545492 ) ) ;
#8372 = EDGE_CURVE ( 'NONE', #43197, #7097, #74450, .T. ) ;
#8373 = CARTESIAN_POINT ( 'NONE',  ( 0.6178305044545818747, 38.49863466993042493, -9.382169495545419124 ) ) ;
#8374 = CARTESIAN_POINT ( 'NONE',  ( 19.84674366389459621, 13.50893115100078568, 7.409399052514197653E-17 ) ) ;
#8376 = EDGE_CURVE ( 'NONE', #13186, #50694, #35965, .T. ) ;
#8375 = DIRECTION ( 'NONE',  ( 0.9975640502598243087, -0.06975647374412535795, 0.000000000000000000 ) ) ;
#8377 = ADVANCED_FACE ( 'NONE', ( #19979 ), #50971, .T. ) ;
#8378 = CARTESIAN_POINT ( 'NONE',  ( 17.20831665107776587, 57.88393115100078745, 7.208316651077764980 ) ) ;
#8380 = CARTESIAN_POINT ( 'NONE',  ( 20.36894250292379382, 3.678748834913967869, 10.36894250292379205 ) ) ;
#8379 = CARTESIAN_POINT ( 'NONE',  ( 0.1532563361054100626, 25.80059781766744820, -2.638427012816831230 ) ) ;
#8381 = CARTESIAN_POINT ( 'NONE',  ( -2.266590686148945544, 12.22041550158063394, 7.082119434687048631 ) ) ;
#8382 = CARTESIAN_POINT ( 'NONE',  ( 0.5774900079438590739, 32.64701867748816966, -5.440088680355550821 ) ) ;
#8383 = CARTESIAN_POINT ( 'NONE',  ( 15.44008868035555793, 6.397018677488170546, -9.422509992056140149 ) ) ;
#8384 = CARTESIAN_POINT ( 'NONE',  ( -0.8801773607111008646, 28.27201867748817321, 2.915334737309923430 ) ) ;
#8385 = CARTESIAN_POINT ( 'NONE',  ( 19.42250999205614193, 35.14701867748816966, 5.440088680355555262 ) ) ;
#8386 = ORIENTED_EDGE ( 'NONE', *, *, #78748, .T. ) ;
#8387 =( BOUNDED_SURFACE ( )  B_SPLINE_SURFACE ( 1, 2, ( 
 ( #38391, #54846, #22904, #15412, #46860, #69874, #14912, #68894, #45895, #14412, #67902, #7412, #54357, #37908, #422, #8380, #1394, #49316, #78840, #25848, #55853, #25368, #11322, #56345, #24871, #71354, #3838, #47346, #64794, #86348, #94819, #2873, #48336, #95313, #87319, #77849, #86839, #62848, #33322, #63817, #17851, #10351, #55353, #41363, #3339, #47840, #94327, #9358, #33801, #34297, #18344, #71830, #79333, #18836, #26815, #85360, #10842, #64308, #16872, #26322, #78343, #79820, #9864, #39863, #32345, #40363, #41841, #1887, #72307, #70864, #2379, #32834, #63336, #93841, #73298, #82276, #88307, #96323, #19805, #20309, #36794, #4822, #12793, #43293, #97310, #11813, #35296, #81779, #65789, #35797, #19321, #13294, #28783, #51789, #5318, #66284, #13793, #59280, #96819, #89295, #20805, #74273, #89780, #74783, #67288, #21297, #44279, #6292, #49805, #80313, #72794, #4332, #34803, #67787, #8269, #37789, #46745, #54244, #7289, #98808, #22786, #7785, #69268, #53760, #68287, #15777, #16262, #46266, #8747, #38280, #60760, #45775, #788, #52768, #91260, #53264, #83770, #31241, #68775, #14801, #98309, #90266, #15293, #84756, #76268, #305, #61256, #30749, #23284, #91761, #39267, #21799, #61736, #92254, #69755, #52281, #83276, #82779, #14299, #44770, #75275, #29763, #60271, #6786, #37299, #45273, #71233, #10238, #9244, #77732, #63218, #25255, #18228, #70252, #55740, #93721, #63706, #85742, #1768, #3228, #70750, #56709, #86231, #40240, #94209, #17742, #25739, #78728, #11207, #92740, #2264, #41240, #40730, #2758, #93225, #87200, #56231, #86725, #54728, #32224, #62725, #18723, #48709, #79212, #10722, #71717, #24750, #55228, #33693, #64191, #94710, #17255, #41726, #1284, #31737, #62233, #24264, #85249, #16754, #47229, #89667, #21178, #4713, #58674, #51680, #13173, #4214, #81180, #34684, #26696, #19204, #65178, #20686, #57191, #35175, #12681, #43180, #43670, #27184, #12188, #88182, #97201, #95701, #42695, #72678, #65676, #82159, #42212, #96198, #73174, #36176, #87689, #19696, #66167, #57687, #73668, #3725, #96700, #51180, #66676, #50183, #80693, #28669, #59161, #27682, #5195, #58167, #80190, #88678, #13671, #72196, #20186, #35683, #34186, #64678, #28179, #95188, #49686, #29653, #45162, #84648, #15183, #24152, #31630, #83665, #76160, #192, #84171, #54135, #31136, #45663, #61629, #92629, #23673, #85141, #15676, #7682, #23175, #16151, #68179, #38175, #68665, #30639, #46635, #46161, #91155, #75666, #6676, #38656, #47121, #61148, #98196, #8165, #53160, #62121, #54620, #76644, #7177, #77137, #30147, #37680, #98698, #16649, #60656, #22679 ),
 ( #69161, #37196, #8646, #67687, #39156, #91657, #69646, #685, #92148, #1170, #53652, #60162, #90658, #22184, #52665, #83167, #14692, #48110, #56125, #71128, #63115, #64575, #2655, #56609, #72091, #70144, #26589, #17642, #63602, #3130, #33107, #94107, #95084, #25152, #32617, #11107, #3615, #78126, #25635, #78624, #19097, #77621, #17151, #87098, #62612, #70634, #9636, #47630, #41626, #86620, #18131, #10135, #40630, #34084, #48603, #40134, #79107, #57091, #39652, #87585, #10619, #18612, #41131, #71619, #9136, #79604, #1665, #33590, #55115, #64085, #94600, #26117, #49101, #2162, #32114, #93119, #93617, #24646, #85633, #55629, #86129, #81560, #5590, #11593, #13067, #27078, #43076, #27573, #12578, #57579, #4605, #82058, #19587, #88075, #89566, #66568, #58068, #73562, #12084, #29049, #5086, #96091, #43559, #50085, #28067, #80088, #74057, #97097, #44053, #80589, #88571, #6074, #51572, #42589, #20583, #35573, #73069, #20075, #67063, #90053, #50580, #81075, #21074, #13566, #35066, #59061, #42112, #72574, #65565, #28568, #66064, #97589, #74558, #96592, #58564, #89069, #51068, #36575, #36067, #49578, #4107, #34571, #65067, #95593, #30530, #98587, #38059, #38548, #83054, #30036, #53035, #45543, #69043, #83, #7066, #90542, #21576, #91037, #46524, #76040, #60544, #53529, #7573, #15563, #68552, #1047, #14075, #22566, #61518, #68057, #83551, #14574, #77024, #91543, #15074, #75051, #22074, #52549, #8538, #61031, #76533, #23060, #84042, #29539, #98080, #46048, #8048, #577, #60044, #31022, #92028, #23558, #37566, #45041, #54027, #84538, #16035, #39039, #69533, #31514, #62013, #52064, #82559, #75550, #44555, #6560, #37070, #67568, #55000, #41009, #9017, #25029, #32992, #25521, #63968, #70519, #32503, #2042, #41510, #85518, #63001, #47994, #18008, #92513, #78991, #3023, #86983, #31996, #18988, #19958, #3992, #27947, #50453, #51448, #13444, #58439, #34457, #89447, #80470, #64948, #12459, #43931, #20462, #5956, #94970, #26472, #82930, #46408, #38426, #98953, #21449, #29914, #37941, #30409, #14946, #15917, #7929, #76896, #53408, #29418, #452, #7443, #45415, #45925, #6434, #30902, #98458, #60419, #91414, #97461, #36449, #6940, #75919, #22443, #21953, #23432, #52915, #76414, #91907, #28926, #84420, #75426, #83427, #22940, #68431, #53911, #66941, #14448, #90411, #59430, #51946, #67443, #82431, #37447, #13956, #44430, #97962, #59923, #52432, #44918, #39410, #46890, #71389, #1917, #47870, #77879, #47380, #33352, #78375, #77381, #62881, #25879, #69406, #86869, #9391, #17884, #93378, #70398, #18378, #10381, #927, #9896, #84900, #55388, #24905 ) ),
 .UNSPECIFIED., .F., .F., .F. ) 
 B_SPLINE_SURFACE_WITH_KNOTS ( ( 2, 2 ),
 ( 3, 2, 2, 2, 2, 2, 2, 2, 2, 2, 2, 2, 2, 2, 2, 2, 2, 2, 2, 2, 2, 2, 2, 2, 2, 2, 2, 2, 2, 2, 2, 2, 2, 2, 2, 2, 2, 2, 2, 2, 2, 2, 2, 2, 2, 2, 2, 2, 2, 2, 2, 2, 2, 2, 2, 2, 2, 2, 2, 2, 2, 2, 2, 2, 2, 2, 2, 2, 2, 2, 2, 2, 2, 2, 2, 2, 2, 2, 2, 2, 2, 2, 2, 2, 2, 2, 2, 2, 2, 2, 2, 2, 2, 2, 2, 2, 2, 2, 2, 2, 2, 2, 2, 2, 2, 2, 2, 2, 2, 2, 2, 2, 2, 2, 2, 2, 2, 2, 2, 2, 2, 2, 2, 2, 2, 2, 2, 2, 2, 2, 2, 2, 2, 2, 2, 2, 2, 2, 2, 2, 2, 2, 2, 2, 2, 2, 2, 2, 2, 2, 2, 2, 2, 2, 2, 2, 2, 2, 2, 2, 2, 2, 3 ),
 ( 0.000000000000000000, 1.000000000000000000 ),
 ( 0.000000000000000000, 0.005952380952380952051, 0.01190476190476190410, 0.01785714285714285615, 0.02380952380952380820, 0.02976190476190476025, 0.03571428571428571230, 0.04166666666666666435, 0.04761904761904761640, 0.05357142857142856845, 0.05952380952380952051, 0.06547619047619047949, 0.07142857142857142461, 0.07738095238095238360, 0.08333333333333332871, 0.08928571428571428770, 0.09523809523809523281, 0.1011904761904761918, 0.1071428571428571369, 0.1130952380952380959, 0.1190476190476190410, 0.1250000000000000000, 0.1309523809523809590, 0.1369047619047619180, 0.1428571428571428492, 0.1488095238095238082, 0.1547619047619047672, 0.1607142857142857262, 0.1666666666666666574, 0.1726190476190476164, 0.1785714285714285754, 0.1845238095238095344, 0.1904761904761904656, 0.1964285714285714246, 0.2023809523809523836, 0.2083333333333333426, 0.2142857142857142738, 0.2202380952380952328, 0.2261904761904761918, 0.2321428571428571508, 0.2380952380952380820, 0.2440476190476190410, 0.2500000000000000000, 0.2559523809523809312, 0.2619047619047619180, 0.2678571428571428492, 0.2738095238095238360, 0.2797619047619047672, 0.2857142857142856984, 0.2916666666666666852, 0.2976190476190476164, 0.3035714285714285476, 0.3095238095238095344, 0.3154761904761904656, 0.3214285714285714524, 0.3273809523809523836, 0.3333333333333333148, 0.3392857142857143016, 0.3452380952380952328, 0.3511904761904761640, 0.3571428571428571508, 0.3630952380952380820, 0.3690476190476190688, 0.3750000000000000000, 0.3809523809523809312, 0.3869047619047619180, 0.3928571428571428492, 0.3988095238095238360, 0.4047619047619047672, 0.4107142857142856984, 0.4166666666666666852, 0.4226190476190476164, 0.4285714285714285476, 0.4345238095238095344, 0.4404761904761904656, 0.4464285714285714524, 0.4523809523809523836, 0.4583333333333333148, 0.4642857142857143016, 0.4702380952380952328, 0.4761904761904761640, 0.4821428571428571508, 0.4880952380952380820, 0.4940476190476190688, 0.5000000000000000000, 0.5059523809523809312, 0.5119047619047618625, 0.5178571428571429047, 0.5238095238095238360, 0.5297619047619047672, 0.5357142857142856984, 0.5416666666666666297, 0.5476190476190476719, 0.5535714285714286031, 0.5595238095238095344, 0.5654761904761904656, 0.5714285714285713969, 0.5773809523809523281, 0.5833333333333333703, 0.5892857142857143016, 0.5952380952380952328, 0.6011904761904761640, 0.6071428571428570953, 0.6130952380952381375, 0.6190476190476190688, 0.6250000000000000000, 0.6309523809523809312, 0.6369047619047618625, 0.6428571428571429047, 0.6488095238095238360, 0.6547619047619047672, 0.6607142857142856984, 0.6666666666666666297, 0.6726190476190476719, 0.6785714285714286031, 0.6845238095238095344, 0.6904761904761904656, 0.6964285714285713969, 0.7023809523809523281, 0.7083333333333333703, 0.7142857142857143016, 0.7202380952380952328, 0.7261904761904761640, 0.7321428571428570953, 0.7380952380952381375, 0.7440476190476190688, 0.7500000000000000000, 0.7559523809523809312, 0.7619047619047618625, 0.7678571428571429047, 0.7738095238095238360, 0.7797619047619047672, 0.7857142857142856984, 0.7916666666666666297, 0.7976190476190476719, 0.8035714285714286031, 0.8095238095238095344, 0.8154761904761904656, 0.8214285714285713969, 0.8273809523809523281, 0.8333333333333333703, 0.8392857142857143016, 0.8452380952380952328, 0.8511904761904761640, 0.8571428571428570953, 0.8630952380952381375, 0.8690476190476190688, 0.8750000000000000000, 0.8809523809523809312, 0.8869047619047618625, 0.8928571428571429047, 0.8988095238095238360, 0.9047619047619047672, 0.9107142857142856984, 0.9166666666666666297, 0.9226190476190476719, 0.9285714285714286031, 0.9345238095238095344, 0.9404761904761904656, 0.9464285714285713969, 0.9523809523809523281, 0.9583333333333333703, 0.9642857142857143016 ),
 .UNSPECIFIED. ) 
 GEOMETRIC_REPRESENTATION_ITEM ( )  RATIONAL_B_SPLINE_SURFACE ( (
 ( 1.000000000000000000, 0.9659258262890683122, 1.000000000000000000, 0.9659258262890683122, 1.000000000000000000, 0.9659258262890683122, 1.000000000000000000, 0.9659258262890683122, 1.000000000000000000, 0.9659258262890683122, 1.000000000000000000, 0.9659258262890683122, 1.000000000000000000, 0.9659258262890683122, 1.000000000000000000, 0.9659258262890683122, 1.000000000000000000, 0.9659258262890683122, 1.000000000000000000, 0.9659258262890683122, 1.000000000000000000, 0.9659258262890683122, 1.000000000000000000, 0.9659258262890683122, 1.000000000000000000, 0.9659258262890683122, 1.000000000000000000, 0.9659258262890683122, 1.000000000000000000, 0.9659258262890683122, 1.000000000000000000, 0.9659258262890683122, 1.000000000000000000, 0.9659258262890683122, 1.000000000000000000, 0.9659258262890683122, 1.000000000000000000, 0.9659258262890683122, 1.000000000000000000, 0.9659258262890683122, 1.000000000000000000, 0.9659258262890683122, 1.000000000000000000, 0.9659258262890683122, 1.000000000000000000, 0.9659258262890683122, 1.000000000000000000, 0.9659258262890683122, 1.000000000000000000, 0.9659258262890683122, 1.000000000000000000, 0.9659258262890683122, 1.000000000000000000, 0.9659258262890683122, 1.000000000000000000, 0.9659258262890683122, 1.000000000000000000, 0.9659258262890683122, 1.000000000000000000, 0.9659258262890683122, 1.000000000000000000, 0.9659258262890683122, 1.000000000000000000, 0.9659258262890683122, 1.000000000000000000, 0.9659258262890683122, 1.000000000000000000, 0.9659258262890683122, 1.000000000000000000, 0.9659258262890683122, 1.000000000000000000, 0.9659258262890683122, 1.000000000000000000, 0.9659258262890683122, 1.000000000000000000, 0.9659258262890683122, 1.000000000000000000, 0.9659258262890683122, 1.000000000000000000, 0.9659258262890683122, 1.000000000000000000, 0.9659258262890683122, 1.000000000000000000, 0.9659258262890683122, 1.000000000000000000, 0.9659258262890683122, 1.000000000000000000, 0.9659258262890683122, 1.000000000000000000, 0.9659258262890683122, 1.000000000000000000, 0.9659258262890683122, 1.000000000000000000, 0.9659258262890683122, 1.000000000000000000, 0.9659258262890683122, 1.000000000000000000, 0.9659258262890683122, 1.000000000000000000, 0.9659258262890683122, 1.000000000000000000, 0.9659258262890683122, 1.000000000000000000, 0.9659258262890683122, 1.000000000000000000, 0.9659258262890683122, 1.000000000000000000, 0.9659258262890683122, 1.000000000000000000, 0.9659258262890683122, 1.000000000000000000, 0.9659258262890683122, 1.000000000000000000, 0.9659258262890683122, 1.000000000000000000, 0.9659258262890683122, 1.000000000000000000, 0.9659258262890683122, 1.000000000000000000, 0.9659258262890683122, 1.000000000000000000, 0.9659258262890683122, 1.000000000000000000, 0.9659258262890683122, 1.000000000000000000, 0.9659258262890683122, 1.000000000000000000, 0.9659258262890683122, 1.000000000000000000, 0.9659258262890683122, 1.000000000000000000, 0.9659258262890683122, 1.000000000000000000, 0.9659258262890683122, 1.000000000000000000, 0.9659258262890683122, 1.000000000000000000, 0.9659258262890683122, 1.000000000000000000, 0.9659258262890683122, 1.000000000000000000, 0.9659258262890683122, 1.000000000000000000, 0.9659258262890683122, 1.000000000000000000, 0.9659258262890683122, 1.000000000000000000, 0.9659258262890683122, 1.000000000000000000, 0.9659258262890683122, 1.000000000000000000, 0.9659258262890683122, 1.000000000000000000, 0.9659258262890683122, 1.000000000000000000, 0.9659258262890683122, 1.000000000000000000, 0.9659258262890683122, 1.000000000000000000, 0.9659258262890683122, 1.000000000000000000, 0.9659258262890683122, 1.000000000000000000, 0.9659258262890683122, 1.000000000000000000, 0.9659258262890683122, 1.000000000000000000, 0.9659258262890683122, 1.000000000000000000, 0.9659258262890683122, 1.000000000000000000, 0.9659258262890683122, 1.000000000000000000, 0.9659258262890683122, 1.000000000000000000, 0.9659258262890683122, 1.000000000000000000, 0.9659258262890683122, 1.000000000000000000, 0.9659258262890683122, 1.000000000000000000, 0.9659258262890683122, 1.000000000000000000, 0.9659258262890683122, 1.000000000000000000, 0.9659258262890683122, 1.000000000000000000, 0.9659258262890683122, 1.000000000000000000, 0.9659258262890683122, 1.000000000000000000, 0.9659258262890683122, 1.000000000000000000, 0.9659258262890683122, 1.000000000000000000, 0.9659258262890683122, 1.000000000000000000, 0.9659258262890683122, 1.000000000000000000, 0.9659258262890683122, 1.000000000000000000, 0.9659258262890683122, 1.000000000000000000, 0.9659258262890683122, 1.000000000000000000, 0.9659258262890683122, 1.000000000000000000, 0.9659258262890683122, 1.000000000000000000, 0.9659258262890683122, 1.000000000000000000, 0.9659258262890683122, 1.000000000000000000, 0.9659258262890683122, 1.000000000000000000, 0.9659258262890683122, 1.000000000000000000, 0.9659258262890683122, 1.000000000000000000, 0.9659258262890683122, 1.000000000000000000, 0.9659258262890683122, 1.000000000000000000, 0.9659258262890683122, 1.000000000000000000, 0.9659258262890683122, 1.000000000000000000, 0.9659258262890683122, 1.000000000000000000, 0.9659258262890683122, 1.000000000000000000, 0.9659258262890683122, 1.000000000000000000, 0.9659258262890683122, 1.000000000000000000, 0.9659258262890683122, 1.000000000000000000, 0.9659258262890683122, 1.000000000000000000, 0.9659258262890683122, 1.000000000000000000, 0.9659258262890683122, 1.000000000000000000, 0.9659258262890683122, 1.000000000000000000, 0.9659258262890683122, 1.000000000000000000, 0.9659258262890683122, 1.000000000000000000, 0.9659258262890683122, 1.000000000000000000, 0.9659258262890683122, 1.000000000000000000, 0.9659258262890683122, 1.000000000000000000, 0.9659258262890683122, 1.000000000000000000, 0.9659258262890683122, 1.000000000000000000, 0.9659258262890683122, 1.000000000000000000, 0.9659258262890683122, 1.000000000000000000, 0.9659258262890683122, 1.000000000000000000, 0.9659258262890683122, 1.000000000000000000, 0.9659258262890683122, 1.000000000000000000, 0.9659258262890683122, 1.000000000000000000, 0.9659258262890683122, 1.000000000000000000, 0.9659258262890683122, 1.000000000000000000, 0.9659258262890683122, 1.000000000000000000, 0.9659258262890683122, 1.000000000000000000, 0.9659258262890683122, 1.000000000000000000, 0.9659258262890683122, 1.000000000000000000, 0.9659258262890683122, 1.000000000000000000, 0.9659258262890683122, 1.000000000000000000, 0.9659258262890683122, 1.000000000000000000, 0.9659258262890683122, 1.000000000000000000, 0.9659258262890683122, 1.000000000000000000, 0.9659258262890683122, 1.000000000000000000, 0.9659258262890683122, 1.000000000000000000, 0.9659258262890683122, 1.000000000000000000, 0.9659258262890683122, 1.000000000000000000, 0.9659258262890683122, 1.000000000000000000, 0.9659258262890683122, 1.000000000000000000, 0.9659258262890683122, 1.000000000000000000, 0.9659258262890683122, 1.000000000000000000, 0.9659258262890683122, 1.000000000000000000, 0.9659258262890683122, 1.000000000000000000, 0.9659258262890683122, 1.000000000000000000, 0.9659258262890683122, 1.000000000000000000, 0.9659258262890683122, 1.000000000000000000, 0.9659258262890683122, 1.000000000000000000, 0.9659258262890683122, 1.000000000000000000, 0.9659258262890683122, 1.000000000000000000),
 ( 1.000000000000000000, 0.9659258262890683122, 1.000000000000000000, 0.9659258262890683122, 1.000000000000000000, 0.9659258262890683122, 1.000000000000000000, 0.9659258262890683122, 1.000000000000000000, 0.9659258262890683122, 1.000000000000000000, 0.9659258262890683122, 1.000000000000000000, 0.9659258262890683122, 1.000000000000000000, 0.9659258262890683122, 1.000000000000000000, 0.9659258262890683122, 1.000000000000000000, 0.9659258262890683122, 1.000000000000000000, 0.9659258262890683122, 1.000000000000000000, 0.9659258262890683122, 1.000000000000000000, 0.9659258262890683122, 1.000000000000000000, 0.9659258262890683122, 1.000000000000000000, 0.9659258262890683122, 1.000000000000000000, 0.9659258262890683122, 1.000000000000000000, 0.9659258262890683122, 1.000000000000000000, 0.9659258262890683122, 1.000000000000000000, 0.9659258262890683122, 1.000000000000000000, 0.9659258262890683122, 1.000000000000000000, 0.9659258262890683122, 1.000000000000000000, 0.9659258262890683122, 1.000000000000000000, 0.9659258262890683122, 1.000000000000000000, 0.9659258262890683122, 1.000000000000000000, 0.9659258262890683122, 1.000000000000000000, 0.9659258262890683122, 1.000000000000000000, 0.9659258262890683122, 1.000000000000000000, 0.9659258262890683122, 1.000000000000000000, 0.9659258262890683122, 1.000000000000000000, 0.9659258262890683122, 1.000000000000000000, 0.9659258262890683122, 1.000000000000000000, 0.9659258262890683122, 1.000000000000000000, 0.9659258262890683122, 1.000000000000000000, 0.9659258262890683122, 1.000000000000000000, 0.9659258262890683122, 1.000000000000000000, 0.9659258262890683122, 1.000000000000000000, 0.9659258262890683122, 1.000000000000000000, 0.9659258262890683122, 1.000000000000000000, 0.9659258262890683122, 1.000000000000000000, 0.9659258262890683122, 1.000000000000000000, 0.9659258262890683122, 1.000000000000000000, 0.9659258262890683122, 1.000000000000000000, 0.9659258262890683122, 1.000000000000000000, 0.9659258262890683122, 1.000000000000000000, 0.9659258262890683122, 1.000000000000000000, 0.9659258262890683122, 1.000000000000000000, 0.9659258262890683122, 1.000000000000000000, 0.9659258262890683122, 1.000000000000000000, 0.9659258262890683122, 1.000000000000000000, 0.9659258262890683122, 1.000000000000000000, 0.9659258262890683122, 1.000000000000000000, 0.9659258262890683122, 1.000000000000000000, 0.9659258262890683122, 1.000000000000000000, 0.9659258262890683122, 1.000000000000000000, 0.9659258262890683122, 1.000000000000000000, 0.9659258262890683122, 1.000000000000000000, 0.9659258262890683122, 1.000000000000000000, 0.9659258262890683122, 1.000000000000000000, 0.9659258262890683122, 1.000000000000000000, 0.9659258262890683122, 1.000000000000000000, 0.9659258262890683122, 1.000000000000000000, 0.9659258262890683122, 1.000000000000000000, 0.9659258262890683122, 1.000000000000000000, 0.9659258262890683122, 1.000000000000000000, 0.9659258262890683122, 1.000000000000000000, 0.9659258262890683122, 1.000000000000000000, 0.9659258262890683122, 1.000000000000000000, 0.9659258262890683122, 1.000000000000000000, 0.9659258262890683122, 1.000000000000000000, 0.9659258262890683122, 1.000000000000000000, 0.9659258262890683122, 1.000000000000000000, 0.9659258262890683122, 1.000000000000000000, 0.9659258262890683122, 1.000000000000000000, 0.9659258262890683122, 1.000000000000000000, 0.9659258262890683122, 1.000000000000000000, 0.9659258262890683122, 1.000000000000000000, 0.9659258262890683122, 1.000000000000000000, 0.9659258262890683122, 1.000000000000000000, 0.9659258262890683122, 1.000000000000000000, 0.9659258262890683122, 1.000000000000000000, 0.9659258262890683122, 1.000000000000000000, 0.9659258262890683122, 1.000000000000000000, 0.9659258262890683122, 1.000000000000000000, 0.9659258262890683122, 1.000000000000000000, 0.9659258262890683122, 1.000000000000000000, 0.9659258262890683122, 1.000000000000000000, 0.9659258262890683122, 1.000000000000000000, 0.9659258262890683122, 1.000000000000000000, 0.9659258262890683122, 1.000000000000000000, 0.9659258262890683122, 1.000000000000000000, 0.9659258262890683122, 1.000000000000000000, 0.9659258262890683122, 1.000000000000000000, 0.9659258262890683122, 1.000000000000000000, 0.9659258262890683122, 1.000000000000000000, 0.9659258262890683122, 1.000000000000000000, 0.9659258262890683122, 1.000000000000000000, 0.9659258262890683122, 1.000000000000000000, 0.9659258262890683122, 1.000000000000000000, 0.9659258262890683122, 1.000000000000000000, 0.9659258262890683122, 1.000000000000000000, 0.9659258262890683122, 1.000000000000000000, 0.9659258262890683122, 1.000000000000000000, 0.9659258262890683122, 1.000000000000000000, 0.9659258262890683122, 1.000000000000000000, 0.9659258262890683122, 1.000000000000000000, 0.9659258262890683122, 1.000000000000000000, 0.9659258262890683122, 1.000000000000000000, 0.9659258262890683122, 1.000000000000000000, 0.9659258262890683122, 1.000000000000000000, 0.9659258262890683122, 1.000000000000000000, 0.9659258262890683122, 1.000000000000000000, 0.9659258262890683122, 1.000000000000000000, 0.9659258262890683122, 1.000000000000000000, 0.9659258262890683122, 1.000000000000000000, 0.9659258262890683122, 1.000000000000000000, 0.9659258262890683122, 1.000000000000000000, 0.9659258262890683122, 1.000000000000000000, 0.9659258262890683122, 1.000000000000000000, 0.9659258262890683122, 1.000000000000000000, 0.9659258262890683122, 1.000000000000000000, 0.9659258262890683122, 1.000000000000000000, 0.9659258262890683122, 1.000000000000000000, 0.9659258262890683122, 1.000000000000000000, 0.9659258262890683122, 1.000000000000000000, 0.9659258262890683122, 1.000000000000000000, 0.9659258262890683122, 1.000000000000000000, 0.9659258262890683122, 1.000000000000000000, 0.9659258262890683122, 1.000000000000000000, 0.9659258262890683122, 1.000000000000000000, 0.9659258262890683122, 1.000000000000000000, 0.9659258262890683122, 1.000000000000000000, 0.9659258262890683122, 1.000000000000000000, 0.9659258262890683122, 1.000000000000000000, 0.9659258262890683122, 1.000000000000000000, 0.9659258262890683122, 1.000000000000000000, 0.9659258262890683122, 1.000000000000000000, 0.9659258262890683122, 1.000000000000000000, 0.9659258262890683122, 1.000000000000000000, 0.9659258262890683122, 1.000000000000000000, 0.9659258262890683122, 1.000000000000000000, 0.9659258262890683122, 1.000000000000000000, 0.9659258262890683122, 1.000000000000000000, 0.9659258262890683122, 1.000000000000000000, 0.9659258262890683122, 1.000000000000000000, 0.9659258262890683122, 1.000000000000000000, 0.9659258262890683122, 1.000000000000000000, 0.9659258262890683122, 1.000000000000000000, 0.9659258262890683122, 1.000000000000000000, 0.9659258262890683122, 1.000000000000000000, 0.9659258262890683122, 1.000000000000000000, 0.9659258262890683122, 1.000000000000000000, 0.9659258262890683122, 1.000000000000000000, 0.9659258262890683122, 1.000000000000000000, 0.9659258262890683122, 1.000000000000000000, 0.9659258262890683122, 1.000000000000000000, 0.9659258262890683122, 1.000000000000000000, 0.9659258262890683122, 1.000000000000000000, 0.9659258262890683122, 1.000000000000000000, 0.9659258262890683122, 1.000000000000000000, 0.9659258262890683122, 1.000000000000000000, 0.9659258262890683122, 1.000000000000000000, 0.9659258262890683122, 1.000000000000000000) ) ) 
 REPRESENTATION_ITEM ( '' )  SURFACE ( )  );
#8388 = CARTESIAN_POINT ( 'NONE',  ( 19.42250999205614193, 35.14701867748816966, 5.440088680355555262 ) ) ;
#8389 = EDGE_LOOP ( 'NONE', ( #87511, #90186, #92006, #53340 ) ) ;
#8390 = CARTESIAN_POINT ( 'NONE',  ( 13.43411237798106583, 57.66530133659708923, -12.81628187352647252 ) ) ;
#8391 = CARTESIAN_POINT ( 'NONE',  ( -0.8801773607111008646, 48.27201867748816966, 2.915334737309923430 ) ) ;
#8392 = AXIS2_PLACEMENT_3D ( 'NONE', #51612, #73601, #5126 ) ;
#8393 = ORIENTED_EDGE ( 'NONE', *, *, #26467, .F. ) ;
#8394 = CARTESIAN_POINT ( 'NONE',  ( 15.44008868035555793, 51.39701867748816966, -9.422509992056140149 ) ) ;
#8395 = CARTESIAN_POINT ( 'NONE',  ( 6.905642986249669768, -69.45547628558871622, 3.999999999999999556 ) ) ;
#8396 = CARTESIAN_POINT ( 'NONE',  ( -14.04391541078760675, 15.00000000000000000, -3.608107528143027043 ) ) ;
#8397 = CARTESIAN_POINT ( 'NONE',  ( -0.3689425029237881626, 57.42874883491397497, 10.36894250292379027 ) ) ;
#8398 = CARTESIAN_POINT ( 'NONE',  ( -0.8801773607111008646, 63.27201867748817676, 2.915334737309923430 ) ) ;
#8399 = CYLINDRICAL_SURFACE ( 'NONE', #76977, 0.2500000000000002220 ) ;
#8400 = CARTESIAN_POINT ( 'NONE',  ( 0.000000000000000000, 14.49999999999999822, 0.000000000000000000 ) ) ;
#8401 = AXIS2_PLACEMENT_3D ( 'NONE', #87395, #9933, #41433 ) ;
#8402 = CARTESIAN_POINT ( 'NONE',  ( 19.84674366389459266, 33.30059781766744464, 2.638427012816836559 ) ) ;
#8403 = ORIENTED_EDGE ( 'NONE', *, *, #62283, .T. ) ;
#8404 = ADVANCED_FACE ( 'NONE', ( #36470 ), #65968, .F. ) ;
#8405 = AXIS2_PLACEMENT_3D ( 'NONE', #50883, #21375, #29843 ) ;
#8406 = CARTESIAN_POINT ( 'NONE',  ( 10.00000000000000178, 37.25893115100078745, 9.846743663894594434 ) ) ;
#8407 = CARTESIAN_POINT ( 'NONE',  ( 20.88017736071110875, 35.77201867748816966, -2.915334737309920765 ) ) ;
#8408 = CARTESIAN_POINT ( 'NONE',  ( 14.92337183194729633, 42.67559781766745886, 8.527530157486181039 ) ) ;
#8409 = CARTESIAN_POINT ( 'NONE',  ( -2.816281873526473856, 19.33196800326375708, 3.434112377981055619 ) ) ;
#8411 = CARTESIAN_POINT ( 'NONE',  ( -12.34086200392831678, 15.00000000000000000, 7.124999999999885425 ) ) ;
#8410 = CARTESIAN_POINT ( 'NONE',  ( 19.88565890683628723, 2.716910754863021804, -6.480892540919843903 ) ) ;
#8413 = CARTESIAN_POINT ( 'NONE',  ( 20.88017736071110164, 5.355352010821502695, 2.915334737309930979 ) ) ;
#8412 = CARTESIAN_POINT ( 'NONE',  ( 12.91533473730993009, 51.60535201082149825, -10.88017736071109987 ) ) ;
#8414 = CARTESIAN_POINT ( 'NONE',  ( 10.00000000000000178, 58.05374883491397497, 14.16423886937410082 ) ) ;
#8415 = MECHANICAL_DESIGN_GEOMETRIC_PRESENTATION_REPRESENTATION (  '', ( #54644 ), #457 ) ;
#8416 = CARTESIAN_POINT ( 'NONE',  ( 3.591859063236761518, 24.95696800326375353, 11.09922568453594849 ) ) ;
#8417 = CARTESIAN_POINT ( 'NONE',  ( 19.72487221294570858, 70.00000000000000000, 6.500000000000000888 ) ) ;
#8418 = ORIENTED_EDGE ( 'NONE', *, *, #70327, .F. ) ;
#8419 = CARTESIAN_POINT ( 'NONE',  ( 6.565887622018943937, 15.16530133659708568, 12.81628187352647430 ) ) ;
#8420 = CARTESIAN_POINT ( 'NONE',  ( 20.88017736071110875, 25.77201867748816966, -2.915334737309920765 ) ) ;
#8421 = CARTESIAN_POINT ( 'NONE',  ( 12.91533473730993009, 66.60535201082150536, -10.88017736071109987 ) ) ;
#8422 = ORIENTED_EDGE ( 'NONE', *, *, #311, .F. ) ;
#8423 = AXIS2_PLACEMENT_3D ( 'NONE', #66964, #49986, #12480 ) ;
#8424 = CARTESIAN_POINT ( 'NONE',  ( 15.44008868035555260, 64.73035201082151957, 9.422509992056143702 ) ) ;
#8425 = CARTESIAN_POINT ( 'NONE',  ( 7.361572987183170547, 47.05059781766745175, 9.846743663894590881 ) ) ;
#8426 = CARTESIAN_POINT ( 'NONE',  ( 7.361572987183170547, 32.05059781766745175, 9.846743663894590881 ) ) ;
#8427 = CARTESIAN_POINT ( 'NONE',  ( 8.879999999999995453, 41.24999999999999289, 4.000000000000000000 ) ) ;
#8428 = CARTESIAN_POINT ( 'NONE',  ( 5.076628168052704559, 30.17559781766745175, -8.527530157486179263 ) ) ;
#8429 = CYLINDRICAL_SURFACE ( 'NONE', #60422, 0.5000000000000004441 ) ;
#8430 = DIRECTION ( 'NONE',  ( 1.000000000000000000, 0.000000000000000000, -0.000000000000000000 ) ) ;
#8432 = CARTESIAN_POINT ( 'NONE',  ( -14.48718990079891888, 15.00000000000000000, -0.6093675230842395818 ) ) ;
#8431 = CARTESIAN_POINT ( 'NONE',  ( 2.791683348922237240, 15.38393115100078212, -7.208316651077763204 ) ) ;
#8433 = CARTESIAN_POINT ( 'NONE',  ( 8.880000000000000782, 1.019547802438458550, 3.750000000000000000 ) ) ;
#8435 = VERTEX_POINT ( 'NONE', #42983 ) ;
#8434 = CARTESIAN_POINT ( 'NONE',  ( 2.791683348922237240, 45.38393115100079456, -7.208316651077763204 ) ) ;
#8436 = AXIS2_PLACEMENT_3D ( 'NONE', #34839, #28334, #20842 ) ;
#8437 = CARTESIAN_POINT ( 'NONE',  ( 3.014428414850129911, 3.659700295649314761, -11.25000000000000000 ) ) ;
#8438 = CARTESIAN_POINT ( 'NONE',  ( 0.6178305044545818747, 18.49863466993041428, -9.382169495545419124 ) ) ;
#8439 = CARTESIAN_POINT ( 'NONE',  ( 17.96484262340118221, 54.93868534415484106, 7.964842623401181321 ) ) ;
#8440 = CARTESIAN_POINT ( 'NONE',  ( -4.164238869374099039, 36.80374883491396787, 8.674139862899312516E-16 ) ) ;
#8441 = CARTESIAN_POINT ( 'NONE',  ( 17.75000000000000711, 43.00000000000000000, -6.500000000000000888 ) ) ;
#8442 = CARTESIAN_POINT ( 'NONE',  ( 20.36894250292379738, 39.92874883491396787, -10.36894250292379027 ) ) ;
#8443 = CARTESIAN_POINT ( 'NONE',  ( 17.08211943468705840, 55.13708216824731068, -12.26659068614894466 ) ) ;
#8444 = CARTESIAN_POINT ( 'NONE',  ( 24.16423886937410614, 24.30374883491396787, 8.672049930838204340E-16 ) ) ;
#8446 = CARTESIAN_POINT ( 'NONE',  ( -0.1503990784575280903, 38.10158574516643171, 6.262539305110076171 ) ) ;
#8445 = CARTESIAN_POINT ( 'NONE',  ( 24.16423886937409904, 24.09541550158063927, 3.795296366450317205 ) ) ;
#8447 = CARTESIAN_POINT ( 'NONE',  ( -3.014428414850141458, 9.076366962315983500, -11.25000000000000000 ) ) ;
#8449 = CARTESIAN_POINT ( 'NONE',  ( 7.361572987183169658, 39.96726448433411605, -9.846743663894592657 ) ) ;
#8448 = LINE ( 'NONE', #16450, #83630 ) ;
#8450 = ORIENTED_EDGE ( 'NONE', *, *, #84364, .F. ) ;
#8451 = CARTESIAN_POINT ( 'NONE',  ( -0.8801773607111008646, 23.27201867748817676, 2.915334737309923430 ) ) ;
#8452 = DIRECTION ( 'NONE',  ( -0.3826834323650877834, 0.000000000000000000, -0.9238795325112876267 ) ) ;
#8453 = CARTESIAN_POINT ( 'NONE',  ( 7.361572987183169658, 64.96726448433412315, -9.846743663894592657 ) ) ;
#8454 = ADVANCED_FACE ( 'NONE', ( #72977 ), #5225, .T. ) ;
#8455 = CARTESIAN_POINT ( 'NONE',  ( 19.67853978997394293, 88.18036594423148244, -5.461515559775651063 ) ) ;
#8456 = CARTESIAN_POINT ( 'NONE',  ( 0.1532563361054100626, 45.80059781766745886, -2.638427012816831230 ) ) ;
#8457 = CARTESIAN_POINT ( 'NONE',  ( -1.099225684535947600, 49.54030133659708923, 6.408140936763237150 ) ) ;
#8458 = CARTESIAN_POINT ( 'NONE',  ( -3.795296366450300773, -12.15458449841936250, 14.16423886937410437 ) ) ;
#8459 = MECHANICAL_DESIGN_GEOMETRIC_PRESENTATION_REPRESENTATION (  '', ( #85112 ), #49989 ) ;
#8460 = CARTESIAN_POINT ( 'NONE',  ( 5.076628168052703671, 36.84226448433412315, 8.527530157486179263 ) ) ;
#8461 = CARTESIAN_POINT ( 'NONE',  ( 18.52753015748618282, 48.92559781766745886, -4.923371831947291888 ) ) ;
#8462 = CARTESIAN_POINT ( 'NONE',  ( 22.26659068614894466, 43.88708216824729647, 7.082119434687054849 ) ) ;
#8463 = ORIENTED_EDGE ( 'NONE', *, *, #88174, .T. ) ;
#8464 = CARTESIAN_POINT ( 'NONE',  ( -4.164238869374099927, 17.01208216824730357, 3.795296366450308767 ) ) ;
#8465 = CARTESIAN_POINT ( 'NONE',  ( 15.44008868035555260, 64.73035201082151957, 9.422509992056143702 ) ) ;
#8466 = CARTESIAN_POINT ( 'NONE',  ( -3.999999999999994671, 43.00000000000000711, 6.250000000000000000 ) ) ;
#8467 = CARTESIAN_POINT ( 'NONE',  ( -0.8801773607111008646, 3.272018677488171434, 2.915334737309923430 ) ) ;
#8468 = CARTESIAN_POINT ( 'NONE',  ( -1.099225684535947600, 14.54030133659708568, 6.408140936763237150 ) ) ;
#8469 = AXIS2_PLACEMENT_3D ( 'NONE', #97882, #44349, #6354 ) ;
#8470 = CARTESIAN_POINT ( 'NONE',  ( 20.24186590665274821, 1.760286857231739610, 6.114288769123088052 ) ) ;
#8471 = CARTESIAN_POINT ( 'NONE',  ( 18.52753015748618282, 3.925597817667451306, -4.923371831947291888 ) ) ;
#8472 =( GEOMETRIC_REPRESENTATION_CONTEXT ( 3 ) GLOBAL_UNCERTAINTY_ASSIGNED_CONTEXT ( ( #95505 ) ) GLOBAL_UNIT_ASSIGNED_CONTEXT ( ( #47072, #92092, #9085 ) ) REPRESENTATION_CONTEXT ( 'NONE', 'WORKASPACE' ) );
#8473 =( NAMED_UNIT ( * ) SI_UNIT ( $, .STERADIAN. ) SOLID_ANGLE_UNIT ( ) );
#8474 = LINE ( 'NONE', #38980, #65951 ) ;
#8475 = DIRECTION ( 'NONE',  ( -1.000000000000000000, 0.000000000000000000, 0.000000000000000000 ) ) ;
#8476 = CARTESIAN_POINT ( 'NONE',  ( 13.79529636645031943, 65.34541550158063217, -14.16423886937409904 ) ) ;
#8477 = LINE ( 'NONE', #32935, #27224 ) ;
#8478 = CARTESIAN_POINT ( 'NONE',  ( 15.44008868035555260, 24.73035201082150891, 9.422509992056143702 ) ) ;
#8480 = MECHANICAL_DESIGN_GEOMETRIC_PRESENTATION_REPRESENTATION (  '', ( #77132 ), #34003 ) ;
#8479 = CARTESIAN_POINT ( 'NONE',  ( 17.96484262340118221, 26.18868534415483396, -7.964842623401177768 ) ) ;
#8481 = CARTESIAN_POINT ( 'NONE',  ( 0.1532563361054082862, 56.21726448433411605, 2.638427012816831674 ) ) ;
#8482 = CARTESIAN_POINT ( 'NONE',  ( 14.92337183194729633, 52.67559781766745175, 8.527530157486181039 ) ) ;
#8483 = CARTESIAN_POINT ( 'NONE',  ( -2.816281873526473856, 59.33196800326374643, 3.434112377981055619 ) ) ;
#8484 = CARTESIAN_POINT ( 'NONE',  ( 17.20831665107776587, 2.883931151000785231, 7.208316651077764980 ) ) ;
#8485 = EDGE_CURVE ( 'NONE', #50974, #88806, #26987, .T. ) ;
#8486 = ORIENTED_EDGE ( 'NONE', *, *, #70639, .F. ) ;
#8487 = CARTESIAN_POINT ( 'NONE',  ( 7.084665262690076126, 22.02201867748817321, -10.88017736071110164 ) ) ;
#8488 = CARTESIAN_POINT ( 'NONE',  ( -2.816281873526473856, 19.33196800326375708, 3.434112377981055619 ) ) ;
#8489 = LINE ( 'NONE', #68996, #72048 ) ;
#8490 = EDGE_CURVE ( 'NONE', #83825, #875, #97483, .T. ) ;
#8491 = CARTESIAN_POINT ( 'NONE',  ( 5.076628168052703671, 66.84226448433412315, 8.527530157486179263 ) ) ;
#8492 = CARTESIAN_POINT ( 'NONE',  ( 17.96484262340118221, 51.18868534415483396, -7.964842623401177768 ) ) ;
#8493 = EDGE_CURVE ( 'NONE', #75199, #87279, #49875, .T. ) ;
#8494 = CARTESIAN_POINT ( 'NONE',  ( -2.816281873526473856, 24.33196800326375353, 3.434112377981055619 ) ) ;
#8496 = CARTESIAN_POINT ( 'NONE',  ( 0.000000000000000000, 15.00000000000000000, 0.000000000000000000 ) ) ;
#8495 = CARTESIAN_POINT ( 'NONE',  ( 0.5774900079438607392, 58.48035201082151247, 5.440088680355550821 ) ) ;
#8497 =( BOUNDED_CURVE ( )  B_SPLINE_CURVE ( 2, ( #81723, #27739, #36740, #29220, #89238, #50239, #43731, #57743, #88246, #88742, #59220, #73732, #66228 ),
 .UNSPECIFIED., .F., .T. ) 
 B_SPLINE_CURVE_WITH_KNOTS ( ( 3, 2, 2, 2, 2, 2, 3 ),
 ( 0.5999999999999999778, 0.6055555555555555136, 0.6111111111111111605, 0.6166666666666666963, 0.6222222222222222321, 0.6277777777777777679, 0.6333333333333333037 ),
 .UNSPECIFIED. ) 
 CURVE ( )  GEOMETRIC_REPRESENTATION_ITEM ( )  RATIONAL_B_SPLINE_CURVE ( ( 1.000000000000000000, 0.9659258262890684232, 1.000000000000000000, 0.9659258262890684232, 1.000000000000000000, 0.9659258262890684232, 1.000000000000000000, 0.9659258262890684232, 1.000000000000000000, 0.9659258262890684232, 1.000000000000000000, 0.9659258262890684232, 1.000000000000000000 ) ) 
 REPRESENTATION_ITEM ( '' )  );
#8498 = CARTESIAN_POINT ( 'NONE',  ( -4.000000000000000000, 10.25000000000000000, -4.000000000000000000 ) ) ;
#8499 = ORIENTED_EDGE ( 'NONE', *, *, #48768, .F. ) ;
#8500 = DIRECTION ( 'NONE',  ( 1.000000000000000000, -1.257568779154408793E-17, 0.000000000000000000 ) ) ;
#8501 = CARTESIAN_POINT ( 'NONE',  ( -3.949999999999997069, 99.99999999999998579, -8.525133428036873795 ) ) ;
#8502 = CARTESIAN_POINT ( 'NONE',  ( 10.00000000000000178, 49.31368534415484106, 10.88017736071110342 ) ) ;
#8504 = CARTESIAN_POINT ( 'NONE',  ( 6.204703633549690345, 17.84541550158063217, 14.16423886937410082 ) ) ;
#8503 = CARTESIAN_POINT ( 'NONE',  ( 22.81628187352648496, 51.83196800326376064, -3.434112377981050290 ) ) ;
#8505 = CARTESIAN_POINT ( 'NONE',  ( 19.84674366389459266, 3.717264484334118713, -2.638427012816827677 ) ) ;
#8506 = DIRECTION ( 'NONE',  ( 0.000000000000000000, 0.000000000000000000, -1.000000000000000000 ) ) ;
#8507 = CARTESIAN_POINT ( 'NONE',  ( 19.84674366389459621, 23.50893115100078390, 7.409399052514197653E-17 ) ) ;
#8508 = DIRECTION ( 'NONE',  ( -0.000000000000000000, -1.000000000000000000, -0.000000000000000000 ) ) ;
#8509 = CARTESIAN_POINT ( 'NONE',  ( 2.917880565312950480, 55.97041550158063217, -12.26659068614894821 ) ) ;
#8510 = FILL_AREA_STYLE_COLOUR ( '', #9071 ) ;
#8511 = CARTESIAN_POINT ( 'NONE',  ( 7.084665262690076126, 7.022018677488169658, -10.88017736071110164 ) ) ;
#8512 = LINE ( 'NONE', #39015, #96684 ) ;
#8513 = ORIENTED_EDGE ( 'NONE', *, *, #44034, .T. ) ;
#8514 = ORIENTED_EDGE ( 'NONE', *, *, #46418, .T. ) ;
#8515 = VECTOR ( 'NONE', #32395, 1000.000000000000000 ) ;
#8516 = CARTESIAN_POINT ( 'NONE',  ( 19.42250999205614548, 10.98035201082150536, -5.440088680355545492 ) ) ;
#8517 = CARTESIAN_POINT ( 'NONE',  ( 10.00000000000000178, 14.31368534415483929, 10.88017736071110342 ) ) ;
#8518 = CARTESIAN_POINT ( 'NONE',  ( 7.361572987183170547, 37.05059781766744464, 9.846743663894590881 ) ) ;
#8519 = CARTESIAN_POINT ( 'NONE',  ( -1.099225684535947600, 34.54030133659708923, 6.408140936763237150 ) ) ;
#8520 = DIRECTION ( 'NONE',  ( 1.000000000000000000, 0.000000000000000000, 0.000000000000000000 ) ) ;
#8522 = CARTESIAN_POINT ( 'NONE',  ( -0.3689425029237898834, 16.17874883491396076, -10.36894250292378850 ) ) ;
#8521 = CARTESIAN_POINT ( 'NONE',  ( -10.17198128013151326, 14.76930270348881002, 10.94389562857658760 ) ) ;
#8523 = CARTESIAN_POINT ( 'NONE',  ( 0.5774900079438590739, 22.64701867748817321, -5.440088680355550821 ) ) ;
#8524 = EDGE_CURVE ( 'NONE', #38545, #83562, #30665, .T. ) ;
#8525 = CARTESIAN_POINT ( 'NONE',  ( -4.164238869374098151, 66.59541550158060375, -3.795296366450310543 ) ) ;
#8526 = EDGE_CURVE ( 'NONE', #20839, #98896, #12969, .T. ) ;
#8527 = CARTESIAN_POINT ( 'NONE',  ( 5.076628168052703671, 41.84226448433411605, 8.527530157486179263 ) ) ;
#8528 = CARTESIAN_POINT ( 'NONE',  ( -7.750000000000000000, 41.24999999999999289, 6.250000000000000000 ) ) ;
#8529 = CARTESIAN_POINT ( 'NONE',  ( 19.84674366389459266, 23.71726448433412315, -2.638427012816827677 ) ) ;
#8530 = EDGE_CURVE ( 'NONE', #54264, #43197, #50476, .T. ) ;
#8531 = CARTESIAN_POINT ( 'NONE',  ( 0.1532563361054083140, 1.008931151000784787, 1.131784320476157264E-15 ) ) ;
#8532 = CARTESIAN_POINT ( 'NONE',  ( -7.208316651077764980, 30.38393115100079456, -7.208316651077759651 ) ) ;
#8533 = ORIENTED_EDGE ( 'NONE', *, *, #48100, .F. ) ;
#8534 = SURFACE_STYLE_USAGE ( .BOTH. , #47503 ) ;
#8535 = ORIENTED_EDGE ( 'NONE', *, *, #73858, .F. ) ;
#8536 = CARTESIAN_POINT ( 'NONE',  ( 17.20831665107776587, 62.88393115100078745, 7.208316651077764980 ) ) ;
#8538 = CARTESIAN_POINT ( 'NONE',  ( 4.559911319644449179, 38.89701867748817676, 9.422509992056141925 ) ) ;
#8537 = CARTESIAN_POINT ( 'NONE',  ( 0.5774900079438590739, 27.64701867748817676, -5.440088680355550821 ) ) ;
#8540 = CARTESIAN_POINT ( 'NONE',  ( -2.816281873526473856, 29.12363466993041783, 9.499525473075851096E-16 ) ) ;
#8539 =( LENGTH_UNIT ( ) NAMED_UNIT ( * ) SI_UNIT ( .MILLI., .METRE. ) );
#8541 = CARTESIAN_POINT ( 'NONE',  ( 22.26659068614894466, 23.88708216824730357, 7.082119434687054849 ) ) ;
#8542 = EDGE_CURVE ( 'NONE', #76182, #68558, #89953, .T. ) ;
#8543 = VECTOR ( 'NONE', #93323, 1000.000000000000227 ) ;
#8544 = CARTESIAN_POINT ( 'NONE',  ( 10.00000000000000000, 42.87363466993042493, -12.81628187352647608 ) ) ;
#8545 = ORIENTED_EDGE ( 'NONE', *, *, #58920, .T. ) ;
#8546 = TOROIDAL_SURFACE ( 'NONE', #78767, 14.49999999999999822, 0.5000000000000000000 ) ;
#8547 = CARTESIAN_POINT ( 'NONE',  ( 19.84674366389459266, 48.30059781766745175, 2.638427012816836559 ) ) ;
#8548 = CARTESIAN_POINT ( 'NONE',  ( 12.91533473730993009, 26.60535201082150536, -10.88017736071109987 ) ) ;
#8549 = ORIENTED_EDGE ( 'NONE', *, *, #51059, .F. ) ;
#8550 = CARTESIAN_POINT ( 'NONE',  ( 0.5774900079438607392, 23.48035201082150536, 5.440088680355550821 ) ) ;
#8551 = ORIENTED_EDGE ( 'NONE', *, *, #76610, .T. ) ;
#8552 = CARTESIAN_POINT ( 'NONE',  ( 15.44008868035555793, 56.39701867748817676, -9.422509992056140149 ) ) ;
#8553 = CARTESIAN_POINT ( 'NONE',  ( 10.00000000000000178, 70.00000000000000000, 0.000000000000000000 ) ) ;
#8554 = CARTESIAN_POINT ( 'NONE',  ( 2.035157376598824452, 68.68868534415484817, 7.964842623401179544 ) ) ;
#8555 = CARTESIAN_POINT ( 'NONE',  ( 18.52753015748618282, 3.925597817667451306, -4.923371831947291888 ) ) ;
#8556 = CARTESIAN_POINT ( 'NONE',  ( -0.8801773607111009756, 63.06368534415484106, 1.068504757029289695E-15 ) ) ;
#8557 = CARTESIAN_POINT ( 'NONE',  ( -10.04796213703165186, 9.757819552369537934E-16, -10.62905469192480723 ) ) ;
#8558 = CARTESIAN_POINT ( 'NONE',  ( -46.94000000000001194, 101.5930487410390270, 7.918115197747519929 ) ) ;
#8560 = VERTEX_POINT ( 'NONE', #82453 ) ;
#8559 = CARTESIAN_POINT ( 'NONE',  ( 10.00000000000000178, 12.25893115100078568, 9.846743663894594434 ) ) ;
#8561 = CARTESIAN_POINT ( 'NONE',  ( 12.63842701281683922, 39.55059781766744464, -9.846743663894590881 ) ) ;
#8562 = VERTEX_POINT ( 'NONE', #74953 ) ;
#8563 = CARTESIAN_POINT ( 'NONE',  ( 19.72487221294571569, 19.78217586085237301, 6.499999999999990230 ) ) ;
#8564 = CARTESIAN_POINT ( 'NONE',  ( 20.25387647958519821, 70.00000000000000000, -6.092576751097364074 ) ) ;
#8565 = SURFACE_STYLE_FILL_AREA ( #29696 ) ;
#8566 = CARTESIAN_POINT ( 'NONE',  ( 6.204703633549690345, 15.76208216824730179, -14.16423886937410259 ) ) ;
#8567 = CARTESIAN_POINT ( 'NONE',  ( -7.595945211628415628, 4.258289072137175049E-16, 12.35117874301636398 ) ) ;
#8568 = LINE ( 'NONE', #78044, #67357 ) ;
#8569 = CARTESIAN_POINT ( 'NONE',  ( 4.559911319644449179, 27.23035201082150536, -9.422509992056141925 ) ) ;
#8570 =( NAMED_UNIT ( * ) SI_UNIT ( $, .STERADIAN. ) SOLID_ANGLE_UNIT ( ) );
#8571 = ORIENTED_EDGE ( 'NONE', *, *, #2248, .F. ) ;
#8572 = CARTESIAN_POINT ( 'NONE',  ( 1.472469842513823179, 6.425597817667451750, 4.923371831947296329 ) ) ;
#8573 = CARTESIAN_POINT ( 'NONE',  ( 7.361572987183169658, -0.03273551566588185635, -9.846743663894592657 ) ) ;
#8574 = CARTESIAN_POINT ( 'NONE',  ( 10.00000000000000178, 35.37363466993042493, 12.81628187352647608 ) ) ;
#8575 = CARTESIAN_POINT ( 'NONE',  ( 2.791683348922240793, 26.63393115100078745, 7.208316651077764092 ) ) ;
#8576 = EDGE_CURVE ( 'NONE', #63305, #37093, #6792, .T. ) ;
#8577 =( NAMED_UNIT ( * ) PLANE_ANGLE_UNIT ( ) SI_UNIT ( $, .RADIAN. ) );
#8578 = CARTESIAN_POINT ( 'NONE',  ( 13.43411237798105340, 15.58196800326374998, 12.81628187352647963 ) ) ;
#8579 = CARTESIAN_POINT ( 'NONE',  ( -18.89999999999999147, 99.99999999999998579, 7.750000000000000000 ) ) ;
#8580 = CARTESIAN_POINT ( 'NONE',  ( 7.361572987183169658, 4.967264484334119601, -9.846743663894592657 ) ) ;
#8581 = ORIENTED_EDGE ( 'NONE', *, *, #97118, .T. ) ;
#8582 = ORIENTED_EDGE ( 'NONE', *, *, #39884, .T. ) ;
#8583 = CARTESIAN_POINT ( 'NONE',  ( 2.035157376598822676, 17.43868534415483751, -7.964842623401177768 ) ) ;
#8584 = CARTESIAN_POINT ( 'NONE',  ( 17.08211943468705130, 13.47041550158063572, 12.26659068614894998 ) ) ;
#8585 = CARTESIAN_POINT ( 'NONE',  ( 17.20831665107776587, 42.88393115100077324, 7.208316651077764980 ) ) ;
#8586 = CARTESIAN_POINT ( 'NONE',  ( 20.88017736071110875, 65.77201867748817676, -2.915334737309920765 ) ) ;
#8588 = CARTESIAN_POINT ( 'NONE',  ( 2.062412797813223616E-17, 1.639999999999999014, 0.000000000000000000 ) ) ;
#8587 = CARTESIAN_POINT ( 'NONE',  ( -1.099225684535947600, 58.70696800326375353, -6.408140936763238038 ) ) ;
#8589 = CARTESIAN_POINT ( 'NONE',  ( 4.559911319644449179, 22.23035201082150536, -9.422509992056141925 ) ) ;
#8590 = DIRECTION ( 'NONE',  ( -1.224646799147353207E-16, 1.540077580099091490E-33, 1.000000000000000000 ) ) ;
#8591 = CARTESIAN_POINT ( 'NONE',  ( 0.6178305044545838731, 14.74863466993041783, 9.382169495545420901 ) ) ;
#8592 = CARTESIAN_POINT ( 'NONE',  ( 10.00000000000000178, 47.25893115100078745, 9.846743663894594434 ) ) ;
#8593 = CARTESIAN_POINT ( 'NONE',  ( 3.469446951953614189E-15, -0.6863146558451562740, 10.88017736071110342 ) ) ;
#8594 = CARTESIAN_POINT ( 'NONE',  ( 16.40814093676324603, 42.45696800326375353, -11.09922568453594671 ) ) ;
#8595 = CARTESIAN_POINT ( 'NONE',  ( 3.969999999999999751, 37.00000000000000000, 2.500000000000000000 ) ) ;
#8597 = CARTESIAN_POINT ( 'NONE',  ( -7.750000000000000000, 41.24999999999999289, 6.500000000000000888 ) ) ;
#8596 = CARTESIAN_POINT ( 'NONE',  ( 2.035157376598822676, 47.43868534415484817, -7.964842623401177768 ) ) ;
#8598 = CARTESIAN_POINT ( 'NONE',  ( -9.898881779040801021, -0.03417435944610275333, 10.25059215482569641 ) ) ;
#8599 = CARTESIAN_POINT ( 'NONE',  ( 10.00000000000000000, 56.81368534415484106, -10.88017736071110342 ) ) ;
#8600 = CARTESIAN_POINT ( 'NONE',  ( 10.00000000000000000, 46.81368534415484106, -10.88017736071110342 ) ) ;
#8601 = CARTESIAN_POINT ( 'NONE',  ( 18.00000000000000355, 73.00000000000001421, 4.000000000000000000 ) ) ;
#8602 = EDGE_CURVE ( 'NONE', #33481, #44632, #56323, .T. ) ;
#8603 = CARTESIAN_POINT ( 'NONE',  ( 4.559911319644449179, 67.23035201082150536, -9.422509992056141925 ) ) ;
#8604 = AXIS2_PLACEMENT_3D ( 'NONE', #38760, #85732, #92247 ) ;
#8605 = ADVANCED_FACE ( 'NONE', ( #37468 ), #61420, .F. ) ;
#8606 = CARTESIAN_POINT ( 'NONE',  ( 0.1532563361054083140, 56.00893115100078745, 1.131784320476157264E-15 ) ) ;
#8608 = CARTESIAN_POINT ( 'NONE',  ( -10.64017930668213374, 0.3640475087720987379, 10.57291749337208842 ) ) ;
#8607 = CARTESIAN_POINT ( 'NONE',  ( 0.5774900079438607392, 28.48035201082150891, 5.440088680355550821 ) ) ;
#8609 = CARTESIAN_POINT ( 'NONE',  ( 0.6178305044545838731, 19.74863466993042138, 9.382169495545420901 ) ) ;
#8610 = ORIENTED_EDGE ( 'NONE', *, *, #45037, .F. ) ;
#8611 = CARTESIAN_POINT ( 'NONE',  ( -0.8801773607110991993, 42.85535201082150536, -2.915334737309923874 ) ) ;
#8612 = AXIS2_PLACEMENT_3D ( 'NONE', #58116, #5141, #20132 ) ;
#8614 = CARTESIAN_POINT ( 'NONE',  ( 0.2751277870542914172, 23.21833443783937767, 6.499999999999992006 ) ) ;
#8613 = CARTESIAN_POINT ( 'NONE',  ( 6.565887622018943937, 10.16530133659708746, 12.81628187352647430 ) ) ;
#8615 = CARTESIAN_POINT ( 'NONE',  ( 7.084665262690076126, 12.02201867748817143, -10.88017736071110164 ) ) ;
#8616 = CARTESIAN_POINT ( 'NONE',  ( 20.88017736071110519, 30.56368534415484106, 2.639326808657452039E-16 ) ) ;
#8617 = CARTESIAN_POINT ( 'NONE',  ( 17.08211943468705130, 38.47041550158063217, 12.26659068614894998 ) ) ;
#8618 = CARTESIAN_POINT ( 'NONE',  ( 19.84674366389459621, 28.50893115100078745, 7.409399052514197653E-17 ) ) ;
#8619 = CARTESIAN_POINT ( 'NONE',  ( 7.084665262690076126, 57.02201867748817676, -10.88017736071110164 ) ) ;
#8620 = CARTESIAN_POINT ( 'NONE',  ( 0.9082943533636183009, 15.00000000000000000, 14.47152380945585648 ) ) ;
#8621 = CARTESIAN_POINT ( 'NONE',  ( -4.164238869374099039, 6.803748834913967869, 8.674139862899312516E-16 ) ) ;
#8622 = DIRECTION ( 'NONE',  ( 0.07845909572783234254, 0.000000000000000000, 0.9969173337331289630 ) ) ;
#8623 = CARTESIAN_POINT ( 'NONE',  ( 10.00000000000000000, 54.75893115100078745, -9.846743663894594434 ) ) ;
#8624 = EDGE_LOOP ( 'NONE', ( #77958, #17574, #54506, #22214 ) ) ;
#8625 = EDGE_LOOP ( 'NONE', ( #4829, #18530, #46835, #15543 ) ) ;
#8626 = CARTESIAN_POINT ( 'NONE',  ( 10.00000000000000000, 30.55374883491397142, -14.16423886937410082 ) ) ;
#8627 = CARTESIAN_POINT ( 'NONE',  ( -2.266590686148945544, 36.38708216824730357, -7.082119434687050408 ) ) ;
#8628 = CARTESIAN_POINT ( 'NONE',  ( 18.52753015748618282, 3.925597817667451306, -4.923371831947291888 ) ) ;
#8629 = CARTESIAN_POINT ( 'NONE',  ( 7.361572987183169658, 59.96726448433410894, -9.846743663894592657 ) ) ;
#8630 = CARTESIAN_POINT ( 'NONE',  ( -9.206628575885845933, -19.70849028575491246, 4.000000000000000000 ) ) ;
#8632 = CARTESIAN_POINT ( 'NONE',  ( -2.816281873526473856, 24.12363466993042138, 9.499525473075851096E-16 ) ) ;
#8631 = CARTESIAN_POINT ( 'NONE',  ( 10.00000000000000178, 59.31368534415484106, 10.88017736071110342 ) ) ;
#8633 = CARTESIAN_POINT ( 'NONE',  ( -0.3689425029237898834, 36.17874883491396787, -10.36894250292378850 ) ) ;
#8634 = CARTESIAN_POINT ( 'NONE',  ( -0.8801773607111009756, 23.06368534415484106, 1.068504757029289695E-15 ) ) ;
#8635 = CARTESIAN_POINT ( 'NONE',  ( 19.42250999205614193, 35.14701867748816966, 5.440088680355555262 ) ) ;
#8636 = CARTESIAN_POINT ( 'NONE',  ( 12.60589901313222327, 0.3640475087720989600, -8.129656208642053627 ) ) ;
#8637 = CARTESIAN_POINT ( 'NONE',  ( 4.559911319644449179, 52.23035201082151247, -9.422509992056141925 ) ) ;
#8638 = CARTESIAN_POINT ( 'NONE',  ( 9.846743663894590881, -11.28273551566587685, -2.638427012816833894 ) ) ;
#8639 = ORIENTED_EDGE ( 'NONE', *, *, #15606, .T. ) ;
#8640 = CYLINDRICAL_SURFACE ( 'NONE', #18817, 0.2500000000000002220 ) ;
#8641 = ORIENTED_EDGE ( 'NONE', *, *, #95637, .T. ) ;
#8642 = LINE ( 'NONE', #78121, #89188 ) ;
#8643 = ORIENTED_EDGE ( 'NONE', *, *, #4333, .T. ) ;
#8644 = CARTESIAN_POINT ( 'NONE',  ( -0.3689425029237898834, 1.178748834913967869, -10.36894250292378850 ) ) ;
#8646 = CARTESIAN_POINT ( 'NONE',  ( 4.559911319644449179, 2.230352010821504916, -9.422509992056141925 ) ) ;
#8645 = CARTESIAN_POINT ( 'NONE',  ( 22.26659068614895176, 54.72041550158063217, -7.082119434687042414 ) ) ;
#8648 = CARTESIAN_POINT ( 'NONE',  ( 1.472469842513823179, 65.59226448433412315, -4.923371831947296329 ) ) ;
#8647 = CARTESIAN_POINT ( 'NONE',  ( 10.00000000000000000, 39.75893115100078745, -9.846743663894594434 ) ) ;
#8649 = DIRECTION ( 'NONE',  ( 1.049065152435176504E-16, -1.000000000000000000, 0.000000000000000000 ) ) ;
#8650 = CARTESIAN_POINT ( 'NONE',  ( -2.816281873526473856, 9.331968003263753531, 3.434112377981055619 ) ) ;
#8651 = ORIENTED_EDGE ( 'NONE', *, *, #23068, .T. ) ;
#8652 = CARTESIAN_POINT ( 'NONE',  ( 6.204703633549690345, 45.76208216824729647, -14.16423886937410259 ) ) ;
#8653 = CARTESIAN_POINT ( 'NONE',  ( -2.266590686148945544, 42.22041550158063217, 7.082119434687048631 ) ) ;
#8654 = ORIENTED_EDGE ( 'NONE', *, *, #42653, .T. ) ;
#8655 = CARTESIAN_POINT ( 'NONE',  ( 2.035157376598822676, 17.43868534415483751, -7.964842623401177768 ) ) ;
#8656 = CARTESIAN_POINT ( 'NONE',  ( 16.40814093676324603, 57.45696800326375353, -11.09922568453594671 ) ) ;
#8657 = CARTESIAN_POINT ( 'NONE',  ( 17.96484262340118221, 26.18868534415483396, -7.964842623401177768 ) ) ;
#8658 = CARTESIAN_POINT ( 'NONE',  ( 18.52753015748617571, 48.09226448433412315, 4.923371831947298993 ) ) ;
#8659 = CARTESIAN_POINT ( 'NONE',  ( 12.91533473730993009, 21.60535201082150536, -10.88017736071109987 ) ) ;
#8660 = CARTESIAN_POINT ( 'NONE',  ( -6.829866546992951370, -69.52413922185967010, 2.500000000000000444 ) ) ;
#8661 = CARTESIAN_POINT ( 'NONE',  ( 7.361572987183170547, 57.05059781766744464, 9.846743663894590881 ) ) ;
#8662 = CYLINDRICAL_SURFACE ( 'NONE', #17075, 0.2500000000000002220 ) ;
#8663 = CARTESIAN_POINT ( 'NONE',  ( 15.44008868035555793, 31.39701867748817676, -9.422509992056140149 ) ) ;
#8665 = ORIENTED_EDGE ( 'NONE', *, *, #57584, .T. ) ;
#8664 = DIRECTION ( 'NONE',  ( 0.000000000000000000, -1.000000000000000000, 0.000000000000000000 ) ) ;
#8666 = DIRECTION ( 'NONE',  ( -1.000000000000000000, 0.000000000000000000, 0.000000000000000000 ) ) ;
#8667 = AXIS2_PLACEMENT_3D ( 'NONE', #62403, #44947, #75452 ) ;
#8668 = SURFACE_STYLE_USAGE ( .BOTH. , #16179 ) ;
#8669 = DIRECTION ( 'NONE',  ( -1.000000000000000000, 0.000000000000000000, 0.000000000000000000 ) ) ;
#8670 = ORIENTED_EDGE ( 'NONE', *, *, #95368, .T. ) ;
#8671 = CARTESIAN_POINT ( 'NONE',  ( 8.900267494636356247, -1.043573704943436598, 3.750000000000000000 ) ) ;
#8672 = CARTESIAN_POINT ( 'NONE',  ( 19.84674366389459266, 33.30059781766744464, 2.638427012816836559 ) ) ;
#8673 = CARTESIAN_POINT ( 'NONE',  ( -7.199999999999996625, 99.99999999999998579, 8.000000000000000000 ) ) ;
#8674 = CARTESIAN_POINT ( 'NONE',  ( -2.816281873526471635, 48.91530133659708213, -3.434112377981056508 ) ) ;
#8675 = DIRECTION ( 'NONE',  ( 0.000000000000000000, 0.000000000000000000, -1.000000000000000000 ) ) ;
#8676 = DIRECTION ( 'NONE',  ( 0.02617694830788287394, 0.000000000000000000, -0.9996573249755570378 ) ) ;
#8677 = EDGE_LOOP ( 'NONE', ( #2652, #83075, #58683 ) ) ;
#8678 = CARTESIAN_POINT ( 'NONE',  ( 17.35999999999999588, 33.99999999999997158, 7.000000000000000000 ) ) ;
#8679 = DIRECTION ( 'NONE',  ( -0.000000000000000000, -0.000000000000000000, -1.000000000000000000 ) ) ;
#8680 = CARTESIAN_POINT ( 'NONE',  ( 2.791683348922237240, 60.38393115100078745, -7.208316651077763204 ) ) ;
#8681 = CARTESIAN_POINT ( 'NONE',  ( -2.266590686148945544, 52.22041550158064638, 7.082119434687048631 ) ) ;
#8682 = CARTESIAN_POINT ( 'NONE',  ( 17.20831665107776587, 57.88393115100078745, 7.208316651077764980 ) ) ;
#8683 = CARTESIAN_POINT ( 'NONE',  ( 12.63842701281683922, 19.55059781766745175, -9.846743663894590881 ) ) ;
#8684 = CARTESIAN_POINT ( 'NONE',  ( 16.40814093676323893, 55.79030133659708923, 11.09922568453595026 ) ) ;
#8685 = CARTESIAN_POINT ( 'NONE',  ( 7.361572987183170547, 62.05059781766745886, 9.846743663894590881 ) ) ;
#8686 = CARTESIAN_POINT ( 'NONE',  ( 20.88017736071110875, 55.77201867748816966, -2.915334737309920765 ) ) ;
#8687 = EDGE_CURVE ( 'NONE', #26584, #48509, #53933, .T. ) ;
#8688 = CARTESIAN_POINT ( 'NONE',  ( 12.63842701281683922, 44.55059781766745175, -9.846743663894590881 ) ) ;
#8689 = CARTESIAN_POINT ( 'NONE',  ( -8.731067818237029599, 8.287123368507817389, 8.731067818237043809 ) ) ;
#8690 = CARTESIAN_POINT ( 'NONE',  ( 2.035157376598824452, 53.68868534415484817, 7.964842623401179544 ) ) ;
#8691 = ORIENTED_EDGE ( 'NONE', *, *, #78213, .T. ) ;
#8692 = FACE_OUTER_BOUND ( 'NONE', #73450, .T. ) ;
#8693 = CARTESIAN_POINT ( 'NONE',  ( 20.88017736071110519, 30.56368534415484106, 2.639326808657452039E-16 ) ) ;
#8695 = CARTESIAN_POINT ( 'NONE',  ( 12.91533473730993009, 51.60535201082149825, -10.88017736071109987 ) ) ;
#8694 = CARTESIAN_POINT ( 'NONE',  ( -2.816281873526473856, 4.123634669930420493, 9.499525473075851096E-16 ) ) ;
#8696 = CARTESIAN_POINT ( 'NONE',  ( -14.97687855664608847, 15.00000000000000000, 0.8325315005899532883 ) ) ;
#8697 = CARTESIAN_POINT ( 'NONE',  ( 7.084665262690076126, 67.02201867748817676, -10.88017736071110164 ) ) ;
#8698 = CARTESIAN_POINT ( 'NONE',  ( 13.78891971893209245, 14.49999999999999112, 5.904717858191670388 ) ) ;
#8700 = CARTESIAN_POINT ( 'NONE',  ( -0.1503990784575247319, 62.22266099184918176, -6.262539305110083276 ) ) ;
#8699 = CARTESIAN_POINT ( 'NONE',  ( 7.084665262690076126, 37.02201867748817676, -10.88017736071110164 ) ) ;
#8701 = CARTESIAN_POINT ( 'NONE',  ( 19.84674366389459266, 38.30059781766745175, 2.638427012816836559 ) ) ;
#8702 = CARTESIAN_POINT ( 'NONE',  ( 19.84674366389459266, 3.300597817667451750, 2.638427012816836559 ) ) ;
#8703 = CARTESIAN_POINT ( 'NONE',  ( -9.422509992056145478, -37.35298132251182324, -5.440088680355541939 ) ) ;
#8704 = CARTESIAN_POINT ( 'NONE',  ( -2.816281873526471635, 13.91530133659708746, -3.434112377981056508 ) ) ;
#8706 =( NAMED_UNIT ( * ) SI_UNIT ( $, .STERADIAN. ) SOLID_ANGLE_UNIT ( ) );
#8705 = CARTESIAN_POINT ( 'NONE',  ( 0.5774900079438590739, 17.64701867748817321, -5.440088680355550821 ) ) ;
#8707 = CIRCLE ( 'NONE', #23081, 0.2500000000000002220 ) ;
#8708 = CARTESIAN_POINT ( 'NONE',  ( -0.3689425029237898834, 21.17874883491396432, -10.36894250292378850 ) ) ;
#8709 = CARTESIAN_POINT ( 'NONE',  ( 10.00000000000000178, 63.05374883491396076, 14.16423886937410082 ) ) ;
#8710 = CARTESIAN_POINT ( 'NONE',  ( 14.92337183194729988, 14.34226448433411782, -8.527530157486177487 ) ) ;
#8711 = SURFACE_STYLE_USAGE ( .BOTH. , #77206 ) ;
#8712 = ORIENTED_EDGE ( 'NONE', *, *, #655, .T. ) ;
#8713 = CARTESIAN_POINT ( 'NONE',  ( 0.1532563361054082862, 21.21726448433412315, 2.638427012816831674 ) ) ;
#8714 = EDGE_CURVE ( 'NONE', #93646, #32106, #89848, .T. ) ;
#8715 = CARTESIAN_POINT ( 'NONE',  ( 20.88017736071110875, 20.77201867748816611, -2.915334737309920765 ) ) ;
#8716 = CARTESIAN_POINT ( 'NONE',  ( 0.1532563361054100626, 60.80059781766744464, -2.638427012816831230 ) ) ;
#8718 = DIRECTION ( 'NONE',  ( 0.000000000000000000, 1.000000000000000000, 0.000000000000000000 ) ) ;
#8717 = CARTESIAN_POINT ( 'NONE',  ( 17.08211943468705840, 5.137082168247300906, -12.26659068614894466 ) ) ;
#8719 = DIRECTION ( 'NONE',  ( 1.000000000000000000, 0.000000000000000000, 0.000000000000000000 ) ) ;
#8720 = CARTESIAN_POINT ( 'NONE',  ( 18.52753015748618282, 13.92559781766745175, -4.923371831947291888 ) ) ;
#8721 = CARTESIAN_POINT ( 'NONE',  ( 19.38216949554541557, 37.24863466993041783, -9.382169495545420901 ) ) ;
#8722 = CARTESIAN_POINT ( 'NONE',  ( 19.84674366389459266, 43.30059781766744464, 2.638427012816836559 ) ) ;
#8723 = ORIENTED_EDGE ( 'NONE', *, *, #39252, .F. ) ;
#8724 = CARTESIAN_POINT ( 'NONE',  ( 10.00000000000000178, 17.25893115100078745, 9.846743663894594434 ) ) ;
#8725 = CARTESIAN_POINT ( 'NONE',  ( 2.603489959281592991, 11.58210964143329313, 6.500000000000006217 ) ) ;
#8726 = CARTESIAN_POINT ( 'NONE',  ( 2.917880565312948704, 47.63708216824730357, 12.26659068614894643 ) ) ;
#8727 = CARTESIAN_POINT ( 'NONE',  ( 15.44008868035555260, 49.73035201082150536, 9.422509992056143702 ) ) ;
#8728 = CARTESIAN_POINT ( 'NONE',  ( -0.04068437667224335946, 32.21974360917720759, -6.396802510829702193 ) ) ;
#8729 = CARTESIAN_POINT ( 'NONE',  ( 12.91533473730993009, 56.60535201082151247, -10.88017736071109987 ) ) ;
#8730 = CARTESIAN_POINT ( 'NONE',  ( 5.076628168052703671, 31.84226448433412315, 8.527530157486179263 ) ) ;
#8731 = CARTESIAN_POINT ( 'NONE',  ( 12.91533473730992121, 14.52201867748817143, 10.88017736071110164 ) ) ;
#8732 = CARTESIAN_POINT ( 'NONE',  ( -7.674241358950697922, 14.76984990496856831, -12.81905807005896136 ) ) ;
#8733 = CARTESIAN_POINT ( 'NONE',  ( 1.472469842513823179, 55.59226448433412315, -4.923371831947296329 ) ) ;
#8734 = CARTESIAN_POINT ( 'NONE',  ( 7.084665262690076126, 47.02201867748818387, -10.88017736071110164 ) ) ;
#8735 = CARTESIAN_POINT ( 'NONE',  ( 5.076628168052704559, 0.1755978176674514724, -8.527530157486179263 ) ) ;
#8736 = EDGE_LOOP ( 'NONE', ( #90155, #44793, #34896, #92702 ) ) ;
#8737 = ORIENTED_EDGE ( 'NONE', *, *, #29591, .F. ) ;
#8738 = PLANE ( 'NONE',  #53282 ) ;
#8739 = CARTESIAN_POINT ( 'NONE',  ( -8.000000000000000000, 1.019547802438466100, -3.750000000000000000 ) ) ;
#8740 = CARTESIAN_POINT ( 'NONE',  ( 18.52753015748618282, 43.92559781766745175, -4.923371831947291888 ) ) ;
#8741 = CARTESIAN_POINT ( 'NONE',  ( 1.472469842513823179, 21.42559781766745175, 4.923371831947296329 ) ) ;
#8742 = CARTESIAN_POINT ( 'NONE',  ( 13.43411237798106583, 57.66530133659708923, -12.81628187352647252 ) ) ;
#8744 = CARTESIAN_POINT ( 'NONE',  ( 18.52753015748617571, 53.09226448433412315, 4.923371831947298993 ) ) ;
#8743 = CARTESIAN_POINT ( 'NONE',  ( 0.5774900079438590739, 22.64701867748817321, -5.440088680355550821 ) ) ;
#8745 = DIRECTION ( 'NONE',  ( -0.8788171126619678253, 0.000000000000000000, 0.4771587602596037425 ) ) ;
#8746 = B_SPLINE_CURVE_WITH_KNOTS ( 'NONE', 3,
 ( #93816, #16848, #78318, #33301, #26298, #86817 ),
 .UNSPECIFIED., .F., .F.,
 ( 4, 2, 4 ),
 ( 3.409110551494476605E-05, 0.0004400426677367900953, 0.0008459942299586354448 ),
 .UNSPECIFIED. ) ;
#8747 = CARTESIAN_POINT ( 'NONE',  ( -2.266590686148945544, 27.22041550158063572, 7.082119434687048631 ) ) ;
#8748 = VECTOR ( 'NONE', #24961, 1000.000000000000000 ) ;
#8749 = CARTESIAN_POINT ( 'NONE',  ( 22.26659068614895176, 54.72041550158063217, -7.082119434687042414 ) ) ;
#8750 = CARTESIAN_POINT ( 'NONE',  ( 19.84674366389459266, 63.30059781766745886, 2.638427012816836559 ) ) ;
#8751 = DIRECTION ( 'NONE',  ( 0.000000000000000000, 0.000000000000000000, 1.000000000000000000 ) ) ;
#8752 = CARTESIAN_POINT ( 'NONE',  ( 20.88017736071110519, 50.56368534415484106, 2.639326808657452039E-16 ) ) ;
#8753 = AXIS2_PLACEMENT_3D ( 'NONE', #11298, #41819, #27771 ) ;
#8754 = CARTESIAN_POINT ( 'NONE',  ( 17.20831665107776587, 9.133931151000787452, -7.208316651077762316 ) ) ;
#8755 = CARTESIAN_POINT ( 'NONE',  ( -6.868018881922843377, -58.39307134327827953, 3.999999999996775024 ) ) ;
#8756 = EDGE_CURVE ( 'NONE', #80446, #51688, #61650, .T. ) ;
#8757 = ORIENTED_EDGE ( 'NONE', *, *, #54271, .F. ) ;
#8758 = DIRECTION ( 'NONE',  ( 0.000000000000000000, 0.000000000000000000, -1.000000000000000000 ) ) ;
#8759 = CIRCLE ( 'NONE', #85405, 15.00000000000000000 ) ;
#8760 = EDGE_LOOP ( 'NONE', ( #62169, #18141, #85288, #16881 ) ) ;
#8761 = CARTESIAN_POINT ( 'NONE',  ( 7.361572987183169658, 14.96726448433411960, -9.846743663894592657 ) ) ;
#8762 = VERTEX_POINT ( 'NONE', #21974 ) ;
#8763 = CARTESIAN_POINT ( 'NONE',  ( 24.16423886937410614, 14.30374883491396787, 8.672049930838204340E-16 ) ) ;
#8764 = CARTESIAN_POINT ( 'NONE',  ( 14.92337183194729988, 14.34226448433411782, -8.527530157486177487 ) ) ;
#8765 = CARTESIAN_POINT ( 'NONE',  ( 2.035157376598822676, 42.43868534415483396, -7.964842623401177768 ) ) ;
#8766 = EDGE_CURVE ( 'NONE', #50677, #65059, #97465, .T. ) ;
#8767 = DIRECTION ( 'NONE',  ( 0.000000000000000000, -1.000000000000000000, 0.000000000000000000 ) ) ;
#8768 = ORIENTED_EDGE ( 'NONE', *, *, #76445, .F. ) ;
#8769 = CARTESIAN_POINT ( 'NONE',  ( 20.88017736071110519, 25.56368534415483751, 2.639326808657452039E-16 ) ) ;
#8770 = CARTESIAN_POINT ( 'NONE',  ( 12.07856007377819907, 15.00000000000000000, 8.022367888854917695 ) ) ;
#8771 = AXIS2_PLACEMENT_3D ( 'NONE', #36382, #74361, #96407 ) ;
#8772 = ORIENTED_EDGE ( 'NONE', *, *, #81136, .T. ) ;
#8773 = CARTESIAN_POINT ( 'NONE',  ( 6.204703633549690345, 7.845415501580634832, 14.16423886937410082 ) ) ;
#8774 = VERTEX_POINT ( 'NONE', #8432 ) ;
#8775 = CARTESIAN_POINT ( 'NONE',  ( -2.816281873526473856, 24.33196800326375353, 3.434112377981055619 ) ) ;
#8776 = CARTESIAN_POINT ( 'NONE',  ( 14.92337183194729633, 12.67559781766745353, 8.527530157486181039 ) ) ;
#8777 = CARTESIAN_POINT ( 'NONE',  ( 0.000000000000000000, 15.00000000000000000, 0.000000000000000000 ) ) ;
#8778 = FACE_OUTER_BOUND ( 'NONE', #85630, .T. ) ;
#8779 = CARTESIAN_POINT ( 'NONE',  ( 12.63842701281683922, 19.55059781766745175, -9.846743663894590881 ) ) ;
#8780 = CARTESIAN_POINT ( 'NONE',  ( -0.8801773607111009756, 28.06368534415484106, 1.068504757029289695E-15 ) ) ;
#8781 = STYLED_ITEM ( 'NONE', ( #20078 ), #52424 ) ;
#8782 = ORIENTED_EDGE ( 'NONE', *, *, #22584, .F. ) ;
#8783 = CARTESIAN_POINT ( 'NONE',  ( 0.000000000000000000, 0.000000000000000000, 0.000000000000000000 ) ) ;
#8784 = CARTESIAN_POINT ( 'NONE',  ( 19.42250999205614548, 55.98035201082150536, -5.440088680355545492 ) ) ;
#8785 = CARTESIAN_POINT ( 'NONE',  ( -1.354709868695722852, 0.5000000000000004441, 14.93870011653150698 ) ) ;
#8786 = PRESENTATION_STYLE_ASSIGNMENT (( #8305 ) ) ;
#8787 = CARTESIAN_POINT ( 'NONE',  ( 7.084665262690076126, 67.02201867748817676, -10.88017736071110164 ) ) ;
#8788 = CARTESIAN_POINT ( 'NONE',  ( 21.09922568453595559, 17.04030133659708923, -6.408140936763230044 ) ) ;
#8789 = B_SPLINE_CURVE_WITH_KNOTS ( 'NONE', 3,
 ( #9844, #69362, #32326, #46842, #883, #85341 ),
 .UNSPECIFIED., .F., .F.,
 ( 4, 2, 4 ),
 ( 0.000000000000000000, 0.0002496607219482335272, 0.0004993214438964670545 ),
 .UNSPECIFIED. ) ;
#8790 = ORIENTED_EDGE ( 'NONE', *, *, #36598, .T. ) ;
#8791 = DIRECTION ( 'NONE',  ( -0.000000000000000000, -1.000000000000000000, -0.000000000000000000 ) ) ;
#8792 = CARTESIAN_POINT ( 'NONE',  ( 19.84674366389459621, 28.50893115100078745, 7.409399052514197653E-17 ) ) ;
#8793 = CARTESIAN_POINT ( 'NONE',  ( 21.09922568453594849, 56.20696800326375353, 6.408140936763242479 ) ) ;
#8794 = CARTESIAN_POINT ( 'NONE',  ( 1.821708436314968482, 36.66792564121895026, -6.500000000000079936 ) ) ;
#8795 = CARTESIAN_POINT ( 'NONE',  ( 19.84674366389459621, 18.50893115100078745, 7.409399052514197653E-17 ) ) ;
#8797 = AXIS2_PLACEMENT_3D ( 'NONE', #83805, #60794, #85282 ) ;
#8796 = CARTESIAN_POINT ( 'NONE',  ( 0.6178305044545818747, 23.49863466993041783, -9.382169495545419124 ) ) ;
#8799 = CARTESIAN_POINT ( 'NONE',  ( -10.53011945866295029, -98.59345040283277228, 3.750000000000000000 ) ) ;
#8798 = CARTESIAN_POINT ( 'NONE',  ( -9.000000000000003553, 80.99999999999994316, 0.000000000000000000 ) ) ;
#8800 = CARTESIAN_POINT ( 'NONE',  ( 20.88017736071110164, 55.35535201082149825, 2.915334737309930979 ) ) ;
#8801 = CARTESIAN_POINT ( 'NONE',  ( 2.791683348922240793, 56.63393115100078035, 7.208316651077764092 ) ) ;
#8802 = FACE_OUTER_BOUND ( 'NONE', #69291, .T. ) ;
#8803 = CARTESIAN_POINT ( 'NONE',  ( 12.63842701281683922, 29.55059781766745175, -9.846743663894590881 ) ) ;
#8804 = CARTESIAN_POINT ( 'NONE',  ( 14.92337183194729633, 17.67559781766745175, 8.527530157486181039 ) ) ;
#8805 = CARTESIAN_POINT ( 'NONE',  ( 12.91533473730992121, 9.522018677488171434, 10.88017736071110164 ) ) ;
#8806 = EDGE_CURVE ( 'NONE', #31975, #10378, #36715, .T. ) ;
#8807 = CARTESIAN_POINT ( 'NONE',  ( -1.099225684535947600, 14.54030133659708568, 6.408140936763237150 ) ) ;
#8808 = CARTESIAN_POINT ( 'NONE',  ( -0.8801773607111008646, 3.272018677488171434, 2.915334737309923430 ) ) ;
#8809 = CARTESIAN_POINT ( 'NONE',  ( 0.000000000000000000, 81.99999999999992895, 5.000000000000000000 ) ) ;
#98989 = CARTESIAN_POINT ( 'NONE',  ( 10.00000000000000178, 37.25893115100078745, 9.846743663894594434 ) ) ;
#8812 = EDGE_CURVE ( 'NONE', #62525, #77069, #79564, .T. ) ;
#8811 = CARTESIAN_POINT ( 'NONE',  ( 2.035157376598824452, 18.68868534415484106, 7.964842623401179544 ) ) ;
#8813 = VECTOR ( 'NONE', #47781, 1000.000000000000000 ) ;
#8814 = PRESENTATION_STYLE_ASSIGNMENT (( #24817 ) ) ;
#8816 = CARTESIAN_POINT ( 'NONE',  ( 17.96484262340118221, 11.18868534415484106, -7.964842623401177768 ) ) ;
#8815 = CARTESIAN_POINT ( 'NONE',  ( 19.84674366389459266, 23.71726448433412315, -2.638427012816827677 ) ) ;
#8817 = CARTESIAN_POINT ( 'NONE',  ( 7.084665262690076126, 37.02201867748817676, -10.88017736071110164 ) ) ;
#8819 = CARTESIAN_POINT ( 'NONE',  ( 1.046131998950050601, 40.73810908735726599, 6.499999999999992006 ) ) ;
#8818 = CARTESIAN_POINT ( 'NONE',  ( -0.3689425029237881626, 67.42874883491396076, 10.36894250292379027 ) ) ;
#8820 = CARTESIAN_POINT ( 'NONE',  ( 1.472469842513823179, 1.425597817667451528, 4.923371831947296329 ) ) ;
#8821 = CARTESIAN_POINT ( 'NONE',  ( 0.1532563361054100626, 35.80059781766745175, -2.638427012816831230 ) ) ;
#8822 = DIRECTION ( 'NONE',  ( 2.478176394252579169E-16, -1.000000000000000000, 0.000000000000000000 ) ) ;
#8823 = CARTESIAN_POINT ( 'NONE',  ( -0.3093388210927633386, 14.63723947401114067, -14.99680997725065978 ) ) ;
#8824 = CARTESIAN_POINT ( 'NONE',  ( -13.07907619356921636, 0.2301500790491314286, -7.222187741820853546 ) ) ;
#8825 = CARTESIAN_POINT ( 'NONE',  ( -10.79676793865326268, -44.60032227172077768, -3.750000000001800782 ) ) ;
#8826 = CARTESIAN_POINT ( 'NONE',  ( 24.16423886937410614, 24.30374883491396787, 8.672049930838204340E-16 ) ) ;
#8827 = CARTESIAN_POINT ( 'NONE',  ( 7.361572987183169658, 39.96726448433411605, -9.846743663894592657 ) ) ;
#8828 = DIRECTION ( 'NONE',  ( 0.000000000000000000, 0.000000000000000000, -1.000000000000000000 ) ) ;
#8829 = ORIENTED_EDGE ( 'NONE', *, *, #24698, .T. ) ;
#8830 = EDGE_CURVE ( 'NONE', #67262, #10027, #31410, .T. ) ;
#8831 = CARTESIAN_POINT ( 'NONE',  ( 22.26659068614894466, 48.88708216824730357, 7.082119434687054849 ) ) ;
#8832 = CARTESIAN_POINT ( 'NONE',  ( 10.00000000000000000, 24.75893115100078745, -9.846743663894594434 ) ) ;
#8834 = CARTESIAN_POINT ( 'NONE',  ( 13.14228782657341732, 14.49999999999999112, 7.230509711182337540 ) ) ;
#8833 = LINE ( 'NONE', #75858, #49853 ) ;
#8835 = CARTESIAN_POINT ( 'NONE',  ( -0.8801773607110991993, 42.85535201082150536, -2.915334737309923874 ) ) ;
#8836 = CARTESIAN_POINT ( 'NONE',  ( 13.43411237798106583, 57.66530133659708923, -12.81628187352647252 ) ) ;
#8837 = CARTESIAN_POINT ( 'NONE',  ( 17.96484262340118221, 19.93868534415484106, 7.964842623401181321 ) ) ;
#8838 = CARTESIAN_POINT ( 'NONE',  ( 6.565887622018943937, 53.08196800326374643, -12.81628187352647608 ) ) ;
#8839 = CARTESIAN_POINT ( 'NONE',  ( 18.52753015748617571, 63.09226448433412315, 4.923371831947298993 ) ) ;
#8841 = VERTEX_POINT ( 'NONE', #36965 ) ;
#8840 = EDGE_CURVE ( 'NONE', #2418, #27580, #21205, .T. ) ;
#8842 = DIRECTION ( 'NONE',  ( 6.938893903907222067E-15, 0.000000000000000000, 1.000000000000000000 ) ) ;
#8843 = CARTESIAN_POINT ( 'NONE',  ( -0.1503990784575328643, 20.12777174578613071, 6.262539305110068177 ) ) ;
#8844 = CARTESIAN_POINT ( 'NONE',  ( 10.00000000000000178, 48.05374883491396787, 14.16423886937410082 ) ) ;
#8845 = CARTESIAN_POINT ( 'NONE',  ( 20.36894250292379382, 8.678748834913967869, 10.36894250292379205 ) ) ;
#8846 = CARTESIAN_POINT ( 'NONE',  ( 15.44008868035555260, 24.73035201082150891, 9.422509992056143702 ) ) ;
#8847 = CARTESIAN_POINT ( 'NONE',  ( 0.5774900079438590739, 42.64701867748816966, -5.440088680355550821 ) ) ;
#8848 = CARTESIAN_POINT ( 'NONE',  ( 8.375939845167756914, 15.00000000000000000, -11.52849216984298941 ) ) ;
#8849 = LINE ( 'NONE', #38871, #33638 ) ;
#8850 = CARTESIAN_POINT ( 'NONE',  ( 10.00000000000000178, 69.31368534415484817, 10.88017736071110342 ) ) ;
#8851 = CARTESIAN_POINT ( 'NONE',  ( 19.42250999205614193, 60.14701867748817676, 5.440088680355555262 ) ) ;
#8852 = CARTESIAN_POINT ( 'NONE',  ( 1.472469842513823179, 26.42559781766745175, 4.923371831947296329 ) ) ;
#8853 = CARTESIAN_POINT ( 'NONE',  ( 5.419894505350611347, 14.63606864254977502, -13.98659156302462314 ) ) ;
#8854 = CARTESIAN_POINT ( 'NONE',  ( 17.20831665107776587, 12.88393115100078390, 7.208316651077764980 ) ) ;
#8855 = CARTESIAN_POINT ( 'NONE',  ( 10.00000000000000000, 34.75893115100078745, -9.846743663894594434 ) ) ;
#8856 = AXIS2_PLACEMENT_3D ( 'NONE', #1346, #55296, #94274 ) ;
#8857 = CARTESIAN_POINT ( 'NONE',  ( -0.8801773607111008646, 8.272018677488171434, 2.915334737309923430 ) ) ;
#8858 = CARTESIAN_POINT ( 'NONE',  ( 0.6178305044545818747, 28.49863466993041783, -9.382169495545419124 ) ) ;
#8859 = AXIS2_PLACEMENT_3D ( 'NONE', #75245, #8719, #76723 ) ;
#8860 = CARTESIAN_POINT ( 'NONE',  ( 1.472469842513823179, 6.425597817667451750, 4.923371831947296329 ) ) ;
#8861 = DIRECTION ( 'NONE',  ( 0.3007057995042701770, -0.000000000000000000, 0.9537169507482278208 ) ) ;
#8862 = CARTESIAN_POINT ( 'NONE',  ( 17.20831665107776587, 47.88393115100078745, 7.208316651077764980 ) ) ;
#8863 = CARTESIAN_POINT ( 'NONE',  ( 14.92337183194729633, 32.67559781766745175, 8.527530157486181039 ) ) ;
#8864 = CARTESIAN_POINT ( 'NONE',  ( -4.164238869374098151, 16.59541550158063927, -3.795296366450310543 ) ) ;
#8865 = CARTESIAN_POINT ( 'NONE',  ( 7.084665262690076126, 52.02201867748816255, -10.88017736071110164 ) ) ;
#8866 = CARTESIAN_POINT ( 'NONE',  ( 7.084665262690076126, 9.105352010821503583, 10.88017736071109987 ) ) ;
#8867 = CARTESIAN_POINT ( 'NONE',  ( 12.91533473730993009, 51.60535201082149825, -10.88017736071109987 ) ) ;
#8868 = CARTESIAN_POINT ( 'NONE',  ( 15.44008868035555793, 36.39701867748816966, -9.422509992056140149 ) ) ;
#8869 = ORIENTED_EDGE ( 'NONE', *, *, #12536, .F. ) ;
#8870 = CARTESIAN_POINT ( 'NONE',  ( 12.91533473730993009, 41.60535201082149825, -10.88017736071109987 ) ) ;
#8871 = ORIENTED_EDGE ( 'NONE', *, *, #59734, .T. ) ;
#8872 = CARTESIAN_POINT ( 'NONE',  ( 0.6178305044545838731, 54.74863466993042493, 9.382169495545420901 ) ) ;
#8873 = ADVANCED_FACE ( 'NONE', ( #23942, #67461 ), #97982, .T. ) ;
#8874 = CARTESIAN_POINT ( 'NONE',  ( 20.88017736071110164, 50.35535201082151247, 2.915334737309930979 ) ) ;
#8875 = CIRCLE ( 'NONE', #48764, 14.49999999999999822 ) ;
#8876 = ORIENTED_EDGE ( 'NONE', *, *, #68114, .T. ) ;
#8877 = CARTESIAN_POINT ( 'NONE',  ( 15.44008868035555260, 49.73035201082150536, 9.422509992056143702 ) ) ;
#8878 = FILL_AREA_STYLE ('',( #91394 ) ) ;
#8879 = CARTESIAN_POINT ( 'NONE',  ( 1.383448333479224024, 27.37718327197428891, -6.499999999999968026 ) ) ;
#8880 = CARTESIAN_POINT ( 'NONE',  ( -14.47650479471822393, 14.49999999999999112, -3.928206833722243108 ) ) ;
#8881 = CARTESIAN_POINT ( 'NONE',  ( 2.917880565312950480, 60.97041550158063927, -12.26659068614894821 ) ) ;
#8883 = ORIENTED_EDGE ( 'NONE', *, *, #24810, .F. ) ;
#8882 = CARTESIAN_POINT ( 'NONE',  ( 10.00000000000000000, 61.81368534415484106, -10.88017736071110342 ) ) ;
#8884 = CARTESIAN_POINT ( 'NONE',  ( 13.79529636645031943, 5.345415501580634832, -14.16423886937409904 ) ) ;
#8885 = VECTOR ( 'NONE', #1000, 1000.000000000000114 ) ;
#8886 = FILL_AREA_STYLE_COLOUR ( '', #3066 ) ;
#8887 = CARTESIAN_POINT ( 'NONE',  ( 2.035157376598824452, 13.68868534415483751, 7.964842623401179544 ) ) ;
#8888 = CARTESIAN_POINT ( 'NONE',  ( 18.52753015748618282, 33.92559781766745886, -4.923371831947291888 ) ) ;
#8889 = ORIENTED_EDGE ( 'NONE', *, *, #86910, .F. ) ;
#8890 = CARTESIAN_POINT ( 'NONE',  ( 7.361572987183170547, 32.05059781766745175, 9.846743663894590881 ) ) ;
#8891 = CARTESIAN_POINT ( 'NONE',  ( 20.88017736071110164, 35.35535201082150536, 2.915334737309930979 ) ) ;
#8892 = CARTESIAN_POINT ( 'NONE',  ( 1.472469842513823179, 41.42559781766745886, 4.923371831947296329 ) ) ;
#8893 = CARTESIAN_POINT ( 'NONE',  ( 21.09922568453595559, 17.04030133659708923, -6.408140936763230044 ) ) ;
#8894 = CARTESIAN_POINT ( 'NONE',  ( -10.88853822400146676, 46.97908644289115898, 0.000000000000000000 ) ) ;
#8895 = CARTESIAN_POINT ( 'NONE',  ( -0.8801773607110991993, 52.85535201082151247, -2.915334737309923874 ) ) ;
#8896 = CARTESIAN_POINT ( 'NONE',  ( 2.917880565312948704, 57.63708216824731068, 12.26659068614894643 ) ) ;
#8897 = TOROIDAL_SURFACE ( 'NONE', #31234, 9.900000000000002132, 0.1000000000000000056 ) ;
#8898 = CARTESIAN_POINT ( 'NONE',  ( 16.40814093676323893, 15.79030133659708746, 11.09922568453595026 ) ) ;
#8899 = DIRECTION ( 'NONE',  ( -0.000000000000000000, -1.000000000000000000, -0.000000000000000000 ) ) ;
#8900 = ORIENTED_EDGE ( 'NONE', *, *, #86042, .T. ) ;
#8901 = CARTESIAN_POINT ( 'NONE',  ( 3.591859063236761518, 29.95696800326375708, 11.09922568453594849 ) ) ;
#8902 = CARTESIAN_POINT ( 'NONE',  ( -0.8801773607111009756, 23.06368534415484106, 1.068504757029289695E-15 ) ) ;
#8903 = EDGE_CURVE ( 'NONE', #69260, #50813, #83447, .T. ) ;
#8904 = ORIENTED_EDGE ( 'NONE', *, *, #91447, .T. ) ;
#8905 = CARTESIAN_POINT ( 'NONE',  ( -18.89999999999999503, 92.00000000000000000, -8.000000000000000000 ) ) ;
#8906 = CARTESIAN_POINT ( 'NONE',  ( 3.115783986955464435, 4.832823856176936692E-16, 14.16128137375399731 ) ) ;
#8907 = CARTESIAN_POINT ( 'NONE',  ( 19.84674366389459621, 3.508931151000785231, 7.409399052514197653E-17 ) ) ;
#8908 = CARTESIAN_POINT ( 'NONE',  ( 19.84674366389459266, 43.71726448433410894, -2.638427012816827677 ) ) ;
#8909 = CARTESIAN_POINT ( 'NONE',  ( 10.00000000000000178, 42.25893115100078745, 9.846743663894594434 ) ) ;
#8910 = CARTESIAN_POINT ( 'NONE',  ( 10.64017930668211598, 14.49999999999999112, -10.57291749337218256 ) ) ;
#8911 = CARTESIAN_POINT ( 'NONE',  ( 19.39235739573469530, 14.87576471608601203, 6.499999999999995559 ) ) ;
#8912 = CARTESIAN_POINT ( 'NONE',  ( 10.00000000000000178, 27.25893115100078390, 9.846743663894594434 ) ) ;
#8913 = CARTESIAN_POINT ( 'NONE',  ( 0.000000000000000000, -97.00000000000000000, 3.750000000000000000 ) ) ;
#8914 = TOROIDAL_SURFACE ( 'NONE', #98320, 14.49999999999999822, 0.5000000000000000000 ) ;
#8915 = DIRECTION ( 'NONE',  ( -0.06975647374412544122, -0.9975640502598243087, 0.000000000000000000 ) ) ;
#8917 = DIRECTION ( 'NONE',  ( -1.000000000000000000, 0.000000000000000000, 0.000000000000000000 ) ) ;
#8916 = CARTESIAN_POINT ( 'NONE',  ( 19.84674366389459621, 8.508931151000785675, 7.409399052514197653E-17 ) ) ;
#8918 = DIRECTION ( 'NONE',  ( -1.000000000000000000, 3.538835890992686473E-15, 0.000000000000000000 ) ) ;
#8919 = EDGE_CURVE ( 'NONE', #23491, #54920, #44942, .T. ) ;
#8921 = EDGE_LOOP ( 'NONE', ( #20040, #85019, #6689, #74280 ) ) ;
#8920 = CARTESIAN_POINT ( 'NONE',  ( 7.361572987183169658, 39.96726448433411605, -9.846743663894592657 ) ) ;
#8922 = DIRECTION ( 'NONE',  ( 1.000000000000000000, -0.000000000000000000, -0.000000000000000000 ) ) ;
#8923 = CARTESIAN_POINT ( 'NONE',  ( 21.09922568453594849, 6.206968003263753531, 6.408140936763242479 ) ) ;
#8924 = ADVANCED_FACE ( 'NONE', ( #30429 ), #45098, .T. ) ;
#8925 = CARTESIAN_POINT ( 'NONE',  ( 20.88017736071110164, 50.35535201082151247, 2.915334737309930979 ) ) ;
#8927 = ADVANCED_FACE ( 'NONE', ( #45947 ), #30921, .T. ) ;
#8926 = CARTESIAN_POINT ( 'NONE',  ( 2.917880565312948704, 52.63708216824730357, 12.26659068614894643 ) ) ;
#8928 = CARTESIAN_POINT ( 'NONE',  ( -0.9940297508535884674, -0.03417435944610275333, -14.21528771620250886 ) ) ;
#8929 = CARTESIAN_POINT ( 'NONE',  ( -10.88853822400146676, 46.97908644289115898, 0.000000000000000000 ) ) ;
#8930 = CARTESIAN_POINT ( 'NONE',  ( -4.164238869374098151, 46.59541550158063927, -3.795296366450310543 ) ) ;
#8931 = CARTESIAN_POINT ( 'NONE',  ( 24.16423886937409904, 59.09541550158063217, 3.795296366450317205 ) ) ;
#8932 = CARTESIAN_POINT ( 'NONE',  ( -0.3689425029237898834, 26.17874883491396432, -10.36894250292378850 ) ) ;
#8933 = CARTESIAN_POINT ( 'NONE',  ( -4.164238869374099927, 22.01208216824730357, 3.795296366450308767 ) ) ;
#8934 = CARTESIAN_POINT ( 'NONE',  ( -3.881909499400240104, 15.00000000000000178, -14.10103859407600169 ) ) ;
#8936 = CARTESIAN_POINT ( 'NONE',  ( 1.472469842513823179, 36.42559781766745175, 4.923371831947296329 ) ) ;
#8935 = CARTESIAN_POINT ( 'NONE',  ( 4.655929185078333532, -8.243906417220228988, 2.750000000000000000 ) ) ;
#8937 = VERTEX_POINT ( 'NONE', #64366 ) ;
#8938 = CARTESIAN_POINT ( 'NONE',  ( -0.8801773607111009756, 43.06368534415484106, 1.068504757029289695E-15 ) ) ;
#8939 = CARTESIAN_POINT ( 'NONE',  ( 20.10239578412225470, 22.63377557478296964, -6.340343622311920058 ) ) ;
#8940 = CARTESIAN_POINT ( 'NONE',  ( 14.71525861348293063, 0.3639310978437776956, -2.908807992686601285 ) ) ;
#8941 = CARTESIAN_POINT ( 'NONE',  ( 1.472469842513823179, 40.59226448433411605, -4.923371831947296329 ) ) ;
#8942 = CARTESIAN_POINT ( 'NONE',  ( -2.816281873526471635, 58.91530133659707502, -3.434112377981056508 ) ) ;
#8944 = PRESENTATION_LAYER_ASSIGNMENT (  '', '', ( #20144 ) ) ;
#8943 = CARTESIAN_POINT ( 'NONE',  ( -14.16423886937410082, -13.19625116508602680, 4.336808689942017736E-15 ) ) ;
#8945 = CARTESIAN_POINT ( 'NONE',  ( 0.1532563361054100626, 35.80059781766745175, -2.638427012816831230 ) ) ;
#8946 = CARTESIAN_POINT ( 'NONE',  ( 19.84674366389459621, 63.50893115100078745, 7.409399052514197653E-17 ) ) ;
#8947 = COLOUR_RGB ( '', 0.66274510, 0.83137255, 0.94901961) ;
#8948 = CARTESIAN_POINT ( 'NONE',  ( 24.16423886937409904, 34.09541550158064638, 3.795296366450317205 ) ) ;
#8949 = ORIENTED_EDGE ( 'NONE', *, *, #6565, .T. ) ;
#8950 = CARTESIAN_POINT ( 'NONE',  ( -2.266590686148945544, 11.38708216824730179, -7.082119434687050408 ) ) ;
#8951 = VECTOR ( 'NONE', #28893, 1000.000000000000000 ) ;
#8953 = LINE ( 'NONE', #75108, #32798 ) ;
#8952 = CARTESIAN_POINT ( 'NONE',  ( 0.1922240491738397838, 68.18878173731741299, 6.499999999999944933 ) ) ;
#8954 = CARTESIAN_POINT ( 'NONE',  ( 19.42250999205614193, 10.14701867748816966, 5.440088680355555262 ) ) ;
#8955 = CARTESIAN_POINT ( 'NONE',  ( 3.591859063236763294, 13.29030133659708746, -11.09922568453595026 ) ) ;
#8956 = LINE ( 'NONE', #47930, #56057 ) ;
#8957 = CARTESIAN_POINT ( 'NONE',  ( 0.1532563361054100626, 0.8005978176674514168, -2.638427012816831230 ) ) ;
#8958 = ADVANCED_FACE ( 'NONE', ( #86405 ), #92905, .T. ) ;
#8959 = CARTESIAN_POINT ( 'NONE',  ( 0.2751277870542980231, 14.36607318730130878, -6.500000000000002665 ) ) ;
#8960 = DIRECTION ( 'NONE',  ( 0.000000000000000000, 0.000000000000000000, 1.000000000000000000 ) ) ;
#8961 = CARTESIAN_POINT ( 'NONE',  ( 22.26659068614895176, 64.72041550158064638, -7.082119434687042414 ) ) ;
#8962 = DIRECTION ( 'NONE',  ( 0.000000000000000000, 1.000000000000000000, 0.000000000000000000 ) ) ;
#8963 =( BOUNDED_SURFACE ( )  B_SPLINE_SURFACE ( 1, 2, ( 
 ( #23671, #9134, #93615, #8644, #47628, #92146, #86127, #17640, #63600, #31628, #70142, #25633, #2653, #62119, #40132, #24644, #77135, #1663, #86618, #48601, #32112, #62610, #33105, #94105, #92627, #78622, #54133, #84646, #39154, #10133, #55113, #18129, #56123, #85631, #78124, #9634, #70632, #79105, #10617, #69159, #16149, #46633, #69644, #24150, #54618, #85139, #80587, #58066, #34082, #42110, #72572, #65065, #50578, #12082, #87583, #11105, #41129, #73067, #28065, #4603, #65563, #96089, #81073, #12576, #5084, #20581, #64083, #35571, #58562, #89067, #51066, #64573, #91035, #98078, #29047, #97095, #21072, #51570, #15072, #97587, #83052, #29537, #37068, #82056, #28566, #52062, #82557, #14572, #90051, #21574, #74556, #45541, #75049, #90540, #13065, #6558, #36573, #45039, #67566, #74055, #75548, #7064, #68055, #30034, #26912, #34400, #64888, #51392, #41941, #57408, #43390, #12400, #49907, #13391, #5418, #96417, #87415, #95920, #4917, #58380, #80906, #81879, #73887, #43874, #20409, #87900, #35888, #73389, #42906, #50895, #72404, #66384, #65394, #27400, #88900, #64408, #3442, #72898, #81390, #57892, #19415, #89389, #88407, #96918, #28394, #94914, #33900, #42418, #19905, #58888, #50396, #20903, #26413, #80418, #11916, #56914, #18932, #4432, #49410, #34898, #79911, #11419, #13894, #53356, #59374, #67379, #6376, #44378, #38370, #67882, #14894, #44864, #14393, #401, #45364, #74877, #29859, #91859, #36392, #53861, #75367, #83863, #60362, #37394, #84372, #76363, #66886, #75868, #51889, #22389, #90858, #6882, #98404, #36891, #30351, #91358, #97908, #52865, #97404, #22884, #23377, #7389, #60858, #28872, #37887, #82371, #83371, #52372, #68380, #29368, #59870, #7877, #90357, #21895, #15387, #45872, #98899, #68871, #30853, #61350, #15871, #74370, #5897, #89879, #21395, #82878, #62825, #63307, #8844, #54824, #77823, #70346, #93817, #24846, #31829, #16356, #46356, #16849, #71329, #1864, #85336, #78319, #32322, #40340, #93325, #25825, #38866, #47324, #86325, #92833, #9338, #39358, #2848, #17349, #39840, #878, #46837, #77332, #33302, #24361, #2356, #47819, #55328, #54335, #23871, #85835, #9839, #25348, #84849, #70843, #32811, #55831, #62325, #69852, #48310, #17829, #78819, #63794, #94302, #10329, #40828, #56322, #86818, #1375, #76844, #8358, #31338, #92345, #69357, #61838, #71809, #49784, #95796, #57775, #88773, #72285, #57288, #34272, #43270, #49296, #87782, #18814, #80291, #96795, #87295, #42298, #19298, #58258, #3315, #64773, #12283, #56799, #27277, #48802, #42790, #65768, #12773, #79798, #95289, #73765, #20284, #11300, #88281, #72770, #26299 ),
 ( #4307, #10818, #19781, #26791, #5294, #66260, #50269, #3817, #27773, #11790, #34781, #73275, #65268, #28270, #41338, #80786, #50782, #4797, #35273, #96296, #35772, #81273, #58765, #33778, #18321, #79311, #64284, #94797, #179, #15168, #53144, #52166, #82659, #7163, #68166, #61134, #14175, #98686, #37666, #76147, #29639, #44659, #46146, #38163, #76632, #61618, #92136, #75651, #30627, #23661, #84157, #75154, #22668, #6664, #97690, #90150, #37180, #91644, #29152, #30135, #83653, #45649, #15663, #98183, #83154, #60147, #69145, #67673, #14679, #90644, #60641, #54123, #22169, #91142, #45145, #8151, #59659, #52651, #68649, #7672, #23162, #74663, #53637, #38644, #673, #31123, #44155, #6174, #36678, #67166, #86117, #40121, #54609, #24636, #34932, #95953, #62601, #55103, #87936, #19452, #9124, #26945, #8634, #39143, #85125, #95454, #85623, #65429, #42453, #93106, #17140, #9621, #93605, #64926, #40618, #47619, #71117, #4464, #34433, #27434, #25143, #78114, #32607, #57446, #77611, #70622, #2147, #63103, #49946, #55620, #1651, #16636, #16138, #17628, #72935, #48099, #78611, #10120, #39639, #47111, #70130, #57929, #32102, #3965, #80451, #11949, #46624, #77122, #69633, #1157, #31617, #62108, #92618, #51923, #66919, #67916, #59901, #29894, #6412, #81424, #52409, #89912, #97440, #36924, #27924, #82910, #51424, #13424, #82407, #50431, #98438, #58923, #28904, #81914, #73924, #75399, #5934, #67414, #14428, #80940, #88438, #28425, #36426, #13933, #21426, #44409, #6918, #35923, #43422, #44897, #19938, #88931, #74912, #89423, #12433, #42941, #58416, #97942, #73424, #12927, #20441, #50929, #4948, #29400, #96452, #20936, #434, #85372, #31373, #98933, #15900, #77861, #22422, #39874, #61381, #69886, #46391, #23412, #70381, #62358, #52896, #61871, #37922, #8391, #76877, #91890, #53895, #30388, #16389, #77364, #60891, #38901, #83406, #8874, #9372, #92376, #46874, #14928, #23902, #68411, #84401, #38405, #69388, #91390, #15428, #92862, #22919, #53388, #1405, #39392, #68906, #909, #83896, #1900, #54371, #84882, #60397, #31859, #45394, #24392, #7910, #16883, #90894, #54860, #45907, #47361, #76394, #75900, #7425, #30885, #49818, #80327, #63829, #18849, #11827, #72318, #63348, #10854, #93853, #85871, #78357, #25381, #49329, #17383, #94342, #41375, #71842, #3852, #86363, #71369, #48347, #57321, #55865, #2883, #32847, #25860, #42335, #2394, #56356, #33334, #34310, #47852, #78853, #26336, #70877, #3352, #62863, #56834, #79831, #26827, #17862, #10364, #87814, #64807, #40863, #33814, #86852, #40376, #18358, #72807, #32356, #48834, #79346, #95327, #19335 ) ),
 .UNSPECIFIED., .F., .F., .F. ) 
 B_SPLINE_SURFACE_WITH_KNOTS ( ( 2, 2 ),
 ( 3, 2, 2, 2, 2, 2, 2, 2, 2, 2, 2, 2, 2, 2, 2, 2, 2, 2, 2, 2, 2, 2, 2, 2, 2, 2, 2, 2, 2, 2, 2, 2, 2, 2, 2, 2, 2, 2, 2, 2, 2, 2, 2, 2, 2, 2, 2, 2, 2, 2, 2, 2, 2, 2, 2, 2, 2, 2, 2, 2, 2, 2, 2, 2, 2, 2, 2, 2, 2, 2, 2, 2, 2, 2, 2, 2, 2, 2, 2, 2, 2, 2, 2, 2, 2, 2, 2, 2, 2, 2, 2, 2, 2, 2, 2, 2, 2, 2, 2, 2, 2, 2, 2, 2, 2, 2, 2, 2, 2, 2, 2, 2, 2, 2, 2, 2, 2, 2, 2, 2, 2, 2, 2, 2, 2, 2, 2, 2, 2, 2, 2, 2, 2, 2, 2, 2, 2, 2, 2, 2, 2, 2, 2, 2, 2, 2, 2, 2, 2, 2, 2, 2, 2, 2, 2, 2, 2, 2, 2, 2, 2, 2, 3 ),
 ( 0.000000000000000000, 1.000000000000000000 ),
 ( 0.000000000000000000, 0.005952380952380952051, 0.01190476190476190410, 0.01785714285714285615, 0.02380952380952380820, 0.02976190476190476025, 0.03571428571428571230, 0.04166666666666666435, 0.04761904761904761640, 0.05357142857142856845, 0.05952380952380952051, 0.06547619047619047949, 0.07142857142857142461, 0.07738095238095238360, 0.08333333333333332871, 0.08928571428571428770, 0.09523809523809523281, 0.1011904761904761918, 0.1071428571428571369, 0.1130952380952380959, 0.1190476190476190410, 0.1250000000000000000, 0.1309523809523809590, 0.1369047619047619180, 0.1428571428571428492, 0.1488095238095238082, 0.1547619047619047672, 0.1607142857142857262, 0.1666666666666666574, 0.1726190476190476164, 0.1785714285714285754, 0.1845238095238095344, 0.1904761904761904656, 0.1964285714285714246, 0.2023809523809523836, 0.2083333333333333426, 0.2142857142857142738, 0.2202380952380952328, 0.2261904761904761918, 0.2321428571428571508, 0.2380952380952380820, 0.2440476190476190410, 0.2500000000000000000, 0.2559523809523809312, 0.2619047619047619180, 0.2678571428571428492, 0.2738095238095238360, 0.2797619047619047672, 0.2857142857142856984, 0.2916666666666666852, 0.2976190476190476164, 0.3035714285714285476, 0.3095238095238095344, 0.3154761904761904656, 0.3214285714285714524, 0.3273809523809523836, 0.3333333333333333148, 0.3392857142857143016, 0.3452380952380952328, 0.3511904761904761640, 0.3571428571428571508, 0.3630952380952380820, 0.3690476190476190688, 0.3750000000000000000, 0.3809523809523809312, 0.3869047619047619180, 0.3928571428571428492, 0.3988095238095238360, 0.4047619047619047672, 0.4107142857142856984, 0.4166666666666666852, 0.4226190476190476164, 0.4285714285714285476, 0.4345238095238095344, 0.4404761904761904656, 0.4464285714285714524, 0.4523809523809523836, 0.4583333333333333148, 0.4642857142857143016, 0.4702380952380952328, 0.4761904761904761640, 0.4821428571428571508, 0.4880952380952380820, 0.4940476190476190688, 0.5000000000000000000, 0.5059523809523809312, 0.5119047619047618625, 0.5178571428571429047, 0.5238095238095238360, 0.5297619047619047672, 0.5357142857142856984, 0.5416666666666666297, 0.5476190476190476719, 0.5535714285714286031, 0.5595238095238095344, 0.5654761904761904656, 0.5714285714285713969, 0.5773809523809523281, 0.5833333333333333703, 0.5892857142857143016, 0.5952380952380952328, 0.6011904761904761640, 0.6071428571428570953, 0.6130952380952381375, 0.6190476190476190688, 0.6250000000000000000, 0.6309523809523809312, 0.6369047619047618625, 0.6428571428571429047, 0.6488095238095238360, 0.6547619047619047672, 0.6607142857142856984, 0.6666666666666666297, 0.6726190476190476719, 0.6785714285714286031, 0.6845238095238095344, 0.6904761904761904656, 0.6964285714285713969, 0.7023809523809523281, 0.7083333333333333703, 0.7142857142857143016, 0.7202380952380952328, 0.7261904761904761640, 0.7321428571428570953, 0.7380952380952381375, 0.7440476190476190688, 0.7500000000000000000, 0.7559523809523809312, 0.7619047619047618625, 0.7678571428571429047, 0.7738095238095238360, 0.7797619047619047672, 0.7857142857142856984, 0.7916666666666666297, 0.7976190476190476719, 0.8035714285714286031, 0.8095238095238095344, 0.8154761904761904656, 0.8214285714285713969, 0.8273809523809523281, 0.8333333333333333703, 0.8392857142857143016, 0.8452380952380952328, 0.8511904761904761640, 0.8571428571428570953, 0.8630952380952381375, 0.8690476190476190688, 0.8750000000000000000, 0.8809523809523809312, 0.8869047619047618625, 0.8928571428571429047, 0.8988095238095238360, 0.9047619047619047672, 0.9107142857142856984, 0.9166666666666666297, 0.9226190476190476719, 0.9285714285714286031, 0.9345238095238095344, 0.9404761904761904656, 0.9464285714285713969, 0.9523809523809523281, 0.9583333333333333703, 0.9642857142857143016 ),
 .UNSPECIFIED. ) 
 GEOMETRIC_REPRESENTATION_ITEM ( )  RATIONAL_B_SPLINE_SURFACE ( (
 ( 1.000000000000000000, 0.9659258262890683122, 1.000000000000000000, 0.9659258262890683122, 1.000000000000000000, 0.9659258262890683122, 1.000000000000000000, 0.9659258262890683122, 1.000000000000000000, 0.9659258262890683122, 1.000000000000000000, 0.9659258262890683122, 1.000000000000000000, 0.9659258262890683122, 1.000000000000000000, 0.9659258262890683122, 1.000000000000000000, 0.9659258262890683122, 1.000000000000000000, 0.9659258262890683122, 1.000000000000000000, 0.9659258262890683122, 1.000000000000000000, 0.9659258262890683122, 1.000000000000000000, 0.9659258262890683122, 1.000000000000000000, 0.9659258262890683122, 1.000000000000000000, 0.9659258262890683122, 1.000000000000000000, 0.9659258262890683122, 1.000000000000000000, 0.9659258262890683122, 1.000000000000000000, 0.9659258262890683122, 1.000000000000000000, 0.9659258262890683122, 1.000000000000000000, 0.9659258262890683122, 1.000000000000000000, 0.9659258262890683122, 1.000000000000000000, 0.9659258262890683122, 1.000000000000000000, 0.9659258262890683122, 1.000000000000000000, 0.9659258262890683122, 1.000000000000000000, 0.9659258262890683122, 1.000000000000000000, 0.9659258262890683122, 1.000000000000000000, 0.9659258262890683122, 1.000000000000000000, 0.9659258262890683122, 1.000000000000000000, 0.9659258262890683122, 1.000000000000000000, 0.9659258262890683122, 1.000000000000000000, 0.9659258262890683122, 1.000000000000000000, 0.9659258262890683122, 1.000000000000000000, 0.9659258262890683122, 1.000000000000000000, 0.9659258262890683122, 1.000000000000000000, 0.9659258262890683122, 1.000000000000000000, 0.9659258262890683122, 1.000000000000000000, 0.9659258262890683122, 1.000000000000000000, 0.9659258262890683122, 1.000000000000000000, 0.9659258262890683122, 1.000000000000000000, 0.9659258262890683122, 1.000000000000000000, 0.9659258262890683122, 1.000000000000000000, 0.9659258262890683122, 1.000000000000000000, 0.9659258262890683122, 1.000000000000000000, 0.9659258262890683122, 1.000000000000000000, 0.9659258262890683122, 1.000000000000000000, 0.9659258262890683122, 1.000000000000000000, 0.9659258262890683122, 1.000000000000000000, 0.9659258262890683122, 1.000000000000000000, 0.9659258262890683122, 1.000000000000000000, 0.9659258262890683122, 1.000000000000000000, 0.9659258262890683122, 1.000000000000000000, 0.9659258262890683122, 1.000000000000000000, 0.9659258262890683122, 1.000000000000000000, 0.9659258262890683122, 1.000000000000000000, 0.9659258262890683122, 1.000000000000000000, 0.9659258262890683122, 1.000000000000000000, 0.9659258262890683122, 1.000000000000000000, 0.9659258262890683122, 1.000000000000000000, 0.9659258262890683122, 1.000000000000000000, 0.9659258262890683122, 1.000000000000000000, 0.9659258262890683122, 1.000000000000000000, 0.9659258262890683122, 1.000000000000000000, 0.9659258262890683122, 1.000000000000000000, 0.9659258262890683122, 1.000000000000000000, 0.9659258262890683122, 1.000000000000000000, 0.9659258262890683122, 1.000000000000000000, 0.9659258262890683122, 1.000000000000000000, 0.9659258262890683122, 1.000000000000000000, 0.9659258262890683122, 1.000000000000000000, 0.9659258262890683122, 1.000000000000000000, 0.9659258262890683122, 1.000000000000000000, 0.9659258262890683122, 1.000000000000000000, 0.9659258262890683122, 1.000000000000000000, 0.9659258262890683122, 1.000000000000000000, 0.9659258262890683122, 1.000000000000000000, 0.9659258262890683122, 1.000000000000000000, 0.9659258262890683122, 1.000000000000000000, 0.9659258262890683122, 1.000000000000000000, 0.9659258262890683122, 1.000000000000000000, 0.9659258262890683122, 1.000000000000000000, 0.9659258262890683122, 1.000000000000000000, 0.9659258262890683122, 1.000000000000000000, 0.9659258262890683122, 1.000000000000000000, 0.9659258262890683122, 1.000000000000000000, 0.9659258262890683122, 1.000000000000000000, 0.9659258262890683122, 1.000000000000000000, 0.9659258262890683122, 1.000000000000000000, 0.9659258262890683122, 1.000000000000000000, 0.9659258262890683122, 1.000000000000000000, 0.9659258262890683122, 1.000000000000000000, 0.9659258262890683122, 1.000000000000000000, 0.9659258262890683122, 1.000000000000000000, 0.9659258262890683122, 1.000000000000000000, 0.9659258262890683122, 1.000000000000000000, 0.9659258262890683122, 1.000000000000000000, 0.9659258262890683122, 1.000000000000000000, 0.9659258262890683122, 1.000000000000000000, 0.9659258262890683122, 1.000000000000000000, 0.9659258262890683122, 1.000000000000000000, 0.9659258262890683122, 1.000000000000000000, 0.9659258262890683122, 1.000000000000000000, 0.9659258262890683122, 1.000000000000000000, 0.9659258262890683122, 1.000000000000000000, 0.9659258262890683122, 1.000000000000000000, 0.9659258262890683122, 1.000000000000000000, 0.9659258262890683122, 1.000000000000000000, 0.9659258262890683122, 1.000000000000000000, 0.9659258262890683122, 1.000000000000000000, 0.9659258262890683122, 1.000000000000000000, 0.9659258262890683122, 1.000000000000000000, 0.9659258262890683122, 1.000000000000000000, 0.9659258262890683122, 1.000000000000000000, 0.9659258262890683122, 1.000000000000000000, 0.9659258262890683122, 1.000000000000000000, 0.9659258262890683122, 1.000000000000000000, 0.9659258262890683122, 1.000000000000000000, 0.9659258262890683122, 1.000000000000000000, 0.9659258262890683122, 1.000000000000000000, 0.9659258262890683122, 1.000000000000000000, 0.9659258262890683122, 1.000000000000000000, 0.9659258262890683122, 1.000000000000000000, 0.9659258262890683122, 1.000000000000000000, 0.9659258262890683122, 1.000000000000000000, 0.9659258262890683122, 1.000000000000000000, 0.9659258262890683122, 1.000000000000000000, 0.9659258262890683122, 1.000000000000000000, 0.9659258262890683122, 1.000000000000000000, 0.9659258262890683122, 1.000000000000000000, 0.9659258262890683122, 1.000000000000000000, 0.9659258262890683122, 1.000000000000000000, 0.9659258262890683122, 1.000000000000000000, 0.9659258262890683122, 1.000000000000000000, 0.9659258262890683122, 1.000000000000000000, 0.9659258262890683122, 1.000000000000000000, 0.9659258262890683122, 1.000000000000000000, 0.9659258262890683122, 1.000000000000000000, 0.9659258262890683122, 1.000000000000000000, 0.9659258262890683122, 1.000000000000000000, 0.9659258262890683122, 1.000000000000000000, 0.9659258262890683122, 1.000000000000000000, 0.9659258262890683122, 1.000000000000000000, 0.9659258262890683122, 1.000000000000000000, 0.9659258262890683122, 1.000000000000000000, 0.9659258262890683122, 1.000000000000000000, 0.9659258262890683122, 1.000000000000000000, 0.9659258262890683122, 1.000000000000000000, 0.9659258262890683122, 1.000000000000000000, 0.9659258262890683122, 1.000000000000000000, 0.9659258262890683122, 1.000000000000000000, 0.9659258262890683122, 1.000000000000000000, 0.9659258262890683122, 1.000000000000000000, 0.9659258262890683122, 1.000000000000000000, 0.9659258262890683122, 1.000000000000000000, 0.9659258262890683122, 1.000000000000000000, 0.9659258262890683122, 1.000000000000000000, 0.9659258262890683122, 1.000000000000000000, 0.9659258262890683122, 1.000000000000000000, 0.9659258262890683122, 1.000000000000000000, 0.9659258262890683122, 1.000000000000000000, 0.9659258262890683122, 1.000000000000000000, 0.9659258262890683122, 1.000000000000000000, 0.9659258262890683122, 1.000000000000000000),
 ( 1.000000000000000000, 0.9659258262890683122, 1.000000000000000000, 0.9659258262890683122, 1.000000000000000000, 0.9659258262890683122, 1.000000000000000000, 0.9659258262890683122, 1.000000000000000000, 0.9659258262890683122, 1.000000000000000000, 0.9659258262890683122, 1.000000000000000000, 0.9659258262890683122, 1.000000000000000000, 0.9659258262890683122, 1.000000000000000000, 0.9659258262890683122, 1.000000000000000000, 0.9659258262890683122, 1.000000000000000000, 0.9659258262890683122, 1.000000000000000000, 0.9659258262890683122, 1.000000000000000000, 0.9659258262890683122, 1.000000000000000000, 0.9659258262890683122, 1.000000000000000000, 0.9659258262890683122, 1.000000000000000000, 0.9659258262890683122, 1.000000000000000000, 0.9659258262890683122, 1.000000000000000000, 0.9659258262890683122, 1.000000000000000000, 0.9659258262890683122, 1.000000000000000000, 0.9659258262890683122, 1.000000000000000000, 0.9659258262890683122, 1.000000000000000000, 0.9659258262890683122, 1.000000000000000000, 0.9659258262890683122, 1.000000000000000000, 0.9659258262890683122, 1.000000000000000000, 0.9659258262890683122, 1.000000000000000000, 0.9659258262890683122, 1.000000000000000000, 0.9659258262890683122, 1.000000000000000000, 0.9659258262890683122, 1.000000000000000000, 0.9659258262890683122, 1.000000000000000000, 0.9659258262890683122, 1.000000000000000000, 0.9659258262890683122, 1.000000000000000000, 0.9659258262890683122, 1.000000000000000000, 0.9659258262890683122, 1.000000000000000000, 0.9659258262890683122, 1.000000000000000000, 0.9659258262890683122, 1.000000000000000000, 0.9659258262890683122, 1.000000000000000000, 0.9659258262890683122, 1.000000000000000000, 0.9659258262890683122, 1.000000000000000000, 0.9659258262890683122, 1.000000000000000000, 0.9659258262890683122, 1.000000000000000000, 0.9659258262890683122, 1.000000000000000000, 0.9659258262890683122, 1.000000000000000000, 0.9659258262890683122, 1.000000000000000000, 0.9659258262890683122, 1.000000000000000000, 0.9659258262890683122, 1.000000000000000000, 0.9659258262890683122, 1.000000000000000000, 0.9659258262890683122, 1.000000000000000000, 0.9659258262890683122, 1.000000000000000000, 0.9659258262890683122, 1.000000000000000000, 0.9659258262890683122, 1.000000000000000000, 0.9659258262890683122, 1.000000000000000000, 0.9659258262890683122, 1.000000000000000000, 0.9659258262890683122, 1.000000000000000000, 0.9659258262890683122, 1.000000000000000000, 0.9659258262890683122, 1.000000000000000000, 0.9659258262890683122, 1.000000000000000000, 0.9659258262890683122, 1.000000000000000000, 0.9659258262890683122, 1.000000000000000000, 0.9659258262890683122, 1.000000000000000000, 0.9659258262890683122, 1.000000000000000000, 0.9659258262890683122, 1.000000000000000000, 0.9659258262890683122, 1.000000000000000000, 0.9659258262890683122, 1.000000000000000000, 0.9659258262890683122, 1.000000000000000000, 0.9659258262890683122, 1.000000000000000000, 0.9659258262890683122, 1.000000000000000000, 0.9659258262890683122, 1.000000000000000000, 0.9659258262890683122, 1.000000000000000000, 0.9659258262890683122, 1.000000000000000000, 0.9659258262890683122, 1.000000000000000000, 0.9659258262890683122, 1.000000000000000000, 0.9659258262890683122, 1.000000000000000000, 0.9659258262890683122, 1.000000000000000000, 0.9659258262890683122, 1.000000000000000000, 0.9659258262890683122, 1.000000000000000000, 0.9659258262890683122, 1.000000000000000000, 0.9659258262890683122, 1.000000000000000000, 0.9659258262890683122, 1.000000000000000000, 0.9659258262890683122, 1.000000000000000000, 0.9659258262890683122, 1.000000000000000000, 0.9659258262890683122, 1.000000000000000000, 0.9659258262890683122, 1.000000000000000000, 0.9659258262890683122, 1.000000000000000000, 0.9659258262890683122, 1.000000000000000000, 0.9659258262890683122, 1.000000000000000000, 0.9659258262890683122, 1.000000000000000000, 0.9659258262890683122, 1.000000000000000000, 0.9659258262890683122, 1.000000000000000000, 0.9659258262890683122, 1.000000000000000000, 0.9659258262890683122, 1.000000000000000000, 0.9659258262890683122, 1.000000000000000000, 0.9659258262890683122, 1.000000000000000000, 0.9659258262890683122, 1.000000000000000000, 0.9659258262890683122, 1.000000000000000000, 0.9659258262890683122, 1.000000000000000000, 0.9659258262890683122, 1.000000000000000000, 0.9659258262890683122, 1.000000000000000000, 0.9659258262890683122, 1.000000000000000000, 0.9659258262890683122, 1.000000000000000000, 0.9659258262890683122, 1.000000000000000000, 0.9659258262890683122, 1.000000000000000000, 0.9659258262890683122, 1.000000000000000000, 0.9659258262890683122, 1.000000000000000000, 0.9659258262890683122, 1.000000000000000000, 0.9659258262890683122, 1.000000000000000000, 0.9659258262890683122, 1.000000000000000000, 0.9659258262890683122, 1.000000000000000000, 0.9659258262890683122, 1.000000000000000000, 0.9659258262890683122, 1.000000000000000000, 0.9659258262890683122, 1.000000000000000000, 0.9659258262890683122, 1.000000000000000000, 0.9659258262890683122, 1.000000000000000000, 0.9659258262890683122, 1.000000000000000000, 0.9659258262890683122, 1.000000000000000000, 0.9659258262890683122, 1.000000000000000000, 0.9659258262890683122, 1.000000000000000000, 0.9659258262890683122, 1.000000000000000000, 0.9659258262890683122, 1.000000000000000000, 0.9659258262890683122, 1.000000000000000000, 0.9659258262890683122, 1.000000000000000000, 0.9659258262890683122, 1.000000000000000000, 0.9659258262890683122, 1.000000000000000000, 0.9659258262890683122, 1.000000000000000000, 0.9659258262890683122, 1.000000000000000000, 0.9659258262890683122, 1.000000000000000000, 0.9659258262890683122, 1.000000000000000000, 0.9659258262890683122, 1.000000000000000000, 0.9659258262890683122, 1.000000000000000000, 0.9659258262890683122, 1.000000000000000000, 0.9659258262890683122, 1.000000000000000000, 0.9659258262890683122, 1.000000000000000000, 0.9659258262890683122, 1.000000000000000000, 0.9659258262890683122, 1.000000000000000000, 0.9659258262890683122, 1.000000000000000000, 0.9659258262890683122, 1.000000000000000000, 0.9659258262890683122, 1.000000000000000000, 0.9659258262890683122, 1.000000000000000000, 0.9659258262890683122, 1.000000000000000000, 0.9659258262890683122, 1.000000000000000000, 0.9659258262890683122, 1.000000000000000000, 0.9659258262890683122, 1.000000000000000000, 0.9659258262890683122, 1.000000000000000000, 0.9659258262890683122, 1.000000000000000000, 0.9659258262890683122, 1.000000000000000000, 0.9659258262890683122, 1.000000000000000000, 0.9659258262890683122, 1.000000000000000000, 0.9659258262890683122, 1.000000000000000000, 0.9659258262890683122, 1.000000000000000000, 0.9659258262890683122, 1.000000000000000000, 0.9659258262890683122, 1.000000000000000000, 0.9659258262890683122, 1.000000000000000000, 0.9659258262890683122, 1.000000000000000000, 0.9659258262890683122, 1.000000000000000000, 0.9659258262890683122, 1.000000000000000000, 0.9659258262890683122, 1.000000000000000000, 0.9659258262890683122, 1.000000000000000000, 0.9659258262890683122, 1.000000000000000000, 0.9659258262890683122, 1.000000000000000000, 0.9659258262890683122, 1.000000000000000000, 0.9659258262890683122, 1.000000000000000000, 0.9659258262890683122, 1.000000000000000000, 0.9659258262890683122, 1.000000000000000000) ) ) 
 REPRESENTATION_ITEM ( '' )  SURFACE ( )  );
#8964 = CARTESIAN_POINT ( 'NONE',  ( 20.88017736071110875, 30.77201867748816966, -2.915334737309920765 ) ) ;
#8965 = CARTESIAN_POINT ( 'NONE',  ( 2.035157376598824452, 28.68868534415484106, 7.964842623401179544 ) ) ;
#8966 = CARTESIAN_POINT ( 'NONE',  ( 13.43411237798106583, 2.665301336597086568, -12.81628187352647252 ) ) ;
#8967 = CARTESIAN_POINT ( 'NONE',  ( 2.791683348922237240, 55.38393115100078745, -7.208316651077763204 ) ) ;
#8968 = CARTESIAN_POINT ( 'NONE',  ( 3.591859063236763294, 58.29030133659708923, -11.09922568453595026 ) ) ;
#8969 = DIRECTION ( 'NONE',  ( -0.9975640502598257520, 0.06975647374410356982, 0.000000000000000000 ) ) ;
#8970 = ORIENTED_EDGE ( 'NONE', *, *, #78248, .F. ) ;
#8971 = CARTESIAN_POINT ( 'NONE',  ( 15.44008868035555260, 24.73035201082150891, 9.422509992056143702 ) ) ;
#8972 = CARTESIAN_POINT ( 'NONE',  ( 19.38216949554541202, 30.99863466993042138, 9.382169495545424454 ) ) ;
#8973 = CARTESIAN_POINT ( 'NONE',  ( 19.05914839598885635, 34.96693863883976405, 6.499999999999962697 ) ) ;
#8974 = CARTESIAN_POINT ( 'NONE',  ( 17.20831665107776587, 57.88393115100078745, 7.208316651077764980 ) ) ;
#8975 = CARTESIAN_POINT ( 'NONE',  ( 10.00000000000000178, 44.31368534415484106, 10.88017736071110342 ) ) ;
#8976 = CARTESIAN_POINT ( 'NONE',  ( 17.20831665107776587, 17.88393115100078745, 7.208316651077764980 ) ) ;
#8977 = CARTESIAN_POINT ( 'NONE',  ( 16.40814093676324603, 17.45696800326375353, -11.09922568453594671 ) ) ;
#8979 = CARTESIAN_POINT ( 'NONE',  ( 19.42250999205614548, 15.98035201082150714, -5.440088680355545492 ) ) ;
#8978 = CARTESIAN_POINT ( 'NONE',  ( 7.084665262690076126, 62.02201867748816966, -10.88017736071110164 ) ) ;
#8980 = FILL_AREA_STYLE_COLOUR ( '', #13029 ) ;
#8981 = VERTEX_POINT ( 'NONE', #33857 ) ;
#8982 = CARTESIAN_POINT ( 'NONE',  ( 0.5774900079438607392, 48.48035201082150536, 5.440088680355550821 ) ) ;
#8983 = CARTESIAN_POINT ( 'NONE',  ( 19.39235739573469175, 24.87576471608601381, 6.499999999999993783 ) ) ;
#8984 = CARTESIAN_POINT ( 'NONE',  ( -0.8801773607111009756, 43.06368534415484106, 1.068504757029289695E-15 ) ) ;
#8986 = CARTESIAN_POINT ( 'NONE',  ( 24.16423886937410614, 9.512082168247301794, -3.795296366450302550 ) ) ;
#8985 = CARTESIAN_POINT ( 'NONE',  ( 16.40814093676324603, 47.45696800326375353, -11.09922568453594671 ) ) ;
#8987 = CARTESIAN_POINT ( 'NONE',  ( 18.52753015748617571, 23.09226448433411960, 4.923371831947298993 ) ) ;
#8988 = CARTESIAN_POINT ( 'NONE',  ( 20.88017736071110164, 10.35535201082150714, 2.915334737309930979 ) ) ;
#8989 = CARTESIAN_POINT ( 'NONE',  ( 7.361572987183170547, 17.05059781766745530, 9.846743663894590881 ) ) ;
#8990 = DIRECTION ( 'NONE',  ( 0.000000000000000000, 1.000000000000000000, 0.000000000000000000 ) ) ;
#8991 = CARTESIAN_POINT ( 'NONE',  ( 24.16423886937410614, 59.30374883491397497, 8.672049930838204340E-16 ) ) ;
#8992 = ORIENTED_EDGE ( 'NONE', *, *, #52734, .F. ) ;
#8993 = VECTOR ( 'NONE', #41411, 1000.000000000000000 ) ;
#8994 = LINE ( 'NONE', #54485, #76168 ) ;
#8995 = CARTESIAN_POINT ( 'NONE',  ( 20.15039907845753220, 46.74884699246888431, 6.262539305110077947 ) ) ;
#8996 = EDGE_LOOP ( 'NONE', ( #98076, #95760, #52171, #44849, #12868, #43804 ) ) ;
#8997 = ORIENTED_EDGE ( 'NONE', *, *, #63713, .F. ) ;
#8998 = CARTESIAN_POINT ( 'NONE',  ( 17.96484262340118221, 11.18868534415484106, -7.964842623401177768 ) ) ;
#8999 = CARTESIAN_POINT ( 'NONE',  ( 19.42250999205614193, 5.147018677488171434, 5.440088680355555262 ) ) ;
#9000 = CARTESIAN_POINT ( 'NONE',  ( 14.92337183194729633, 42.67559781766745886, 8.527530157486181039 ) ) ;
#9001 = CARTESIAN_POINT ( 'NONE',  ( 16.40814093676324603, 42.45696800326375353, -11.09922568453594671 ) ) ;
#9002 = CARTESIAN_POINT ( 'NONE',  ( 20.04068437667222469, 64.71974360917720048, 6.396802510829778576 ) ) ;
#9004 = CARTESIAN_POINT ( 'NONE',  ( 24.16423886937409904, 14.09541550158063217, 3.795296366450317205 ) ) ;
#9003 = CARTESIAN_POINT ( 'NONE',  ( 0.000000000000000000, 15.00000000000000000, 0.000000000000000000 ) ) ;
#9005 = CARTESIAN_POINT ( 'NONE',  ( 19.42250999205614548, 30.98035201082150536, -5.440088680355545492 ) ) ;
#9006 = CARTESIAN_POINT ( 'NONE',  ( 6.204703633549690345, 65.76208216824731778, -14.16423886937410259 ) ) ;
#9007 = CARTESIAN_POINT ( 'NONE',  ( 12.63842701281683034, 42.46726448433412315, 9.846743663894596210 ) ) ;
#9008 = LINE ( 'NONE', #91534, #34860 ) ;
#9009 = CARTESIAN_POINT ( 'NONE',  ( 0.1532563361054082862, 41.21726448433411605, 2.638427012816831674 ) ) ;
#9010 = CARTESIAN_POINT ( 'NONE',  ( 2.791683348922237240, 0.3839311510007847872, -7.208316651077763204 ) ) ;
#9011 = CARTESIAN_POINT ( 'NONE',  ( 7.208316651077764980, 27.88393115100078745, 7.208316651077762316 ) ) ;
#9012 = VERTEX_POINT ( 'NONE', #10893 ) ;
#9013 = CARTESIAN_POINT ( 'NONE',  ( 20.88017736071110164, 5.355352010821502695, 2.915334737309930979 ) ) ;
#9014 = CARTESIAN_POINT ( 'NONE',  ( 15.44008868035555260, 64.73035201082151957, 9.422509992056143702 ) ) ;
#9015 = CARTESIAN_POINT ( 'NONE',  ( 2.791683348922240793, 56.63393115100078035, 7.208316651077764092 ) ) ;
#9017 = CARTESIAN_POINT ( 'NONE',  ( 20.88017736071110519, 45.56368534415484106, 2.639326808657452039E-16 ) ) ;
#9016 = CARTESIAN_POINT ( 'NONE',  ( 7.084665262690076126, 47.02201867748818387, -10.88017736071110164 ) ) ;
#9019 = CARTESIAN_POINT ( 'NONE',  ( 10.00000000000000000, 27.87363466993042138, -12.81628187352647608 ) ) ;
#9018 = CARTESIAN_POINT ( 'NONE',  ( 19.42250999205614548, 10.98035201082150358, -5.440088680355545492 ) ) ;
#9020 = CARTESIAN_POINT ( 'NONE',  ( -0.3689425029237881626, 22.42874883491397142, 10.36894250292379027 ) ) ;
#9021 = EDGE_CURVE ( 'NONE', #97143, #17007, #48391, .T. ) ;
#9022 = AXIS2_PLACEMENT_3D ( 'NONE', #57762, #72757, #11777 ) ;
#9023 = CIRCLE ( 'NONE', #80892, 0.5000000000000004441 ) ;
#9024 = VERTEX_POINT ( 'NONE', #62901 ) ;
#9026 = CARTESIAN_POINT ( 'NONE',  ( -2.816281873526473856, 49.33196800326374643, 3.434112377981055619 ) ) ;
#9025 = VECTOR ( 'NONE', #76551, 1000.000000000000114 ) ;
#9027 = VERTEX_POINT ( 'NONE', #47401 ) ;
#9028 = CARTESIAN_POINT ( 'NONE',  ( 12.63842701281683034, 57.46726448433411605, 9.846743663894596210 ) ) ;
#9029 = CARTESIAN_POINT ( 'NONE',  ( 20.88017736071110164, 15.35535201082150358, 2.915334737309930979 ) ) ;
#9030 = ORIENTED_EDGE ( 'NONE', *, *, #22024, .T. ) ;
#9031 = CARTESIAN_POINT ( 'NONE',  ( 19.42250999205614193, 20.14701867748817321, 5.440088680355555262 ) ) ;
#9032 = ORIENTED_EDGE ( 'NONE', *, *, #77438, .F. ) ;
#9033 = CARTESIAN_POINT ( 'NONE',  ( 17.96484262340118221, 64.93868534415483396, 7.964842623401181321 ) ) ;
#9034 = FILL_AREA_STYLE ('',( #69547 ) ) ;
#9035 = CARTESIAN_POINT ( 'NONE',  ( 10.00000000000000000, 9.758931151000785675, -9.846743663894594434 ) ) ;
#9036 = EDGE_CURVE ( 'NONE', #59690, #23318, #47308, .T. ) ;
#9037 = CARTESIAN_POINT ( 'NONE',  ( 0.5774900079438607392, 68.48035201082150536, 5.440088680355550821 ) ) ;
#9038 = COLOUR_RGB ( '', 0.66274510, 0.83137255, 0.94901961) ;
#9039 = CARTESIAN_POINT ( 'NONE',  ( -12.84737282370062061, 15.00000000000000000, -9.530079116402557560 ) ) ;
#9041 = CARTESIAN_POINT ( 'NONE',  ( -46.94000000000001194, 100.3306229069515325, 9.153711987617667134 ) ) ;
#9040 = CIRCLE ( 'NONE', #36157, 15.00000000000000000 ) ;
#9043 = VERTEX_POINT ( 'NONE', #63391 ) ;
#9042 = CARTESIAN_POINT ( 'NONE',  ( 1.472469842513823179, 11.42559781766745175, 4.923371831947296329 ) ) ;
#9044 = STYLED_ITEM ( 'NONE', ( #2184 ), #72298 ) ;
#9045 = EDGE_CURVE ( 'NONE', #37066, #82533, #22792, .T. ) ;
#9046 = TOROIDAL_SURFACE ( 'NONE', #77698, 14.49999999999999822, 0.5000000000000000000 ) ;
#9047 = CARTESIAN_POINT ( 'NONE',  ( 10.00000000000000000, 44.75893115100078745, -9.846743663894594434 ) ) ;
#9048 = EDGE_LOOP ( 'NONE', ( #74803, #17346, #36868, #88710 ) ) ;
#9049 = DIRECTION ( 'NONE',  ( 1.257568779154408793E-17, 1.000000000000000000, -0.000000000000000000 ) ) ;
#9051 = ADVANCED_FACE ( 'NONE', ( #39433 ), #31747, .T. ) ;
#9050 = CARTESIAN_POINT ( 'NONE',  ( 2.917880565312948704, 7.637082168247301794, 12.26659068614894643 ) ) ;
#9052 = CARTESIAN_POINT ( 'NONE',  ( 13.43411237798106583, 62.66530133659708923, -12.81628187352647252 ) ) ;
#9053 = CARTESIAN_POINT ( 'NONE',  ( -2.266590686148945544, 1.387082168247301128, -7.082119434687050408 ) ) ;
#9054 = CARTESIAN_POINT ( 'NONE',  ( 24.16423886937409904, 14.09541550158063217, 3.795296366450317205 ) ) ;
#9055 =( LENGTH_UNIT ( ) NAMED_UNIT ( * ) SI_UNIT ( .MILLI., .METRE. ) );
#9057 = CARTESIAN_POINT ( 'NONE',  ( 2.035157376598822676, 62.43868534415483396, -7.964842623401177768 ) ) ;
#9056 = DIRECTION ( 'NONE',  ( -0.000000000000000000, -0.000000000000000000, 1.000000000000000000 ) ) ;
#9058 = CARTESIAN_POINT ( 'NONE',  ( 17.96484262340118221, 14.93868534415484106, 7.964842623401181321 ) ) ;
#9059 = CARTESIAN_POINT ( 'NONE',  ( 1.472469842513823179, 66.42559781766745175, 4.923371831947296329 ) ) ;
#9060 = ORIENTED_EDGE ( 'NONE', *, *, #95734, .T. ) ;
#9061 = CARTESIAN_POINT ( 'NONE',  ( 10.00000000000000178, 7.258931151000785675, 9.846743663894594434 ) ) ;
#9062 = CARTESIAN_POINT ( 'NONE',  ( 18.52753015748617571, 8.092264484334117824, 4.923371831947298993 ) ) ;
#9063 = COLOUR_RGB ( '', 0.09019608, 0.27058824, 0.51372549) ;
#9064 = CARTESIAN_POINT ( 'NONE',  ( 13.43411237798105340, 30.58196800326374998, 12.81628187352647963 ) ) ;
#9065 = CARTESIAN_POINT ( 'NONE',  ( 0.1532563361054082862, 26.21726448433411605, 2.638427012816831674 ) ) ;
#9066 = FACE_OUTER_BOUND ( 'NONE', #94299, .T. ) ;
#9067 = CARTESIAN_POINT ( 'NONE',  ( 22.81628187352648496, 16.83196800326374998, -3.434112377981050290 ) ) ;
#9068 = LINE ( 'NONE', #94041, #16017 ) ;
#9069 = CARTESIAN_POINT ( 'NONE',  ( 7.361572987183170547, 2.050597817667451750, 9.846743663894590881 ) ) ;
#9070 = ORIENTED_EDGE ( 'NONE', *, *, #41733, .T. ) ;
#9071 = COLOUR_RGB ( '', 0.66274510, 0.83137255, 0.94901961) ;
#9072 = CARTESIAN_POINT ( 'NONE',  ( 4.559911319644449179, 42.23035201082151247, -9.422509992056141925 ) ) ;
#9073 = CARTESIAN_POINT ( 'NONE',  ( -2.266590686148945544, 31.38708216824730002, -7.082119434687050408 ) ) ;
#9074 = CARTESIAN_POINT ( 'NONE',  ( 14.92337183194729633, 37.67559781766745175, 8.527530157486181039 ) ) ;
#9075 = CARTESIAN_POINT ( 'NONE',  ( 19.84674366389459621, 3.508931151000785231, 7.409399052514197653E-17 ) ) ;
#9077 = CARTESIAN_POINT ( 'NONE',  ( 14.62617646268087768, 0.5000000000000004441, -3.327906561566883692 ) ) ;
#9076 = CARTESIAN_POINT ( 'NONE',  ( 22.81628187352647785, 56.62363466993042493, 6.195893100308588602E-16 ) ) ;
#9078 = CARTESIAN_POINT ( 'NONE',  ( 7.084665262690076126, 24.10535201082150181, 10.88017736071109987 ) ) ;
#9079 = ADVANCED_FACE ( 'NONE', ( #7194 ), #91674, .T. ) ;
#9080 = DIRECTION ( 'NONE',  ( 0.000000000000000000, 0.000000000000000000, -1.000000000000000000 ) ) ;
#9081 = CARTESIAN_POINT ( 'NONE',  ( 0.6178305044545818747, 8.498634669930421381, -9.382169495545419124 ) ) ;
#9082 = CARTESIAN_POINT ( 'NONE',  ( 5.076628168052703671, 41.84226448433411605, 8.527530157486179263 ) ) ;
#9083 = CARTESIAN_POINT ( 'NONE',  ( 5.440088680355556150, 4.730352010821510689, 9.422509992056138373 ) ) ;
#9084 = CARTESIAN_POINT ( 'NONE',  ( 3.591859063236761518, 54.95696800326376064, 11.09922568453594849 ) ) ;
#9085 =( NAMED_UNIT ( * ) SI_UNIT ( $, .STERADIAN. ) SOLID_ANGLE_UNIT ( ) );
#9087 = DIRECTION ( 'NONE',  ( -0.06975647374412544122, -0.9975640502598241977, 0.000000000000000000 ) ) ;
#9086 = CARTESIAN_POINT ( 'NONE',  ( 0.5774900079438590739, 57.64701867748817676, -5.440088680355550821 ) ) ;
#9088 = CARTESIAN_POINT ( 'NONE',  ( 8.209432707284774366, 14.49999999999999822, 12.55409154915492032 ) ) ;
#9089 = CARTESIAN_POINT ( 'NONE',  ( 4.629999999999994564, 43.00000000000000711, -4.000000000000000000 ) ) ;
#9090 = CARTESIAN_POINT ( 'NONE',  ( 4.559911319644449179, 53.89701867748817676, 9.422509992056141925 ) ) ;
#9091 = CARTESIAN_POINT ( 'NONE',  ( 15.44008868035555260, 54.73035201082150536, 9.422509992056143702 ) ) ;
#9092 = LINE ( 'NONE', #70096, #42535 ) ;
#9093 = LINE ( 'NONE', #56563, #33146 ) ;
#9094 = VECTOR ( 'NONE', #93648, 1000.000000000000000 ) ;
#9095 = CARTESIAN_POINT ( 'NONE',  ( 10.00000000000000178, 9.313685344154839285, 10.88017736071110342 ) ) ;
#9096 = CARTESIAN_POINT ( 'NONE',  ( 0.1532563361054100626, 50.80059781766745175, -2.638427012816831230 ) ) ;
#9098 = CARTESIAN_POINT ( 'NONE',  ( -10.27191093752570339, 9.232659125071871724E-16, 10.41278984915619432 ) ) ;
#9097 = CARTESIAN_POINT ( 'NONE',  ( 19.42250999205614193, 20.14701867748817321, 5.440088680355555262 ) ) ;
#9099 = CARTESIAN_POINT ( 'NONE',  ( -2.816281873526471635, 28.91530133659708213, -3.434112377981056508 ) ) ;
#9100 = ORIENTED_EDGE ( 'NONE', *, *, #47309, .T. ) ;
#9101 = CARTESIAN_POINT ( 'NONE',  ( 15.44008868035555793, 36.39701867748816966, -9.422509992056140149 ) ) ;
#9103 = CARTESIAN_POINT ( 'NONE',  ( 8.880000000000020322, 80.07179676972448590, -6.250000000000000000 ) ) ;
#9102 = CARTESIAN_POINT ( 'NONE',  ( 21.09922568453595559, 12.04030133659708746, -6.408140936763230044 ) ) ;
#9104 = CARTESIAN_POINT ( 'NONE',  ( 20.88017736071110164, 10.35535201082150714, 2.915334737309930979 ) ) ;
#9105 = CARTESIAN_POINT ( 'NONE',  ( 4.559911319644449179, 42.23035201082151247, -9.422509992056141925 ) ) ;
#9106 = CARTESIAN_POINT ( 'NONE',  ( -0.3689425029237881626, 47.42874883491396787, 10.36894250292379027 ) ) ;
#9107 = CARTESIAN_POINT ( 'NONE',  ( 17.20831665107776587, 29.13393115100078390, -7.208316651077762316 ) ) ;
#9108 = CARTESIAN_POINT ( 'NONE',  ( 7.084665262690076126, 62.02201867748816966, -10.88017736071110164 ) ) ;
#9109 = LINE ( 'NONE', #39623, #87335 ) ;
#9110 = CARTESIAN_POINT ( 'NONE',  ( 13.79529636645030344, 23.26208216824730002, 14.16423886937410614 ) ) ;
#9111 = AXIS2_PLACEMENT_3D ( 'NONE', #63896, #49887, #94409 ) ;
#9112 = SURFACE_SIDE_STYLE ('',( #54110 ) ) ;
#9113 = CARTESIAN_POINT ( 'NONE',  ( 1.932340009482153231, 21.49127512925448613, -6.500000000000008882 ) ) ;
#9114 = EDGE_LOOP ( 'NONE', ( #44094, #24276, #13831, #44125 ) ) ;
#9115 = ORIENTED_EDGE ( 'NONE', *, *, #59622, .T. ) ;
#9116 = CARTESIAN_POINT ( 'NONE',  ( 13.79529636645031943, 40.34541550158063217, -14.16423886937409904 ) ) ;
#9117 = CARTESIAN_POINT ( 'NONE',  ( -2.266590686148945544, 31.38708216824730002, -7.082119434687050408 ) ) ;
#9118 = CARTESIAN_POINT ( 'NONE',  ( 5.076628168052704559, 0.1755978176674514724, -8.527530157486179263 ) ) ;
#9119 = CARTESIAN_POINT ( 'NONE',  ( 18.52753015748618282, 63.92559781766745886, -4.923371831947291888 ) ) ;
#9120 = CARTESIAN_POINT ( 'NONE',  ( -18.89999999999999503, 98.99999999999998579, -7.750000000000000000 ) ) ;
#9122 = CARTESIAN_POINT ( 'NONE',  ( 10.00000000000000000, 22.87363466993042138, -12.81628187352647608 ) ) ;
#9121 = CARTESIAN_POINT ( 'NONE',  ( 20.88017736071110164, 60.35535201082151957, 2.915334737309930979 ) ) ;
#9123 = CARTESIAN_POINT ( 'NONE',  ( -2.266590686148945544, 36.38708216824730357, -7.082119434687050408 ) ) ;
#9124 = CARTESIAN_POINT ( 'NONE',  ( 0.5774900079438590739, 22.64701867748817321, -5.440088680355550821 ) ) ;
#9125 = CARTESIAN_POINT ( 'NONE',  ( 10.00000000000000000, 26.81368534415484106, -10.88017736071110342 ) ) ;
#9126 = DIRECTION ( 'NONE',  ( 0.000000000000000000, -1.000000000000000000, 0.000000000000000000 ) ) ;
#9127 = CARTESIAN_POINT ( 'NONE',  ( 4.923371831947295441, -15.65773551566587685, -8.527530157486179263 ) ) ;
#9128 = EDGE_CURVE ( 'NONE', #37577, #2183, #21709, .T. ) ;
#9129 = ORIENTED_EDGE ( 'NONE', *, *, #54687, .F. ) ;
#9130 = CARTESIAN_POINT ( 'NONE',  ( 19.72487221294570858, 0.5000000000000000000, 6.500000000000000888 ) ) ;
#9131 = VERTEX_POINT ( 'NONE', #23193 ) ;
#9132 = DIRECTION ( 'NONE',  ( -1.000000000000000000, -0.000000000000000000, -0.000000000000000000 ) ) ;
#9133 = ORIENTED_EDGE ( 'NONE', *, *, #86940, .F. ) ;
#9134 = CARTESIAN_POINT ( 'NONE',  ( 6.204703633549690345, 0.7620821682473009062, -14.16423886937410259 ) ) ;
#9136 = CARTESIAN_POINT ( 'NONE',  ( 19.42250999205614193, 15.14701867748817143, 5.440088680355555262 ) ) ;
#9135 = CARTESIAN_POINT ( 'NONE',  ( 24.16423886937410614, 54.30374883491396787, 8.672049930838204340E-16 ) ) ;
#9138 = CARTESIAN_POINT ( 'NONE',  ( 18.52753015748618282, 58.92559781766745886, -4.923371831947291888 ) ) ;
#9137 = CARTESIAN_POINT ( 'NONE',  ( 7.361572987183170547, 37.05059781766744464, 9.846743663894590881 ) ) ;
#9139 = SURFACE_STYLE_FILL_AREA ( #94110 ) ;
#9140 = EDGE_CURVE ( 'NONE', #22285, #41784, #72464, .T. ) ;
#9141 = CYLINDRICAL_SURFACE ( 'NONE', #30298, 2.000000000000000888 ) ;
#9142 = CARTESIAN_POINT ( 'NONE',  ( 6.565887622018943937, 3.081968003263753531, -12.81628187352647608 ) ) ;
#9143 = AXIS2_PLACEMENT_3D ( 'NONE', #60867, #91367, #22893 ) ;
#9144 = ORIENTED_EDGE ( 'NONE', *, *, #98768, .T. ) ;
#9145 = CARTESIAN_POINT ( 'NONE',  ( -4.164238869374099927, 47.01208216824729647, 3.795296366450308767 ) ) ;
#9146 = VERTEX_POINT ( 'NONE', #6205 ) ;
#9147 = CARTESIAN_POINT ( 'NONE',  ( 6.204703633549690345, 37.84541550158063927, 14.16423886937410082 ) ) ;
#9148 = ORIENTED_EDGE ( 'NONE', *, *, #12731, .T. ) ;
#9149 = CARTESIAN_POINT ( 'NONE',  ( 10.00000000000000178, 24.31368534415484106, 10.88017736071110342 ) ) ;
#9150 = LINE ( 'NONE', #42004, #21850 ) ;
#9151 = CARTESIAN_POINT ( 'NONE',  ( 4.559911319644449179, 33.89701867748817676, 9.422509992056141925 ) ) ;
#9152 = CARTESIAN_POINT ( 'NONE',  ( 19.84674366389459266, 53.30059781766744464, 2.638427012816836559 ) ) ;
#9153 = CARTESIAN_POINT ( 'NONE',  ( 12.91533473730992121, 34.52201867748817676, 10.88017736071110164 ) ) ;
#9154 = DIRECTION ( 'NONE',  ( 6.325067799096631348E-17, -2.128331934758712753E-15, 1.000000000000000000 ) ) ;
#9155 = CARTESIAN_POINT ( 'NONE',  ( -0.8801773607111008646, 68.27201867748817676, 2.915334737309923430 ) ) ;
#9156 = CARTESIAN_POINT ( 'NONE',  ( 12.91533473730992121, 29.52201867748817321, 10.88017736071110164 ) ) ;
#9158 = ORIENTED_EDGE ( 'NONE', *, *, #61400, .F. ) ;
#9157 = CARTESIAN_POINT ( 'NONE',  ( 0.1558200433086288639, 4.218224077326415689E-16, -14.62618286184525829 ) ) ;
#9159 = EDGE_CURVE ( 'NONE', #81080, #44839, #52195, .T. ) ;
#9160 = CARTESIAN_POINT ( 'NONE',  ( 17.20831665107776587, 4.133931151000785675, -7.208316651077762316 ) ) ;
#9161 = CARTESIAN_POINT ( 'NONE',  ( 0.000000000000000000, 0.5000000000000004441, 0.000000000000000000 ) ) ;
#9162 = ORIENTED_EDGE ( 'NONE', *, *, #368, .T. ) ;
#9163 = FACE_OUTER_BOUND ( 'NONE', #30817, .T. ) ;
#9164 = CARTESIAN_POINT ( 'NONE',  ( 17.20831665107776587, 29.13393115100078390, -7.208316651077762316 ) ) ;
#9166 = ADVANCED_FACE ( 'NONE', ( #21209 ), #51707, .F. ) ;
#9165 = CARTESIAN_POINT ( 'NONE',  ( 6.349999999999995204, -97.00000000000000000, -3.750000000000000000 ) ) ;
#9167 = LINE ( 'NONE', #24185, #16468 ) ;
#9168 = CARTESIAN_POINT ( 'NONE',  ( 8.375939845167682307, 15.00000000000000000, 11.52849216984304448 ) ) ;
#9169 = MECHANICAL_DESIGN_GEOMETRIC_PRESENTATION_REPRESENTATION (  '', ( #28301 ), #29862 ) ;
#9170 = CARTESIAN_POINT ( 'NONE',  ( 14.42525372082711144, 0.2301507929055687240, -3.890283033989180517 ) ) ;
#9171 = LINE ( 'NONE', #93155, #61759 ) ;
#9172 = CARTESIAN_POINT ( 'NONE',  ( 14.92337183194729633, 52.67559781766745175, 8.527530157486181039 ) ) ;
#9173 = CARTESIAN_POINT ( 'NONE',  ( 22.26659068614894466, 48.88708216824730357, 7.082119434687054849 ) ) ;
#9174 = CARTESIAN_POINT ( 'NONE',  ( 2.791683348922237240, 65.38393115100078035, -7.208316651077763204 ) ) ;
#9175 = VERTEX_POINT ( 'NONE', #36708 ) ;
#9176 = CARTESIAN_POINT ( 'NONE',  ( -11.62719953690051788, 0.5000000000000004441, -9.476720473301954328 ) ) ;
#9177 = CARTESIAN_POINT ( 'NONE',  ( 19.84674366389459266, 18.30059781766745175, 2.638427012816836559 ) ) ;
#9178 = CIRCLE ( 'NONE', #23623, 15.00000000000000000 ) ;
#9179 = CARTESIAN_POINT ( 'NONE',  ( 16.40814093676323893, 45.79030133659708923, 11.09922568453595026 ) ) ;
#9180 = CARTESIAN_POINT ( 'NONE',  ( 1.472469842513823179, 60.59226448433412315, -4.923371831947296329 ) ) ;
#9181 = CARTESIAN_POINT ( 'NONE',  ( 0.5774900079438607392, 58.48035201082151247, 5.440088680355550821 ) ) ;
#9182 = AXIS2_PLACEMENT_3D ( 'NONE', #48387, #1936, #94379 ) ;
#9183 = CARTESIAN_POINT ( 'NONE',  ( 17.20831665107776587, 49.13393115100078745, -7.208316651077762316 ) ) ;
#9184 = CIRCLE ( 'NONE', #69868, 14.49999999999999822 ) ;
#9185 = CARTESIAN_POINT ( 'NONE',  ( 6.935117329331200509, -80.58074665965396832, -2.750000000000000888 ) ) ;
#9186 = EDGE_LOOP ( 'NONE', ( #64457, #92181, #23407, #74927, #76119, #26006 ) ) ;
#9187 = CARTESIAN_POINT ( 'NONE',  ( 6.204703633549690345, 50.76208216824730357, -14.16423886937410259 ) ) ;
#9188 = SURFACE_STYLE_FILL_AREA ( #17201 ) ;
#9189 = CARTESIAN_POINT ( 'NONE',  ( 4.559911319644449179, 23.89701867748817321, 9.422509992056141925 ) ) ;
#9191 = CARTESIAN_POINT ( 'NONE',  ( -0.8801773607110991993, 62.85535201082150536, -2.915334737309923874 ) ) ;
#9190 = CARTESIAN_POINT ( 'NONE',  ( 6.565887622018943937, 8.081968003263751754, -12.81628187352647608 ) ) ;
#9192 = CARTESIAN_POINT ( 'NONE',  ( -8.549759589250339076, 0.2301501389895029837, 12.25250350990691572 ) ) ;
#9194 = EDGE_CURVE ( 'NONE', #36460, #52625, #45181, .T. ) ;
#9193 = DIRECTION ( 'NONE',  ( 0.1059530667249611452, -0.9943711317468825195, 0.000000000000000000 ) ) ;
#9195 = CARTESIAN_POINT ( 'NONE',  ( 20.10421743870887568, 45.60736173766201063, -6.337391062633419558 ) ) ;
#9197 = CARTESIAN_POINT ( 'NONE',  ( 0.1955144967549070634, 54.32703681773340065, -6.500000000002873257 ) ) ;
#9196 = CARTESIAN_POINT ( 'NONE',  ( -0.8801773607111009756, 58.06368534415484106, 1.068504757029289695E-15 ) ) ;
#9198 = CARTESIAN_POINT ( 'NONE',  ( 7.361572987183170547, 37.05059781766744464, 9.846743663894590881 ) ) ;
#9199 = FILL_AREA_STYLE_COLOUR ( '', #12218 ) ;
#9200 = CARTESIAN_POINT ( 'NONE',  ( -7.082119434687044190, 32.63708216824731778, 12.26659068614894998 ) ) ;
#9201 = CARTESIAN_POINT ( 'NONE',  ( 3.591859063236763294, 3.290301336597087012, -11.09922568453595026 ) ) ;
#9203 = CARTESIAN_POINT ( 'NONE',  ( 15.55000000000000071, 99.99999999999998579, -8.000000000000000000 ) ) ;
#9202 = CARTESIAN_POINT ( 'NONE',  ( 4.559911319644449179, 13.89701867748817321, 9.422509992056141925 ) ) ;
#9204 = CARTESIAN_POINT ( 'NONE',  ( -2.266590686148945544, 42.22041550158063217, 7.082119434687048631 ) ) ;
#9205 = CARTESIAN_POINT ( 'NONE',  ( 24.16423886937410614, 59.51208216824728936, -3.795296366450302550 ) ) ;
#9206 = CARTESIAN_POINT ( 'NONE',  ( 1.472469842513823179, 15.59226448433411960, -4.923371831947296329 ) ) ;
#9207 = CARTESIAN_POINT ( 'NONE',  ( 19.42250999205614193, 10.14701867748816966, 5.440088680355555262 ) ) ;
#9208 = ORIENTED_EDGE ( 'NONE', *, *, #80937, .T. ) ;
#9209 = CARTESIAN_POINT ( 'NONE',  ( 17.20831665107776587, 37.88393115100078745, 7.208316651077764980 ) ) ;
#9210 = CARTESIAN_POINT ( 'NONE',  ( -0.8801773607111009756, 28.06368534415484106, 1.068504757029289695E-15 ) ) ;
#9211 = CARTESIAN_POINT ( 'NONE',  ( 6.565887622018943937, -1.918031996736246692, -12.81628187352647608 ) ) ;
#9213 = CARTESIAN_POINT ( 'NONE',  ( 0.1532563361054100626, 60.80059781766744464, -2.638427012816831230 ) ) ;
#9212 = CARTESIAN_POINT ( 'NONE',  ( 17.08211943468705130, 18.47041550158063572, 12.26659068614894998 ) ) ;
#9214 = CARTESIAN_POINT ( 'NONE',  ( -5.803070148808410877, 4.629725225344712954E-16, 13.28812917035384267 ) ) ;
#9215 = UNCERTAINTY_MEASURE_WITH_UNIT (LENGTH_MEASURE( 1.000000000000000082E-05 ), #31377, 'distance_accuracy_value', 'NONE');
#9216 = CARTESIAN_POINT ( 'NONE',  ( 2.791683348922237240, 10.38393115100078390, -7.208316651077763204 ) ) ;
#9217 = CARTESIAN_POINT ( 'NONE',  ( 13.43411237798106583, 57.66530133659708923, -12.81628187352647252 ) ) ;
#9218 = CARTESIAN_POINT ( 'NONE',  ( 14.92337183194729633, 57.67559781766745886, 8.527530157486181039 ) ) ;
#9219 = EDGE_LOOP ( 'NONE', ( #85513, #98030, #66562, #84543 ) ) ;
#9220 = CARTESIAN_POINT ( 'NONE',  ( 1.472469842513823179, 20.59226448433411960, -4.923371831947296329 ) ) ;
#9221 = CARTESIAN_POINT ( 'NONE',  ( 8.630000001796595654, -0.01508430609074851159, -4.000000000000000000 ) ) ;
#9222 = CARTESIAN_POINT ( 'NONE',  ( 8.879999999999999005, 20.99999999999999645, 0.000000000000000000 ) ) ;
#9223 = CARTESIAN_POINT ( 'NONE',  ( 10.00000000000000000, 1.813685344154838175, -10.88017736071110342 ) ) ;
#9224 = CARTESIAN_POINT ( 'NONE',  ( 19.42250999205614548, 55.98035201082150536, -5.440088680355545492 ) ) ;
#9225 = CARTESIAN_POINT ( 'NONE',  ( 13.79529636645031943, 10.34541550158063394, -14.16423886937409904 ) ) ;
#9226 = AXIS2_PLACEMENT_3D ( 'NONE', #28726, #67228, #37725 ) ;
#9227 = CARTESIAN_POINT ( 'NONE',  ( 20.88017736071110519, 50.56368534415484106, 2.639326808657452039E-16 ) ) ;
#9228 = CARTESIAN_POINT ( 'NONE',  ( 5.076628168052704559, 35.17559781766745175, -8.527530157486179263 ) ) ;
#9229 = CARTESIAN_POINT ( 'NONE',  ( 7.084665262690076126, 22.02201867748817321, -10.88017736071110164 ) ) ;
#9230 = DIRECTION ( 'NONE',  ( -0.09584575252022721481, 0.000000000000000000, 0.9953961983671785196 ) ) ;
#9231 = CARTESIAN_POINT ( 'NONE',  ( 17.20831665107776587, 57.88393115100078745, 7.208316651077764980 ) ) ;
#9232 = DIRECTION ( 'NONE',  ( 0.3665012267243070720, 0.000000000000000000, -0.9304175679820205769 ) ) ;
#9233 = UNCERTAINTY_MEASURE_WITH_UNIT (LENGTH_MEASURE( 1.000000000000000082E-05 ), #25621, 'distance_accuracy_value', 'NONE');
#9234 = STYLED_ITEM ( 'NONE', ( #89550 ), #15837 ) ;
#9235 = ORIENTED_EDGE ( 'NONE', *, *, #71364, .T. ) ;
#9236 = ORIENTED_EDGE ( 'NONE', *, *, #2869, .F. ) ;
#9237 = CARTESIAN_POINT ( 'NONE',  ( 0.2751277870542908621, 32.28217586085237656, -6.499999999999992006 ) ) ;
#9238 = CARTESIAN_POINT ( 'NONE',  ( 0.1532563361054082862, 46.21726448433411605, 2.638427012816831674 ) ) ;
#9239 = CARTESIAN_POINT ( 'NONE',  ( 0.1532563361054082862, 26.21726448433411605, 2.638427012816831674 ) ) ;
#9240 = CARTESIAN_POINT ( 'NONE',  ( 3.591859063236763294, 63.29030133659708923, -11.09922568453595026 ) ) ;
#9242 = CARTESIAN_POINT ( 'NONE',  ( 14.92337183194729633, 47.67559781766745175, 8.527530157486181039 ) ) ;
#9241 = CARTESIAN_POINT ( 'NONE',  ( 4.559911319644449179, 22.23035201082150536, -9.422509992056141925 ) ) ;
#9243 = CARTESIAN_POINT ( 'NONE',  ( -0.2418659066527639179, 34.26028685723174050, -6.114288769123057854 ) ) ;
#9244 = CARTESIAN_POINT ( 'NONE',  ( 10.00000000000000000, 35.55374883491396787, -14.16423886937410082 ) ) ;
#9245 = CARTESIAN_POINT ( 'NONE',  ( 24.16423886937410614, 54.30374883491396787, 8.672049930838204340E-16 ) ) ;
#9246 = CARTESIAN_POINT ( 'NONE',  ( -4.265913727722004722, 0.04962886353675339396, -14.12300574719584034 ) ) ;
#9247 = CARTESIAN_POINT ( 'NONE',  ( 18.00000000000000000, 77.07179676972447169, 4.250000000000000000 ) ) ;
#9248 = CARTESIAN_POINT ( 'NONE',  ( 7.084665262690076126, 54.10535201082151247, 10.88017736071109987 ) ) ;
#9249 = CARTESIAN_POINT ( 'NONE',  ( 14.92337183194729633, 17.67559781766745175, 8.527530157486181039 ) ) ;
#9250 = AXIS2_PLACEMENT_3D ( 'NONE', #42219, #96708, #95197 ) ;
#9251 = CARTESIAN_POINT ( 'NONE',  ( 17.85999999999999943, 37.99999999999997868, -10.00000000000000000 ) ) ;
#9252 = ORIENTED_EDGE ( 'NONE', *, *, #92831, .F. ) ;
#9253 = CARTESIAN_POINT ( 'NONE',  ( 0.8719017118913385822, 123.9374316453451144, 4.500000000000000888 ) ) ;
#9254 = EDGE_LOOP ( 'NONE', ( #24691, #37207, #46599, #14551 ) ) ;
#9255 = AXIS2_PLACEMENT_3D ( 'NONE', #2829, #86308, #10800 ) ;
#9256 = CARTESIAN_POINT ( 'NONE',  ( 2.791683348922240793, 11.63393115100078568, 7.208316651077764092 ) ) ;
#9257 = EDGE_LOOP ( 'NONE', ( #55525, #43373, #18459, #31335, #56607, #35813 ) ) ;
#9258 = CARTESIAN_POINT ( 'NONE',  ( 17.08211943468705130, 18.47041550158063572, 12.26659068614894998 ) ) ;
#9259 = CARTESIAN_POINT ( 'NONE',  ( 17.20831665107776587, 24.13393115100078035, -7.208316651077762316 ) ) ;
#9260 = CARTESIAN_POINT ( 'NONE',  ( -0.8801773607111008646, 38.27201867748816255, 2.915334737309923430 ) ) ;
#9261 = EDGE_CURVE ( 'NONE', #40893, #89049, #94630, .T. ) ;
#9262 = MECHANICAL_DESIGN_GEOMETRIC_PRESENTATION_REPRESENTATION (  '', ( #47580 ), #14047 ) ;
#9263 = ORIENTED_EDGE ( 'NONE', *, *, #80380, .F. ) ;
#9264 = AXIS2_PLACEMENT_3D ( 'NONE', #69635, #53642, #1159 ) ;
#9265 = CARTESIAN_POINT ( 'NONE',  ( 17.96484262340118221, 41.18868534415484106, -7.964842623401177768 ) ) ;
#9266 = CARTESIAN_POINT ( 'NONE',  ( 19.72487221294571214, 37.80223176428831522, -6.499999999999988454 ) ) ;
#9267 = ORIENTED_EDGE ( 'NONE', *, *, #38200, .T. ) ;
#9268 = CARTESIAN_POINT ( 'NONE',  ( 6.204703633549690345, 5.762082168247301794, -14.16423886937410259 ) ) ;
#9269 = EDGE_LOOP ( 'NONE', ( #16063, #4130, #22269, #42755 ) ) ;
#9270 = ORIENTED_EDGE ( 'NONE', *, *, #65480, .T. ) ;
#9271 = CARTESIAN_POINT ( 'NONE',  ( -2.816281873526473856, 29.33196800326376064, 3.434112377981055619 ) ) ;
#9272 = CARTESIAN_POINT ( 'NONE',  ( 19.84674366389459621, 8.508931151000785675, 7.409399052514197653E-17 ) ) ;
#9273 = DIRECTION ( 'NONE',  ( -1.000000000000000000, -1.636349903325072848E-16, 0.000000000000000000 ) ) ;
#9274 = CARTESIAN_POINT ( 'NONE',  ( 2.241241388159942801E-47, 3.851859888774471706E-31, -7.000000000000000000 ) ) ;
#9275 = CARTESIAN_POINT ( 'NONE',  ( 7.361572987183169658, 19.96726448433411960, -9.846743663894592657 ) ) ;
#9276 = CARTESIAN_POINT ( 'NONE',  ( 19.42250999205614193, 30.14701867748817321, 5.440088680355555262 ) ) ;
#9277 = B_SPLINE_CURVE_WITH_KNOTS ( 'NONE', 3,
 ( #60245, #74244, #97283, #82748, #58759, #74753 ),
 .UNSPECIFIED., .F., .F.,
 ( 4, 2, 4 ),
 ( 3.409110551495907074E-05, 0.0004400426677367846201, 0.0008459942299586101829 ),
 .UNSPECIFIED. ) ;
#9278 = EDGE_LOOP ( 'NONE', ( #51801, #68106, #89158, #16682, #86655, #76300 ) ) ;
#9279 = EDGE_CURVE ( 'NONE', #70392, #70139, #65862, .T. ) ;
#9280 = FACE_OUTER_BOUND ( 'NONE', #72739, .T. ) ;
#9281 = CARTESIAN_POINT ( 'NONE',  ( 2.035157376598824452, 58.68868534415482685, 7.964842623401179544 ) ) ;
#9282 = CARTESIAN_POINT ( 'NONE',  ( -14.69266224296346479, 14.95037104324862476, 1.335284760096034695 ) ) ;
#9283 = CARTESIAN_POINT ( 'NONE',  ( 15.44008868035555260, 54.73035201082150536, 9.422509992056143702 ) ) ;
#9284 = EDGE_CURVE ( 'NONE', #18606, #78790, #58035, .T. ) ;
#9285 = VERTEX_POINT ( 'NONE', #74522 ) ;
#9286 = CARTESIAN_POINT ( 'NONE',  ( 11.94665733272772812, 0.2301501672491274575, 8.972157519073714838 ) ) ;
#9287 = CARTESIAN_POINT ( 'NONE',  ( 18.52753015748617571, 28.09226448433411960, 4.923371831947298993 ) ) ;
#9288 = CARTESIAN_POINT ( 'NONE',  ( 22.81628187352648496, 61.83196800326376774, -3.434112377981050290 ) ) ;
#9289 = CARTESIAN_POINT ( 'NONE',  ( 24.16423886937410614, 14.30374883491396787, 8.672049930838204340E-16 ) ) ;
#9290 = CARTESIAN_POINT ( 'NONE',  ( 1.472469842513823179, 21.42559781766745175, 4.923371831947296329 ) ) ;
#9291 = CARTESIAN_POINT ( 'NONE',  ( 0.6178305044545838731, 19.74863466993042138, 9.382169495545420901 ) ) ;
#9293 = CYLINDRICAL_SURFACE ( 'NONE', #54552, 11.92686044187656513 ) ;
#9292 = DIRECTION ( 'NONE',  ( 0.000000000000000000, 0.000000000000000000, 1.000000000000000000 ) ) ;
#9294 = CARTESIAN_POINT ( 'NONE',  ( -0.8801773607110991993, 47.85535201082150536, -2.915334737309923874 ) ) ;
#9295 = CARTESIAN_POINT ( 'NONE',  ( 2.791683348922237240, 65.38393115100078035, -7.208316651077763204 ) ) ;
#9296 = SURFACE_STYLE_FILL_AREA ( #23829 ) ;
#9297 = CARTESIAN_POINT ( 'NONE',  ( 2.791683348922240793, 16.63393115100078745, 7.208316651077764092 ) ) ;
#9298 = CARTESIAN_POINT ( 'NONE',  ( 17.96484262340118221, 16.18868534415483396, -7.964842623401177768 ) ) ;
#9299 = CARTESIAN_POINT ( 'NONE',  ( 22.81628187352648496, 16.83196800326374998, -3.434112377981050290 ) ) ;
#9300 = CARTESIAN_POINT ( 'NONE',  ( 19.84674366389459266, 18.71726448433411960, -2.638427012816827677 ) ) ;
#9301 = CARTESIAN_POINT ( 'NONE',  ( -8.224651678658434051, 85.81254401277075772, 3.937446577531860559 ) ) ;
#9302 = CARTESIAN_POINT ( 'NONE',  ( 19.42250999205614548, 15.98035201082150714, -5.440088680355545492 ) ) ;
#9303 = CARTESIAN_POINT ( 'NONE',  ( 0.000000000000000000, 14.49999999999999822, 0.000000000000000000 ) ) ;
#9305 = CARTESIAN_POINT ( 'NONE',  ( 19.42250999205614548, 20.98035201082150891, -5.440088680355545492 ) ) ;
#9304 = CARTESIAN_POINT ( 'NONE',  ( 2.791683348922240793, 36.63393115100078035, 7.208316651077764092 ) ) ;
#9306 = LINE ( 'NONE', #24331, #51965 ) ;
#9307 = CARTESIAN_POINT ( 'NONE',  ( 17.96484262340118221, 36.18868534415484106, -7.964842623401177768 ) ) ;
#9309 = SURFACE_STYLE_FILL_AREA ( #54796 ) ;
#9308 = CARTESIAN_POINT ( 'NONE',  ( 10.00000000000000178, 9.313685344154839285, 10.88017736071110342 ) ) ;
#9310 = CARTESIAN_POINT ( 'NONE',  ( 2.791683348922237240, 10.38393115100078390, -7.208316651077763204 ) ) ;
#9311 = ADVANCED_FACE ( 'NONE', ( #80057 ), #12052, .T. ) ;
#9312 = CARTESIAN_POINT ( 'NONE',  ( 18.52753015748617571, 43.09226448433412315, 4.923371831947298993 ) ) ;
#9313 = LINE ( 'NONE', #62801, #36207 ) ;
#9314 = CARTESIAN_POINT ( 'NONE',  ( -0.7117905103454820193, 0.000000000000000000, -5.406585696355432624 ) ) ;
#9315 = ADVANCED_FACE ( 'NONE', ( #74024 ), #75260, .T. ) ;
#9317 = CARTESIAN_POINT ( 'NONE',  ( -12.07856007377814223, 15.00000000000000000, -8.022367888855001183 ) ) ;
#9316 = AXIS2_PLACEMENT_3D ( 'NONE', #9412, #67952, #83932 ) ;
#9318 = VECTOR ( 'NONE', #69524, 1000.000000000000114 ) ;
#9319 = CARTESIAN_POINT ( 'NONE',  ( -8.028888469548853379, -1.053269085617737799, -4.000000000000000000 ) ) ;
#9320 = CARTESIAN_POINT ( 'NONE',  ( 24.16423886937409904, 29.09541550158063572, 3.795296366450317205 ) ) ;
#9321 = CARTESIAN_POINT ( 'NONE',  ( 18.52753015748617571, 33.09226448433411605, 4.923371831947298993 ) ) ;
#9322 = CARTESIAN_POINT ( 'NONE',  ( 2.618367889266248100E-15, 44.99999999999999289, 7.000000000000000000 ) ) ;
#9323 = VERTEX_POINT ( 'NONE', #64932 ) ;
#9324 = CARTESIAN_POINT ( 'NONE',  ( -0.3689425029237881626, 57.42874883491397497, 10.36894250292379027 ) ) ;
#9325 = CARTESIAN_POINT ( 'NONE',  ( 0.1532563361054083140, 21.00893115100078745, 1.131784320476157264E-15 ) ) ;
#9327 = LINE ( 'NONE', #40819, #2371 ) ;
#9326 = DIRECTION ( 'NONE',  ( 0.8073289077885641429, -0.5901017155109146151, 0.000000000000000000 ) ) ;
#9328 = CARTESIAN_POINT ( 'NONE',  ( 15.44008868035555260, 44.73035201082151247, 9.422509992056143702 ) ) ;
#9329 = CARTESIAN_POINT ( 'NONE',  ( 0.6178305044545818747, 58.49863466993042493, -9.382169495545419124 ) ) ;
#9330 = EDGE_LOOP ( 'NONE', ( #54598, #67961, #80216, #59564 ) ) ;
#9331 = CARTESIAN_POINT ( 'NONE',  ( 15.44008868035555260, 19.73035201082150536, 9.422509992056143702 ) ) ;
#9332 = CARTESIAN_POINT ( 'NONE',  ( 22.81628187352648496, 46.83196800326376064, -3.434112377981050290 ) ) ;
#9333 = CARTESIAN_POINT ( 'NONE',  ( 0.6178305044545838731, 14.74863466993041783, 9.382169495545420901 ) ) ;
#9334 = CARTESIAN_POINT ( 'NONE',  ( 18.52753015748618282, 13.92559781766745175, -4.923371831947291888 ) ) ;
#9335 = ORIENTED_EDGE ( 'NONE', *, *, #9159, .F. ) ;
#9336 = FILL_AREA_STYLE_COLOUR ( '', #80403 ) ;
#9337 = CARTESIAN_POINT ( 'NONE',  ( 14.49999999999999822, 11.00000000000000000, -6.500000000000000888 ) ) ;
#9338 = CARTESIAN_POINT ( 'NONE',  ( 2.917880565312948704, 52.63708216824730357, 12.26659068614894643 ) ) ;
#9339 = CARTESIAN_POINT ( 'NONE',  ( -0.3689425029237881626, 12.42874883491396609, 10.36894250292379027 ) ) ;
#9340 = CARTESIAN_POINT ( 'NONE',  ( 17.96484262340118221, 21.18868534415483396, -7.964842623401177768 ) ) ;
#9341 = CARTESIAN_POINT ( 'NONE',  ( 2.035157376598822676, 37.43868534415484106, -7.964842623401177768 ) ) ;
#9342 = CARTESIAN_POINT ( 'NONE',  ( 20.15039907845753220, 21.74884699246888786, 6.262539305110078836 ) ) ;
#9343 = CARTESIAN_POINT ( 'NONE',  ( 19.42250999205614548, 60.98035201082151247, -5.440088680355545492 ) ) ;
#9344 = CARTESIAN_POINT ( 'NONE',  ( 12.63842701281683922, 24.55059781766745175, -9.846743663894590881 ) ) ;
#9345 = DIRECTION ( 'NONE',  ( -1.000000000000000000, 0.000000000000000000, 0.000000000000000000 ) ) ;
#9346 = FILL_AREA_STYLE_COLOUR ( '', #46777 ) ;
#9347 = CARTESIAN_POINT ( 'NONE',  ( 14.92337183194729988, 14.34226448433411782, -8.527530157486177487 ) ) ;
#9348 = CARTESIAN_POINT ( 'NONE',  ( 18.52753015748617571, 33.09226448433411605, 4.923371831947298993 ) ) ;
#9349 = CARTESIAN_POINT ( 'NONE',  ( 0.5774900079438590739, 7.647018677488171434, -5.440088680355550821 ) ) ;
#9350 = UNCERTAINTY_MEASURE_WITH_UNIT (LENGTH_MEASURE( 1.000000000000000082E-05 ), #41081, 'distance_accuracy_value', 'NONE');
#9351 = CARTESIAN_POINT ( 'NONE',  ( -1.099225684535947600, 28.70696800326375353, -6.408140936763238038 ) ) ;
#9352 = CARTESIAN_POINT ( 'NONE',  ( 15.44008868035555793, 56.39701867748817676, -9.422509992056140149 ) ) ;
#9354 = CARTESIAN_POINT ( 'NONE',  ( 14.92337183194729988, 14.34226448433411782, -8.527530157486177487 ) ) ;
#9353 = CARTESIAN_POINT ( 'NONE',  ( 10.00000000000000178, 48.05374883491396787, 14.16423886937410082 ) ) ;
#9355 = DIRECTION ( 'NONE',  ( -0.000000000000000000, -0.000000000000000000, -1.000000000000000000 ) ) ;
#9356 = CARTESIAN_POINT ( 'NONE',  ( 0.1532563361054083140, 46.00893115100079456, 1.131784320476157264E-15 ) ) ;
#9358 = CARTESIAN_POINT ( 'NONE',  ( 13.79529636645031943, 10.34541550158063394, -14.16423886937409904 ) ) ;
#9357 = CARTESIAN_POINT ( 'NONE',  ( 18.52753015748617571, 33.09226448433411605, 4.923371831947298993 ) ) ;
#9359 = EDGE_CURVE ( 'NONE', #20156, #26894, #50438, .T. ) ;
#9360 = CARTESIAN_POINT ( 'NONE',  ( 24.16423886937410614, 24.30374883491396787, 8.672049930838204340E-16 ) ) ;
#9361 = CARTESIAN_POINT ( 'NONE',  ( 12.91533473730992121, 44.52201867748816966, 10.88017736071110164 ) ) ;
#9362 = CARTESIAN_POINT ( 'NONE',  ( 20.88017736071110164, 15.35535201082150358, 2.915334737309930979 ) ) ;
#9363 = CARTESIAN_POINT ( 'NONE',  ( 10.00000000000000000, 41.81368534415484106, -10.88017736071110342 ) ) ;
#9364 = MANIFOLD_SOLID_BREP ( 'Fillet10', #77781 ) ;
#9365 = CARTESIAN_POINT ( 'NONE',  ( 4.559911319644449179, 32.23035201082150536, -9.422509992056141925 ) ) ;
#9366 = ORIENTED_EDGE ( 'NONE', *, *, #58135, .F. ) ;
#9367 = CARTESIAN_POINT ( 'NONE',  ( 3.591859063236763294, 33.29030133659708213, -11.09922568453595026 ) ) ;
#9368 = CARTESIAN_POINT ( 'NONE',  ( 2.035157376598824452, 38.68868534415483396, 7.964842623401179544 ) ) ;
#9369 = ORIENTED_EDGE ( 'NONE', *, *, #54989, .T. ) ;
#9370 = CARTESIAN_POINT ( 'NONE',  ( 3.591859063236763294, 63.29030133659708923, -11.09922568453595026 ) ) ;
#9371 = EDGE_CURVE ( 'NONE', #37098, #39036, #14117, .T. ) ;
#9372 = CARTESIAN_POINT ( 'NONE',  ( 20.88017736071110519, 50.56368534415484106, 2.639326808657452039E-16 ) ) ;
#9373 = ORIENTED_EDGE ( 'NONE', *, *, #19468, .F. ) ;
#9374 = CARTESIAN_POINT ( 'NONE',  ( 0.5774900079438590739, 52.64701867748817676, -5.440088680355550821 ) ) ;
#9375 = CARTESIAN_POINT ( 'NONE',  ( 12.91533473730992121, 4.522018677488169658, 10.88017736071110164 ) ) ;
#9376 = FACE_OUTER_BOUND ( 'NONE', #92952, .T. ) ;
#9377 = CARTESIAN_POINT ( 'NONE',  ( 4.391347328462916089, 0.2301508954901538839, 14.28069739540083738 ) ) ;
#9378 = CARTESIAN_POINT ( 'NONE',  ( 24.16423886937410614, 64.51208216824728936, -3.795296366450302550 ) ) ;
#9379 = CARTESIAN_POINT ( 'NONE',  ( 0.1532563361054100626, 0.8005978176674514168, -2.638427012816831230 ) ) ;
#9380 = CARTESIAN_POINT ( 'NONE',  ( -4.164238869374098151, 1.595415501580634388, -3.795296366450310543 ) ) ;
#9381 = CARTESIAN_POINT ( 'NONE',  ( -0.8801773607110991993, 12.85535201082150358, -2.915334737309923874 ) ) ;
#9382 = CARTESIAN_POINT ( 'NONE',  ( 5.076628168052704559, 45.17559781766745175, -8.527530157486179263 ) ) ;
#9383 = ORIENTED_EDGE ( 'NONE', *, *, #26758, .T. ) ;
#9384 = B_SPLINE_CURVE_WITH_KNOTS ( 'NONE', 3,
 ( #58656, #74138, #21161, #12172, #80176, #4196, #51663, #34666 ),
 .UNSPECIFIED., .F., .F.,
 ( 4, 2, 2, 4 ),
 ( 1.734723475976807094E-18, 0.001337541016207008859, 0.002675082032414015983, 0.005350164064828043242 ),
 .UNSPECIFIED. ) ;
#9385 = CARTESIAN_POINT ( 'NONE',  ( 0.1532563361054083140, 51.00893115100078745, 1.131784320476157264E-15 ) ) ;
#9386 = STYLED_ITEM ( 'NONE', ( #1340 ), #13909 ) ;
#9387 = CARTESIAN_POINT ( 'NONE',  ( -0.8801773607111009756, 68.06368534415484817, 1.068504757029289695E-15 ) ) ;
#9388 = CARTESIAN_POINT ( 'NONE',  ( 20.88017736071110164, 40.35535201082150536, 2.915334737309930979 ) ) ;
#9389 = CARTESIAN_POINT ( 'NONE',  ( 0.1532563361054083140, 41.00893115100078745, 1.131784320476157264E-15 ) ) ;
#9391 = CARTESIAN_POINT ( 'NONE',  ( 4.559911319644449179, 67.23035201082150536, -9.422509992056141925 ) ) ;
#9390 = CARTESIAN_POINT ( 'NONE',  ( 26.00000000000000355, 35.99999999999997158, -10.00000000000000000 ) ) ;
#9392 = CARTESIAN_POINT ( 'NONE',  ( 7.084665262690076126, 52.02201867748816255, -10.88017736071110164 ) ) ;
#9393 = CARTESIAN_POINT ( 'NONE',  ( 24.16423886937410614, 64.30374883491396076, 8.672049930838204340E-16 ) ) ;
#9394 = CIRCLE ( 'NONE', #50926, 0.2500000000000002220 ) ;
#9395 = MECHANICAL_DESIGN_GEOMETRIC_PRESENTATION_REPRESENTATION (  '', ( #7839 ), #14195 ) ;
#9396 = EDGE_CURVE ( 'NONE', #71843, #16281, #39879, .T. ) ;
#9397 = CARTESIAN_POINT ( 'NONE',  ( -2.816281873526473856, 19.33196800326375708, 3.434112377981055619 ) ) ;
#9398 = CYLINDRICAL_SURFACE ( 'NONE', #32337, 0.5000000000000004441 ) ;
#9399 = ORIENTED_EDGE ( 'NONE', *, *, #65693, .F. ) ;
#9400 = CARTESIAN_POINT ( 'NONE',  ( 22.81628187352647785, 31.41530133659709279, 3.434112377981063169 ) ) ;
#9401 = CARTESIAN_POINT ( 'NONE',  ( 12.91533473730993009, 16.60535201082150891, -10.88017736071109987 ) ) ;
#9402 = EDGE_CURVE ( 'NONE', #30783, #74488, #79351, .T. ) ;
#9403 = VERTEX_POINT ( 'NONE', #2397 ) ;
#9404 = CARTESIAN_POINT ( 'NONE',  ( 0.000000000000000000, 0.000000000000000000, 0.000000000000000000 ) ) ;
#9405 = CARTESIAN_POINT ( 'NONE',  ( 10.00000000000000178, 69.31368534415484817, 10.88017736071110342 ) ) ;
#9406 = CARTESIAN_POINT ( 'NONE',  ( 2.791683348922237240, 45.38393115100079456, -7.208316651077763204 ) ) ;
#9408 = CARTESIAN_POINT ( 'NONE',  ( 7.361572987183170547, 42.05059781766745886, 9.846743663894590881 ) ) ;
#9407 = CARTESIAN_POINT ( 'NONE',  ( 1.472469842513823179, 10.59226448433411782, -4.923371831947296329 ) ) ;
#9409 = CARTESIAN_POINT ( 'NONE',  ( 0.1922240491738394785, 28.18878173731741299, 6.499999999999960920 ) ) ;
#9410 = SURFACE_STYLE_FILL_AREA ( #69423 ) ;
#9411 = CARTESIAN_POINT ( 'NONE',  ( 5.076628168052703671, 21.84226448433411960, 8.527530157486179263 ) ) ;
#9412 = CARTESIAN_POINT ( 'NONE',  ( 0.000000000000000000, 0.000000000000000000, 0.000000000000000000 ) ) ;
#9413 = DIRECTION ( 'NONE',  ( -1.483861936729427615E-16, 1.000000000000000000, 0.000000000000000000 ) ) ;
#9414 = AXIS2_PLACEMENT_3D ( 'NONE', #34830, #93373, #24901 ) ;
#9415 = CARTESIAN_POINT ( 'NONE',  ( 2.791683348922240793, 31.63393115100078745, 7.208316651077764092 ) ) ;
#9416 = FACE_BOUND ( 'NONE', #37266, .T. ) ;
#9418 = VERTEX_POINT ( 'NONE', #93857 ) ;
#9417 = CARTESIAN_POINT ( 'NONE',  ( 7.361572987183169658, 44.96726448433412315, -9.846743663894592657 ) ) ;
#9419 = CARTESIAN_POINT ( 'NONE',  ( 6.432108699068926683, -88.20011490510430008, -2.500000000000000000 ) ) ;
#9420 = CARTESIAN_POINT ( 'NONE',  ( 21.09922568453595559, 32.04030133659708923, -6.408140936763230044 ) ) ;
#9421 = DIRECTION ( 'NONE',  ( -0.1650476058606676066, 0.000000000000000000, -0.9862856015372331031 ) ) ;
#9422 = CARTESIAN_POINT ( 'NONE',  ( -4.164238869374098151, 51.59541550158063217, -3.795296366450310543 ) ) ;
#9423 = CARTESIAN_POINT ( 'NONE',  ( 7.361572987183169658, 19.96726448433411960, -9.846743663894592657 ) ) ;
#9424 = DIRECTION ( 'NONE',  ( 6.661338147750940505E-14, 0.000000000000000000, 1.000000000000000000 ) ) ;
#9425 = CARTESIAN_POINT ( 'NONE',  ( 2.917880565312948704, 37.63708216824731068, 12.26659068614894643 ) ) ;
#9426 = CARTESIAN_POINT ( 'NONE',  ( 7.361572987183169658, 59.96726448433410894, -9.846743663894592657 ) ) ;
#9427 = CARTESIAN_POINT ( 'NONE',  ( -2.266590686148945544, 57.22041550158063217, 7.082119434687048631 ) ) ;
#9428 = CARTESIAN_POINT ( 'NONE',  ( 13.79529636645030344, 23.26208216824730002, 14.16423886937410614 ) ) ;
#9429 = CARTESIAN_POINT ( 'NONE',  ( -4.164238869374099039, 21.80374883491396787, 8.674139862899312516E-16 ) ) ;
#9430 = CARTESIAN_POINT ( 'NONE',  ( 13.75503023589407015, 14.95077488074853456, 5.333408231410830425 ) ) ;
#9431 = CIRCLE ( 'NONE', #11005, 8.250000000000007105 ) ;
#9433 = CARTESIAN_POINT ( 'NONE',  ( 1.472469842513823179, 61.42559781766745175, 4.923371831947296329 ) ) ;
#9432 = DIRECTION ( 'NONE',  ( 1.000000000000000000, -5.818595309480553908E-17, 0.000000000000000000 ) ) ;
#9434 = ORIENTED_EDGE ( 'NONE', *, *, #94306, .F. ) ;
#9435 = CARTESIAN_POINT ( 'NONE',  ( 15.44008868035555260, 39.73035201082150536, 9.422509992056143702 ) ) ;
#9436 = CARTESIAN_POINT ( 'NONE',  ( 3.866352809136213597, 0.04962897115651117991, -14.23757791217069801 ) ) ;
#9437 = CARTESIAN_POINT ( 'NONE',  ( 11.18060183609497571, -93.00793896048890019, 3.750000000000000888 ) ) ;
#9438 = EDGE_CURVE ( 'NONE', #77456, #63872, #80292, .T. ) ;
#9439 = CARTESIAN_POINT ( 'NONE',  ( 19.84674366389459621, 38.50893115100078745, 7.409399052514197653E-17 ) ) ;
#9440 = CARTESIAN_POINT ( 'NONE',  ( 22.81628187352647785, 56.41530133659708213, 3.434112377981063169 ) ) ;
#9441 = CARTESIAN_POINT ( 'NONE',  ( 14.16423886937410259, -5.696251165086027690, -2.602085213965210642E-15 ) ) ;
#9442 = CARTESIAN_POINT ( 'NONE',  ( 19.84674366389459266, 48.30059781766745175, 2.638427012816836559 ) ) ;
#9443 = CARTESIAN_POINT ( 'NONE',  ( 24.50000000000000000, 35.99999999999997158, -10.00000000000000000 ) ) ;
#9444 = ORIENTED_EDGE ( 'NONE', *, *, #90779, .F. ) ;
#9445 = CARTESIAN_POINT ( 'NONE',  ( 6.204703633549690345, 15.76208216824730179, -14.16423886937410259 ) ) ;
#9446 = LINE ( 'NONE', #23971, #48628 ) ;
#9448 = DIRECTION ( 'NONE',  ( 0.5519369853120561498, -0.000000000000000000, 0.8338858220671695465 ) ) ;
#9447 = CARTESIAN_POINT ( 'NONE',  ( 18.72515096720571037, 45.05509018479935435, 6.499999999999982236 ) ) ;
#9449 = CARTESIAN_POINT ( 'NONE',  ( 17.96484262340118221, 11.18868534415484106, -7.964842623401177768 ) ) ;
#9450 = CARTESIAN_POINT ( 'NONE',  ( 22.81628187352648496, 6.831968003263753531, -3.434112377981050290 ) ) ;
#9451 = CARTESIAN_POINT ( 'NONE',  ( 17.74999999999999645, 78.80384757729336798, 4.000000000000000000 ) ) ;
#9452 = CARTESIAN_POINT ( 'NONE',  ( 12.91533473730993009, 61.60535201082150536, -10.88017736071109987 ) ) ;
#9453 = CARTESIAN_POINT ( 'NONE',  ( -8.900000000000002132, 80.99999999999994316, 0.000000000000000000 ) ) ;
#9454 = STYLED_ITEM ( 'NONE', ( #11330 ), #14380 ) ;
#9455 = CARTESIAN_POINT ( 'NONE',  ( -46.94000000000001194, 101.0890360526157252, -7.984865333617746863 ) ) ;
#9456 = DIRECTION ( 'NONE',  ( -0.000000000000000000, -1.000000000000000000, -0.000000000000000000 ) ) ;
#9457 = CARTESIAN_POINT ( 'NONE',  ( 22.26659068614895176, 59.72041550158063927, -7.082119434687042414 ) ) ;
#9458 = CARTESIAN_POINT ( 'NONE',  ( 64.56412365047461321, -3.756725070333740926E-15, 7.000000000000000000 ) ) ;
#9459 = CARTESIAN_POINT ( 'NONE',  ( 19.42250999205614548, 25.98035201082150891, -5.440088680355545492 ) ) ;
#9460 = CARTESIAN_POINT ( 'NONE',  ( 0.5774900079438590739, 37.64701867748817676, -5.440088680355550821 ) ) ;
#9461 = CARTESIAN_POINT ( 'NONE',  ( 21.09922568453595559, 2.040301336597086568, -6.408140936763230044 ) ) ;
#9462 = CARTESIAN_POINT ( 'NONE',  ( 1.472469842513823179, 51.42559781766745886, 4.923371831947296329 ) ) ;
#9463 = CARTESIAN_POINT ( 'NONE',  ( -43.14624366973443870, 107.3138868136391864, -4.970300893257880048 ) ) ;
#9464 = CARTESIAN_POINT ( 'NONE',  ( 19.84674366389459266, 3.300597817667451750, 2.638427012816836559 ) ) ;
#9465 = ORIENTED_EDGE ( 'NONE', *, *, #1003, .F. ) ;
#9466 = AXIS2_PLACEMENT_3D ( 'NONE', #14569, #91539, #75046 ) ;
#9467 = CARTESIAN_POINT ( 'NONE',  ( 20.88017736071110164, 30.35535201082151247, 2.915334737309930979 ) ) ;
#9468 = CARTESIAN_POINT ( 'NONE',  ( 10.00000000000000178, 35.37363466993042493, 12.81628187352647608 ) ) ;
#9469 = CARTESIAN_POINT ( 'NONE',  ( -1.926860441876563801, 54.89664270246084499, 3.195792623639529761 ) ) ;
#9470 = CARTESIAN_POINT ( 'NONE',  ( 2.791683348922240793, 66.63393115100079456, 7.208316651077764092 ) ) ;
#9471 = CARTESIAN_POINT ( 'NONE',  ( 15.44008868035555260, 54.73035201082150536, 9.422509992056143702 ) ) ;
#9472 = CARTESIAN_POINT ( 'NONE',  ( 14.92337183194729633, 12.67559781766745353, 8.527530157486181039 ) ) ;
#9473 = CARTESIAN_POINT ( 'NONE',  ( 0.6178305044545818747, 38.49863466993042493, -9.382169495545419124 ) ) ;
#9475 = DIRECTION ( 'NONE',  ( -0.000000000000000000, 1.000000000000000000, -0.000000000000000000 ) ) ;
#9474 = CARTESIAN_POINT ( 'NONE',  ( 20.88017736071110164, 65.35535201082150536, 2.915334737309930979 ) ) ;
#9476 = CARTESIAN_POINT ( 'NONE',  ( 19.42250999205614548, 55.98035201082150536, -5.440088680355545492 ) ) ;
#9477 = CARTESIAN_POINT ( 'NONE',  ( 6.565887622018943937, 65.16530133659709634, 12.81628187352647430 ) ) ;
#9478 = ORIENTED_EDGE ( 'NONE', *, *, #60792, .F. ) ;
#9479 =( LENGTH_UNIT ( ) NAMED_UNIT ( * ) SI_UNIT ( .MILLI., .METRE. ) );
#9480 = FILL_AREA_STYLE_COLOUR ( '', #44676 ) ;
#9481 = CARTESIAN_POINT ( 'NONE',  ( 20.88017736071110519, 10.56368534415483751, 2.639326808657452039E-16 ) ) ;
#9483 = CARTESIAN_POINT ( 'NONE',  ( 10.00000000000000000, 10.55374883491396787, -14.16423886937410082 ) ) ;
#9482 = CARTESIAN_POINT ( 'NONE',  ( 19.38216949554541202, 50.99863466993042493, 9.382169495545424454 ) ) ;
#9484 = CARTESIAN_POINT ( 'NONE',  ( 14.92337183194729633, 22.67559781766745175, 8.527530157486181039 ) ) ;
#9485 = CARTESIAN_POINT ( 'NONE',  ( 5.076628168052704559, 15.17559781766745175, -8.527530157486179263 ) ) ;
#9486 = CARTESIAN_POINT ( 'NONE',  ( 17.08211943468705840, 50.13708216824730357, -12.26659068614894466 ) ) ;
#9487 = ORIENTED_EDGE ( 'NONE', *, *, #82436, .T. ) ;
#9488 = VECTOR ( 'NONE', #28891, 1000.000000000000000 ) ;
#9489 = EDGE_CURVE ( 'NONE', #19583, #72554, #75842, .T. ) ;
#9490 = CARTESIAN_POINT ( 'NONE',  ( -0.8801773607110991993, 22.85535201082150181, -2.915334737309923874 ) ) ;
#9491 = CARTESIAN_POINT ( 'NONE',  ( 1.602071938427508391, 32.02224192338639597, -6.499999999999986677 ) ) ;
#9492 = ORIENTED_EDGE ( 'NONE', *, *, #6319, .F. ) ;
#9493 = ORIENTED_EDGE ( 'NONE', *, *, #66589, .F. ) ;
#9494 = CARTESIAN_POINT ( 'NONE',  ( 0.5774900079438590739, 12.64701867748817321, -5.440088680355550821 ) ) ;
#9495 = CARTESIAN_POINT ( 'NONE',  ( 0.5774900079438607392, 13.48035201082150358, 5.440088680355550821 ) ) ;
#9496 = CARTESIAN_POINT ( 'NONE',  ( 19.84674366389459621, 63.50893115100078745, 7.409399052514197653E-17 ) ) ;
#9497 = CARTESIAN_POINT ( 'NONE',  ( 13.43411237798105340, 50.58196800326375353, 12.81628187352647963 ) ) ;
#9498 = DIRECTION ( 'NONE',  ( 0.000000000000000000, -1.000000000000000000, 0.000000000000000000 ) ) ;
#9500 = CARTESIAN_POINT ( 'NONE',  ( 10.00000000000000000, 15.55374883491396787, -14.16423886937410082 ) ) ;
#9499 = CARTESIAN_POINT ( 'NONE',  ( 17.39651004071838614, 62.93575266056827644, 6.500000000000032863 ) ) ;
#9501 = CARTESIAN_POINT ( 'NONE',  ( 19.42250999205614193, 30.14701867748817321, 5.440088680355555262 ) ) ;
#9502 = CARTESIAN_POINT ( 'NONE',  ( -0.8801773607111009756, 3.063685344154838397, 1.068504757029289695E-15 ) ) ;
#9503 = ADVANCED_FACE ( 'NONE', ( #78857 ), #32386, .T. ) ;
#9504 = CARTESIAN_POINT ( 'NONE',  ( 7.361572987183170547, 62.05059781766745886, 9.846743663894590881 ) ) ;
#9505 = CARTESIAN_POINT ( 'NONE',  ( 18.17829156368508592, 44.16792564121893605, 6.499999999999926281 ) ) ;
#9506 = CARTESIAN_POINT ( 'NONE',  ( 0.1532563361054100626, 35.80059781766745175, -2.638427012816831230 ) ) ;
#9507 = CARTESIAN_POINT ( 'NONE',  ( 14.92337183194729633, 2.675597817667451750, 8.527530157486181039 ) ) ;
#9508 = CARTESIAN_POINT ( 'NONE',  ( -12.81628187352647608, -40.87636533006958217, 3.903127820947815962E-15 ) ) ;
#9509 = VERTEX_POINT ( 'NONE', #40381 ) ;
#9510 = TOROIDAL_SURFACE ( 'NONE', #15876, 14.49999999999999822, 0.5000000000000000000 ) ;
#9511 = CARTESIAN_POINT ( 'NONE',  ( 7.084665262690076126, 2.022018677488170990, -10.88017736071110164 ) ) ;
#9512 = CARTESIAN_POINT ( 'NONE',  ( 0.1532563361054083140, 1.008931151000784787, 1.131784320476157264E-15 ) ) ;
#9513 = EDGE_CURVE ( 'NONE', #26946, #50486, #62866, .T. ) ;
#9514 = CARTESIAN_POINT ( 'NONE',  ( 21.09922568453595559, 2.040301336597086568, -6.408140936763230044 ) ) ;
#9515 = CARTESIAN_POINT ( 'NONE',  ( 17.96484262340118221, 46.18868534415484106, -7.964842623401177768 ) ) ;
#9517 = CARTESIAN_POINT ( 'NONE',  ( -2.816281873526471635, 38.91530133659708213, -3.434112377981056508 ) ) ;
#9516 = CARTESIAN_POINT ( 'NONE',  ( 4.559911319644449179, 12.23035201082150536, -9.422509992056141925 ) ) ;
#9518 = CARTESIAN_POINT ( 'NONE',  ( -0.3689425029237898834, 16.17874883491396076, -10.36894250292378850 ) ) ;
#9519 = EDGE_CURVE ( 'NONE', #91046, #6749, #21198, .T. ) ;
#9520 = CARTESIAN_POINT ( 'NONE',  ( -2.816281873526471635, 38.91530133659708213, -3.434112377981056508 ) ) ;
#9521 = VERTEX_POINT ( 'NONE', #56362 ) ;
#9522 = CARTESIAN_POINT ( 'NONE',  ( 17.20831665107776587, 57.88393115100078745, 7.208316651077764980 ) ) ;
#9523 = CARTESIAN_POINT ( 'NONE',  ( 4.559911319644449179, 13.89701867748817321, 9.422509992056141925 ) ) ;
#9524 = ADVANCED_FACE ( 'NONE', ( #39397 ), #86855, .F. ) ;
#9525 = CARTESIAN_POINT ( 'NONE',  ( 2.035157376598824452, 33.68868534415484106, 7.964842623401179544 ) ) ;
#9526 = ORIENTED_EDGE ( 'NONE', *, *, #3962, .T. ) ;
#9527 = CARTESIAN_POINT ( 'NONE',  ( 1.472469842513823179, 10.59226448433411782, -4.923371831947296329 ) ) ;
#9528 = SURFACE_SIDE_STYLE ('',( #54523 ) ) ;
#9529 = CARTESIAN_POINT ( 'NONE',  ( 3.468686501387114429, 0.000000000000000000, 4.207853202970351703 ) ) ;
#9530 = CARTESIAN_POINT ( 'NONE',  ( 19.84674366389459621, 13.50893115100078568, 7.409399052514197653E-17 ) ) ;
#9531 = CARTESIAN_POINT ( 'NONE',  ( 5.076628168052704559, 0.1755978176674514724, -8.527530157486179263 ) ) ;
#9532 = CARTESIAN_POINT ( 'NONE',  ( 19.72487221294571569, 49.78217586085237656, 6.499999999999993783 ) ) ;
#9533 = CARTESIAN_POINT ( 'NONE',  ( 1.274849032794231007, 38.57228050351032067, 6.499999999999895195 ) ) ;
#9534 = CARTESIAN_POINT ( 'NONE',  ( 2.035157376598822676, 67.43868534415484817, -7.964842623401177768 ) ) ;
#9536 = ORIENTED_EDGE ( 'NONE', *, *, #79976, .F. ) ;
#9535 = CARTESIAN_POINT ( 'NONE',  ( 1.472469842513823179, 5.592264484334118713, -4.923371831947296329 ) ) ;
#9537 = CARTESIAN_POINT ( 'NONE',  ( 0.1532563361054082862, 61.21726448433412315, 2.638427012816831674 ) ) ;
#9538 = VERTEX_POINT ( 'NONE', #2887 ) ;
#9539 = VERTEX_POINT ( 'NONE', #69890 ) ;
#9540 = DIRECTION ( 'NONE',  ( -0.8320502943378437211, 0.5547001962252290364, 0.000000000000000000 ) ) ;
#9541 = CARTESIAN_POINT ( 'NONE',  ( -2.266590686148945544, 7.220415501580634832, 7.082119434687048631 ) ) ;
#9542 = CARTESIAN_POINT ( 'NONE',  ( -1.099225684535947600, 54.54030133659708923, 6.408140936763237150 ) ) ;
#9543 = CARTESIAN_POINT ( 'NONE',  ( 2.917880565312948704, 2.637082168247300906, 12.26659068614894643 ) ) ;
#9544 = AXIS2_PLACEMENT_3D ( 'NONE', #67886, #30355, #77336 ) ;
#9545 = CARTESIAN_POINT ( 'NONE',  ( -4.164238869374099927, 22.01208216824730357, 3.795296366450308767 ) ) ;
#9546 = DIRECTION ( 'NONE',  ( 0.000000000000000000, 1.000000000000000000, 0.000000000000000000 ) ) ;
#9547 = CARTESIAN_POINT ( 'NONE',  ( 19.42250999205614193, 60.14701867748817676, 5.440088680355555262 ) ) ;
#9548 = CARTESIAN_POINT ( 'NONE',  ( 20.88017736071110875, 15.77201867748817143, -2.915334737309920765 ) ) ;
#9549 = ORIENTED_EDGE ( 'NONE', *, *, #75097, .F. ) ;
#9550 = CARTESIAN_POINT ( 'NONE',  ( 2.791683348922240793, 1.633931151000784565, 7.208316651077764092 ) ) ;
#9552 = MECHANICAL_DESIGN_GEOMETRIC_PRESENTATION_REPRESENTATION (  '', ( #70236 ), #35084 ) ;
#9551 = CARTESIAN_POINT ( 'NONE',  ( 12.63842701281683034, 7.467264484334118713, 9.846743663894596210 ) ) ;
#9553 = CARTESIAN_POINT ( 'NONE',  ( 22.81628187352647785, 31.62363466993042138, 6.195893100308588602E-16 ) ) ;
#9554 = CARTESIAN_POINT ( 'NONE',  ( 10.00000000000000000, 39.75893115100078745, -9.846743663894594434 ) ) ;
#9555 = CARTESIAN_POINT ( 'NONE',  ( 14.24131928502211331, -0.03417435944610275333, 0.4973178280106892446 ) ) ;
#9556 = ADVANCED_FACE ( 'NONE', ( #9376 ), #70385, .T. ) ;
#9557 = CARTESIAN_POINT ( 'NONE',  ( 16.40814093676324603, 17.45696800326375353, -11.09922568453594671 ) ) ;
#9558 = CARTESIAN_POINT ( 'NONE',  ( 4.792102989642838651, -0.03417435944610275333, 15.26149223938176291 ) ) ;
#9559 = CARTESIAN_POINT ( 'NONE',  ( 12.63842701281683922, 29.55059781766745175, -9.846743663894590881 ) ) ;
#9560 = CARTESIAN_POINT ( 'NONE',  ( 0.1532563361054083140, 11.00893115100078568, 1.131784320476157264E-15 ) ) ;
#9561 = ORIENTED_EDGE ( 'NONE', *, *, #55802, .T. ) ;
#9562 = B_SPLINE_CURVE_WITH_KNOTS ( 'NONE', 3,
 ( #17251, #25735, #33689, #93221, #49682, #40236 ),
 .UNSPECIFIED., .F., .F.,
 ( 4, 2, 4 ),
 ( 0.000000000000000000, 0.0002605067024380875980, 0.0005210134048761751960 ),
 .UNSPECIFIED. ) ;
#9563 = ORIENTED_EDGE ( 'NONE', *, *, #50053, .T. ) ;
#9564 = CARTESIAN_POINT ( 'NONE',  ( 12.91533473730993009, 31.60535201082150891, -10.88017736071109987 ) ) ;
#9565 = CARTESIAN_POINT ( 'NONE',  ( 17.08211943468705130, 38.47041550158063217, 12.26659068614894998 ) ) ;
#9566 = CARTESIAN_POINT ( 'NONE',  ( 12.63842701281683922, 44.55059781766745175, -9.846743663894590881 ) ) ;
#9567 = CARTESIAN_POINT ( 'NONE',  ( 19.84674366389459266, 13.71726448433411782, -2.638427012816827677 ) ) ;
#9569 = DIRECTION ( 'NONE',  ( -1.257568779154408793E-17, -1.000000000000000000, 0.000000000000000000 ) ) ;
#9568 = CARTESIAN_POINT ( 'NONE',  ( 21.09922568453595559, 52.04030133659708923, -6.408140936763230044 ) ) ;
#9570 = CARTESIAN_POINT ( 'NONE',  ( 10.00000000000000178, 24.31368534415484106, 10.88017736071110342 ) ) ;
#9571 = DIRECTION ( 'NONE',  ( -0.000000000000000000, 1.000000000000000000, -0.000000000000000000 ) ) ;
#9572 = COLOUR_RGB ( '', 0.40784314, 0.44705882, 0.49803922) ;
#9573 = CARTESIAN_POINT ( 'NONE',  ( 21.09922568453594849, 16.20696800326375353, 6.408140936763242479 ) ) ;
#9574 = CARTESIAN_POINT ( 'NONE',  ( 13.43411237798105340, 15.58196800326374998, 12.81628187352647963 ) ) ;
#9575 = CARTESIAN_POINT ( 'NONE',  ( 10.00000000000000000, 44.75893115100078745, -9.846743663894594434 ) ) ;
#9576 = CARTESIAN_POINT ( 'NONE',  ( 10.88017736071110164, -4.644647989178486647, 2.915334737309921209 ) ) ;
#9577 = CARTESIAN_POINT ( 'NONE',  ( 13.43411237798106583, 42.66530133659707502, -12.81628187352647252 ) ) ;
#9578 = CARTESIAN_POINT ( 'NONE',  ( 14.88585913059882948, 0.2301501830257872971, 1.278057234793960939 ) ) ;
#9580 = FACE_OUTER_BOUND ( 'NONE', #2732, .T. ) ;
#9579 = CARTESIAN_POINT ( 'NONE',  ( 12.91533473730992121, 49.52201867748817676, 10.88017736071110164 ) ) ;
#9581 = CARTESIAN_POINT ( 'NONE',  ( -11.26387636255947733, -65.37812658113172404, 3.999999999999999112 ) ) ;
#9582 = CARTESIAN_POINT ( 'NONE',  ( -7.313705784284419309, 0.5000000000000004441, -13.09617149020753502 ) ) ;
#9583 = CARTESIAN_POINT ( 'NONE',  ( 7.084665262690076126, 49.10535201082149825, 10.88017736071109987 ) ) ;
#9584 = CARTESIAN_POINT ( 'NONE',  ( 7.084665262690076126, 64.10535201082150536, 10.88017736071109987 ) ) ;
#9585 = FACE_OUTER_BOUND ( 'NONE', #11194, .T. ) ;
#9586 = CARTESIAN_POINT ( 'NONE',  ( 11.92686044187656336, 12.18830936912751461, -2.602085213965210642E-15 ) ) ;
#9587 = CARTESIAN_POINT ( 'NONE',  ( 19.42250999205614548, 5.980352010821504471, -5.440088680355545492 ) ) ;
#9588 = CARTESIAN_POINT ( 'NONE',  ( 7.361572987183169658, 64.96726448433412315, -9.846743663894592657 ) ) ;
#9590 = FACE_OUTER_BOUND ( 'NONE', #64282, .T. ) ;
#9589 = CARTESIAN_POINT ( 'NONE',  ( 19.42250999205614193, 25.14701867748817321, 5.440088680355555262 ) ) ;
#9591 = CARTESIAN_POINT ( 'NONE',  ( 0.6178305044545838731, 24.74863466993042493, 9.382169495545420901 ) ) ;
#9592 = EDGE_LOOP ( 'NONE', ( #77530, #49576, #88467, #68377 ) ) ;
#9593 = CARTESIAN_POINT ( 'NONE',  ( -0.8801773607110991993, 52.85535201082151247, -2.915334737309923874 ) ) ;
#9594 = CARTESIAN_POINT ( 'NONE',  ( 10.00000000000000000, 34.75893115100078745, -9.846743663894594434 ) ) ;
#9596 = DIRECTION ( 'NONE',  ( 1.000000000000000000, 0.000000000000000000, -0.000000000000000000 ) ) ;
#9595 = CARTESIAN_POINT ( 'NONE',  ( 16.40814093676324603, 2.456968003263753531, -11.09922568453594671 ) ) ;
#9597 = CARTESIAN_POINT ( 'NONE',  ( 15.44008868035555793, 11.39701867748817143, -9.422509992056140149 ) ) ;
#9598 = CARTESIAN_POINT ( 'NONE',  ( 17.96484262340118221, 36.18868534415484106, -7.964842623401177768 ) ) ;
#9599 = CARTESIAN_POINT ( 'NONE',  ( -0.3689425029237881626, 52.42874883491396076, 10.36894250292379027 ) ) ;
#9600 = CARTESIAN_POINT ( 'NONE',  ( 10.00000000000000000, 39.75893115100078745, -9.846743663894594434 ) ) ;
#9601 = CARTESIAN_POINT ( 'NONE',  ( 0.5774900079438607392, 58.48035201082151247, 5.440088680355550821 ) ) ;
#9602 = DIRECTION ( 'NONE',  ( -0.000000000000000000, -0.000000000000000000, -1.000000000000000000 ) ) ;
#9603 = CARTESIAN_POINT ( 'NONE',  ( -2.266590686148945544, 11.38708216824730179, -7.082119434687050408 ) ) ;
#9604 = EDGE_CURVE ( 'NONE', #107, #91043, #35549, .T. ) ;
#9605 = LINE ( 'NONE', #30614, #49712 ) ;
#9606 = CARTESIAN_POINT ( 'NONE',  ( 1.602071938427508169, 22.02224192338640307, -6.499999999999988454 ) ) ;
#9607 = VECTOR ( 'NONE', #9230, 1000.000000000000000 ) ;
#9609 = VERTEX_POINT ( 'NONE', #56840 ) ;
#9608 = EDGE_CURVE ( 'NONE', #981, #15638, #26831, .T. ) ;
#9610 = ORIENTED_EDGE ( 'NONE', *, *, #67392, .F. ) ;
#9611 = CARTESIAN_POINT ( 'NONE',  ( 17.08211943468705130, 33.47041550158063927, 12.26659068614894998 ) ) ;
#9612 = CARTESIAN_POINT ( 'NONE',  ( -4.164238869374099927, 42.01208216824728936, 3.795296366450308767 ) ) ;
#9613 = CARTESIAN_POINT ( 'NONE',  ( 0.5774900079438607392, 68.48035201082150536, 5.440088680355550821 ) ) ;
#9614 = CARTESIAN_POINT ( 'NONE',  ( 21.09922568453595559, 17.04030133659708923, -6.408140936763230044 ) ) ;
#9615 = CARTESIAN_POINT ( 'NONE',  ( 2.791683348922240793, 61.63393115100079456, 7.208316651077764092 ) ) ;
#9616 = CARTESIAN_POINT ( 'NONE',  ( 17.39651004071838614, 52.93575266056826933, 6.500000000000032863 ) ) ;
#9618 = CARTESIAN_POINT ( 'NONE',  ( 13.43411237798106583, 27.66530133659708568, -12.81628187352647252 ) ) ;
#9617 = CARTESIAN_POINT ( 'NONE',  ( -0.8801773607111008646, 53.27201867748816966, 2.915334737309923430 ) ) ;
#9619 = CARTESIAN_POINT ( 'NONE',  ( 13.79529636645030344, 33.26208216824730357, 14.16423886937410614 ) ) ;
#9620 = EDGE_CURVE ( 'NONE', #21055, #93709, #7544, .T. ) ;
#9621 = CARTESIAN_POINT ( 'NONE',  ( 17.96484262340118221, 24.93868534415484461, 7.964842623401181321 ) ) ;
#9622 = EDGE_CURVE ( 'NONE', #46867, #18218, #79834, .T. ) ;
#9623 = DIRECTION ( 'NONE',  ( 0.000000000000000000, 0.000000000000000000, 1.000000000000000000 ) ) ;
#9624 = CARTESIAN_POINT ( 'NONE',  ( -0.8801773607111008646, 68.27201867748817676, 2.915334737309923430 ) ) ;
#9625 = AXIS2_PLACEMENT_3D ( 'NONE', #2119, #24610, #15636 ) ;
#9626 = CARTESIAN_POINT ( 'NONE',  ( -8.527530157486182816, -9.407735515665871517, -4.923371831947288335 ) ) ;
#9627 = CARTESIAN_POINT ( 'NONE',  ( 5.076628168052703671, 6.842264484334118713, 8.527530157486179263 ) ) ;
#9628 = EDGE_LOOP ( 'NONE', ( #42076, #20815, #49514, #74021, #76422 ) ) ;
#9629 = DIRECTION ( 'NONE',  ( 1.000000000000000000, 0.000000000000000000, 0.000000000000000000 ) ) ;
#9630 = ORIENTED_EDGE ( 'NONE', *, *, #67068, .T. ) ;
#9631 =( NAMED_UNIT ( * ) SI_UNIT ( $, .STERADIAN. ) SOLID_ANGLE_UNIT ( ) );
#9632 = CIRCLE ( 'NONE', #31947, 0.2499999999999997780 ) ;
#9633 = ORIENTED_EDGE ( 'NONE', *, *, #75189, .F. ) ;
#9634 = CARTESIAN_POINT ( 'NONE',  ( 6.204703633549690345, 7.845415501580634832, 14.16423886937410082 ) ) ;
#9636 = CARTESIAN_POINT ( 'NONE',  ( 15.44008868035555793, 11.39701867748817143, -9.422509992056140149 ) ) ;
#9635 = CARTESIAN_POINT ( 'NONE',  ( 19.42250999205614548, 5.980352010821504471, -5.440088680355545492 ) ) ;
#9638 = CARTESIAN_POINT ( 'NONE',  ( 6.565887622018943937, 3.081968003263753531, -12.81628187352647608 ) ) ;
#9637 = CARTESIAN_POINT ( 'NONE',  ( 19.84674366389459621, 33.50893115100078745, 7.409399052514197653E-17 ) ) ;
#9639 = EDGE_CURVE ( 'NONE', #57707, #65696, #17751, .T. ) ;
#9640 = FACE_OUTER_BOUND ( 'NONE', #73323, .T. ) ;
#9641 = CARTESIAN_POINT ( 'NONE',  ( 19.38216949554541202, 5.998634669930420493, 9.382169495545424454 ) ) ;
#9642 = CARTESIAN_POINT ( 'NONE',  ( 3.469446951953614189E-15, 30.37363466993042849, 12.81628187352647608 ) ) ;
#9643 = ORIENTED_EDGE ( 'NONE', *, *, #28800, .F. ) ;
#9644 = CARTESIAN_POINT ( 'NONE',  ( -0.3689425029237881626, 47.42874883491396787, 10.36894250292379027 ) ) ;
#9645 = ORIENTED_EDGE ( 'NONE', *, *, #26323, .T. ) ;
#9646 = EDGE_CURVE ( 'NONE', #11601, #15080, #27200, .T. ) ;
#9647 = CARTESIAN_POINT ( 'NONE',  ( 13.79529636645031943, 55.34541550158062506, -14.16423886937409904 ) ) ;
#9648 = EDGE_LOOP ( 'NONE', ( #53660, #81650, #31401, #10037 ) ) ;
#9649 = CARTESIAN_POINT ( 'NONE',  ( 12.91533473730993009, 26.60535201082150536, -10.88017736071109987 ) ) ;
#9650 = CARTESIAN_POINT ( 'NONE',  ( 4.559911319644449179, 38.89701867748817676, 9.422509992056141925 ) ) ;
#9651 = CARTESIAN_POINT ( 'NONE',  ( 14.92337183194729988, 59.34226448433412315, -8.527530157486177487 ) ) ;
#9652 = CARTESIAN_POINT ( 'NONE',  ( 12.91533473730993009, 41.60535201082149825, -10.88017736071109987 ) ) ;
#9653 = CARTESIAN_POINT ( 'NONE',  ( 7.084665262690076126, 59.10535201082150536, 10.88017736071109987 ) ) ;
#9654 = CARTESIAN_POINT ( 'NONE',  ( 17.96484262340118221, 24.93868534415484461, 7.964842623401181321 ) ) ;
#9655 = B_SPLINE_CURVE_WITH_KNOTS ( 'NONE', 3,
 ( #2805, #47777, #87247, #25298 ),
 .UNSPECIFIED., .F., .F.,
 ( 4, 4 ),
 ( 2.138679957953595447E-16, 0.002392975128318489825 ),
 .UNSPECIFIED. ) ;
#9656 = EDGE_CURVE ( 'NONE', #75294, #60216, #49822, .T. ) ;
#9658 = ORIENTED_EDGE ( 'NONE', *, *, #66371, .T. ) ;
#9657 = CARTESIAN_POINT ( 'NONE',  ( -8.099999999999999645, 80.99999999999994316, -2.900000000000000799 ) ) ;
#9659 = CIRCLE ( 'NONE', #86310, 14.49999999999999822 ) ;
#9660 = FILL_AREA_STYLE_COLOUR ( '', #51425 ) ;
#9661 = ORIENTED_EDGE ( 'NONE', *, *, #69352, .F. ) ;
#9662 = SURFACE_SIDE_STYLE ('',( #39681 ) ) ;
#9663 = CARTESIAN_POINT ( 'NONE',  ( 19.84674366389459266, 43.71726448433410894, -2.638427012816827677 ) ) ;
#9664 = CARTESIAN_POINT ( 'NONE',  ( -14.26139399674453578, 3.905478766663822759E-16, -2.619664342929995282 ) ) ;
#9665 = SURFACE_STYLE_USAGE ( .BOTH. , #16680 ) ;
#9666 = FACE_OUTER_BOUND ( 'NONE', #6308, .T. ) ;
#9667 = CARTESIAN_POINT ( 'NONE',  ( -46.68456736488007408, 103.6675473310227034, 5.775421524742653467 ) ) ;
#9668 = CARTESIAN_POINT ( 'NONE',  ( 8.880000000000020322, 79.82179676972448590, 6.500000000000000888 ) ) ;
#9669 = CARTESIAN_POINT ( 'NONE',  ( 5.076628168052704559, 55.17559781766745175, -8.527530157486179263 ) ) ;
#9670 = CARTESIAN_POINT ( 'NONE',  ( 24.16423886937410614, 54.30374883491396787, 8.672049930838204340E-16 ) ) ;
#9671 = CARTESIAN_POINT ( 'NONE',  ( 7.361572987183170547, 57.05059781766744464, 9.846743663894590881 ) ) ;
#9672 = ORIENTED_EDGE ( 'NONE', *, *, #28883, .T. ) ;
#9673 = DIRECTION ( 'NONE',  ( 6.938893903907222067E-15, 0.000000000000000000, 1.000000000000000000 ) ) ;
#9674 = CARTESIAN_POINT ( 'NONE',  ( 18.52753015748618282, 23.92559781766745530, -4.923371831947291888 ) ) ;
#9675 = CARTESIAN_POINT ( 'NONE',  ( 22.81628187352648496, 46.83196800326376064, -3.434112377981050290 ) ) ;
#9676 = CARTESIAN_POINT ( 'NONE',  ( 7.361572987183169658, 64.96726448433412315, -9.846743663894592657 ) ) ;
#9677 = CARTESIAN_POINT ( 'NONE',  ( 2.035157376598824452, 63.68868534415484106, 7.964842623401179544 ) ) ;
#9678 = CARTESIAN_POINT ( 'NONE',  ( 4.380000000000002558, 1.019547802438462547, -2.750000000000000000 ) ) ;
#9679 = VECTOR ( 'NONE', #57666, 1000.000000000000000 ) ;
#9680 = ORIENTED_EDGE ( 'NONE', *, *, #49895, .T. ) ;
#9681 =( BOUNDED_CURVE ( )  B_SPLINE_CURVE ( 3, ( #66859, #97378, #21368, #50372 ),
 .UNSPECIFIED., .F., .F. ) 
 B_SPLINE_CURVE_WITH_KNOTS ( ( 4, 4 ),
 ( 3.694400132159521011, 4.712388980384689674 ),
 .UNSPECIFIED. ) 
 CURVE ( )  GEOMETRIC_REPRESENTATION_ITEM ( )  RATIONAL_B_SPLINE_CURVE ( ( 1.000000000000000000, 0.9154899770527742398, 0.9154899770527742398, 1.000000000000000000 ) ) 
 REPRESENTATION_ITEM ( '' )  );
#9682 = CARTESIAN_POINT ( 'NONE',  ( -4.164238869374098151, 56.59541550158063927, -3.795296366450310543 ) ) ;
#9683 = CARTESIAN_POINT ( 'NONE',  ( 12.91533473730992121, 24.52201867748816966, 10.88017736071110164 ) ) ;
#9684 = AXIS2_PLACEMENT_3D ( 'NONE', #11424, #95420, #65399 ) ;
#9686 = CARTESIAN_POINT ( 'NONE',  ( 7.084665262690076126, 57.02201867748817676, -10.88017736071110164 ) ) ;
#9685 = CARTESIAN_POINT ( 'NONE',  ( 22.81628187352648496, 16.83196800326374998, -3.434112377981050290 ) ) ;
#9687 = CARTESIAN_POINT ( 'NONE',  ( -8.564643372776702179, 0.5000000000000004441, 12.31449893000734797 ) ) ;
#9688 = CARTESIAN_POINT ( 'NONE',  ( 4.219999999999999751, 37.00000000000000000, 2.750000000000000000 ) ) ;
#9689 = DIRECTION ( 'NONE',  ( -1.000000000000000000, 0.000000000000000000, 0.000000000000000000 ) ) ;
#9690 = PLANE ( 'NONE',  #87115 ) ;
#9691 = EDGE_CURVE ( 'NONE', #14954, #31369, #45786, .T. ) ;
#9692 = CARTESIAN_POINT ( 'NONE',  ( 19.84674366389459621, 48.50893115100078745, 7.409399052514197653E-17 ) ) ;
#9693 = CARTESIAN_POINT ( 'NONE',  ( 1.915564264621337554, 4.132324795315745510E-16, 14.37291249357991774 ) ) ;
#9694 = CARTESIAN_POINT ( 'NONE',  ( 14.16423886937410437, 29.09541550158064638, 3.795296366450304770 ) ) ;
#9695 = CARTESIAN_POINT ( 'NONE',  ( 21.09922568453595559, 7.040301336597086568, -6.408140936763230044 ) ) ;
#9696 = CARTESIAN_POINT ( 'NONE',  ( 7.084665262690076126, 19.10535201082150181, 10.88017736071109987 ) ) ;
#9697 = ADVANCED_FACE ( 'NONE', ( #43798 ), #5820, .F. ) ;
#9698 = CARTESIAN_POINT ( 'NONE',  ( -4.164238869374099039, 36.80374883491396787, 8.674139862899312516E-16 ) ) ;
#9699 = CARTESIAN_POINT ( 'NONE',  ( -0.3689425029237881626, 27.42874883491397142, 10.36894250292379027 ) ) ;
#9700 = CARTESIAN_POINT ( 'NONE',  ( 13.79529636645030344, 58.26208216824728936, 14.16423886937410614 ) ) ;
#9701 = CARTESIAN_POINT ( 'NONE',  ( 10.00000000000000000, 29.75893115100078745, -9.846743663894594434 ) ) ;
#9702 = CARTESIAN_POINT ( 'NONE',  ( 2.791683348922237240, 20.38393115100078745, -7.208316651077763204 ) ) ;
#9703 = CARTESIAN_POINT ( 'NONE',  ( 10.00000000000000000, 16.81368534415483751, -10.88017736071110342 ) ) ;
#9704 = ORIENTED_EDGE ( 'NONE', *, *, #63333, .T. ) ;
#9705 = CARTESIAN_POINT ( 'NONE',  ( 12.63842701281683922, 44.55059781766745175, -9.846743663894590881 ) ) ;
#9706 = CARTESIAN_POINT ( 'NONE',  ( 20.88017736071110164, 45.35535201082149115, 2.915334737309930979 ) ) ;
#9707 = CARTESIAN_POINT ( 'NONE',  ( 10.00000000000000178, 57.25893115100078745, 9.846743663894594434 ) ) ;
#9709 = DIRECTION ( 'NONE',  ( -1.000000000000000000, 0.000000000000000000, 0.000000000000000000 ) ) ;
#9708 = CARTESIAN_POINT ( 'NONE',  ( 24.16423886937410614, 19.51208216824729647, -3.795296366450302550 ) ) ;
#9710 = CARTESIAN_POINT ( 'NONE',  ( 10.64017930668198453, 15.00000000000000000, 10.57291749337222875 ) ) ;
#9711 = CARTESIAN_POINT ( 'NONE',  ( 1.472469842513823179, 15.59226448433411960, -4.923371831947296329 ) ) ;
#9712 = CARTESIAN_POINT ( 'NONE',  ( 22.81628187352647785, 51.62363466993042493, 6.195893100308588602E-16 ) ) ;
#9713 = CARTESIAN_POINT ( 'NONE',  ( 0.1532563361054100626, 50.80059781766745175, -2.638427012816831230 ) ) ;
#9714 = ORIENTED_EDGE ( 'NONE', *, *, #74034, .T. ) ;
#9715 = DIRECTION ( 'NONE',  ( -0.2840153447039170387, 0.000000000000000000, -0.9588197348681947174 ) ) ;
#9716 = CYLINDRICAL_SURFACE ( 'NONE', #50768, 0.5000000000000004441 ) ;
#9717 = CARTESIAN_POINT ( 'NONE',  ( 4.559911319644449179, 7.230352010821505360, -9.422509992056141925 ) ) ;
#9718 = CARTESIAN_POINT ( 'NONE',  ( 15.44008868035555793, 56.39701867748817676, -9.422509992056140149 ) ) ;
#9719 = CARTESIAN_POINT ( 'NONE',  ( -4.164238869374098151, 6.595415501580634832, -3.795296366450310543 ) ) ;
#9720 = CARTESIAN_POINT ( 'NONE',  ( 5.076628168052704559, 0.1755978176674514724, -8.527530157486179263 ) ) ;
#9721 = CARTESIAN_POINT ( 'NONE',  ( 2.791683348922237240, 55.38393115100078745, -7.208316651077763204 ) ) ;
#9722 = CARTESIAN_POINT ( 'NONE',  ( 10.00000000000000000, 21.81368534415484106, -10.88017736071110342 ) ) ;
#9723 = CARTESIAN_POINT ( 'NONE',  ( -0.07285406091746288171, 0.4131759111665359585, 10.00000000000000000 ) ) ;
#9724 = AXIS2_PLACEMENT_3D ( 'NONE', #48543, #56547, #87042 ) ;
#9725 = CARTESIAN_POINT ( 'NONE',  ( 19.84674366389459266, 3.717264484334118713, -2.638427012816827677 ) ) ;
#9726 = CARTESIAN_POINT ( 'NONE',  ( 10.00000000000000178, 55.37363466993042493, 12.81628187352647608 ) ) ;
#9728 = ORIENTED_EDGE ( 'NONE', *, *, #15044, .T. ) ;
#9727 = EDGE_CURVE ( 'NONE', #21688, #71973, #35816, .T. ) ;
#9729 = ORIENTED_EDGE ( 'NONE', *, *, #85921, .F. ) ;
#9730 = AXIS2_PLACEMENT_3D ( 'NONE', #15976, #46949, #63431 ) ;
#9731 = LINE ( 'NONE', #24739, #85269 ) ;
#9732 = CARTESIAN_POINT ( 'NONE',  ( 14.99847009497950800, 14.49999999999999112, 0.2142307401081135487 ) ) ;
#9733 = CARTESIAN_POINT ( 'NONE',  ( 17.08211943468705840, 45.13708216824730357, -12.26659068614894466 ) ) ;
#9734 = CARTESIAN_POINT ( 'NONE',  ( 5.076628168052703671, 41.84226448433411605, 8.527530157486179263 ) ) ;
#9735 = CARTESIAN_POINT ( 'NONE',  ( 2.791683348922237240, 20.38393115100078745, -7.208316651077763204 ) ) ;
#9736 = DIRECTION ( 'NONE',  ( 1.000000000000000000, -6.938893903907221278E-15, -6.938893903907221278E-15 ) ) ;
#9738 = CARTESIAN_POINT ( 'NONE',  ( 2.791683348922237240, 65.38393115100078035, -7.208316651077763204 ) ) ;
#9737 = CARTESIAN_POINT ( 'NONE',  ( 20.88017736071110519, 15.56368534415483751, 2.639326808657452039E-16 ) ) ;
#9739 = CARTESIAN_POINT ( 'NONE',  ( 13.82192141328807011, 15.00000000000000000, 4.382292601468777526 ) ) ;
#9740 = EDGE_CURVE ( 'NONE', #23897, #81593, #72814, .T. ) ;
#9741 = CARTESIAN_POINT ( 'NONE',  ( 6.204703633549690345, 60.76208216824730357, -14.16423886937410259 ) ) ;
#9742 = DIRECTION ( 'NONE',  ( -0.000000000000000000, -1.000000000000000000, -0.000000000000000000 ) ) ;
#9743 = CARTESIAN_POINT ( 'NONE',  ( 17.99999999999999645, 78.09931407715556873, 3.985200473436547597 ) ) ;
#9744 = CARTESIAN_POINT ( 'NONE',  ( 19.42250999205614548, 60.98035201082151247, -5.440088680355545492 ) ) ;
#9745 = CARTESIAN_POINT ( 'NONE',  ( 1.472469842513823179, 10.59226448433411782, -4.923371831947296329 ) ) ;
#9746 = CARTESIAN_POINT ( 'NONE',  ( -5.331138373813207210, -28.69357394137744421, 3.749999999999193534 ) ) ;
#9747 = ORIENTED_EDGE ( 'NONE', *, *, #42576, .T. ) ;
#9748 = DIRECTION ( 'NONE',  ( 0.000000000000000000, 1.000000000000000000, 0.000000000000000000 ) ) ;
#9749 = EDGE_LOOP ( 'NONE', ( #80712, #87828, #97382, #65064 ) ) ;
#9750 = PRESENTATION_LAYER_ASSIGNMENT (  '', '', ( #76821 ) ) ;
#9751 = CARTESIAN_POINT ( 'NONE',  ( 19.84674366389459266, 28.30059781766745886, 2.638427012816836559 ) ) ;
#9752 = VERTEX_POINT ( 'NONE', #34820 ) ;
#9753 = CARTESIAN_POINT ( 'NONE',  ( 6.204703633549690345, 30.76208216824730357, -14.16423886937410259 ) ) ;
#9754 = CARTESIAN_POINT ( 'NONE',  ( 5.076628168052703671, 16.84226448433411960, 8.527530157486179263 ) ) ;
#9755 = CARTESIAN_POINT ( 'NONE',  ( 19.42250999205614548, 40.98035201082150536, -5.440088680355545492 ) ) ;
#9756 = CARTESIAN_POINT ( 'NONE',  ( 15.00000000000000000, 77.07179676972447169, -6.250000000000000000 ) ) ;
#9757 = ORIENTED_EDGE ( 'NONE', *, *, #1205, .T. ) ;
#9758 = AXIS2_PLACEMENT_3D ( 'NONE', #41077, #93566, #25099 ) ;
#9759 = CARTESIAN_POINT ( 'NONE',  ( 2.035157376598824452, 38.68868534415483396, 7.964842623401179544 ) ) ;
#9760 = DIRECTION ( 'NONE',  ( 0.000000000000000000, 0.000000000000000000, -1.000000000000000000 ) ) ;
#9761 = EDGE_CURVE ( 'NONE', #53936, #51000, #85652, .T. ) ;
#9762 = B_SPLINE_CURVE_WITH_KNOTS ( 'NONE', 3,
 ( #65596, #43596, #28097, #97128, #57609, #57118, #28598, #74084, #5617, #59087, #51604, #34605, #6103, #89595, #87615, #64605, #21105, #82088, #13599, #44079, #74588, #19617 ),
 .UNSPECIFIED., .F., .F.,
 ( 4, 2, 2, 2, 2, 2, 2, 2, 2, 2, 4 ),
 ( -6.000000000051943759E-08, 0.002788756707268867478, 0.005577573414537735468, 0.01115520682907547058, 0.02231047365815094080, 0.03346574048722640582, 0.04462100731630187084, 0.06693154097445282169, 0.07808680780352829365, 0.08366444121806604350, 0.08924207463260379336 ),
 .UNSPECIFIED. ) ;
#9763 = CARTESIAN_POINT ( 'NONE',  ( -11.09922568453595382, -11.29303199673624469, -6.408140936763226492 ) ) ;
#9764 = ORIENTED_EDGE ( 'NONE', *, *, #31800, .T. ) ;
#9765 = CARTESIAN_POINT ( 'NONE',  ( 10.00000000000000000, 41.81368534415484106, -10.88017736071110342 ) ) ;
#9766 = VECTOR ( 'NONE', #2853, 1000.000000000000000 ) ;
#9767 = CARTESIAN_POINT ( 'NONE',  ( -0.3689425029237898834, 11.17874883491396787, -10.36894250292378850 ) ) ;
#9768 = EDGE_LOOP ( 'NONE', ( #56220, #97938, #49430, #27017, #64205, #41047 ) ) ;
#9769 = ADVANCED_FACE ( 'NONE', ( #32739 ), #24770, .T. ) ;
#9770 = ORIENTED_EDGE ( 'NONE', *, *, #23064, .T. ) ;
#9771 = CARTESIAN_POINT ( 'NONE',  ( 6.565887622018943937, 35.16530133659708923, 12.81628187352647430 ) ) ;
#9772 = CARTESIAN_POINT ( 'NONE',  ( 19.84674366389459266, 8.300597817667451750, 2.638427012816836559 ) ) ;
#9773 = DIRECTION ( 'NONE',  ( 0.000000000000000000, -1.000000000000000000, 0.000000000000000000 ) ) ;
#9774 = DIRECTION ( 'NONE',  ( 1.000000000000000000, 0.000000000000000000, 0.000000000000000000 ) ) ;
#9775 = CARTESIAN_POINT ( 'NONE',  ( 0.1532563361054082862, 31.21726448433412315, 2.638427012816831674 ) ) ;
#9776 = ORIENTED_EDGE ( 'NONE', *, *, #81843, .T. ) ;
#9777 = CARTESIAN_POINT ( 'NONE',  ( -9.024359497401759356, 75.07164295747612925, -2.900000000000000799 ) ) ;
#9778 = CARTESIAN_POINT ( 'NONE',  ( 7.084665262690076126, 52.02201867748816255, -10.88017736071110164 ) ) ;
#9779 = CARTESIAN_POINT ( 'NONE',  ( 9.402796353261051010, 0.5000000000000004441, 11.68706210897763320 ) ) ;
#9780 = CARTESIAN_POINT ( 'NONE',  ( 0.000000000000000000, 14.49999999999999822, 0.000000000000000000 ) ) ;
#9781 = CARTESIAN_POINT ( 'NONE',  ( 12.63842701281683922, 9.550597817667449974, -9.846743663894590881 ) ) ;
#9782 = CARTESIAN_POINT ( 'NONE',  ( 6.565887622018943937, 10.16530133659708746, 12.81628187352647430 ) ) ;
#9783 = CARTESIAN_POINT ( 'NONE',  ( -15.86177583122253765, 15.00000000000000000, 2.069169861586545700 ) ) ;
#9784 = CARTESIAN_POINT ( 'NONE',  ( 10.00000000000000178, 37.25893115100078745, 9.846743663894594434 ) ) ;
#9785 = DIRECTION ( 'NONE',  ( -2.107602052970795044E-16, 1.000000000000000000, 0.000000000000000000 ) ) ;
#9786 = CARTESIAN_POINT ( 'NONE',  ( 2.917880565312948704, 7.637082168247301794, 12.26659068614894643 ) ) ;
#9787 = CARTESIAN_POINT ( 'NONE',  ( 7.361572987183169658, 19.96726448433411960, -9.846743663894592657 ) ) ;
#9788 = CARTESIAN_POINT ( 'NONE',  ( -2.816281873526471635, 23.91530133659708568, -3.434112377981056508 ) ) ;
#9790 = LINE ( 'NONE', #40289, #8259 ) ;
#9789 = CARTESIAN_POINT ( 'NONE',  ( 0.000000000000000000, 0.5000000000000004441, 0.000000000000000000 ) ) ;
#9791 = CARTESIAN_POINT ( 'NONE',  ( 7.084665262690076126, 44.10535201082151247, 10.88017736071109987 ) ) ;
#9792 = CARTESIAN_POINT ( 'NONE',  ( 0.6178305044545818747, -1.501365330069579951, -9.382169495545419124 ) ) ;
#9793 = AXIS2_PLACEMENT_3D ( 'NONE', #1848, #55312, #32305 ) ;
#9794 = CIRCLE ( 'NONE', #72016, 0.2500000000000002220 ) ;
#9795 = CARTESIAN_POINT ( 'NONE',  ( 9.641087339108921128, 0.04922511925147053657, -11.16671550067049878 ) ) ;
#9796 = CARTESIAN_POINT ( 'NONE',  ( 1.472469842513823179, 25.59226448433412315, -4.923371831947296329 ) ) ;
#9797 = CARTESIAN_POINT ( 'NONE',  ( 7.084665262690076126, 12.02201867748817143, -10.88017736071110164 ) ) ;
#9798 = CARTESIAN_POINT ( 'NONE',  ( -1.099225684535947600, 18.70696800326375353, -6.408140936763238038 ) ) ;
#9799 = CARTESIAN_POINT ( 'NONE',  ( 1.472469842513823179, 20.59226448433411960, -4.923371831947296329 ) ) ;
#9800 = CARTESIAN_POINT ( 'NONE',  ( 13.21236992757673789, 0.000000000000000000, -5.338143956176714333 ) ) ;
#9801 = VECTOR ( 'NONE', #32931, 1000.000000000000000 ) ;
#9802 = CARTESIAN_POINT ( 'NONE',  ( 10.00000000000000000, 21.81368534415484106, -10.88017736071110342 ) ) ;
#9803 = EDGE_LOOP ( 'NONE', ( #85046, #23767, #55361, #74914 ) ) ;
#9804 = CARTESIAN_POINT ( 'NONE',  ( 20.88017736071110875, 60.77201867748817676, -2.915334737309920765 ) ) ;
#9805 = CARTESIAN_POINT ( 'NONE',  ( 4.698669664746458530, 0.000000000000000000, 2.767727949825354195 ) ) ;
#9807 = CARTESIAN_POINT ( 'NONE',  ( 17.96484262340118221, 21.18868534415483396, -7.964842623401177768 ) ) ;
#9806 = CARTESIAN_POINT ( 'NONE',  ( 18.52753015748617571, 48.09226448433412315, 4.923371831947298993 ) ) ;
#9808 =( NAMED_UNIT ( * ) PLANE_ANGLE_UNIT ( ) SI_UNIT ( $, .RADIAN. ) );
#9809 = CARTESIAN_POINT ( 'NONE',  ( 20.88017736071110164, 40.35535201082150536, 2.915334737309930979 ) ) ;
#9811 = CARTESIAN_POINT ( 'NONE',  ( -1.926860441876562025, 19.47997603579417358, -3.195792623639529761 ) ) ;
#9810 = CARTESIAN_POINT ( 'NONE',  ( -0.8801773607110991993, 12.85535201082150358, -2.915334737309923874 ) ) ;
#9812 = CARTESIAN_POINT ( 'NONE',  ( 1.472469842513823179, 10.59226448433411782, -4.923371831947296329 ) ) ;
#9813 = CARTESIAN_POINT ( 'NONE',  ( 0.1532563361054082862, 41.21726448433411605, 2.638427012816831674 ) ) ;
#9814 = STYLED_ITEM ( 'NONE', ( #58621 ), #33558 ) ;
#9815 = CARTESIAN_POINT ( 'NONE',  ( 18.00000000000000711, 77.35013740655264769, -4.131316298316595415 ) ) ;
#9816 = DIRECTION ( 'NONE',  ( 0.000000000000000000, 0.000000000000000000, -1.000000000000000000 ) ) ;
#9817 = EDGE_CURVE ( 'NONE', #57516, #86312, #10256, .T. ) ;
#9818 = CARTESIAN_POINT ( 'NONE',  ( 1.472469842513823179, 66.42559781766745175, 4.923371831947296329 ) ) ;
#9819 = CARTESIAN_POINT ( 'NONE',  ( -12.54397927573557681, 14.76930270348881002, -8.117058495689191133 ) ) ;
#9820 = CARTESIAN_POINT ( 'NONE',  ( 22.26659068614894466, 18.88708216824730002, 7.082119434687054849 ) ) ;
#9821 = VECTOR ( 'NONE', #17961, 1000.000000000000000 ) ;
#9822 = CARTESIAN_POINT ( 'NONE',  ( 14.92337183194729633, 42.67559781766745886, 8.527530157486181039 ) ) ;
#9823 = CARTESIAN_POINT ( 'NONE',  ( 7.079515573063597245, -88.00917032380692717, -3.749999999999998668 ) ) ;
#9824 = EDGE_LOOP ( 'NONE', ( #17145, #10361, #38287, #96638, #48377 ) ) ;
#9825 = CARTESIAN_POINT ( 'NONE',  ( 19.42250999205614548, 5.980352010821504471, -5.440088680355545492 ) ) ;
#9826 = CARTESIAN_POINT ( 'NONE',  ( 14.92337183194729988, 19.34226448433411960, -8.527530157486177487 ) ) ;
#9828 = CARTESIAN_POINT ( 'NONE',  ( 8.629999999999995453, 41.24999999999999289, -6.500000000000000888 ) ) ;
#9827 = CARTESIAN_POINT ( 'NONE',  ( -4.873787042390880231, -0.03417435944610275333, 13.39061984619915791 ) ) ;
#9829 = CARTESIAN_POINT ( 'NONE',  ( 7.084665262690076126, 52.02201867748816255, -10.88017736071110164 ) ) ;
#9830 = PLANE ( 'NONE',  #59567 ) ;
#9831 = CARTESIAN_POINT ( 'NONE',  ( 0.5774900079438607392, 13.48035201082150358, 5.440088680355550821 ) ) ;
#9832 = VECTOR ( 'NONE', #87552, 1000.000000000000000 ) ;
#9833 = CARTESIAN_POINT ( 'NONE',  ( 3.591859063236761518, 49.95696800326375353, 11.09922568453594849 ) ) ;
#9834 = CARTESIAN_POINT ( 'NONE',  ( 6.565887622018943937, 10.16530133659708746, 12.81628187352647430 ) ) ;
#9835 = CARTESIAN_POINT ( 'NONE',  ( 2.791683348922237240, 15.38393115100078212, -7.208316651077763204 ) ) ;
#9836 = ORIENTED_EDGE ( 'NONE', *, *, #37057, .F. ) ;
#9837 = SURFACE_STYLE_USAGE ( .BOTH. , #62823 ) ;
#9838 = CARTESIAN_POINT ( 'NONE',  ( -14.67697702673046933, 15.00000000000000000, 6.361111679013309761 ) ) ;
#9839 = CARTESIAN_POINT ( 'NONE',  ( 2.917880565312950480, 55.97041550158063217, -12.26659068614894821 ) ) ;
#9840 = CARTESIAN_POINT ( 'NONE',  ( 13.79529636645030344, 23.26208216824730002, 14.16423886937410614 ) ) ;
#9841 = CARTESIAN_POINT ( 'NONE',  ( 10.00000000000000178, 19.31368534415484106, 10.88017736071110342 ) ) ;
#9842 = CARTESIAN_POINT ( 'NONE',  ( 20.88017736071110519, 55.56368534415484817, 2.639326808657452039E-16 ) ) ;
#9843 = FILL_AREA_STYLE_COLOUR ( '', #65485 ) ;
#9844 = CARTESIAN_POINT ( 'NONE',  ( -46.44000000000001194, 100.8660254037844339, -9.500000000000000000 ) ) ;
#9845 = CARTESIAN_POINT ( 'NONE',  ( 12.63842701281683034, 2.467264484334118269, 9.846743663894596210 ) ) ;
#9846 = PRESENTATION_STYLE_ASSIGNMENT (( #92839 ) ) ;
#9847 = CARTESIAN_POINT ( 'NONE',  ( 0.1532563361054100626, 15.80059781766745353, -2.638427012816831230 ) ) ;
#9848 = CARTESIAN_POINT ( 'NONE',  ( 7.361572987183169658, -0.03273551566588185635, -9.846743663894592657 ) ) ;
#9849 = STYLED_ITEM ( 'NONE', ( #84623 ), #74133 ) ;
#9850 = CARTESIAN_POINT ( 'NONE',  ( -12.34086200392831678, 0.000000000000000000, 7.124999999999885425 ) ) ;
#9851 = CARTESIAN_POINT ( 'NONE',  ( 2.791683348922237240, 30.38393115100078390, -7.208316651077763204 ) ) ;
#9852 = CARTESIAN_POINT ( 'NONE',  ( 1.472469842513823179, 55.59226448433412315, -4.923371831947296329 ) ) ;
#9853 = CARTESIAN_POINT ( 'NONE',  ( 12.91533473730992121, 14.52201867748817143, 10.88017736071110164 ) ) ;
#9854 = B_SPLINE_CURVE_WITH_KNOTS ( 'NONE', 3,
 ( #40438, #46928, #47911, #15955, #38468, #55427 ),
 .UNSPECIFIED., .F., .F.,
 ( 4, 2, 4 ),
 ( 3.409110551435918168E-05, 0.0004400426677361854357, 0.0008459942299580117033 ),
 .UNSPECIFIED. ) ;
#9855 = EDGE_CURVE ( 'NONE', #86126, #63027, #4556, .T. ) ;
#9856 = CARTESIAN_POINT ( 'NONE',  ( 6.565887622018943937, 28.08196800326375353, -12.81628187352647608 ) ) ;
#9857 = CARTESIAN_POINT ( 'NONE',  ( 17.96484262340118221, 51.18868534415483396, -7.964842623401177768 ) ) ;
#9858 = CARTESIAN_POINT ( 'NONE',  ( 18.52753015748617571, 23.09226448433411960, 4.923371831947298993 ) ) ;
#9860 = CARTESIAN_POINT ( 'NONE',  ( 0.1532563361054083140, 11.00893115100078568, 1.131784320476157264E-15 ) ) ;
#9859 = CARTESIAN_POINT ( 'NONE',  ( 20.36894250292379382, 48.67874883491396076, 10.36894250292379205 ) ) ;
#9861 = PLANE ( 'NONE',  #95068 ) ;
#9862 = CARTESIAN_POINT ( 'NONE',  ( 2.791683348922237240, 55.38393115100078745, -7.208316651077763204 ) ) ;
#9864 = CARTESIAN_POINT ( 'NONE',  ( 17.08211943468705130, 13.47041550158063572, 12.26659068614894998 ) ) ;
#9863 = CARTESIAN_POINT ( 'NONE',  ( 5.076628168052704559, 30.17559781766745175, -8.527530157486179263 ) ) ;
#9865 = EDGE_CURVE ( 'NONE', #1556, #25275, #41580, .T. ) ;
#9866 = CARTESIAN_POINT ( 'NONE',  ( 24.16423886937410614, 24.51208216824730002, -3.795296366450302550 ) ) ;
#9867 = CARTESIAN_POINT ( 'NONE',  ( 0.1532563361054083140, 36.00893115100078745, 1.131784320476157264E-15 ) ) ;
#9868 = CARTESIAN_POINT ( 'NONE',  ( -0.8801773607111008646, 48.27201867748816966, 2.915334737309923430 ) ) ;
#9869 = CARTESIAN_POINT ( 'NONE',  ( 19.42250999205614548, 25.98035201082150891, -5.440088680355545492 ) ) ;
#9870 = CARTESIAN_POINT ( 'NONE',  ( 20.88017736071110875, 40.77201867748818387, -2.915334737309920765 ) ) ;
#9871 = CARTESIAN_POINT ( 'NONE',  ( 12.91533473730992121, 29.52201867748817321, 10.88017736071110164 ) ) ;
#9872 = ORIENTED_EDGE ( 'NONE', *, *, #18920, .F. ) ;
#9873 = CARTESIAN_POINT ( 'NONE',  ( 10.00000000000000178, 35.37363466993042493, 12.81628187352647608 ) ) ;
#9874 = CARTESIAN_POINT ( 'NONE',  ( 2.035157376598822676, 37.43868534415484106, -7.964842623401177768 ) ) ;
#9875 = VERTEX_POINT ( 'NONE', #23799 ) ;
#9876 = CARTESIAN_POINT ( 'NONE',  ( 3.591859063236763294, 53.29030133659708923, -11.09922568453595026 ) ) ;
#9877 = DIRECTION ( 'NONE',  ( 0.09584575252022037306, 0.000000000000000000, 0.9953961983671790748 ) ) ;
#9878 = VERTEX_POINT ( 'NONE', #54262 ) ;
#9879 = CARTESIAN_POINT ( 'NONE',  ( -0.8801773607110991993, 52.85535201082151247, -2.915334737309923874 ) ) ;
#9880 = MECHANICAL_DESIGN_GEOMETRIC_PRESENTATION_REPRESENTATION (  '', ( #22587 ), #81652 ) ;
#9881 = CARTESIAN_POINT ( 'NONE',  ( 10.58981376305288613, -0.03417435944610275333, -9.535111140613709679 ) ) ;
#9882 = DIRECTION ( 'NONE',  ( 0.000000000000000000, 1.000000000000000000, 0.000000000000000000 ) ) ;
#9883 = CARTESIAN_POINT ( 'NONE',  ( 13.79529636645030344, 63.26208216824730357, 14.16423886937410614 ) ) ;
#9884 = CARTESIAN_POINT ( 'NONE',  ( 0.1532563361054100626, 10.80059781766745175, -2.638427012816831230 ) ) ;
#9885 = CARTESIAN_POINT ( 'NONE',  ( -2.266590686148945544, 1.387082168247301128, -7.082119434687050408 ) ) ;
#9886 = CARTESIAN_POINT ( 'NONE',  ( 17.20831665107776587, 9.133931151000787452, -7.208316651077762316 ) ) ;
#9887 = CARTESIAN_POINT ( 'NONE',  ( 10.00000000000000000, 16.81368534415483751, -10.88017736071110342 ) ) ;
#9888 = CARTESIAN_POINT ( 'NONE',  ( 1.472469842513823179, 45.59226448433412315, -4.923371831947296329 ) ) ;
#9889 = VERTEX_POINT ( 'NONE', #55248 ) ;
#9890 = CARTESIAN_POINT ( 'NONE',  ( 10.00000000000000178, 52.25893115100078745, 9.846743663894594434 ) ) ;
#9891 = CARTESIAN_POINT ( 'NONE',  ( 2.831191079880678085, 79.91181047996344944, 9.500000000000000000 ) ) ;
#9892 = CARTESIAN_POINT ( 'NONE',  ( 20.88017736071110875, 45.77201867748816966, -2.915334737309920765 ) ) ;
#9893 = CARTESIAN_POINT ( 'NONE',  ( 19.84674366389459621, 48.50893115100078745, 7.409399052514197653E-17 ) ) ;
#9894 = CARTESIAN_POINT ( 'NONE',  ( 19.38216949554541557, 27.24863466993041783, -9.382169495545420901 ) ) ;
#9896 = CARTESIAN_POINT ( 'NONE',  ( 2.035157376598824452, 68.68868534415484817, 7.964842623401179544 ) ) ;
#9895 = FACE_OUTER_BOUND ( 'NONE', #17618, .T. ) ;
#9897 = CARTESIAN_POINT ( 'NONE',  ( 20.88017736071110875, 45.77201867748816966, -2.915334737309920765 ) ) ;
#9898 = CARTESIAN_POINT ( 'NONE',  ( 10.00000000000000000, 6.813685344154838397, -10.88017736071110342 ) ) ;
#9899 = EDGE_CURVE ( 'NONE', #77971, #37161, #35525, .T. ) ;
#9900 = CARTESIAN_POINT ( 'NONE',  ( 16.40814093676324603, 47.45696800326375353, -11.09922568453594671 ) ) ;
#9901 = DIRECTION ( 'NONE',  ( 0.000000000000000000, 0.000000000000000000, -1.000000000000000000 ) ) ;
#9902 = ORIENTED_EDGE ( 'NONE', *, *, #6008, .F. ) ;
#9903 = CARTESIAN_POINT ( 'NONE',  ( 10.00000000000000000, 27.87363466993042138, -12.81628187352647608 ) ) ;
#9904 = CARTESIAN_POINT ( 'NONE',  ( 10.00000000000000000, 21.81368534415484106, -10.88017736071110342 ) ) ;
#9905 = CIRCLE ( 'NONE', #5112, 1.000000000000000888 ) ;
#9906 = ORIENTED_EDGE ( 'NONE', *, *, #4415, .F. ) ;
#9907 = B_SPLINE_CURVE_WITH_KNOTS ( 'NONE', 3,
 ( #21904, #27900, #96925, #5427, #81399, #6890 ),
 .UNSPECIFIED., .F., .F.,
 ( 4, 2, 4 ),
 ( 0.000000000000000000, 0.0002605067024380873270, 0.0005210134048761746539 ),
 .UNSPECIFIED. ) ;
#9908 = CARTESIAN_POINT ( 'NONE',  ( 4.559911319644449179, 68.89701867748817676, 9.422509992056141925 ) ) ;
#9909 = CARTESIAN_POINT ( 'NONE',  ( 17.20831665107776587, 44.13393115100078745, -7.208316651077762316 ) ) ;
#9911 = CARTESIAN_POINT ( 'NONE',  ( 17.20831665107776587, 32.88393115100078745, 7.208316651077764980 ) ) ;
#9910 = CARTESIAN_POINT ( 'NONE',  ( 18.52753015748618282, 18.92559781766745175, -4.923371831947291888 ) ) ;
#9912 = CARTESIAN_POINT ( 'NONE',  ( -11.42264910390652233, -90.33240963618720798, 3.750000000000000888 ) ) ;
#9913 = CARTESIAN_POINT ( 'NONE',  ( -6.715867195167532167, 15.00000000000000000, 12.85095824508320028 ) ) ;
#9914 = CARTESIAN_POINT ( 'NONE',  ( 12.63842701281683922, 29.55059781766745175, -9.846743663894590881 ) ) ;
#9915 = CARTESIAN_POINT ( 'NONE',  ( 0.1077916266722770133, 52.24062864464239198, -6.478736007406002528 ) ) ;
#9916 = CARTESIAN_POINT ( 'NONE',  ( -15.94000000000001371, 93.50000000000000000, 9.500000000000000000 ) ) ;
#9918 = CARTESIAN_POINT ( 'NONE',  ( 5.076628168052703671, 1.842264484334118047, 8.527530157486179263 ) ) ;
#9917 = CARTESIAN_POINT ( 'NONE',  ( 7.361572987183170547, 22.05059781766745530, 9.846743663894590881 ) ) ;
#9920 = VERTEX_POINT ( 'NONE', #39286 ) ;
#9919 = CARTESIAN_POINT ( 'NONE',  ( 5.076628168052704559, 40.17559781766745175, -8.527530157486179263 ) ) ;
#9921 = CARTESIAN_POINT ( 'NONE',  ( 13.74385066382883913, 14.76930270348882779, -5.860428621090359336 ) ) ;
#9922 = CARTESIAN_POINT ( 'NONE',  ( -1.099225684535947600, 24.54030133659708923, 6.408140936763237150 ) ) ;
#9923 = CARTESIAN_POINT ( 'NONE',  ( -9.000000000000001776, 80.99999999999994316, -2.900000000000000799 ) ) ;
#9924 = CARTESIAN_POINT ( 'NONE',  ( 2.917880565312950480, 40.97041550158063217, -12.26659068614894821 ) ) ;
#9925 = CARTESIAN_POINT ( 'NONE',  ( 0.1532563361054082862, 21.21726448433412315, 2.638427012816831674 ) ) ;
#9926 = CARTESIAN_POINT ( 'NONE',  ( 1.472469842513823179, 5.592264484334118713, -4.923371831947296329 ) ) ;
#9927 = LINE ( 'NONE', #62912, #66400 ) ;
#9928 = CARTESIAN_POINT ( 'NONE',  ( 6.204703633549690345, 47.84541550158064638, 14.16423886937410082 ) ) ;
#9929 = CARTESIAN_POINT ( 'NONE',  ( 12.63842701281683922, 59.55059781766744464, -9.846743663894590881 ) ) ;
#9930 = CARTESIAN_POINT ( 'NONE',  ( 17.96484262340118221, 6.188685344154837509, -7.964842623401177768 ) ) ;
#9931 = CARTESIAN_POINT ( 'NONE',  ( -4.164238869374098151, 16.59541550158063927, -3.795296366450310543 ) ) ;
#9932 = CARTESIAN_POINT ( 'NONE',  ( -4.164238869374099039, 41.80374883491397497, 8.674139862899312516E-16 ) ) ;
#9933 = DIRECTION ( 'NONE',  ( 0.000000000000000000, 1.000000000000000000, 0.000000000000000000 ) ) ;
#9935 = CARTESIAN_POINT ( 'NONE',  ( 1.472469842513823179, 55.59226448433412315, -4.923371831947296329 ) ) ;
#9934 = CARTESIAN_POINT ( 'NONE',  ( 6.507545146407271552, -58.30914921483925895, 2.500000000000000000 ) ) ;
#9936 = CARTESIAN_POINT ( 'NONE',  ( 10.00000000000000178, 34.31368534415484106, 10.88017736071110342 ) ) ;
#9937 = FACE_OUTER_BOUND ( 'NONE', #84895, .T. ) ;
#9938 = CARTESIAN_POINT ( 'NONE',  ( 19.59274024544229675, 95.43182565554037922, -5.128398454507786752 ) ) ;
#9939 = EDGE_CURVE ( 'NONE', #15989, #67813, #18898, .T. ) ;
#9940 = CARTESIAN_POINT ( 'NONE',  ( 12.63842701281683034, 37.46726448433411605, 9.846743663894596210 ) ) ;
#9941 = DIRECTION ( 'NONE',  ( -0.8038568606172123987, 0.000000000000000000, -0.5948227867513479206 ) ) ;
#9942 = CARTESIAN_POINT ( 'NONE',  ( -10.36894250292379205, -8.821251165086028578, -10.36894250292378672 ) ) ;
#9943 = CARTESIAN_POINT ( 'NONE',  ( 14.92337183194729633, 37.67559781766745175, 8.527530157486181039 ) ) ;
#9944 = CARTESIAN_POINT ( 'NONE',  ( 10.00000000000000000, 59.75893115100078745, -9.846743663894594434 ) ) ;
#9945 = STYLED_ITEM ( 'NONE', ( #28279 ), #80618 ) ;
#9946 = ORIENTED_EDGE ( 'NONE', *, *, #67793, .F. ) ;
#9947 = CARTESIAN_POINT ( 'NONE',  ( 22.26659068614895176, 9.720415501580633943, -7.082119434687042414 ) ) ;
#9948 = CARTESIAN_POINT ( 'NONE',  ( -12.50534872682722565, 15.00000000000000000, -7.339363270777700343 ) ) ;
#9949 = CARTESIAN_POINT ( 'NONE',  ( -6.030006457173053391, -39.79017371240020395, -2.499999999999193534 ) ) ;
#9950 = CARTESIAN_POINT ( 'NONE',  ( -4.164238869374098151, 66.59541550158060375, -3.795296366450310543 ) ) ;
#9951 = CARTESIAN_POINT ( 'NONE',  ( 21.09922568453594849, 21.20696800326375353, 6.408140936763242479 ) ) ;
#9952 = CARTESIAN_POINT ( 'NONE',  ( 7.084665262690076126, 67.02201867748817676, -10.88017736071110164 ) ) ;
#9953 = CARTESIAN_POINT ( 'NONE',  ( 4.380000000000001670, 1.019547802438464768, -4.000000000000000000 ) ) ;
#9954 = CARTESIAN_POINT ( 'NONE',  ( 3.969999999999999751, 36.75000000000000000, -4.000000000000000000 ) ) ;
#9955 = LINE ( 'NONE', #47450, #45176 ) ;
#9956 = CARTESIAN_POINT ( 'NONE',  ( 4.559911319644449179, 13.89701867748817321, 9.422509992056141925 ) ) ;
#9957 = CARTESIAN_POINT ( 'NONE',  ( 17.75000000000000355, 73.00000000000001421, -6.250000000000000000 ) ) ;
#9958 = CARTESIAN_POINT ( 'NONE',  ( 0.5774900079438590739, 22.64701867748817321, -5.440088680355550821 ) ) ;
#9959 = CARTESIAN_POINT ( 'NONE',  ( 2.035157376598822676, 37.43868534415484106, -7.964842623401177768 ) ) ;
#9960 = CARTESIAN_POINT ( 'NONE',  ( 10.00000000000000178, 0.3736346699304200492, 12.81628187352647608 ) ) ;
#9962 = CARTESIAN_POINT ( 'NONE',  ( 7.361572987183170547, 52.05059781766745175, 9.846743663894590881 ) ) ;
#9961 = B_SPLINE_CURVE_WITH_KNOTS ( 'NONE', 3,
 ( #76475, #67503, #68983, #30964, #89508, #14014 ),
 .UNSPECIFIED., .F., .F.,
 ( 4, 2, 4 ),
 ( 3.409110551494635847E-05, 0.0004400426677367929142, 0.0008459942299586394564 ),
 .UNSPECIFIED. ) ;
#9963 = CARTESIAN_POINT ( 'NONE',  ( 22.81628187352647785, 61.62363466993041783, 6.195893100308588602E-16 ) ) ;
#9964 = CARTESIAN_POINT ( 'NONE',  ( 1.472469842513823179, 11.42559781766745175, 4.923371831947296329 ) ) ;
#9965 = ORIENTED_EDGE ( 'NONE', *, *, #17637, .T. ) ;
#9966 = CARTESIAN_POINT ( 'NONE',  ( 4.559911319644449179, 28.89701867748817321, 9.422509992056141925 ) ) ;
#9967 = CARTESIAN_POINT ( 'NONE',  ( -2.816281873526473856, 34.33196800326376064, 3.434112377981055619 ) ) ;
#9968 = DIRECTION ( 'NONE',  ( 0.000000000000000000, 0.000000000000000000, 1.000000000000000000 ) ) ;
#9969 = TOROIDAL_SURFACE ( 'NONE', #68997, 14.49999999999999822, 0.5000000000000000000 ) ;
#9970 = EDGE_CURVE ( 'NONE', #85332, #79199, #56389, .T. ) ;
#9971 = CARTESIAN_POINT ( 'NONE',  ( 3.591859063236763294, -1.709698663402913210, -11.09922568453595026 ) ) ;
#9972 = CARTESIAN_POINT ( 'NONE',  ( -0.8801773607110991993, 42.85535201082150536, -2.915334737309923874 ) ) ;
#9973 = CARTESIAN_POINT ( 'NONE',  ( 17.20831665107776587, 9.133931151000787452, -7.208316651077762316 ) ) ;
#9974 = CARTESIAN_POINT ( 'NONE',  ( 19.38216949554541202, 40.99863466993042493, 9.382169495545424454 ) ) ;
#9975 = CARTESIAN_POINT ( 'NONE',  ( 15.44008868035555793, 56.39701867748817676, -9.422509992056140149 ) ) ;
#9976 = CARTESIAN_POINT ( 'NONE',  ( -0.1503990784575328643, 69.92552686551195507, -6.262539305110068177 ) ) ;
#9977 = TOROIDAL_SURFACE ( 'NONE', #56292, 14.49999999999999822, 0.5000000000000000000 ) ;
#9978 = CARTESIAN_POINT ( 'NONE',  ( 0.6178305044545818747, 63.49863466993043204, -9.382169495545419124 ) ) ;
#9979 = ORIENTED_EDGE ( 'NONE', *, *, #11731, .T. ) ;
#9980 = DIRECTION ( 'NONE',  ( -0.000000000000000000, -1.000000000000000000, -0.000000000000000000 ) ) ;
#9981 = CARTESIAN_POINT ( 'NONE',  ( -9.000000000000001776, 80.99999999999994316, 0.000000000000000000 ) ) ;
#9982 = EDGE_CURVE ( 'NONE', #37318, #79695, #37208, .T. ) ;
#9984 = CARTESIAN_POINT ( 'NONE',  ( 22.26659068614894466, 18.88708216824730002, 7.082119434687054849 ) ) ;
#9983 = CARTESIAN_POINT ( 'NONE',  ( 0.6178305044545818747, 43.49863466993042493, -9.382169495545419124 ) ) ;
#9985 = CARTESIAN_POINT ( 'NONE',  ( 0.1532563361054083140, 21.00893115100078745, 1.131784320476157264E-15 ) ) ;
#9986 = CIRCLE ( 'NONE', #91406, 1.000000000000000888 ) ;
#9987 = CARTESIAN_POINT ( 'NONE',  ( 7.084665262690076126, 2.022018677488170990, -10.88017736071110164 ) ) ;
#9988 = CARTESIAN_POINT ( 'NONE',  ( 7.361572987183169658, 19.96726448433411960, -9.846743663894592657 ) ) ;
#9989 = B_SPLINE_CURVE_WITH_KNOTS ( 'NONE', 3,
 ( #34851, #58837, #89344, #30675, #88851, #83699 ),
 .UNSPECIFIED., .F., .F.,
 ( 4, 2, 4 ),
 ( 0.0002800206007755223943, 0.0006862260317143878017, 0.001092431462653253209 ),
 .UNSPECIFIED. ) ;
#9990 = CARTESIAN_POINT ( 'NONE',  ( 10.00000000000000000, 50.55374883491396787, -14.16423886937410082 ) ) ;
#9991 = ORIENTED_EDGE ( 'NONE', *, *, #54745, .F. ) ;
#9992 =( GEOMETRIC_REPRESENTATION_CONTEXT ( 3 ) GLOBAL_UNCERTAINTY_ASSIGNED_CONTEXT ( ( #70115 ) ) GLOBAL_UNIT_ASSIGNED_CONTEXT ( ( #15972, #69959, #46462 ) ) REPRESENTATION_CONTEXT ( 'NONE', 'WORKASPACE' ) );
#9993 = CARTESIAN_POINT ( 'NONE',  ( 12.91533473730992121, 4.522018677488169658, 10.88017736071110164 ) ) ;
#9994 = CARTESIAN_POINT ( 'NONE',  ( 20.88017736071110164, 20.35535201082150891, 2.915334737309930979 ) ) ;
#9995 = CARTESIAN_POINT ( 'NONE',  ( -5.056330833731550456, 15.00000000000000000, -13.58983143750704592 ) ) ;
#9996 = MECHANICAL_DESIGN_GEOMETRIC_PRESENTATION_REPRESENTATION (  '', ( #64270 ), #62636 ) ;
#9997 = EDGE_LOOP ( 'NONE', ( #37064, #42220, #32695, #55711 ) ) ;
#9998 = CARTESIAN_POINT ( 'NONE',  ( 20.88017736071110875, 10.77201867748817143, -2.915334737309920765 ) ) ;
#9999 = CARTESIAN_POINT ( 'NONE',  ( 19.84674366389459621, 53.50893115100078745, 7.409399052514197653E-17 ) ) ;
#10000 = CARTESIAN_POINT ( 'NONE',  ( 13.43411237798105340, 55.58196800326374643, 12.81628187352647963 ) ) ;
#10001 = CARTESIAN_POINT ( 'NONE',  ( 9.779999999999990479, 20.99999999999999645, 0.000000000000000000 ) ) ;
#10003 = CARTESIAN_POINT ( 'NONE',  ( 2.917880565312950480, 15.97041550158063217, -12.26659068614894821 ) ) ;
#10002 = SURFACE_STYLE_USAGE ( .BOTH. , #78488 ) ;
#10004 = CARTESIAN_POINT ( 'NONE',  ( 4.559911319644449179, 27.23035201082150536, -9.422509992056141925 ) ) ;
#10005 = CARTESIAN_POINT ( 'NONE',  ( 15.44008868035555793, 16.39701867748817321, -9.422509992056140149 ) ) ;
#10006 = CARTESIAN_POINT ( 'NONE',  ( 19.84674366389459266, 53.30059781766744464, 2.638427012816836559 ) ) ;
#10007 = CARTESIAN_POINT ( 'NONE',  ( -8.899065713163235358, -15.58770999055384365, -3.750000000000000888 ) ) ;
#10008 = CARTESIAN_POINT ( 'NONE',  ( 2.791683348922240793, 36.63393115100078035, 7.208316651077764092 ) ) ;
#10009 = CARTESIAN_POINT ( 'NONE',  ( -19.19000000000001194, 93.50000000000000000, -10.09898361729590199 ) ) ;
#10010 = VECTOR ( 'NONE', #98976, 1000.000000000000000 ) ;
#10011 = CARTESIAN_POINT ( 'NONE',  ( 0.1532563361054082862, 11.21726448433411605, 2.638427012816831674 ) ) ;
#10012 = CARTESIAN_POINT ( 'NONE',  ( -11.09922568453594316, -40.45969866340291077, 6.408140936763246920 ) ) ;
#10013 = ORIENTED_EDGE ( 'NONE', *, *, #12166, .T. ) ;
#10014 = EDGE_CURVE ( 'NONE', #12471, #67320, #9955, .T. ) ;
#10015 = CARTESIAN_POINT ( 'NONE',  ( 2.791683348922237240, 5.383931151000785675, -7.208316651077763204 ) ) ;
#10016 = CARTESIAN_POINT ( 'NONE',  ( 22.81628187352647785, 1.623634669930420271, 6.195893100308588602E-16 ) ) ;
#10017 = CARTESIAN_POINT ( 'NONE',  ( 4.559911319644449179, 47.23035201082150536, -9.422509992056141925 ) ) ;
#10019 = CARTESIAN_POINT ( 'NONE',  ( 10.00000000000000000, 47.87363466993042493, -12.81628187352647608 ) ) ;
#10018 = CARTESIAN_POINT ( 'NONE',  ( -0.8801773607110991993, 7.855352010821504471, -2.915334737309923874 ) ) ;
#10020 = CARTESIAN_POINT ( 'NONE',  ( -2.266590686148945544, 17.22041550158063572, 7.082119434687048631 ) ) ;
#10021 = ADVANCED_FACE ( 'NONE', ( #33414 ), #15980, .T. ) ;
#10022 = CIRCLE ( 'NONE', #56337, 0.2500000000000002220 ) ;
#10023 = CARTESIAN_POINT ( 'NONE',  ( 21.09922568453594849, 56.20696800326375353, 6.408140936763242479 ) ) ;
#10024 = ORIENTED_EDGE ( 'NONE', *, *, #49376, .F. ) ;
#10025 = CARTESIAN_POINT ( 'NONE',  ( 2.791683348922240793, 61.63393115100079456, 7.208316651077764092 ) ) ;
#10026 = CARTESIAN_POINT ( 'NONE',  ( 4.559911319644449179, 23.89701867748817321, 9.422509992056141925 ) ) ;
#10027 = VERTEX_POINT ( 'NONE', #16970 ) ;
#10028 = CARTESIAN_POINT ( 'NONE',  ( 0.1532563361054082862, 6.217264484334118713, 2.638427012816831674 ) ) ;
#10029 = CARTESIAN_POINT ( 'NONE',  ( 10.93781366033347169, 0.5000000000000004441, -10.26470809774065351 ) ) ;
#10030 = CARTESIAN_POINT ( 'NONE',  ( 14.92337183194729988, 9.342264484334119601, -8.527530157486177487 ) ) ;
#10031 = CARTESIAN_POINT ( 'NONE',  ( 15.44008868035555260, 64.73035201082151957, 9.422509992056143702 ) ) ;
#10032 = LINE ( 'NONE', #32016, #73039 ) ;
#10033 = CARTESIAN_POINT ( 'NONE',  ( 10.00000000000000178, 59.31368534415484106, 10.88017736071110342 ) ) ;
#10034 = CARTESIAN_POINT ( 'NONE',  ( 0.5774900079438607392, 68.48035201082150536, 5.440088680355550821 ) ) ;
#10037 = ORIENTED_EDGE ( 'NONE', *, *, #18120, .F. ) ;
#10036 = AXIS2_PLACEMENT_3D ( 'NONE', #59589, #50619, #43603 ) ;
#10035 = CARTESIAN_POINT ( 'NONE',  ( 19.84674366389459621, 8.508931151000785675, 7.409399052514197653E-17 ) ) ;
#10038 = DIRECTION ( 'NONE',  ( 0.8788171126619711560, 0.000000000000000000, -0.4771587602595978028 ) ) ;
#10039 = CARTESIAN_POINT ( 'NONE',  ( 10.00000000000000000, 49.75893115100078745, -9.846743663894594434 ) ) ;
#10040 = VERTEX_POINT ( 'NONE', #39957 ) ;
#10041 = ORIENTED_EDGE ( 'NONE', *, *, #10407, .T. ) ;
#10042 = DIRECTION ( 'NONE',  ( 0.000000000000000000, 0.000000000000000000, -1.000000000000000000 ) ) ;
#10043 = CARTESIAN_POINT ( 'NONE',  ( -4.164238869374099039, 1.803748834913967647, 8.674139862899312516E-16 ) ) ;
#10044 = CIRCLE ( 'NONE', #96262, 1.500000000000001332 ) ;
#10045 = AXIS2_PLACEMENT_3D ( 'NONE', #49388, #85933, #24943 ) ;
#10046 = CARTESIAN_POINT ( 'NONE',  ( 21.09922568453595559, 62.04030133659709634, -6.408140936763230044 ) ) ;
#10047 = AXIS2_PLACEMENT_3D ( 'NONE', #6360, #67865, #22370 ) ;
#10048 = CARTESIAN_POINT ( 'NONE',  ( 6.204703633549690345, 22.84541550158062861, 14.16423886937410082 ) ) ;
#10049 = CARTESIAN_POINT ( 'NONE',  ( -0.3689425029237881626, 2.428748834913967869, 10.36894250292379027 ) ) ;
#10050 = CARTESIAN_POINT ( 'NONE',  ( 12.91533473730993009, 21.60535201082150536, -10.88017736071109987 ) ) ;
#10051 = ORIENTED_EDGE ( 'NONE', *, *, #59021, .F. ) ;
#10053 = CIRCLE ( 'NONE', #22832, 6.599999999999995204 ) ;
#10052 = CARTESIAN_POINT ( 'NONE',  ( 12.63842701281683922, 4.550597817667451750, -9.846743663894590881 ) ) ;
#10054 = CARTESIAN_POINT ( 'NONE',  ( 0.1532563361054083140, 16.00893115100078390, 1.131784320476157264E-15 ) ) ;
#10055 = CARTESIAN_POINT ( 'NONE',  ( 0.6178305044545818747, 28.49863466993041783, -9.382169495545419124 ) ) ;
#10056 = CARTESIAN_POINT ( 'NONE',  ( 19.84674366389459621, 43.50893115100078745, 7.409399052514197653E-17 ) ) ;
#10057 = CARTESIAN_POINT ( 'NONE',  ( 0.000000000000000000, 15.00000000000000000, 0.000000000000000000 ) ) ;
#10058 = EDGE_CURVE ( 'NONE', #23012, #13614, #66522, .T. ) ;
#10059 = CARTESIAN_POINT ( 'NONE',  ( -2.816281873526473856, 24.12363466993042138, 9.499525473075851096E-16 ) ) ;
#10060 = CARTESIAN_POINT ( 'NONE',  ( -6.715867195167276371, 15.00000000000000000, -12.85095824508335838 ) ) ;
#10061 = CARTESIAN_POINT ( 'NONE',  ( 12.63842701281683034, 22.46726448433411605, 9.846743663894596210 ) ) ;
#10062 = CARTESIAN_POINT ( 'NONE',  ( 24.16423886937409904, 9.095415501580633943, 3.795296366450317205 ) ) ;
#10063 = VERTEX_POINT ( 'NONE', #55950 ) ;
#10064 = ADVANCED_FACE ( 'NONE', ( #86449 ), #2964, .T. ) ;
#10065 = CARTESIAN_POINT ( 'NONE',  ( 19.42250999205614548, 30.98035201082150536, -5.440088680355545492 ) ) ;
#10066 = CARTESIAN_POINT ( 'NONE',  ( 6.204703633549690345, 37.84541550158063927, 14.16423886937410082 ) ) ;
#10067 = CARTESIAN_POINT ( 'NONE',  ( 19.84674366389459621, 53.50893115100078745, 7.409399052514197653E-17 ) ) ;
#10068 = CARTESIAN_POINT ( 'NONE',  ( 0.1532563361054083140, 16.00893115100078390, 1.131784320476157264E-15 ) ) ;
#10070 = DIRECTION ( 'NONE',  ( -0.1478094111296113511, 0.000000000000000000, 0.9890158633619168249 ) ) ;
#10069 = CARTESIAN_POINT ( 'NONE',  ( 16.40814093676324603, 47.45696800326375353, -11.09922568453594671 ) ) ;
#10071 = CARTESIAN_POINT ( 'NONE',  ( -0.8801773607111008646, 33.27201867748817676, 2.915334737309923430 ) ) ;
#10072 = LINE ( 'NONE', #64029, #75773 ) ;
#10073 = CARTESIAN_POINT ( 'NONE',  ( 10.00000000000000000, 22.87363466993042138, -12.81628187352647608 ) ) ;
#10074 = CARTESIAN_POINT ( 'NONE',  ( 17.20831665107776587, 39.13393115100079456, -7.208316651077762316 ) ) ;
#10075 = CARTESIAN_POINT ( 'NONE',  ( 5.440088680355556150, -0.2696479891784869798, 9.422509992056138373 ) ) ;
#10076 = CARTESIAN_POINT ( 'NONE',  ( 19.38216949554541557, 52.24863466993041072, -9.382169495545420901 ) ) ;
#10077 = CARTESIAN_POINT ( 'NONE',  ( 14.94699059465100888, 0.5000000000000004441, 1.259949270174915981 ) ) ;
#10079 = CARTESIAN_POINT ( 'NONE',  ( 17.85999999999998522, 22.49999999999995026, 9.500000000000000000 ) ) ;
#10078 = CARTESIAN_POINT ( 'NONE',  ( 15.44008868035555793, 56.39701867748817676, -9.422509992056140149 ) ) ;
#10080 = VECTOR ( 'NONE', #35640, 1000.000000000000000 ) ;
#10081 = DIRECTION ( 'NONE',  ( 0.000000000000000000, -0.000000000000000000, 1.000000000000000000 ) ) ;
#10082 = DIRECTION ( 'NONE',  ( -0.000000000000000000, -0.000000000000000000, -1.000000000000000000 ) ) ;
#10083 = CARTESIAN_POINT ( 'NONE',  ( 0.5774900079438607392, 58.48035201082151247, 5.440088680355550821 ) ) ;
#10085 = CARTESIAN_POINT ( 'NONE',  ( 20.88017736071110875, 60.77201867748817676, -2.915334737309920765 ) ) ;
#10084 = AXIS2_PLACEMENT_3D ( 'NONE', #52202, #15701, #45687 ) ;
#10086 = CARTESIAN_POINT ( 'NONE',  ( -10.00000000000007105, 92.00000000000000000, -9.500000000000000000 ) ) ;
#10088 = ADVANCED_FACE ( 'NONE', ( #2478 ), #32445, .T. ) ;
#10087 = CARTESIAN_POINT ( 'NONE',  ( 4.949168087017304707, 13.09799106954466019, -10.91454864610492059 ) ) ;
#10089 = CARTESIAN_POINT ( 'NONE',  ( 0.5774900079438590739, 7.647018677488171434, -5.440088680355550821 ) ) ;
#10090 = CARTESIAN_POINT ( 'NONE',  ( 0.6178305044545818747, -1.501365330069579951, -9.382169495545419124 ) ) ;
#10092 = CARTESIAN_POINT ( 'NONE',  ( -6.030735108402915934, -39.80307983730808274, -3.749999999999999556 ) ) ;
#10091 = CARTESIAN_POINT ( 'NONE',  ( 2.035157376598822676, 22.43868534415483396, -7.964842623401177768 ) ) ;
#10093 = FILL_AREA_STYLE_COLOUR ( '', #28866 ) ;
#10094 = CARTESIAN_POINT ( 'NONE',  ( -1.099225684535947600, 28.70696800326375353, -6.408140936763238038 ) ) ;
#10095 = VERTEX_POINT ( 'NONE', #31453 ) ;
#10096 = CARTESIAN_POINT ( 'NONE',  ( 12.91533473730993009, 46.60535201082150536, -10.88017736071109987 ) ) ;
#10097 = EDGE_CURVE ( 'NONE', #18033, #83367, #80605, .T. ) ;
#10098 = CARTESIAN_POINT ( 'NONE',  ( 12.63842701281683034, 42.46726448433412315, 9.846743663894596210 ) ) ;
#10100 = CARTESIAN_POINT ( 'NONE',  ( 8.879999999999991900, 27.04366094290857347, 2.900000000000000355 ) ) ;
#10099 = CARTESIAN_POINT ( 'NONE',  ( 16.40814093676323893, 5.790301336597087456, 11.09922568453595026 ) ) ;
#10101 = CARTESIAN_POINT ( 'NONE',  ( 15.44008868035555793, 21.39701867748817321, -9.422509992056140149 ) ) ;
#10102 = CARTESIAN_POINT ( 'NONE',  ( 20.88017736071110164, 35.35535201082150536, 2.915334737309930979 ) ) ;
#10103 = CARTESIAN_POINT ( 'NONE',  ( -2.266590686148945544, 52.22041550158064638, 7.082119434687048631 ) ) ;
#10104 = CARTESIAN_POINT ( 'NONE',  ( 1.472469842513823179, 45.59226448433412315, -4.923371831947296329 ) ) ;
#10105 = CARTESIAN_POINT ( 'NONE',  ( -0.8801773607111008646, 63.27201867748817676, 2.915334737309923430 ) ) ;
#10106 = DIRECTION ( 'NONE',  ( -0.04361938736532633420, 0.000000000000000000, -0.9990482215818581313 ) ) ;
#10107 = CARTESIAN_POINT ( 'NONE',  ( 10.00000000000000178, 13.05374883491396787, 14.16423886937410082 ) ) ;
#10108 = CARTESIAN_POINT ( 'NONE',  ( -9.383624259804166812, 0.2301501999355076711, 11.62625599701874179 ) ) ;
#10109 = CARTESIAN_POINT ( 'NONE',  ( 8.630000000000000782, 1.019547802438458550, -4.000000000000000000 ) ) ;
#10110 = VERTEX_POINT ( 'NONE', #48434 ) ;
#10111 = CARTESIAN_POINT ( 'NONE',  ( -2.266590686148945544, 52.22041550158064638, 7.082119434687048631 ) ) ;
#10112 = CARTESIAN_POINT ( 'NONE',  ( 2.917880565312948704, 42.63708216824729647, 12.26659068614894643 ) ) ;
#10113 = CARTESIAN_POINT ( 'NONE',  ( 0.1532563361054083140, 21.00893115100078745, 1.131784320476157264E-15 ) ) ;
#10114 = CARTESIAN_POINT ( 'NONE',  ( 3.591859063236761518, 19.95696800326375353, 11.09922568453594849 ) ) ;
#10115 = CARTESIAN_POINT ( 'NONE',  ( 7.361572987183170547, 57.05059781766744464, 9.846743663894590881 ) ) ;
#10116 = DIRECTION ( 'NONE',  ( 0.000000000000000000, -1.000000000000000000, 0.000000000000000000 ) ) ;
#10118 = CARTESIAN_POINT ( 'NONE',  ( 6.565887622018943937, 28.08196800326375353, -12.81628187352647608 ) ) ;
#10117 = CARTESIAN_POINT ( 'NONE',  ( 2.035157376598824452, 53.68868534415484817, 7.964842623401179544 ) ) ;
#10119 = CARTESIAN_POINT ( 'NONE',  ( 24.16423886937410614, 39.30374883491396787, 8.672049930838204340E-16 ) ) ;
#10120 = CARTESIAN_POINT ( 'NONE',  ( 20.88017736071110164, 30.35535201082151247, 2.915334737309930979 ) ) ;
#10121 = TOROIDAL_SURFACE ( 'NONE', #27648, 14.49999999999999822, 0.5000000000000000000 ) ;
#10122 = FACE_OUTER_BOUND ( 'NONE', #4375, .T. ) ;
#10123 = CARTESIAN_POINT ( 'NONE',  ( 12.91533473730993009, 66.60535201082150536, -10.88017736071109987 ) ) ;
#10124 = COLOUR_RGB ( '', 0.09019608, 0.27058824, 0.51372549) ;
#10125 = CARTESIAN_POINT ( 'NONE',  ( -9.846743663894590881, -8.782735515665878623, 2.638427012816840111 ) ) ;
#10126 = CARTESIAN_POINT ( 'NONE',  ( 1.472469842513823179, 6.425597817667451750, 4.923371831947296329 ) ) ;
#10127 = ORIENTED_EDGE ( 'NONE', *, *, #79404, .T. ) ;
#10128 = DIRECTION ( 'NONE',  ( -0.9170600743851211600, 0.000000000000000000, -0.3987490689252528031 ) ) ;
#10129 = AXIS2_PLACEMENT_3D ( 'NONE', #8314, #67329, #98355 ) ;
#10130 = ORIENTED_EDGE ( 'NONE', *, *, #59434, .F. ) ;
#10131 = DIRECTION ( 'NONE',  ( -0.000000000000000000, -0.000000000000000000, 1.000000000000000000 ) ) ;
#10132 = EDGE_LOOP ( 'NONE', ( #62322, #75282, #36985, #87582 ) ) ;
#10133 = CARTESIAN_POINT ( 'NONE',  ( -4.164238869374098151, 6.595415501580634832, -3.795296366450310543 ) ) ;
#10135 = CARTESIAN_POINT ( 'NONE',  ( 2.035157376598822676, 12.43868534415483751, -7.964842623401177768 ) ) ;
#10134 = CARTESIAN_POINT ( 'NONE',  ( 0.5774900079438590739, 7.647018677488171434, -5.440088680355550821 ) ) ;
#10137 = CARTESIAN_POINT ( 'NONE',  ( 13.43411237798106583, 2.665301336597086568, -12.81628187352647252 ) ) ;
#10136 = CARTESIAN_POINT ( 'NONE',  ( 19.84674366389459266, 38.30059781766745175, 2.638427012816836559 ) ) ;
#10138 = CARTESIAN_POINT ( 'NONE',  ( -13.55157833323626271, 14.76930270348881535, -6.292279346205571500 ) ) ;
#10139 = DIRECTION ( 'NONE',  ( 1.000000000000000000, 0.000000000000000000, 0.000000000000000000 ) ) ;
#10140 = ADVANCED_FACE ( 'NONE', ( #46953 ), #85957, .T. ) ;
#10141 = CARTESIAN_POINT ( 'NONE',  ( 22.81628187352647785, 16.62363466993042138, 6.195893100308588602E-16 ) ) ;
#10142 = ORIENTED_EDGE ( 'NONE', *, *, #76054, .F. ) ;
#10143 = CARTESIAN_POINT ( 'NONE',  ( -2.266590686148945544, 52.22041550158064638, 7.082119434687048631 ) ) ;
#10144 = ORIENTED_EDGE ( 'NONE', *, *, #38845, .T. ) ;
#10145 = CARTESIAN_POINT ( 'NONE',  ( 6.204703633549690345, 52.84541550158062506, 14.16423886937410082 ) ) ;
#10146 = ORIENTED_EDGE ( 'NONE', *, *, #63448, .F. ) ;
#10147 = CARTESIAN_POINT ( 'NONE',  ( 12.91533473730992121, 29.52201867748817321, 10.88017736071110164 ) ) ;
#10148 = CARTESIAN_POINT ( 'NONE',  ( 2.035157376598824452, 38.68868534415483396, 7.964842623401179544 ) ) ;
#10149 = CARTESIAN_POINT ( 'NONE',  ( 19.42250999205614548, 35.98035201082151247, -5.440088680355545492 ) ) ;
#10150 = DIRECTION ( 'NONE',  ( 0.8320502943378436100, -0.5547001962252291474, 0.000000000000000000 ) ) ;
#10151 = CARTESIAN_POINT ( 'NONE',  ( 7.084665262690076126, 27.02201867748817676, -10.88017736071110164 ) ) ;
#10152 =( GEOMETRIC_REPRESENTATION_CONTEXT ( 3 ) GLOBAL_UNCERTAINTY_ASSIGNED_CONTEXT ( ( #53115 ) ) GLOBAL_UNIT_ASSIGNED_CONTEXT ( ( #82735, #62186, #2219 ) ) REPRESENTATION_CONTEXT ( 'NONE', 'WORKASPACE' ) );
#10154 = ORIENTED_EDGE ( 'NONE', *, *, #54141, .T. ) ;
#10153 = CARTESIAN_POINT ( 'NONE',  ( -11.22915323889586858, -0.03417435944610275333, 8.773176023390528044 ) ) ;
#10155 = CARTESIAN_POINT ( 'NONE',  ( 5.076628168052704559, 10.17559781766745175, -8.527530157486179263 ) ) ;
#10156 = CARTESIAN_POINT ( 'NONE',  ( -3.887834249412648546, -8.254296980873792933, 2.750000000000000888 ) ) ;
#10157 = ORIENTED_EDGE ( 'NONE', *, *, #43796, .T. ) ;
#10158 = CARTESIAN_POINT ( 'NONE',  ( 10.00000000000000000, 49.75893115100078745, -9.846743663894594434 ) ) ;
#10159 = DIRECTION ( 'NONE',  ( -0.9999619230641711987, 0.000000000000000000, -0.008726535498381204903 ) ) ;
#10160 = CARTESIAN_POINT ( 'NONE',  ( 13.43411237798105340, 45.58196800326374643, 12.81628187352647963 ) ) ;
#10161 = LINE ( 'NONE', #92658, #10758 ) ;
#10162 = CARTESIAN_POINT ( 'NONE',  ( -1.847340224724643987, 0.04922511925147186884, -14.63671528203495065 ) ) ;
#10163 = DIRECTION ( 'NONE',  ( 0.000000000000000000, 1.000000000000000000, -0.000000000000000000 ) ) ;
#10164 = CARTESIAN_POINT ( 'NONE',  ( 14.92337183194729633, 57.67559781766745886, 8.527530157486181039 ) ) ;
#10165 = CARTESIAN_POINT ( 'NONE',  ( -2.266590686148945544, 42.22041550158063217, 7.082119434687048631 ) ) ;
#10166 = LINE ( 'NONE', #4638, #35512 ) ;
#10167 = B_SPLINE_CURVE_WITH_KNOTS ( 'NONE', 3,
 ( #76310, #6830, #29810, #38814, #69307, #8794, #60319, #829, #37836, #14844 ),
 .UNSPECIFIED., .F., .F.,
 ( 4, 3, 3, 4 ),
 ( 0.000000000000000000, 0.0006253016069561017883, 0.001250604074564958586, 0.002501455912506553476 ),
 .UNSPECIFIED. ) ;
#10168 = ORIENTED_EDGE ( 'NONE', *, *, #94472, .T. ) ;
#10169 = CARTESIAN_POINT ( 'NONE',  ( -11.49638213510170104, 0.04922511925147123046, -9.245501498402102669 ) ) ;
#10170 = CARTESIAN_POINT ( 'NONE',  ( 0.1532563361054083140, 16.00893115100078390, 1.131784320476157264E-15 ) ) ;
#10171 = CARTESIAN_POINT ( 'NONE',  ( 19.38216949554541202, 60.99863466993042493, 9.382169495545424454 ) ) ;
#10172 = CARTESIAN_POINT ( 'NONE',  ( 18.52753015748618282, 58.92559781766745886, -4.923371831947291888 ) ) ;
#10173 = CARTESIAN_POINT ( 'NONE',  ( 15.44008868035555793, 61.39701867748817676, -9.422509992056140149 ) ) ;
#10174 = CARTESIAN_POINT ( 'NONE',  ( 12.63842701281683034, 42.46726448433412315, 9.846743663894596210 ) ) ;
#10175 = CARTESIAN_POINT ( 'NONE',  ( 3.469446951953614189E-15, 8.912123368507815613, 11.92686044187656513 ) ) ;
#10176 = B_SPLINE_CURVE_WITH_KNOTS ( 'NONE', 3,
 ( #61691, #54196, #6248, #36752, #21757, #9693 ),
 .UNSPECIFIED., .F., .F.,
 ( 4, 2, 4 ),
 ( 3.409110551496051408E-05, 0.0004400426677367857043, 0.0008459942299586108334 ),
 .UNSPECIFIED. ) ;
#10177 = VECTOR ( 'NONE', #10229, 1000.000000000000114 ) ;
#10178 = EDGE_CURVE ( 'NONE', #59059, #43266, #39477, .T. ) ;
#10179 = EDGE_CURVE ( 'NONE', #61376, #30551, #54941, .T. ) ;
#10180 = ORIENTED_EDGE ( 'NONE', *, *, #94043, .F. ) ;
#10181 = CARTESIAN_POINT ( 'NONE',  ( 20.36894250292379738, 64.92874883491397497, -10.36894250292379027 ) ) ;
#10182 = CARTESIAN_POINT ( 'NONE',  ( -45.94000000000001194, 100.9999999999999858, 9.500000000000000000 ) ) ;
#10183 = CARTESIAN_POINT ( 'NONE',  ( 0.5774900079438590739, 47.64701867748817676, -5.440088680355550821 ) ) ;
#10185 = CARTESIAN_POINT ( 'NONE',  ( 20.88017736071110875, 65.77201867748817676, -2.915334737309920765 ) ) ;
#10184 = CARTESIAN_POINT ( 'NONE',  ( 22.81628187352647785, 11.62363466993042138, 6.195893100308588602E-16 ) ) ;
#10186 = CARTESIAN_POINT ( 'NONE',  ( -0.1503990784575277573, 63.10158574516643171, 6.262539305110076171 ) ) ;
#10187 = VECTOR ( 'NONE', #76500, 1000.000000000000114 ) ;
#10188 = LINE ( 'NONE', #25205, #74699 ) ;
#10189 = DIRECTION ( 'NONE',  ( 0.9170600743851183845, 0.000000000000000000, 0.3987490689252593534 ) ) ;
#10190 = CARTESIAN_POINT ( 'NONE',  ( -13.96521320569128299, 14.95077488074852923, 4.755935267939069178 ) ) ;
#10191 = CARTESIAN_POINT ( 'NONE',  ( 19.84674366389459266, 53.30059781766744464, 2.638427012816836559 ) ) ;
#10192 = CARTESIAN_POINT ( 'NONE',  ( 5.440088680355549045, -33.60298132251182324, -9.422509992056141925 ) ) ;
#10193 = CARTESIAN_POINT ( 'NONE',  ( 0.6178305044545838731, 9.748634669930416052, 9.382169495545420901 ) ) ;
#10195 = CARTESIAN_POINT ( 'NONE',  ( -14.03351048042399007, -0.03417435944610275333, 2.474486531753619989 ) ) ;
#10194 = CARTESIAN_POINT ( 'NONE',  ( 4.559911319644449179, 17.23035201082150536, -9.422509992056141925 ) ) ;
#10196 = DIRECTION ( 'NONE',  ( -1.000000000000000000, 0.000000000000000000, 0.000000000000000000 ) ) ;
#10197 = CARTESIAN_POINT ( 'NONE',  ( 6.204703633549690345, 35.76208216824729647, -14.16423886937410259 ) ) ;
#10198 = CARTESIAN_POINT ( 'NONE',  ( 20.36894250292379382, 28.67874883491396787, 10.36894250292379205 ) ) ;
#10199 = CARTESIAN_POINT ( 'NONE',  ( -4.164238869374099927, 67.01208216824728936, 3.795296366450308767 ) ) ;
#10200 = CARTESIAN_POINT ( 'NONE',  ( 10.00000000000000178, 32.25893115100078745, 9.846743663894594434 ) ) ;
#10201 = CARTESIAN_POINT ( 'NONE',  ( 16.40814093676324603, 32.45696800326375353, -11.09922568453594671 ) ) ;
#10202 = CARTESIAN_POINT ( 'NONE',  ( 12.91533473730993009, 16.60535201082150891, -10.88017736071109987 ) ) ;
#10203 = ORIENTED_EDGE ( 'NONE', *, *, #22207, .F. ) ;
#10204 = CARTESIAN_POINT ( 'NONE',  ( 2.791683348922240793, 41.63393115100078745, 7.208316651077764092 ) ) ;
#10205 = CARTESIAN_POINT ( 'NONE',  ( 4.559911319644449179, 47.23035201082150536, -9.422509992056141925 ) ) ;
#10206 = CARTESIAN_POINT ( 'NONE',  ( 1.472469842513823179, 66.42559781766745175, 4.923371831947296329 ) ) ;
#10208 = CARTESIAN_POINT ( 'NONE',  ( 2.603489959281613420, 45.43575266056827644, -6.500000000000031086 ) ) ;
#10207 = CARTESIAN_POINT ( 'NONE',  ( 10.00000000000000178, 18.05374883491396787, 14.16423886937410082 ) ) ;
#10209 = CARTESIAN_POINT ( 'NONE',  ( 18.28836319691945889, 34.34492782695770785, 6.500000000000000888 ) ) ;
#10210 = UNCERTAINTY_MEASURE_WITH_UNIT (LENGTH_MEASURE( 1.000000000000000082E-05 ), #67804, 'distance_accuracy_value', 'NONE');
#10211 = CARTESIAN_POINT ( 'NONE',  ( 7.361572987183169658, 29.96726448433411960, -9.846743663894592657 ) ) ;
#10212 = CARTESIAN_POINT ( 'NONE',  ( 3.591859063236763294, 53.29030133659708923, -11.09922568453595026 ) ) ;
#10213 = CARTESIAN_POINT ( 'NONE',  ( 17.20831665107776587, 57.88393115100078745, 7.208316651077764980 ) ) ;
#10214 = VERTEX_POINT ( 'NONE', #35890 ) ;
#10215 = EDGE_CURVE ( 'NONE', #87579, #85555, #65889, .T. ) ;
#10216 = DIRECTION ( 'NONE',  ( -0.3826834323650877279, 0.000000000000000000, -0.9238795325112876267 ) ) ;
#10217 = CARTESIAN_POINT ( 'NONE',  ( -46.50634649544846866, 102.7699257839083486, -6.812960513223167425 ) ) ;
#10218 = CARTESIAN_POINT ( 'NONE',  ( 10.00000000000000178, 4.313685344154837509, 10.88017736071110342 ) ) ;
#10219 = CARTESIAN_POINT ( 'NONE',  ( 12.91533473730992121, 59.52201867748816966, 10.88017736071110164 ) ) ;
#10220 = CARTESIAN_POINT ( 'NONE',  ( 24.16423886937409904, 14.09541550158063217, 3.795296366450317205 ) ) ;
#10221 = CARTESIAN_POINT ( 'NONE',  ( 19.84674366389459621, 3.508931151000785231, 7.409399052514197653E-17 ) ) ;
#10222 = CARTESIAN_POINT ( 'NONE',  ( 17.20831665107776587, 52.88393115100078035, 7.208316651077764980 ) ) ;
#10223 = CARTESIAN_POINT ( 'NONE',  ( 17.96484262340118221, 21.18868534415483396, -7.964842623401177768 ) ) ;
#10224 = CARTESIAN_POINT ( 'NONE',  ( 13.82671409943296226, -0.03417435944610275333, -3.447387012295225261 ) ) ;
#10225 = CARTESIAN_POINT ( 'NONE',  ( 0.000000000000000000, 0.5000000000000004441, 0.000000000000000000 ) ) ;
#10226 = FILL_AREA_STYLE ('',( #79697 ) ) ;
#10227 = VERTEX_POINT ( 'NONE', #66385 ) ;
#10228 = ORIENTED_EDGE ( 'NONE', *, *, #15758, .F. ) ;
#10229 = DIRECTION ( 'NONE',  ( -0.5075383629606967650, 0.000000000000000000, -0.8616291604415300398 ) ) ;
#10230 = CARTESIAN_POINT ( 'NONE',  ( 24.16423886937409904, 14.09541550158063217, 3.795296366450317205 ) ) ;
#10231 = CARTESIAN_POINT ( 'NONE',  ( -4.164238869374099039, 41.80374883491397497, 8.674139862899312516E-16 ) ) ;
#10232 = CARTESIAN_POINT ( 'NONE',  ( 12.63842701281683922, 54.55059781766745175, -9.846743663894590881 ) ) ;
#10233 = CARTESIAN_POINT ( 'NONE',  ( 18.52753015748618282, 23.92559781766745530, -4.923371831947291888 ) ) ;
#10234 = CARTESIAN_POINT ( 'NONE',  ( 2.962741594152983993, 15.00000000000000000, 13.93860331045674883 ) ) ;
#10236 = CARTESIAN_POINT ( 'NONE',  ( 18.52753015748618282, 58.92559781766745886, -4.923371831947291888 ) ) ;
#10235 = CARTESIAN_POINT ( 'NONE',  ( 2.035157376598824452, 18.68868534415484106, 7.964842623401179544 ) ) ;
#10237 = DIRECTION ( 'NONE',  ( 0.000000000000000000, 0.000000000000000000, 1.000000000000000000 ) ) ;
#10238 = CARTESIAN_POINT ( 'NONE',  ( 13.79529636645031943, 35.34541550158063927, -14.16423886937409904 ) ) ;
#10239 = CARTESIAN_POINT ( 'NONE',  ( 17.96484262340118221, 6.188685344154837509, -7.964842623401177768 ) ) ;
#10240 = PLANE ( 'NONE',  #94503 ) ;
#10241 = CARTESIAN_POINT ( 'NONE',  ( 6.284583270191198778, -88.40194713205143273, 3.750000000000000000 ) ) ;
#10242 = CARTESIAN_POINT ( 'NONE',  ( 15.44008868035555260, 59.73035201082151247, 9.422509992056143702 ) ) ;
#10243 = CARTESIAN_POINT ( 'NONE',  ( 18.52753015748617571, 13.09226448433411960, 4.923371831947298993 ) ) ;
#10244 = DIRECTION ( 'NONE',  ( 0.9961946980917453232, -0.08715574274766037244, 0.000000000000000000 ) ) ;
#10245 = EDGE_LOOP ( 'NONE', ( #5632, #31028 ) ) ;
#10246 = CARTESIAN_POINT ( 'NONE',  ( -1.114591949024829054, 4.106534489568945963E-16, -14.45709807627966015 ) ) ;
#10247 = ORIENTED_EDGE ( 'NONE', *, *, #29623, .F. ) ;
#10248 = CARTESIAN_POINT ( 'NONE',  ( 17.20831665107776587, 19.13393115100078035, -7.208316651077762316 ) ) ;
#10249 = ORIENTED_EDGE ( 'NONE', *, *, #3741, .T. ) ;
#10250 = CARTESIAN_POINT ( 'NONE',  ( 17.08211943468705130, 33.47041550158063927, 12.26659068614894998 ) ) ;
#10251 = CARTESIAN_POINT ( 'NONE',  ( 2.791683348922237240, 40.38393115100078035, -7.208316651077763204 ) ) ;
#10252 = CARTESIAN_POINT ( 'NONE',  ( 19.42250999205614193, 45.14701867748817676, 5.440088680355555262 ) ) ;
#10253 =( NAMED_UNIT ( * ) PLANE_ANGLE_UNIT ( ) SI_UNIT ( $, .RADIAN. ) );
#10254 = ORIENTED_EDGE ( 'NONE', *, *, #85921, .T. ) ;
#10255 = CARTESIAN_POINT ( 'NONE',  ( 0.5774900079438590739, 37.64701867748817676, -5.440088680355550821 ) ) ;
#10256 = LINE ( 'NONE', #807, #73938 ) ;
#10257 = VECTOR ( 'NONE', #72982, 1000.000000000000114 ) ;
#10258 = CARTESIAN_POINT ( 'NONE',  ( -6.408140936763246032, -11.70969866340290721, -11.09922568453594316 ) ) ;
#10259 = ORIENTED_EDGE ( 'NONE', *, *, #38991, .F. ) ;
#10260 = CARTESIAN_POINT ( 'NONE',  ( 6.204703633549690345, 2.845415501580634388, 14.16423886937410082 ) ) ;
#10261 = ORIENTED_EDGE ( 'NONE', *, *, #42403, .T. ) ;
#10262 = VECTOR ( 'NONE', #39214, 1000.000000000000000 ) ;
#10263 = ORIENTED_EDGE ( 'NONE', *, *, #71711, .F. ) ;
#10264 = CARTESIAN_POINT ( 'NONE',  ( -2.816281873526473856, 34.12363466993042493, 9.499525473075851096E-16 ) ) ;
#10265 = CARTESIAN_POINT ( 'NONE',  ( 7.361572987183169658, 29.96726448433411960, -9.846743663894592657 ) ) ;
#10266 = CARTESIAN_POINT ( 'NONE',  ( 14.88232117145531141, 0.5000000000000004441, -1.875237731503139438 ) ) ;
#10267 = CARTESIAN_POINT ( 'NONE',  ( 13.43411237798105340, 45.58196800326374643, 12.81628187352647963 ) ) ;
#10268 = CARTESIAN_POINT ( 'NONE',  ( 12.63842701281683034, 32.46726448433412315, 9.846743663894596210 ) ) ;
#10269 = ADVANCED_FACE ( 'NONE', ( #64890 ), #4434, .T. ) ;
#10270 = CARTESIAN_POINT ( 'NONE',  ( 7.084665262690076126, 57.02201867748817676, -10.88017736071110164 ) ) ;
#10271 = CARTESIAN_POINT ( 'NONE',  ( 1.114591949024928752, 4.429576435485488210E-16, 14.45709807627965304 ) ) ;
#10272 = CARTESIAN_POINT ( 'NONE',  ( 8.629999999999995453, 43.00000000000000000, -6.500000000000000888 ) ) ;
#10273 = CARTESIAN_POINT ( 'NONE',  ( 9.282040431732605512, 2.405573570202212963E-16, 11.30407325590345025 ) ) ;
#10274 = DIRECTION ( 'NONE',  ( 0.000000000000000000, 1.000000000000000000, 0.000000000000000000 ) ) ;
#10275 = CARTESIAN_POINT ( 'NONE',  ( 1.472469842513823179, 0.5922644843341181575, -4.923371831947296329 ) ) ;
#10276 = CARTESIAN_POINT ( 'NONE',  ( 0.6178305044545838731, 14.74863466993041783, 9.382169495545420901 ) ) ;
#10277 = CARTESIAN_POINT ( 'NONE',  ( -6.715867195167276371, 4.396228481599465503E-16, -12.85095824508335838 ) ) ;
#10278 = CARTESIAN_POINT ( 'NONE',  ( 5.076628168052704559, 50.17559781766745886, -8.527530157486179263 ) ) ;
#10279 = DIRECTION ( 'NONE',  ( 1.000000000000000000, 0.000000000000000000, 0.000000000000000000 ) ) ;
#10280 = CARTESIAN_POINT ( 'NONE',  ( 13.79529636645031943, 10.34541550158063394, -14.16423886937409904 ) ) ;
#10281 = CARTESIAN_POINT ( 'NONE',  ( 18.52753015748617571, 23.09226448433411960, 4.923371831947298993 ) ) ;
#10282 = CARTESIAN_POINT ( 'NONE',  ( 0.6178305044545818747, 33.49863466993042493, -9.382169495545419124 ) ) ;
#10284 = CARTESIAN_POINT ( 'NONE',  ( 0.5774900079438607392, 23.48035201082150536, 5.440088680355550821 ) ) ;
#10283 = DIRECTION ( 'NONE',  ( 0.8141155183563185682, 0.000000000000000000, -0.5807029557109406603 ) ) ;
#10285 = CARTESIAN_POINT ( 'NONE',  ( 0.5774900079438590739, 47.64701867748817676, -5.440088680355550821 ) ) ;
#10286 = EDGE_CURVE ( 'NONE', #49769, #36460, #10932, .T. ) ;
#10287 = CARTESIAN_POINT ( 'NONE',  ( -1.099225684535947600, 3.706968003263753531, -6.408140936763238038 ) ) ;
#10288 = CARTESIAN_POINT ( 'NONE',  ( 13.61802159414987479, 14.99999999999808509, -5.334603887713429415 ) ) ;
#10289 = CIRCLE ( 'NONE', #94926, 15.00000000000000000 ) ;
#10290 = CARTESIAN_POINT ( 'NONE',  ( 0.1532563361054083140, 21.00893115100078745, 1.131784320476157264E-15 ) ) ;
#10291 = CARTESIAN_POINT ( 'NONE',  ( -0.8801773607110991993, 32.85535201082151247, -2.915334737309923874 ) ) ;
#10292 = CARTESIAN_POINT ( 'NONE',  ( 22.81628187352647785, 36.41530133659707502, 3.434112377981063169 ) ) ;
#10293 = CARTESIAN_POINT ( 'NONE',  ( 17.20831665107776587, 22.88393115100078745, 7.208316651077764980 ) ) ;
#10294 = CARTESIAN_POINT ( 'NONE',  ( -9.247107438774047949, 88.00886336720424197, 5.024692236534948009 ) ) ;
#10295 = EDGE_CURVE ( 'NONE', #70888, #57109, #96419, .T. ) ;
#10296 = CARTESIAN_POINT ( 'NONE',  ( -0.8801773607111008646, 23.27201867748817676, 2.915334737309923430 ) ) ;
#10297 = EDGE_CURVE ( 'NONE', #14567, #83178, #49864, .T. ) ;
#10298 = ORIENTED_EDGE ( 'NONE', *, *, #48882, .T. ) ;
#10299 = CARTESIAN_POINT ( 'NONE',  ( 10.00000000000000000, 56.81368534415484106, -10.88017736071110342 ) ) ;
#10300 = PRESENTATION_STYLE_ASSIGNMENT (( #86788 ) ) ;
#10302 = CARTESIAN_POINT ( 'NONE',  ( -0.8801773607111008646, 23.27201867748817676, 2.915334737309923430 ) ) ;
#10301 = CARTESIAN_POINT ( 'NONE',  ( 12.63842701281683922, 44.55059781766745175, -9.846743663894590881 ) ) ;
#10303 = FACE_OUTER_BOUND ( 'NONE', #8736, .T. ) ;
#10304 = CARTESIAN_POINT ( 'NONE',  ( 10.00000000000000000, 51.81368534415484106, -10.88017736071110342 ) ) ;
#10306 = CARTESIAN_POINT ( 'NONE',  ( -0.1503990784575242878, 19.24884699246888786, -6.262539305110083276 ) ) ;
#10305 = CARTESIAN_POINT ( 'NONE',  ( 10.00000000000000000, 11.81368534415483751, -10.88017736071110342 ) ) ;
#10307 = DIRECTION ( 'NONE',  ( 0.000000000000000000, 0.000000000000000000, 1.000000000000000000 ) ) ;
#10308 = CARTESIAN_POINT ( 'NONE',  ( 17.20831665107776587, 34.13393115100078745, -7.208316651077762316 ) ) ;
#10309 = LINE ( 'NONE', #86798, #20217 ) ;
#10310 = DIRECTION ( 'NONE',  ( 0.000000000000000000, 0.000000000000000000, -1.000000000000000000 ) ) ;
#10311 = CARTESIAN_POINT ( 'NONE',  ( -4.164238869374098151, 26.59541550158063217, -3.795296366450310543 ) ) ;
#10312 = DIRECTION ( 'NONE',  ( 0.3173046564051031360, 0.000000000000000000, -0.9483236552061955482 ) ) ;
#10313 = ORIENTED_EDGE ( 'NONE', *, *, #28574, .T. ) ;
#10314 =( GEOMETRIC_REPRESENTATION_CONTEXT ( 3 ) GLOBAL_UNCERTAINTY_ASSIGNED_CONTEXT ( ( #73472 ) ) GLOBAL_UNIT_ASSIGNED_CONTEXT ( ( #71293, #55288, #3283 ) ) REPRESENTATION_CONTEXT ( 'NONE', 'WORKASPACE' ) );
#10315 = CARTESIAN_POINT ( 'NONE',  ( 6.204703633549690345, 62.84541550158063927, 14.16423886937410082 ) ) ;
#10316 = CARTESIAN_POINT ( 'NONE',  ( 0.1532563361054082862, 16.21726448433411960, 2.638427012816831674 ) ) ;
#10317 = DIRECTION ( 'NONE',  ( -0.6087614290087131064, 0.000000000000000000, -0.7933533402912409382 ) ) ;
#10318 = CARTESIAN_POINT ( 'NONE',  ( 19.42250999205614193, 50.14701867748817676, 5.440088680355555262 ) ) ;
#10319 = CARTESIAN_POINT ( 'NONE',  ( 5.148594389986208775, 15.00000000000000711, 13.69051944078650607 ) ) ;
#10320 = CARTESIAN_POINT ( 'NONE',  ( 10.00000000000000178, 34.31368534415484106, 10.88017736071110342 ) ) ;
#10321 = CARTESIAN_POINT ( 'NONE',  ( 0.6178305044545838731, 59.74863466993041783, 9.382169495545420901 ) ) ;
#10322 = CARTESIAN_POINT ( 'NONE',  ( 13.43411237798105340, 5.581968003263753531, 12.81628187352647963 ) ) ;
#10323 = CARTESIAN_POINT ( 'NONE',  ( 19.84674366389459266, 8.300597817667451750, 2.638427012816836559 ) ) ;
#10324 = VERTEX_POINT ( 'NONE', #65396 ) ;
#10325 = AXIS2_PLACEMENT_3D ( 'NONE', #98524, #29977, #21019 ) ;
#10326 = SURFACE_STYLE_USAGE ( .BOTH. , #57286 ) ;
#10327 = EDGE_CURVE ( 'NONE', #17231, #47751, #16601, .T. ) ;
#10328 = CARTESIAN_POINT ( 'NONE',  ( 0.000000000000000000, 61.50000000000000711, -6.500000000000000888 ) ) ;
#10329 = CARTESIAN_POINT ( 'NONE',  ( 20.36894250292379382, 58.67874883491396076, 10.36894250292379205 ) ) ;
#10330 = CARTESIAN_POINT ( 'NONE',  ( 22.26659068614895176, 29.72041550158063572, -7.082119434687042414 ) ) ;
#10331 = CARTESIAN_POINT ( 'NONE',  ( -0.8801773607111008646, 23.27201867748817676, 2.915334737309923430 ) ) ;
#10332 = CARTESIAN_POINT ( 'NONE',  ( 17.96484262340118221, 54.93868534415484106, 7.964842623401181321 ) ) ;
#10333 = DIRECTION ( 'NONE',  ( 0.5547001962252290364, 0.8320502943378437211, 0.000000000000000000 ) ) ;
#10334 = CARTESIAN_POINT ( 'NONE',  ( 11.08992015851877078, -87.81706477658710241, -4.000000000000000888 ) ) ;
#10335 = CARTESIAN_POINT ( 'NONE',  ( 5.076628168052703671, 16.84226448433411960, 8.527530157486179263 ) ) ;
#10336 = CARTESIAN_POINT ( 'NONE',  ( -14.56368227077860844, 0.2306972965111897811, 3.337246381125087424 ) ) ;
#10337 = CARTESIAN_POINT ( 'NONE',  ( 19.84674366389459266, 18.30059781766745175, 2.638427012816836559 ) ) ;
#10338 = CARTESIAN_POINT ( 'NONE',  ( 24.35999999999999233, 44.49999999999997868, -10.00000000000000000 ) ) ;
#10339 = FACE_OUTER_BOUND ( 'NONE', #85895, .T. ) ;
#10340 = CARTESIAN_POINT ( 'NONE',  ( 14.92337183194729988, 19.34226448433411960, -8.527530157486177487 ) ) ;
#10341 = CARTESIAN_POINT ( 'NONE',  ( 12.63842701281683034, 52.46726448433413026, 9.846743663894596210 ) ) ;
#10342 = CARTESIAN_POINT ( 'NONE',  ( 13.43411237798106583, 27.66530133659708568, -12.81628187352647252 ) ) ;
#10343 = STYLED_ITEM ( 'NONE', ( #41809 ), #7167 ) ;
#10344 = CARTESIAN_POINT ( 'NONE',  ( 10.00000000000000000, 46.81368534415484106, -10.88017736071110342 ) ) ;
#10345 = CARTESIAN_POINT ( 'NONE',  ( 12.63842701281683922, 29.55059781766745175, -9.846743663894590881 ) ) ;
#10347 = CARTESIAN_POINT ( 'NONE',  ( 7.361572987183170547, 17.05059781766745530, 9.846743663894590881 ) ) ;
#10346 = CARTESIAN_POINT ( 'NONE',  ( 2.917880565312948704, 42.63708216824729647, 12.26659068614894643 ) ) ;
#10348 = DIRECTION ( 'NONE',  ( 0.06975647374410356982, 0.9975640502598257520, -0.000000000000000000 ) ) ;
#10349 = CARTESIAN_POINT ( 'NONE',  ( 2.791683348922240793, 56.63393115100078035, 7.208316651077764092 ) ) ;
#10351 = CARTESIAN_POINT ( 'NONE',  ( 24.16423886937409904, 9.095415501580633943, 3.795296366450317205 ) ) ;
#10350 = CARTESIAN_POINT ( 'NONE',  ( 10.00000000000000000, 44.75893115100078745, -9.846743663894594434 ) ) ;
#10352 = CARTESIAN_POINT ( 'NONE',  ( -2.266590686148945544, 36.38708216824730357, -7.082119434687050408 ) ) ;
#10353 = CARTESIAN_POINT ( 'NONE',  ( 2.791683348922240793, 26.63393115100078745, 7.208316651077764092 ) ) ;
#10354 = CARTESIAN_POINT ( 'NONE',  ( 0.5774900079438590739, 42.64701867748816966, -5.440088680355550821 ) ) ;
#10355 = CARTESIAN_POINT ( 'NONE',  ( 19.42250999205614548, 20.98035201082150891, -5.440088680355545492 ) ) ;
#10356 = CARTESIAN_POINT ( 'NONE',  ( 12.91533473730992121, 44.52201867748816966, 10.88017736071110164 ) ) ;
#10357 = CARTESIAN_POINT ( 'NONE',  ( 4.559911319644449179, 27.23035201082150536, -9.422509992056141925 ) ) ;
#10358 = ORIENTED_EDGE ( 'NONE', *, *, #12845, .F. ) ;
#10359 = CARTESIAN_POINT ( 'NONE',  ( 13.43411237798105340, 30.58196800326374998, 12.81628187352647963 ) ) ;
#10360 = CARTESIAN_POINT ( 'NONE',  ( 7.084665262690076126, 59.10535201082150536, 10.88017736071109987 ) ) ;
#10361 = ORIENTED_EDGE ( 'NONE', *, *, #12228, .T. ) ;
#10362 = CIRCLE ( 'NONE', #55019, 15.00000000000000000 ) ;
#10363 = DIRECTION ( 'NONE',  ( 0.000000000000000000, 1.000000000000000000, 0.000000000000000000 ) ) ;
#10364 = CARTESIAN_POINT ( 'NONE',  ( 12.91533473730993009, 66.60535201082150536, -10.88017736071109987 ) ) ;
#10365 = VERTEX_POINT ( 'NONE', #26415 ) ;
#10366 = B_SPLINE_CURVE_WITH_KNOTS ( 'NONE', 3,
 ( #35875, #72035, #34022, #95025, #57030, #2097, #18064, #25573, #66367, #96903, #94052, #49521, #81378, #63057, #93554, #40569, #43372, #55570 ),
 .UNSPECIFIED., .F., .F.,
 ( 4, 2, 2, 2, 2, 2, 2, 2, 4 ),
 ( 0.0005459035990385047079, 0.001906373199480198037, 0.003266842799921891582, 0.004627312400363584911, 0.005987782000805278240, 0.007348251601246971569, 0.008708721201688664898, 0.01006919080213035909, 0.01142966040257205156 ),
 .UNSPECIFIED. ) ;
#10367 = CARTESIAN_POINT ( 'NONE',  ( 10.00000000000000000, 61.81368534415484106, -10.88017736071110342 ) ) ;
#10368 =( LENGTH_UNIT ( ) NAMED_UNIT ( * ) SI_UNIT ( .MILLI., .METRE. ) );
#10369 = DIRECTION ( 'NONE',  ( 0.000000000000000000, -1.000000000000000000, 0.000000000000000000 ) ) ;
#10370 = CARTESIAN_POINT ( 'NONE',  ( 7.850000000000003197, 98.49999999999998579, 8.000000000000000000 ) ) ;
#10371 = CARTESIAN_POINT ( 'NONE',  ( 10.00000000000000000, 55.55374883491396787, -14.16423886937410082 ) ) ;
#10372 = CARTESIAN_POINT ( 'NONE',  ( 12.63842701281683922, 9.550597817667449974, -9.846743663894590881 ) ) ;
#10373 = CARTESIAN_POINT ( 'NONE',  ( 24.16423886937410614, 4.303748834913967869, 8.672049930838204340E-16 ) ) ;
#10374 = CARTESIAN_POINT ( 'NONE',  ( 0.1532563361054082862, 1.217264484334117824, 2.638427012816831674 ) ) ;
#10375 = CARTESIAN_POINT ( 'NONE',  ( 18.52753015748618282, 43.92559781766745175, -4.923371831947291888 ) ) ;
#10376 = VERTEX_POINT ( 'NONE', #5420 ) ;
#10377 = CARTESIAN_POINT ( 'NONE',  ( 19.84674366389459621, 53.50893115100078745, 7.409399052514197653E-17 ) ) ;
#10378 = VERTEX_POINT ( 'NONE', #33902 ) ;
#10379 = CARTESIAN_POINT ( 'NONE',  ( 7.084665262690076126, 59.10535201082150536, 10.88017736071109987 ) ) ;
#10380 = CARTESIAN_POINT ( 'NONE',  ( 14.92337183194729988, 54.34226448433412315, -8.527530157486177487 ) ) ;
#10381 = CARTESIAN_POINT ( 'NONE',  ( -0.8801773607111008646, 68.27201867748817676, 2.915334737309923430 ) ) ;
#10382 = CARTESIAN_POINT ( 'NONE',  ( 17.96484262340118221, 61.18868534415482685, -7.964842623401177768 ) ) ;
#10383 = CARTESIAN_POINT ( 'NONE',  ( 20.88017736071110875, 5.772018677488170546, -2.915334737309920765 ) ) ;
#10384 = ADVANCED_FACE ( 'NONE', ( #19417 ), #72041, .T. ) ;
#10385 =( GEOMETRIC_REPRESENTATION_CONTEXT ( 3 ) GLOBAL_UNCERTAINTY_ASSIGNED_CONTEXT ( ( #50490 ) ) GLOBAL_UNIT_ASSIGNED_CONTEXT ( ( #65354, #91821, #6842 ) ) REPRESENTATION_CONTEXT ( 'NONE', 'WORKASPACE' ) );
#10386 = CARTESIAN_POINT ( 'NONE',  ( 22.81628187352648496, 41.83196800326375353, -3.434112377981050290 ) ) ;
#10387 = DIRECTION ( 'NONE',  ( -0.000000000000000000, -1.000000000000000000, -0.000000000000000000 ) ) ;
#10388 = ORIENTED_EDGE ( 'NONE', *, *, #89192, .F. ) ;
#10389 = STYLED_ITEM ( 'NONE', ( #91815 ), #85238 ) ;
#10390 = CARTESIAN_POINT ( 'NONE',  ( 22.81628187352648496, 26.83196800326374998, -3.434112377981050290 ) ) ;
#10391 = CARTESIAN_POINT ( 'NONE',  ( -0.8801773607111008646, 28.27201867748817321, 2.915334737309923430 ) ) ;
#10392 = ORIENTED_EDGE ( 'NONE', *, *, #63758, .T. ) ;
#10393 = CARTESIAN_POINT ( 'NONE',  ( 0.1532563361054100626, 10.80059781766745175, -2.638427012816831230 ) ) ;
#10394 = CARTESIAN_POINT ( 'NONE',  ( 10.00000000000000178, 67.25893115100079456, 9.846743663894594434 ) ) ;
#10396 = CARTESIAN_POINT ( 'NONE',  ( 0.1532563361054100626, 55.80059781766745175, -2.638427012816831230 ) ) ;
#10395 = CARTESIAN_POINT ( 'NONE',  ( 18.52753015748617571, 8.092264484334117824, 4.923371831947298993 ) ) ;
#10397 = CARTESIAN_POINT ( 'NONE',  ( 14.03351048042395632, 15.00000000000000000, 2.474486531753810059 ) ) ;
#10398 = CARTESIAN_POINT ( 'NONE',  ( 19.84674366389459266, 33.71726448433410894, -2.638427012816827677 ) ) ;
#10399 = CARTESIAN_POINT ( 'NONE',  ( -10.88853822400146676, 46.97908644289115898, 3.000000000000000000 ) ) ;
#10400 = DIRECTION ( 'NONE',  ( -0.000000000000000000, -0.000000000000000000, -1.000000000000000000 ) ) ;
#10402 = DIRECTION ( 'NONE',  ( 0.000000000000000000, -1.000000000000000000, 0.000000000000000000 ) ) ;
#10401 = CARTESIAN_POINT ( 'NONE',  ( 17.20831665107776587, 32.88393115100078745, 7.208316651077764980 ) ) ;
#10403 = LINE ( 'NONE', #63392, #29797 ) ;
#10405 = EDGE_LOOP ( 'NONE', ( #78253, #83545, #80972, #3170 ) ) ;
#10404 = CARTESIAN_POINT ( 'NONE',  ( 2.791683348922240793, 56.63393115100078035, 7.208316651077764092 ) ) ;
#10406 = DIRECTION ( 'NONE',  ( 0.8526401643540917341, 0.000000000000000000, -0.5224985647159496871 ) ) ;
#10407 = EDGE_CURVE ( 'NONE', #15068, #83910, #5317, .T. ) ;
#10408 = CARTESIAN_POINT ( 'NONE',  ( -2.816281873526473856, 29.33196800326376064, 3.434112377981055619 ) ) ;
#10409 = CARTESIAN_POINT ( 'NONE',  ( 2.791683348922237240, 50.38393115100078035, -7.208316651077763204 ) ) ;
#10410 = PLANE ( 'NONE',  #39299 ) ;
#10411 = CARTESIAN_POINT ( 'NONE',  ( 6.204703633549690345, 40.76208216824731778, -14.16423886937410259 ) ) ;
#10412 = CARTESIAN_POINT ( 'NONE',  ( 2.791683348922240793, 16.63393115100078745, 7.208316651077764092 ) ) ;
#10413 = ADVANCED_FACE ( 'NONE', ( #72793 ), #79332, .T. ) ;
#10414 = CARTESIAN_POINT ( 'NONE',  ( 19.84674366389459266, 3.300597817667451750, 2.638427012816836559 ) ) ;
#10415 = CARTESIAN_POINT ( 'NONE',  ( -46.90021668353733730, 100.5602553471094183, 9.231058622660704316 ) ) ;
#10416 = CARTESIAN_POINT ( 'NONE',  ( -4.164238869374098151, 41.59541550158061796, -3.795296366450310543 ) ) ;
#10417 = CARTESIAN_POINT ( 'NONE',  ( 14.92337183194729633, 62.67559781766745886, 8.527530157486181039 ) ) ;
#10418 = CARTESIAN_POINT ( 'NONE',  ( 20.88017736071110519, 10.56368534415483929, 2.639326808657452039E-16 ) ) ;
#10419 = CARTESIAN_POINT ( 'NONE',  ( 10.00000000000000178, 28.05374883491396787, 14.16423886937410082 ) ) ;
#10421 = CARTESIAN_POINT ( 'NONE',  ( 19.84674366389459621, 33.50893115100078745, 7.409399052514197653E-17 ) ) ;
#10420 = CARTESIAN_POINT ( 'NONE',  ( 13.79529636645030344, 33.26208216824730357, 14.16423886937410614 ) ) ;
#10422 = LINE ( 'NONE', #93914, #85050 ) ;
#10424 = CARTESIAN_POINT ( 'NONE',  ( 19.84674366389459266, 58.71726448433411605, -2.638427012816827677 ) ) ;
#10423 = CARTESIAN_POINT ( 'NONE',  ( -0.8801773607111009756, 28.27201867748817321, 2.915334737309923874 ) ) ;
#10425 = VERTEX_POINT ( 'NONE', #96322 ) ;
#10426 = CARTESIAN_POINT ( 'NONE',  ( 7.084665262690076126, 39.10535201082150536, 10.88017736071109987 ) ) ;
#10427 = DIRECTION ( 'NONE',  ( 0.000000000000000000, 1.000000000000000000, 0.000000000000000000 ) ) ;
#10428 = CARTESIAN_POINT ( 'NONE',  ( 10.72261300086672797, -40.29758884457105239, 3.750000000000000444 ) ) ;
#10429 = CARTESIAN_POINT ( 'NONE',  ( 3.591859063236761518, 64.95696800326376774, 11.09922568453594849 ) ) ;
#10430 = CARTESIAN_POINT ( 'NONE',  ( 14.16423886937410259, 9.303748834913978527, -2.602085213965210642E-15 ) ) ;
#10431 = CARTESIAN_POINT ( 'NONE',  ( 10.00000000000000000, 59.75893115100078745, -9.846743663894594434 ) ) ;
#10432 = CARTESIAN_POINT ( 'NONE',  ( 0.1532563361054100626, 65.80059781766745175, -2.638427012816831230 ) ) ;
#10433 = ORIENTED_EDGE ( 'NONE', *, *, #12492, .T. ) ;
#10434 = CIRCLE ( 'NONE', #96663, 0.2500000000000002220 ) ;
#10435 = CARTESIAN_POINT ( 'NONE',  ( 24.16423886937409904, 24.09541550158063927, 3.795296366450317205 ) ) ;
#10436 = EDGE_CURVE ( 'NONE', #54278, #91250, #19320, .T. ) ;
#10437 = DIRECTION ( 'NONE',  ( 3.197442310920450836E-14, 0.000000000000000000, 1.000000000000000000 ) ) ;
#10438 = DIRECTION ( 'NONE',  ( 0.000000000000000000, 1.000000000000000000, -0.000000000000000000 ) ) ;
#10439 = CARTESIAN_POINT ( 'NONE',  ( 2.917880565312950480, 65.97041550158063217, -12.26659068614894821 ) ) ;
#10440 = CARTESIAN_POINT ( 'NONE',  ( 22.81628187352647785, 21.62363466993041783, 6.195893100308588602E-16 ) ) ;
#10441 = DIRECTION ( 'NONE',  ( -1.000000000000000000, 0.000000000000000000, -1.734723475976805517E-15 ) ) ;
#10442 = CARTESIAN_POINT ( 'NONE',  ( 5.076628168052703671, 16.84226448433411960, 8.527530157486179263 ) ) ;
#10443 = CARTESIAN_POINT ( 'NONE',  ( -0.1503990784575328643, 5.127771745786130708, 6.262539305110068177 ) ) ;
#10444 = DIRECTION ( 'NONE',  ( 1.000000000000000000, 0.000000000000000000, 0.000000000000000000 ) ) ;
#10445 = CARTESIAN_POINT ( 'NONE',  ( 14.04391541078763161, 4.402316570082688340E-16, 3.608107528142934228 ) ) ;
#10446 = CARTESIAN_POINT ( 'NONE',  ( 20.88017736071110519, 15.56368534415483751, 2.639326808657452039E-16 ) ) ;
#10447 = LINE ( 'NONE', #65892, #40025 ) ;
#10448 = CARTESIAN_POINT ( 'NONE',  ( -0.8801773607110991993, 37.85535201082151247, -2.915334737309923874 ) ) ;
#10449 = CARTESIAN_POINT ( 'NONE',  ( 4.559911319644449179, 33.89701867748817676, 9.422509992056141925 ) ) ;
#10450 = CARTESIAN_POINT ( 'NONE',  ( -1.099225684535947600, 4.540301336597087456, 6.408140936763237150 ) ) ;
#10451 = CARTESIAN_POINT ( 'NONE',  ( 0.1532563361054100626, 60.80059781766744464, -2.638427012816831230 ) ) ;
#10452 = CARTESIAN_POINT ( 'NONE',  ( -45.63603160005279591, 104.8105884637807890, -5.540438805289570112 ) ) ;
#10453 = CARTESIAN_POINT ( 'NONE',  ( 14.92337183194729988, 9.342264484334119601, -8.527530157486177487 ) ) ;
#10454 = ORIENTED_EDGE ( 'NONE', *, *, #41583, .T. ) ;
#10455 = CARTESIAN_POINT ( 'NONE',  ( 19.42250999205614193, 25.14701867748817321, 5.440088680355555262 ) ) ;
#10456 = CARTESIAN_POINT ( 'NONE',  ( 16.40814093676324603, 32.45696800326375353, -11.09922568453594671 ) ) ;
#10457 = CARTESIAN_POINT ( 'NONE',  ( -1.926860441876562025, 54.47997603579417358, -3.195792623639529761 ) ) ;
#10458 =( BOUNDED_SURFACE ( )  B_SPLINE_SURFACE ( 3, 2, ( 
 ( #93443, #39476, #16475 ),
 ( #31938, #23003, #47449 ),
 ( #992, #46952, #68984 ),
 ( #62439, #53470, #24477 ),
 ( #52978, #77948, #9455 ),
 ( #75982, #62942, #15010 ),
 ( #7511, #15979, #38002 ),
 ( #68495, #38490, #21 ),
 ( #30469, #30965, #94422 ),
 ( #24969, #63433, #10930 ) ),
 .UNSPECIFIED., .F., .F., .F. ) 
 B_SPLINE_SURFACE_WITH_KNOTS ( ( 4, 2, 2, 2, 4 ),
 ( 3, 3 ),
 ( 0.000000000000000000, 0.002067014858588510882, 0.003100522287882766324, 0.003617276002529893827, 0.004134029717177021765 ),
 ( 0.000000000000000000, 1.000000000000000000 ),
 .UNSPECIFIED. ) 
 GEOMETRIC_REPRESENTATION_ITEM ( )  RATIONAL_B_SPLINE_SURFACE ( (
 ( 1.000000000000000000, 0.7411386215561424073, 1.000000000000000000),
 ( 1.000000000000000000, 0.7517628147009809414, 1.000000000000000000),
 ( 1.000000000000000000, 0.7644153482607498606, 1.000000000000000000),
 ( 1.000000000000000000, 0.8033584422216667464, 1.000000000000000000),
 ( 1.000000000000000000, 0.8197614970480194829, 1.000000000000000000),
 ( 1.000000000000000000, 0.8550190949536496943, 1.000000000000000000),
 ( 1.000000000000000000, 0.8686037895732486858, 1.000000000000000000),
 ( 1.000000000000000000, 0.9009153382757982831, 1.000000000000000000),
 ( 1.000000000000000000, 0.9197777054298900135, 1.000000000000000000),
 ( 1.000000000000000000, 0.9412039349194007976, 1.000000000000000000) ) ) 
 REPRESENTATION_ITEM ( '' )  SURFACE ( )  );
#10459 = CARTESIAN_POINT ( 'NONE',  ( 7.361572987183170547, 57.05059781766744464, 9.846743663894590881 ) ) ;
#10460 = CARTESIAN_POINT ( 'NONE',  ( 15.44008868035555793, 66.39701867748817676, -9.422509992056140149 ) ) ;
#10461 = CARTESIAN_POINT ( 'NONE',  ( 19.84674366389459621, 18.50893115100078745, 7.409399052514197653E-17 ) ) ;
#10462 = CARTESIAN_POINT ( 'NONE',  ( 16.40814093676323893, 30.79030133659708923, 11.09922568453595026 ) ) ;
#10464 = CARTESIAN_POINT ( 'NONE',  ( 18.72515096720579209, 51.07228050351030646, -6.499999999999869438 ) ) ;
#10463 = CARTESIAN_POINT ( 'NONE',  ( 17.96484262340118221, 59.93868534415484106, 7.964842623401181321 ) ) ;
#10465 = CARTESIAN_POINT ( 'NONE',  ( 6.565887622018943937, 63.08196800326376064, -12.81628187352647608 ) ) ;
#10466 = ORIENTED_EDGE ( 'NONE', *, *, #46090, .F. ) ;
#10467 = CARTESIAN_POINT ( 'NONE',  ( 0.000000000000000000, 14.49999999999999822, 0.000000000000000000 ) ) ;
#10468 = CARTESIAN_POINT ( 'NONE',  ( 15.44008868035555793, 11.39701867748817143, -9.422509992056140149 ) ) ;
#10469 = CARTESIAN_POINT ( 'NONE',  ( 6.565887622018943937, 65.16530133659709634, 12.81628187352647430 ) ) ;
#10470 = CARTESIAN_POINT ( 'NONE',  ( 10.00000000000000178, 22.25893115100078745, 9.846743663894594434 ) ) ;
#10471 = CARTESIAN_POINT ( 'NONE',  ( 10.00000000000000000, 1.813685344154837731, -10.88017736071110342 ) ) ;
#10472 = CARTESIAN_POINT ( 'NONE',  ( 19.84674366389459266, 23.30059781766745530, 2.638427012816836559 ) ) ;
#10473 = CARTESIAN_POINT ( 'NONE',  ( 24.16423886937410614, 59.51208216824728936, -3.795296366450302550 ) ) ;
#10474 = ORIENTED_EDGE ( 'NONE', *, *, #77960, .T. ) ;
#10475 = CARTESIAN_POINT ( 'NONE',  ( -0.8801773607110991993, 7.855352010821504471, -2.915334737309923874 ) ) ;
#10476 = CARTESIAN_POINT ( 'NONE',  ( -0.8801773607110991993, 27.85535201082150181, -2.915334737309923874 ) ) ;
#10477 = CARTESIAN_POINT ( 'NONE',  ( -0.1503990784575327533, 7.222660991849186196, -6.262539305110070842 ) ) ;
#10478 = EDGE_LOOP ( 'NONE', ( #12078, #74864, #52246, #33021 ) ) ;
#10479 = ORIENTED_EDGE ( 'NONE', *, *, #48984, .F. ) ;
#10480 = CARTESIAN_POINT ( 'NONE',  ( 7.084665262690076126, 22.02201867748817321, -10.88017736071110164 ) ) ;
#10481 = CARTESIAN_POINT ( 'NONE',  ( 5.076628168052704559, 55.17559781766745175, -8.527530157486179263 ) ) ;
#10482 = STYLED_ITEM ( 'NONE', ( #51125 ), #5997 ) ;
#10483 = CARTESIAN_POINT ( 'NONE',  ( 6.565887622018943937, 50.16530133659708213, 12.81628187352647430 ) ) ;
#10484 = CARTESIAN_POINT ( 'NONE',  ( 4.219999999999999751, 36.75000000000000000, -4.000000000000000000 ) ) ;
#10485 = CARTESIAN_POINT ( 'NONE',  ( 24.16423886937410614, 24.51208216824730002, -3.795296366450302550 ) ) ;
#10486 = CARTESIAN_POINT ( 'NONE',  ( 12.91533473730992121, 39.52201867748817676, 10.88017736071110164 ) ) ;
#10487 = CARTESIAN_POINT ( 'NONE',  ( 7.084665262690076126, 12.02201867748817321, -10.88017736071110164 ) ) ;
#10488 = CARTESIAN_POINT ( 'NONE',  ( 10.00000000000000000, 59.75893115100078745, -9.846743663894594434 ) ) ;
#10489 = CARTESIAN_POINT ( 'NONE',  ( -10.57647196447611648, -40.47791205351722965, -3.749999999999999556 ) ) ;
#10490 = CARTESIAN_POINT ( 'NONE',  ( 12.63842701281683922, 34.55059781766745886, -9.846743663894590881 ) ) ;
#10491 = CARTESIAN_POINT ( 'NONE',  ( 7.361572987183170547, 7.050597817667451750, 9.846743663894590881 ) ) ;
#10492 = CARTESIAN_POINT ( 'NONE',  ( -12.81628187352647252, -25.66803199673624292, 3.434112377981066722 ) ) ;
#10493 = ORIENTED_EDGE ( 'NONE', *, *, #77155, .F. ) ;
#10494 = CARTESIAN_POINT ( 'NONE',  ( 10.00000000000000000, 9.758931151000785675, -9.846743663894594434 ) ) ;
#10495 = CARTESIAN_POINT ( 'NONE',  ( 10.00000000000000178, 67.25893115100079456, 9.846743663894594434 ) ) ;
#10496 = CARTESIAN_POINT ( 'NONE',  ( 10.00000000000000178, 49.31368534415484106, 10.88017736071110342 ) ) ;
#10498 = CARTESIAN_POINT ( 'NONE',  ( 16.40814093676323893, 40.79030133659708923, 11.09922568453595026 ) ) ;
#10497 = CARTESIAN_POINT ( 'NONE',  ( 7.084665262690076126, 19.10535201082150181, 10.88017736071109987 ) ) ;
#10499 = CARTESIAN_POINT ( 'NONE',  ( -4.164238869374099039, 26.80374883491397142, 8.674139862899312516E-16 ) ) ;
#10500 = EDGE_CURVE ( 'NONE', #23770, #60007, #65292, .T. ) ;
#10501 = CARTESIAN_POINT ( 'NONE',  ( 20.15039907845753930, 11.74884699246888964, 6.262539305110064625 ) ) ;
#10502 = CARTESIAN_POINT ( 'NONE',  ( 22.81628187352647785, 61.41530133659709634, 3.434112377981063169 ) ) ;
#10503 = ORIENTED_EDGE ( 'NONE', *, *, #37300, .F. ) ;
#10504 = CARTESIAN_POINT ( 'NONE',  ( 12.63842701281683922, 59.55059781766744464, -9.846743663894590881 ) ) ;
#10505 = CARTESIAN_POINT ( 'NONE',  ( 10.00000000000000178, 39.31368534415484106, 10.88017736071110342 ) ) ;
#10506 = ORIENTED_EDGE ( 'NONE', *, *, #18879, .T. ) ;
#10507 = CARTESIAN_POINT ( 'NONE',  ( 0.1532563361054082862, 1.217264484334117824, 2.638427012816831674 ) ) ;
#10508 = CARTESIAN_POINT ( 'NONE',  ( 19.84674366389459621, 28.50893115100078745, 7.409399052514197653E-17 ) ) ;
#10509 = CARTESIAN_POINT ( 'NONE',  ( 10.00000000000000000, 66.81368534415484817, -10.88017736071110342 ) ) ;
#10510 = B_SPLINE_CURVE_WITH_KNOTS ( 'NONE', 3,
 ( #2135, #1143, #15650, #16622, #92121, #46133 ),
 .UNSPECIFIED., .F., .F.,
 ( 4, 2, 4 ),
 ( 0.0002800001862105968306, 0.0006862054174524884372, 0.001092410648694380152 ),
 .UNSPECIFIED. ) ;
#10511 =( NAMED_UNIT ( * ) SI_UNIT ( $, .STERADIAN. ) SOLID_ANGLE_UNIT ( ) );
#10513 = FACE_OUTER_BOUND ( 'NONE', #1182, .T. ) ;
#10512 = CARTESIAN_POINT ( 'NONE',  ( 20.88017736071110519, 55.56368534415484817, 2.639326808657452039E-16 ) ) ;
#10514 = CARTESIAN_POINT ( 'NONE',  ( 12.91533473730992121, 64.52201867748817676, 10.88017736071110164 ) ) ;
#10515 = PRESENTATION_LAYER_ASSIGNMENT (  '', '', ( #53621 ) ) ;
#10517 = ORIENTED_EDGE ( 'NONE', *, *, #17240, .F. ) ;
#10516 = CARTESIAN_POINT ( 'NONE',  ( 0.1532563361054100626, 10.80059781766745175, -2.638427012816831230 ) ) ;
#10518 = AXIS2_PLACEMENT_3D ( 'NONE', #46159, #8163, #61146 ) ;
#10519 = AXIS2_PLACEMENT_3D ( 'NONE', #25436, #77413, #69937 ) ;
#10520 = B_SPLINE_CURVE_WITH_KNOTS ( 'NONE', 3,
 ( #35098, #97127, #28597, #89594 ),
 .UNSPECIFIED., .F., .F.,
 ( 4, 4 ),
 ( 6.254634441385501671E-17, 0.001060528352561988753 ),
 .UNSPECIFIED. ) ;
#10521 = CARTESIAN_POINT ( 'NONE',  ( 5.093587308868497310, 15.00000000000000000, -15.16353404595997567 ) ) ;
#10522 = EDGE_CURVE ( 'NONE', #15284, #18635, #44589, .T. ) ;
#10523 = CARTESIAN_POINT ( 'NONE',  ( 19.84674366389459621, 58.50893115100078745, 7.409399052514197653E-17 ) ) ;
#10524 = ORIENTED_EDGE ( 'NONE', *, *, #45654, .T. ) ;
#10525 = ORIENTED_EDGE ( 'NONE', *, *, #5001, .T. ) ;
#10526 = CARTESIAN_POINT ( 'NONE',  ( 13.99999999999999822, 10.49999999999999822, -6.500000000000000888 ) ) ;
#10527 = CIRCLE ( 'NONE', #63253, 15.00000000000000000 ) ;
#10528 = CARTESIAN_POINT ( 'NONE',  ( 22.26659068614895176, 9.720415501580633943, -7.082119434687042414 ) ) ;
#10529 =( BOUNDED_SURFACE ( )  B_SPLINE_SURFACE ( 1, 2, ( 
 ( #64496, #94516, #19508, #10534, #56527, #33028, #34492, #34984, #72991, #10049, #64984, #95003, #40548, #95509, #4521, #27492, #48520, #41044, #57500, #87995, #86048, #17559, #3052, #94031, #25552, #56044, #33506, #64004, #96510, #67477, #43964, #90451, #88992, #13486, #42995, #12981, #20993, #51480, #28964, #82470, #59467, #89969, #36977, #58479, #6977, #37482, #29452, #80992, #27982, #97997, #66480, #75461, #82967, #35979, #28486, #59959, #14486, #89483, #21989, #20496, #12495, #52465, #51983, #97008, #98496, #74468, #97500, #74968, #50984, #58980, #81974, #43478, #44958, #67971, #81479, #73477, #5992, #50495, #88491, #36487, #66979, #21485, #13991, #73979, #44466, #57986, #6473, #19993, #5006, #35488, #65984, #5504, #91824, #60942, #53443, #7482, #62414, #31424, #37979, #15952, #77923, #77417, #9429, #8933, #76936, #30937, #69941, #53946, #22476, #61928, #76450, #85430, #39933, #8445, #30443, #54427, #61436, #91453, #69444, #39450, #91942, #23473, #70436, #16939, #92429, #22978, #84936, #23954, #14983, #84453, #16447, #90946, #47421, #68469, #52951, #29951, #92919, #60456, #83952, #964, #38952, #46925, #15478, #45961, #7966, #46445, #31912, #38464, #68956, #488, #1461, #24449, #83462, #45454, #54916, #75955, #42392, #10420, #56416, #72380, #93913, #64865, #18911, #79888, #3909, #62919, #71893, #40928, #2453, #55424, #19391, #71426, #1953, #32417, #40436, #94399, #93419, #25441, #55924, #49387, #79409, #34376, #86423, #24942, #95386, #11395, #63887, #10910, #87875, #70935, #85932, #2941, #17442, #47909, #33389, #32909, #41917, #78414, #9932, #94892, #64382, #49877, #63409, #17924, #48408, #57381, #78911, #86902, #25914, #26390, #18412, #48895, #41432, #80389, #56890, #3416, #33877, #87394, #26888, #11892, #96892, #89850, #88380, #89362, #36862, #65367, #43849, #35865, #58351, #51364, #21366, #35373, #12377, #59347, #96392, #81365, #19877, #74343, #21870, #67354, #34873, #5871, #12864, #95897, #28369, #90331, #59841, #73365, #65864, #36363, #43362, #97880, #20873, #4893, #66858, #97376, #28844, #82845, #58856, #42882, #82346, #81851, #6353, #27866, #13364, #57869, #88873, #66354, #51861, #13867, #44347, #74852, #29340, #52348, #20380, #14365, #72871, #4406, #27376, #50873, #50370, #73862, #80878, #5390, #22855, #15361, #84822, #69826, #76333, #77304, #45339, #67858, #16329, #38836, #83836, #85312, #30823, #84344, #61811, #7359, #53327, #7849, #98871, #46812, #1349, #14867, #60341, #38347, #37365, #75339, #375, #45846, #76816, #61321, #75839, #69330, #24335, #91832, #852, #44835, #15846, #8818, #6854, #37861, #68353 ),
 ( #39332, #98377, #46330, #68842, #30326, #29833, #62298, #23350, #90835, #22362, #83345, #53832, #52836, #60828, #91329, #92317, #8333, #31801, #31309, #23842, #92806, #54309, #54795, #94276, #3793, #85809, #57260, #78797, #2333, #25799, #64260, #78294, #55298, #3292, #56774, #40804, #9308, #18294, #63285, #72265, #64748, #56299, #17322, #41311, #17806, #47795, #86793, #94773, #10305, #71304, #95260, #34248, #79284, #9810, #71783, #10793, #1836, #2824, #48777, #77798, #26766, #24822, #39816, #16820, #79773, #47296, #93298, #33756, #26272, #87269, #40312, #70817, #32788, #33276, #18791, #93791, #25321, #55807, #49274, #63768, #70321, #32293, #11272, #62798, #86300, #48286, #41792, #59226, #80760, #51746, #5756, #66741, #89730, #49753, #58739, #96272, #88252, #42276, #6244, #58228, #29226, #87755, #27251, #81246, #19269, #12255, #42762, #36245, #66234, #21247, #73245, #80264, #82229, #97266, #50759, #96769, #74731, #57750, #11767, #27745, #72746, #4279, #88748, #19760, #28736, #34753, #65243, #81729, #51242, #36748, #50244, #95769, #4772, #44227, #35245, #73739, #12745, #13244, #43243, #65742, #35746, #67238, #43736, #20258, #5269, #28244, #89244, #13744, #20753, #97761, #74223, #76224, #23730, #52234, #30699, #82726, #84708, #98259, #91714, #45223, #29717, #61688, #53706, #6735, #44726, #68722, #15734, #46695, #16211, #8699, #59726, #60711, #75223, #46217, #91208, #22736, #68241, #92205, #83225, #98758, #37251, #61210, #39215, #54193, #21753, #23234, #30208, #14245, #15243, #77193, #69702, #60224, #22243, #84226, #53219, #1232, #7738, #90718, #76703, #8222, #38717, #90221, #45722, #52720, #69216, #38232, #67740, #14750, #251, #75720, #7235, #83721, #742, #31195, #37742, #4048, #34510, #12026, #32172, #81013, #12514, #4541, #54678, #70196, #42525, #41563, #50516, #58004, #11042, #3557, #73009, #88513, #64514, #65506, #62675, #85199, #35003, #27020, #72030, #73498, #19040, #72514, #50025, #93175, #34017, #95020, #87036, #96028, #20015, #1716, #47177, #26528, #24212, #62177, #87526, #57025, #65003, #49516, #24701, #57520, #43016, #80025, #88016, #31685, #95530, #27510, #92687, #55172, #18546, #49038, #9196, #16704, #19528, #39709, #11529, #77682, #80527, #79542, #42050, #52004, #6015, #35508, #66002, #59980, #67497, #89011, #97522, #6493, #96530, #60477, #13003, #28005, #5024, #67994, #58501, #81498, #74990, #14009, #22008, #43498, #66506, #97031, #59490, #6997, #59001, #28507, #89503, #44978, #21506, #90966, #20518, #75484, #22500, #45474, #13507, #89990, #37502, #21014, #98519, #52482, #82990, #29972, #51003, #37001, #43989 ) ),
 .UNSPECIFIED., .F., .F., .T. ) 
 B_SPLINE_SURFACE_WITH_KNOTS ( ( 2, 2 ),
 ( 3, 2, 2, 2, 2, 2, 2, 2, 2, 2, 2, 2, 2, 2, 2, 2, 2, 2, 2, 2, 2, 2, 2, 2, 2, 2, 2, 2, 2, 2, 2, 2, 2, 2, 2, 2, 2, 2, 2, 2, 2, 2, 2, 2, 2, 2, 2, 2, 2, 2, 2, 2, 2, 2, 2, 2, 2, 2, 2, 2, 2, 2, 2, 2, 2, 2, 2, 2, 2, 2, 2, 2, 2, 2, 2, 2, 2, 2, 2, 2, 2, 2, 2, 2, 2, 2, 2, 2, 2, 2, 2, 2, 2, 2, 2, 2, 2, 2, 2, 2, 2, 2, 2, 2, 2, 2, 2, 2, 2, 2, 2, 2, 2, 2, 2, 2, 2, 2, 2, 2, 2, 2, 2, 2, 2, 2, 2, 2, 2, 2, 2, 2, 2, 2, 2, 2, 2, 2, 2, 2, 2, 2, 2, 2, 2, 2, 2, 2, 2, 2, 2, 2, 2, 2, 2, 2, 2, 2, 2, 2, 2, 2, 3 ),
 ( 0.000000000000000000, 1.000000000000000000 ),
 ( 0.000000000000000000, 0.005952380952380952051, 0.01190476190476190410, 0.01785714285714285615, 0.02380952380952380820, 0.02976190476190476025, 0.03571428571428571230, 0.04166666666666666435, 0.04761904761904761640, 0.05357142857142856845, 0.05952380952380952051, 0.06547619047619047949, 0.07142857142857142461, 0.07738095238095238360, 0.08333333333333332871, 0.08928571428571428770, 0.09523809523809523281, 0.1011904761904761918, 0.1071428571428571369, 0.1130952380952380959, 0.1190476190476190410, 0.1250000000000000000, 0.1309523809523809590, 0.1369047619047619180, 0.1428571428571428492, 0.1488095238095238082, 0.1547619047619047672, 0.1607142857142857262, 0.1666666666666666574, 0.1726190476190476164, 0.1785714285714285754, 0.1845238095238095344, 0.1904761904761904656, 0.1964285714285714246, 0.2023809523809523836, 0.2083333333333333426, 0.2142857142857142738, 0.2202380952380952328, 0.2261904761904761918, 0.2321428571428571508, 0.2380952380952380820, 0.2440476190476190410, 0.2500000000000000000, 0.2559523809523809312, 0.2619047619047619180, 0.2678571428571428492, 0.2738095238095238360, 0.2797619047619047672, 0.2857142857142856984, 0.2916666666666666852, 0.2976190476190476164, 0.3035714285714285476, 0.3095238095238095344, 0.3154761904761904656, 0.3214285714285714524, 0.3273809523809523836, 0.3333333333333333148, 0.3392857142857143016, 0.3452380952380952328, 0.3511904761904761640, 0.3571428571428571508, 0.3630952380952380820, 0.3690476190476190688, 0.3750000000000000000, 0.3809523809523809312, 0.3869047619047619180, 0.3928571428571428492, 0.3988095238095238360, 0.4047619047619047672, 0.4107142857142856984, 0.4166666666666666852, 0.4226190476190476164, 0.4285714285714285476, 0.4345238095238095344, 0.4404761904761904656, 0.4464285714285714524, 0.4523809523809523836, 0.4583333333333333148, 0.4642857142857143016, 0.4702380952380952328, 0.4761904761904761640, 0.4821428571428571508, 0.4880952380952380820, 0.4940476190476190688, 0.5000000000000000000, 0.5059523809523809312, 0.5119047619047618625, 0.5178571428571429047, 0.5238095238095238360, 0.5297619047619047672, 0.5357142857142856984, 0.5416666666666666297, 0.5476190476190476719, 0.5535714285714286031, 0.5595238095238095344, 0.5654761904761904656, 0.5714285714285713969, 0.5773809523809523281, 0.5833333333333333703, 0.5892857142857143016, 0.5952380952380952328, 0.6011904761904761640, 0.6071428571428570953, 0.6130952380952381375, 0.6190476190476190688, 0.6250000000000000000, 0.6309523809523809312, 0.6369047619047618625, 0.6428571428571429047, 0.6488095238095238360, 0.6547619047619047672, 0.6607142857142856984, 0.6666666666666666297, 0.6726190476190476719, 0.6785714285714286031, 0.6845238095238095344, 0.6904761904761904656, 0.6964285714285713969, 0.7023809523809523281, 0.7083333333333333703, 0.7142857142857143016, 0.7202380952380952328, 0.7261904761904761640, 0.7321428571428570953, 0.7380952380952381375, 0.7440476190476190688, 0.7500000000000000000, 0.7559523809523809312, 0.7619047619047618625, 0.7678571428571429047, 0.7738095238095238360, 0.7797619047619047672, 0.7857142857142856984, 0.7916666666666666297, 0.7976190476190476719, 0.8035714285714286031, 0.8095238095238095344, 0.8154761904761904656, 0.8214285714285713969, 0.8273809523809523281, 0.8333333333333333703, 0.8392857142857143016, 0.8452380952380952328, 0.8511904761904761640, 0.8571428571428570953, 0.8630952380952381375, 0.8690476190476190688, 0.8750000000000000000, 0.8809523809523809312, 0.8869047619047618625, 0.8928571428571429047, 0.8988095238095238360, 0.9047619047619047672, 0.9107142857142856984, 0.9166666666666666297, 0.9226190476190476719, 0.9285714285714286031, 0.9345238095238095344, 0.9404761904761904656, 0.9464285714285713969, 0.9523809523809523281, 0.9583333333333333703, 0.9642857142857143016 ),
 .UNSPECIFIED. ) 
 GEOMETRIC_REPRESENTATION_ITEM ( )  RATIONAL_B_SPLINE_SURFACE ( (
 ( 1.000000000000000000, 0.9659258262890683122, 1.000000000000000000, 0.9659258262890683122, 1.000000000000000000, 0.9659258262890683122, 1.000000000000000000, 0.9659258262890683122, 1.000000000000000000, 0.9659258262890683122, 1.000000000000000000, 0.9659258262890683122, 1.000000000000000000, 0.9659258262890683122, 1.000000000000000000, 0.9659258262890683122, 1.000000000000000000, 0.9659258262890683122, 1.000000000000000000, 0.9659258262890683122, 1.000000000000000000, 0.9659258262890683122, 1.000000000000000000, 0.9659258262890683122, 1.000000000000000000, 0.9659258262890683122, 1.000000000000000000, 0.9659258262890683122, 1.000000000000000000, 0.9659258262890683122, 1.000000000000000000, 0.9659258262890683122, 1.000000000000000000, 0.9659258262890683122, 1.000000000000000000, 0.9659258262890683122, 1.000000000000000000, 0.9659258262890683122, 1.000000000000000000, 0.9659258262890683122, 1.000000000000000000, 0.9659258262890683122, 1.000000000000000000, 0.9659258262890683122, 1.000000000000000000, 0.9659258262890683122, 1.000000000000000000, 0.9659258262890683122, 1.000000000000000000, 0.9659258262890683122, 1.000000000000000000, 0.9659258262890683122, 1.000000000000000000, 0.9659258262890683122, 1.000000000000000000, 0.9659258262890683122, 1.000000000000000000, 0.9659258262890683122, 1.000000000000000000, 0.9659258262890683122, 1.000000000000000000, 0.9659258262890683122, 1.000000000000000000, 0.9659258262890683122, 1.000000000000000000, 0.9659258262890683122, 1.000000000000000000, 0.9659258262890683122, 1.000000000000000000, 0.9659258262890683122, 1.000000000000000000, 0.9659258262890683122, 1.000000000000000000, 0.9659258262890683122, 1.000000000000000000, 0.9659258262890683122, 1.000000000000000000, 0.9659258262890683122, 1.000000000000000000, 0.9659258262890683122, 1.000000000000000000, 0.9659258262890683122, 1.000000000000000000, 0.9659258262890683122, 1.000000000000000000, 0.9659258262890683122, 1.000000000000000000, 0.9659258262890683122, 1.000000000000000000, 0.9659258262890683122, 1.000000000000000000, 0.9659258262890683122, 1.000000000000000000, 0.9659258262890683122, 1.000000000000000000, 0.9659258262890683122, 1.000000000000000000, 0.9659258262890683122, 1.000000000000000000, 0.9659258262890683122, 1.000000000000000000, 0.9659258262890683122, 1.000000000000000000, 0.9659258262890683122, 1.000000000000000000, 0.9659258262890683122, 1.000000000000000000, 0.9659258262890683122, 1.000000000000000000, 0.9659258262890683122, 1.000000000000000000, 0.9659258262890683122, 1.000000000000000000, 0.9659258262890683122, 1.000000000000000000, 0.9659258262890683122, 1.000000000000000000, 0.9659258262890683122, 1.000000000000000000, 0.9659258262890683122, 1.000000000000000000, 0.9659258262890683122, 1.000000000000000000, 0.9659258262890683122, 1.000000000000000000, 0.9659258262890683122, 1.000000000000000000, 0.9659258262890683122, 1.000000000000000000, 0.9659258262890683122, 1.000000000000000000, 0.9659258262890683122, 1.000000000000000000, 0.9659258262890683122, 1.000000000000000000, 0.9659258262890683122, 1.000000000000000000, 0.9659258262890683122, 1.000000000000000000, 0.9659258262890683122, 1.000000000000000000, 0.9659258262890683122, 1.000000000000000000, 0.9659258262890683122, 1.000000000000000000, 0.9659258262890683122, 1.000000000000000000, 0.9659258262890683122, 1.000000000000000000, 0.9659258262890683122, 1.000000000000000000, 0.9659258262890683122, 1.000000000000000000, 0.9659258262890683122, 1.000000000000000000, 0.9659258262890683122, 1.000000000000000000, 0.9659258262890683122, 1.000000000000000000, 0.9659258262890683122, 1.000000000000000000, 0.9659258262890683122, 1.000000000000000000, 0.9659258262890683122, 1.000000000000000000, 0.9659258262890683122, 1.000000000000000000, 0.9659258262890683122, 1.000000000000000000, 0.9659258262890683122, 1.000000000000000000, 0.9659258262890683122, 1.000000000000000000, 0.9659258262890683122, 1.000000000000000000, 0.9659258262890683122, 1.000000000000000000, 0.9659258262890683122, 1.000000000000000000, 0.9659258262890683122, 1.000000000000000000, 0.9659258262890683122, 1.000000000000000000, 0.9659258262890683122, 1.000000000000000000, 0.9659258262890683122, 1.000000000000000000, 0.9659258262890683122, 1.000000000000000000, 0.9659258262890683122, 1.000000000000000000, 0.9659258262890683122, 1.000000000000000000, 0.9659258262890683122, 1.000000000000000000, 0.9659258262890683122, 1.000000000000000000, 0.9659258262890683122, 1.000000000000000000, 0.9659258262890683122, 1.000000000000000000, 0.9659258262890683122, 1.000000000000000000, 0.9659258262890683122, 1.000000000000000000, 0.9659258262890683122, 1.000000000000000000, 0.9659258262890683122, 1.000000000000000000, 0.9659258262890683122, 1.000000000000000000, 0.9659258262890683122, 1.000000000000000000, 0.9659258262890683122, 1.000000000000000000, 0.9659258262890683122, 1.000000000000000000, 0.9659258262890683122, 1.000000000000000000, 0.9659258262890683122, 1.000000000000000000, 0.9659258262890683122, 1.000000000000000000, 0.9659258262890683122, 1.000000000000000000, 0.9659258262890683122, 1.000000000000000000, 0.9659258262890683122, 1.000000000000000000, 0.9659258262890683122, 1.000000000000000000, 0.9659258262890683122, 1.000000000000000000, 0.9659258262890683122, 1.000000000000000000, 0.9659258262890683122, 1.000000000000000000, 0.9659258262890683122, 1.000000000000000000, 0.9659258262890683122, 1.000000000000000000, 0.9659258262890683122, 1.000000000000000000, 0.9659258262890683122, 1.000000000000000000, 0.9659258262890683122, 1.000000000000000000, 0.9659258262890683122, 1.000000000000000000, 0.9659258262890683122, 1.000000000000000000, 0.9659258262890683122, 1.000000000000000000, 0.9659258262890683122, 1.000000000000000000, 0.9659258262890683122, 1.000000000000000000, 0.9659258262890683122, 1.000000000000000000, 0.9659258262890683122, 1.000000000000000000, 0.9659258262890683122, 1.000000000000000000, 0.9659258262890683122, 1.000000000000000000, 0.9659258262890683122, 1.000000000000000000, 0.9659258262890683122, 1.000000000000000000, 0.9659258262890683122, 1.000000000000000000, 0.9659258262890683122, 1.000000000000000000, 0.9659258262890683122, 1.000000000000000000, 0.9659258262890683122, 1.000000000000000000, 0.9659258262890683122, 1.000000000000000000, 0.9659258262890683122, 1.000000000000000000, 0.9659258262890683122, 1.000000000000000000, 0.9659258262890683122, 1.000000000000000000, 0.9659258262890683122, 1.000000000000000000, 0.9659258262890683122, 1.000000000000000000, 0.9659258262890683122, 1.000000000000000000, 0.9659258262890683122, 1.000000000000000000, 0.9659258262890683122, 1.000000000000000000, 0.9659258262890683122, 1.000000000000000000, 0.9659258262890683122, 1.000000000000000000, 0.9659258262890683122, 1.000000000000000000, 0.9659258262890683122, 1.000000000000000000, 0.9659258262890683122, 1.000000000000000000, 0.9659258262890683122, 1.000000000000000000, 0.9659258262890683122, 1.000000000000000000, 0.9659258262890683122, 1.000000000000000000, 0.9659258262890683122, 1.000000000000000000, 0.9659258262890683122, 1.000000000000000000, 0.9659258262890683122, 1.000000000000000000, 0.9659258262890683122, 1.000000000000000000, 0.9659258262890683122, 1.000000000000000000, 0.9659258262890683122, 1.000000000000000000, 0.9659258262890683122, 1.000000000000000000),
 ( 1.000000000000000000, 0.9659258262890683122, 1.000000000000000000, 0.9659258262890683122, 1.000000000000000000, 0.9659258262890683122, 1.000000000000000000, 0.9659258262890683122, 1.000000000000000000, 0.9659258262890683122, 1.000000000000000000, 0.9659258262890683122, 1.000000000000000000, 0.9659258262890683122, 1.000000000000000000, 0.9659258262890683122, 1.000000000000000000, 0.9659258262890683122, 1.000000000000000000, 0.9659258262890683122, 1.000000000000000000, 0.9659258262890683122, 1.000000000000000000, 0.9659258262890683122, 1.000000000000000000, 0.9659258262890683122, 1.000000000000000000, 0.9659258262890683122, 1.000000000000000000, 0.9659258262890683122, 1.000000000000000000, 0.9659258262890683122, 1.000000000000000000, 0.9659258262890683122, 1.000000000000000000, 0.9659258262890683122, 1.000000000000000000, 0.9659258262890683122, 1.000000000000000000, 0.9659258262890683122, 1.000000000000000000, 0.9659258262890683122, 1.000000000000000000, 0.9659258262890683122, 1.000000000000000000, 0.9659258262890683122, 1.000000000000000000, 0.9659258262890683122, 1.000000000000000000, 0.9659258262890683122, 1.000000000000000000, 0.9659258262890683122, 1.000000000000000000, 0.9659258262890683122, 1.000000000000000000, 0.9659258262890683122, 1.000000000000000000, 0.9659258262890683122, 1.000000000000000000, 0.9659258262890683122, 1.000000000000000000, 0.9659258262890683122, 1.000000000000000000, 0.9659258262890683122, 1.000000000000000000, 0.9659258262890683122, 1.000000000000000000, 0.9659258262890683122, 1.000000000000000000, 0.9659258262890683122, 1.000000000000000000, 0.9659258262890683122, 1.000000000000000000, 0.9659258262890683122, 1.000000000000000000, 0.9659258262890683122, 1.000000000000000000, 0.9659258262890683122, 1.000000000000000000, 0.9659258262890683122, 1.000000000000000000, 0.9659258262890683122, 1.000000000000000000, 0.9659258262890683122, 1.000000000000000000, 0.9659258262890683122, 1.000000000000000000, 0.9659258262890683122, 1.000000000000000000, 0.9659258262890683122, 1.000000000000000000, 0.9659258262890683122, 1.000000000000000000, 0.9659258262890683122, 1.000000000000000000, 0.9659258262890683122, 1.000000000000000000, 0.9659258262890683122, 1.000000000000000000, 0.9659258262890683122, 1.000000000000000000, 0.9659258262890683122, 1.000000000000000000, 0.9659258262890683122, 1.000000000000000000, 0.9659258262890683122, 1.000000000000000000, 0.9659258262890683122, 1.000000000000000000, 0.9659258262890683122, 1.000000000000000000, 0.9659258262890683122, 1.000000000000000000, 0.9659258262890683122, 1.000000000000000000, 0.9659258262890683122, 1.000000000000000000, 0.9659258262890683122, 1.000000000000000000, 0.9659258262890683122, 1.000000000000000000, 0.9659258262890683122, 1.000000000000000000, 0.9659258262890683122, 1.000000000000000000, 0.9659258262890683122, 1.000000000000000000, 0.9659258262890683122, 1.000000000000000000, 0.9659258262890683122, 1.000000000000000000, 0.9659258262890683122, 1.000000000000000000, 0.9659258262890683122, 1.000000000000000000, 0.9659258262890683122, 1.000000000000000000, 0.9659258262890683122, 1.000000000000000000, 0.9659258262890683122, 1.000000000000000000, 0.9659258262890683122, 1.000000000000000000, 0.9659258262890683122, 1.000000000000000000, 0.9659258262890683122, 1.000000000000000000, 0.9659258262890683122, 1.000000000000000000, 0.9659258262890683122, 1.000000000000000000, 0.9659258262890683122, 1.000000000000000000, 0.9659258262890683122, 1.000000000000000000, 0.9659258262890683122, 1.000000000000000000, 0.9659258262890683122, 1.000000000000000000, 0.9659258262890683122, 1.000000000000000000, 0.9659258262890683122, 1.000000000000000000, 0.9659258262890683122, 1.000000000000000000, 0.9659258262890683122, 1.000000000000000000, 0.9659258262890683122, 1.000000000000000000, 0.9659258262890683122, 1.000000000000000000, 0.9659258262890683122, 1.000000000000000000, 0.9659258262890683122, 1.000000000000000000, 0.9659258262890683122, 1.000000000000000000, 0.9659258262890683122, 1.000000000000000000, 0.9659258262890683122, 1.000000000000000000, 0.9659258262890683122, 1.000000000000000000, 0.9659258262890683122, 1.000000000000000000, 0.9659258262890683122, 1.000000000000000000, 0.9659258262890683122, 1.000000000000000000, 0.9659258262890683122, 1.000000000000000000, 0.9659258262890683122, 1.000000000000000000, 0.9659258262890683122, 1.000000000000000000, 0.9659258262890683122, 1.000000000000000000, 0.9659258262890683122, 1.000000000000000000, 0.9659258262890683122, 1.000000000000000000, 0.9659258262890683122, 1.000000000000000000, 0.9659258262890683122, 1.000000000000000000, 0.9659258262890683122, 1.000000000000000000, 0.9659258262890683122, 1.000000000000000000, 0.9659258262890683122, 1.000000000000000000, 0.9659258262890683122, 1.000000000000000000, 0.9659258262890683122, 1.000000000000000000, 0.9659258262890683122, 1.000000000000000000, 0.9659258262890683122, 1.000000000000000000, 0.9659258262890683122, 1.000000000000000000, 0.9659258262890683122, 1.000000000000000000, 0.9659258262890683122, 1.000000000000000000, 0.9659258262890683122, 1.000000000000000000, 0.9659258262890683122, 1.000000000000000000, 0.9659258262890683122, 1.000000000000000000, 0.9659258262890683122, 1.000000000000000000, 0.9659258262890683122, 1.000000000000000000, 0.9659258262890683122, 1.000000000000000000, 0.9659258262890683122, 1.000000000000000000, 0.9659258262890683122, 1.000000000000000000, 0.9659258262890683122, 1.000000000000000000, 0.9659258262890683122, 1.000000000000000000, 0.9659258262890683122, 1.000000000000000000, 0.9659258262890683122, 1.000000000000000000, 0.9659258262890683122, 1.000000000000000000, 0.9659258262890683122, 1.000000000000000000, 0.9659258262890683122, 1.000000000000000000, 0.9659258262890683122, 1.000000000000000000, 0.9659258262890683122, 1.000000000000000000, 0.9659258262890683122, 1.000000000000000000, 0.9659258262890683122, 1.000000000000000000, 0.9659258262890683122, 1.000000000000000000, 0.9659258262890683122, 1.000000000000000000, 0.9659258262890683122, 1.000000000000000000, 0.9659258262890683122, 1.000000000000000000, 0.9659258262890683122, 1.000000000000000000, 0.9659258262890683122, 1.000000000000000000, 0.9659258262890683122, 1.000000000000000000, 0.9659258262890683122, 1.000000000000000000, 0.9659258262890683122, 1.000000000000000000, 0.9659258262890683122, 1.000000000000000000, 0.9659258262890683122, 1.000000000000000000, 0.9659258262890683122, 1.000000000000000000, 0.9659258262890683122, 1.000000000000000000, 0.9659258262890683122, 1.000000000000000000, 0.9659258262890683122, 1.000000000000000000, 0.9659258262890683122, 1.000000000000000000, 0.9659258262890683122, 1.000000000000000000, 0.9659258262890683122, 1.000000000000000000, 0.9659258262890683122, 1.000000000000000000, 0.9659258262890683122, 1.000000000000000000, 0.9659258262890683122, 1.000000000000000000, 0.9659258262890683122, 1.000000000000000000, 0.9659258262890683122, 1.000000000000000000, 0.9659258262890683122, 1.000000000000000000, 0.9659258262890683122, 1.000000000000000000, 0.9659258262890683122, 1.000000000000000000, 0.9659258262890683122, 1.000000000000000000, 0.9659258262890683122, 1.000000000000000000, 0.9659258262890683122, 1.000000000000000000, 0.9659258262890683122, 1.000000000000000000, 0.9659258262890683122, 1.000000000000000000) ) ) 
 REPRESENTATION_ITEM ( '' )  SURFACE ( )  );
#10530 = CARTESIAN_POINT ( 'NONE',  ( 10.00000000000000178, 65.37363466993042493, 12.81628187352647608 ) ) ;
#10531 = CARTESIAN_POINT ( 'NONE',  ( -2.266590686148945544, 6.387082168247300906, -7.082119434687050408 ) ) ;
#10532 = CARTESIAN_POINT ( 'NONE',  ( -2.266590686148945544, 36.38708216824730357, -7.082119434687050408 ) ) ;
#10533 = DIRECTION ( 'NONE',  ( 0.9799247046208268141, 0.000000000000000000, 0.1993679344172108459 ) ) ;
#10534 = CARTESIAN_POINT ( 'NONE',  ( -0.3689425029237898834, 1.178748834913967869, -10.36894250292378850 ) ) ;
#10535 = CARTESIAN_POINT ( 'NONE',  ( 15.44008868035555260, 19.73035201082150536, 9.422509992056143702 ) ) ;
#10536 = FACE_OUTER_BOUND ( 'NONE', #14421, .T. ) ;
#10537 = ORIENTED_EDGE ( 'NONE', *, *, #42020, .F. ) ;
#10538 = CARTESIAN_POINT ( 'NONE',  ( 17.20831665107776587, 22.88393115100078745, 7.208316651077764980 ) ) ;
#10539 = CARTESIAN_POINT ( 'NONE',  ( 7.361572987183170547, 17.05059781766745530, 9.846743663894590881 ) ) ;
#10540 = CARTESIAN_POINT ( 'NONE',  ( 22.81628187352647785, 46.41530133659708213, 3.434112377981063169 ) ) ;
#10541 = CARTESIAN_POINT ( 'NONE',  ( 7.361572987183170547, 32.05059781766745175, 9.846743663894590881 ) ) ;
#10542 = DIRECTION ( 'NONE',  ( 0.000000000000000000, 1.000000000000000000, 0.000000000000000000 ) ) ;
#10543 = CARTESIAN_POINT ( 'NONE',  ( 17.96484262340118221, 56.18868534415484817, -7.964842623401177768 ) ) ;
#10544 = CARTESIAN_POINT ( 'NONE',  ( -1.099225684535947600, 23.70696800326375708, -6.408140936763238038 ) ) ;
#10545 = CARTESIAN_POINT ( 'NONE',  ( 14.16423886937410259, -30.69625116508602858, -2.602085213965210642E-15 ) ) ;
#10546 = CARTESIAN_POINT ( 'NONE',  ( 5.076628168052704559, 20.17559781766745175, -8.527530157486179263 ) ) ;
#10547 = AXIS2_PLACEMENT_3D ( 'NONE', #11908, #32436, #62936 ) ;
#10548 = CARTESIAN_POINT ( 'NONE',  ( 20.36894250292379738, 14.92874883491396432, -10.36894250292379027 ) ) ;
#10549 = EDGE_LOOP ( 'NONE', ( #54737, #91566, #78747, #96781, #2068, #21875 ) ) ;
#10550 = CARTESIAN_POINT ( 'NONE',  ( 17.96484262340118221, 36.18868534415484106, -7.964842623401177768 ) ) ;
#10551 = CARTESIAN_POINT ( 'NONE',  ( 20.36894250292379738, 34.92874883491396076, -10.36894250292379027 ) ) ;
#10552 = CARTESIAN_POINT ( 'NONE',  ( 10.00000000000000000, 54.75893115100078745, -9.846743663894594434 ) ) ;
#10553 = CARTESIAN_POINT ( 'NONE',  ( 10.00000000000000178, 7.258931151000785675, 9.846743663894594434 ) ) ;
#10555 = CARTESIAN_POINT ( 'NONE',  ( -5.795997163829992083, -0.03417435944610275333, -13.01802277140713926 ) ) ;
#10554 = CARTESIAN_POINT ( 'NONE',  ( 10.00000000000000000, 47.87363466993042493, -12.81628187352647608 ) ) ;
#10556 = CARTESIAN_POINT ( 'NONE',  ( 20.88017736071110519, 40.56368534415484106, 2.639326808657452039E-16 ) ) ;
#10557 = CARTESIAN_POINT ( 'NONE',  ( 7.595945211628243321, 4.245086020036709294E-16, 12.35117874301647056 ) ) ;
#10558 = ADVANCED_FACE ( 'NONE', ( #73297 ), #34296, .T. ) ;
#10559 = CARTESIAN_POINT ( 'NONE',  ( 0.6178305044545818747, 23.49863466993041783, -9.382169495545419124 ) ) ;
#10560 = CARTESIAN_POINT ( 'NONE',  ( 17.20831665107776587, 44.13393115100078745, -7.208316651077762316 ) ) ;
#10561 = CARTESIAN_POINT ( 'NONE',  ( -10.88017736071110164, 7.855352010821508024, -2.915334737309917212 ) ) ;
#10562 = LINE ( 'NONE', #72042, #61207 ) ;
#10564 = CARTESIAN_POINT ( 'NONE',  ( -11.01424773205765817, -93.41215259629041157, -4.000000000000000888 ) ) ;
#10563 = DIRECTION ( 'NONE',  ( -0.000000000000000000, -0.000000000000000000, -1.000000000000000000 ) ) ;
#10565 = VECTOR ( 'NONE', #17594, 1000.000000000000000 ) ;
#10566 = CIRCLE ( 'NONE', #66444, 3.940000000000000835 ) ;
#10567 = EDGE_CURVE ( 'NONE', #79224, #4697, #13584, .T. ) ;
#10568 = FACE_OUTER_BOUND ( 'NONE', #83860, .T. ) ;
#10569 = CARTESIAN_POINT ( 'NONE',  ( 5.056330833731659702, 4.503963689120695453E-16, 13.58983143750703348 ) ) ;
#10570 = CARTESIAN_POINT ( 'NONE',  ( 17.96484262340118221, 54.93868534415484106, 7.964842623401181321 ) ) ;
#10571 = CARTESIAN_POINT ( 'NONE',  ( 19.42250999205614548, 60.98035201082151247, -5.440088680355545492 ) ) ;
#10572 = LINE ( 'NONE', #3088, #10565 ) ;
#10573 = CARTESIAN_POINT ( 'NONE',  ( 11.24699797944280100, 54.09857164847241506, 0.000000000000000000 ) ) ;
#10574 = CARTESIAN_POINT ( 'NONE',  ( -0.8801773607111009756, 28.06368534415484106, 1.068504757029289695E-15 ) ) ;
#10575 = CARTESIAN_POINT ( 'NONE',  ( -2.816281873526471635, -1.084698663402913210, -3.434112377981056508 ) ) ;
#10577 = CARTESIAN_POINT ( 'NONE',  ( 18.95785429995050464, 37.24216108172004880, 6.499999999999924505 ) ) ;
#10576 = CARTESIAN_POINT ( 'NONE',  ( 7.084665262690076126, 24.10535201082150181, 10.88017736071109987 ) ) ;
#10578 = FACE_OUTER_BOUND ( 'NONE', #96129, .T. ) ;
#10579 = CARTESIAN_POINT ( 'NONE',  ( 16.40814093676323893, 20.79030133659708923, 11.09922568453595026 ) ) ;
#10580 = ORIENTED_EDGE ( 'NONE', *, *, #74756, .F. ) ;
#10581 = CARTESIAN_POINT ( 'NONE',  ( 0.5774900079438590739, 57.64701867748817676, -5.440088680355550821 ) ) ;
#10582 = CARTESIAN_POINT ( 'NONE',  ( 0.1532563361054083140, 36.00893115100078745, 1.131784320476157264E-15 ) ) ;
#10584 = CARTESIAN_POINT ( 'NONE',  ( 20.03743638938529159, 51.75197528031018379, 6.399506433553905360 ) ) ;
#10583 = CARTESIAN_POINT ( 'NONE',  ( 3.591859063236761518, 19.95696800326375353, 11.09922568453594849 ) ) ;
#10585 = CARTESIAN_POINT ( 'NONE',  ( 12.91533473730992121, 34.52201867748817676, 10.88017736071110164 ) ) ;
#10586 = CARTESIAN_POINT ( 'NONE',  ( 22.26659068614895176, 54.72041550158063217, -7.082119434687042414 ) ) ;
#10587 = CARTESIAN_POINT ( 'NONE',  ( 5.076628168052704559, 35.17559781766745175, -8.527530157486179263 ) ) ;
#10588 = CARTESIAN_POINT ( 'NONE',  ( 12.91533473730993009, 61.60535201082150536, -10.88017736071109987 ) ) ;
#10589 = CARTESIAN_POINT ( 'NONE',  ( 12.91533473730992121, 49.52201867748817676, 10.88017736071110164 ) ) ;
#10590 = CARTESIAN_POINT ( 'NONE',  ( 12.98685442714197791, 15.00000000000000000, -6.449155920600934344 ) ) ;
#10591 = CARTESIAN_POINT ( 'NONE',  ( 10.00000000000000000, 10.55374883491396787, -14.16423886937410082 ) ) ;
#10592 = CIRCLE ( 'NONE', #87233, 15.00000000000000000 ) ;
#10593 = FILL_AREA_STYLE_COLOUR ( '', #94402 ) ;
#10594 = CARTESIAN_POINT ( 'NONE',  ( 7.361572987183170547, 67.05059781766746596, 9.846743663894590881 ) ) ;
#10595 = AXIS2_PLACEMENT_3D ( 'NONE', #92312, #70812, #17315 ) ;
#10596 = CIRCLE ( 'NONE', #69689, 0.5000000000000041078 ) ;
#10597 = VERTEX_POINT ( 'NONE', #29277 ) ;
#10598 = CARTESIAN_POINT ( 'NONE',  ( 20.36894250292379738, 49.92874883491396787, -10.36894250292379027 ) ) ;
#10599 = CARTESIAN_POINT ( 'NONE',  ( 10.00000000000000000, 50.55374883491396787, -14.16423886937410082 ) ) ;
#10600 = CARTESIAN_POINT ( 'NONE',  ( 17.20831665107776587, 12.88393115100078390, 7.208316651077764980 ) ) ;
#10601 = CARTESIAN_POINT ( 'NONE',  ( 13.43411237798106583, 12.66530133659708746, -12.81628187352647252 ) ) ;
#10602 = CARTESIAN_POINT ( 'NONE',  ( -13.34397673082797020, 90.99712473415623037, 7.994997298710761591 ) ) ;
#10603 = CARTESIAN_POINT ( 'NONE',  ( 19.88565890683627657, 52.71691075486304356, -6.480892540919849232 ) ) ;
#10605 = CARTESIAN_POINT ( 'NONE',  ( 10.00000000000000000, 32.87363466993042493, -12.81628187352647608 ) ) ;
#10604 = CARTESIAN_POINT ( 'NONE',  ( 4.559911319644449179, 68.89701867748817676, 9.422509992056141925 ) ) ;
#10606 = CARTESIAN_POINT ( 'NONE',  ( 20.36894250292379382, 38.67874883491396076, 10.36894250292379205 ) ) ;
#10607 = VECTOR ( 'NONE', #95232, 1000.000000000000000 ) ;
#10608 = FILL_AREA_STYLE_COLOUR ( '', #22051 ) ;
#10609 = CARTESIAN_POINT ( 'NONE',  ( 4.559911319644449179, 68.89701867748817676, 9.422509992056141925 ) ) ;
#10610 = B_SPLINE_CURVE_WITH_KNOTS ( 'NONE', 3,
 ( #48147, #3159, #42144, #87126 ),
 .UNSPECIFIED., .F., .F.,
 ( 4, 4 ),
 ( 1.453963218420191702E-17, 0.001060528352561989837 ),
 .UNSPECIFIED. ) ;
#10611 = CARTESIAN_POINT ( 'NONE',  ( 9.846743663894590881, 8.717264484334116048, -2.638427012816833894 ) ) ;
#10612 = ORIENTED_EDGE ( 'NONE', *, *, #71373, .T. ) ;
#10613 = DIRECTION ( 'NONE',  ( 0.000000000000000000, 0.000000000000000000, -1.000000000000000000 ) ) ;
#10614 = CARTESIAN_POINT ( 'NONE',  ( 1.472469842513823179, 21.42559781766745175, 4.923371831947296329 ) ) ;
#10615 = FACE_OUTER_BOUND ( 'NONE', #87677, .T. ) ;
#10616 = ORIENTED_EDGE ( 'NONE', *, *, #50019, .T. ) ;
#10617 = CARTESIAN_POINT ( 'NONE',  ( 17.08211943468705130, 8.470415501580635720, 12.26659068614894998 ) ) ;
#10619 = CARTESIAN_POINT ( 'NONE',  ( 10.00000000000000178, 14.31368534415483929, 10.88017736071110342 ) ) ;
#10618 = CARTESIAN_POINT ( 'NONE',  ( 19.42250999205614193, 5.147018677488171434, 5.440088680355555262 ) ) ;
#10621 = CARTESIAN_POINT ( 'NONE',  ( 3.591859063236761518, 4.956968003263753531, 11.09922568453594849 ) ) ;
#10620 = CARTESIAN_POINT ( 'NONE',  ( 2.791683348922240793, 36.63393115100078035, 7.208316651077764092 ) ) ;
#10622 = DIRECTION ( 'NONE',  ( 1.000000000000000000, 0.000000000000000000, 0.000000000000000000 ) ) ;
#10623 = EDGE_CURVE ( 'NONE', #22589, #16383, #13792, .T. ) ;
#10624 = CIRCLE ( 'NONE', #23411, 4.250000000000001776 ) ;
#10625 = TOROIDAL_SURFACE ( 'NONE', #12244, 7.250000000000002665, 0.2500000000000000000 ) ;
#10626 = TOROIDAL_SURFACE ( 'NONE', #5837, 1.750000000000000888, 0.2500000000000000000 ) ;
#10627 = CARTESIAN_POINT ( 'NONE',  ( -2.816281873526471635, 13.91530133659708746, -3.434112377981056508 ) ) ;
#10628 = ORIENTED_EDGE ( 'NONE', *, *, #77317, .T. ) ;
#10629 = CARTESIAN_POINT ( 'NONE',  ( 24.16423886937409904, 44.09541550158063927, 3.795296366450317205 ) ) ;
#10630 = ORIENTED_EDGE ( 'NONE', *, *, #35460, .F. ) ;
#10631 = CARTESIAN_POINT ( 'NONE',  ( 13.79529636645030344, 53.26208216824730357, 14.16423886937410614 ) ) ;
#10632 = ORIENTED_EDGE ( 'NONE', *, *, #69001, .T. ) ;
#10633 = CARTESIAN_POINT ( 'NONE',  ( 7.084665262690076126, 32.02201867748816966, -10.88017736071110164 ) ) ;
#10634 = CARTESIAN_POINT ( 'NONE',  ( 20.88017736071110875, 40.77201867748818387, -2.915334737309920765 ) ) ;
#10635 = CARTESIAN_POINT ( 'NONE',  ( -0.8801773607110991993, 62.85535201082150536, -2.915334737309923874 ) ) ;
#10636 = CARTESIAN_POINT ( 'NONE',  ( 7.084665262690076126, 29.10535201082150181, 10.88017736071109987 ) ) ;
#10637 = CARTESIAN_POINT ( 'NONE',  ( 0.1922240491738455848, 33.18878173731742010, 6.499999999999968914 ) ) ;
#10638 = ADVANCED_FACE ( 'NONE', ( #67786 ), #31131, .T. ) ;
#10639 = CARTESIAN_POINT ( 'NONE',  ( 2.791683348922240793, 16.63393115100078745, 7.208316651077764092 ) ) ;
#10640 = FACE_OUTER_BOUND ( 'NONE', #9048, .T. ) ;
#10641 = ORIENTED_EDGE ( 'NONE', *, *, #4975, .F. ) ;
#10642 = CARTESIAN_POINT ( 'NONE',  ( 10.93736952808811047, -97.13260119838979278, 3.750000000000000000 ) ) ;
#10643 = CARTESIAN_POINT ( 'NONE',  ( 18.52753015748617571, 48.09226448433412315, 4.923371831947298993 ) ) ;
#10644 = PLANE ( 'NONE',  #18117 ) ;
#10645 = CARTESIAN_POINT ( 'NONE',  ( 21.09922568453595559, 47.04030133659708923, -6.408140936763230044 ) ) ;
#10646 = EDGE_CURVE ( 'NONE', #15318, #11601, #97815, .T. ) ;
#10647 = ORIENTED_EDGE ( 'NONE', *, *, #10058, .T. ) ;
#10648 = CARTESIAN_POINT ( 'NONE',  ( 18.95785429995060767, 22.24216108172003459, 6.499999999999853451 ) ) ;
#10649 = CARTESIAN_POINT ( 'NONE',  ( 14.82269085861168811, 15.00000000000000000, -2.299529454046961519 ) ) ;
#10650 = CARTESIAN_POINT ( 'NONE',  ( 12.63842701281683034, 62.46726448433410894, 9.846743663894596210 ) ) ;
#10651 = CARTESIAN_POINT ( 'NONE',  ( 6.204703633549690345, 50.76208216824730357, -14.16423886937410259 ) ) ;
#10652 = DIRECTION ( 'NONE',  ( 1.000000000000000000, 0.000000000000000000, 0.000000000000000000 ) ) ;
#10653 = ORIENTED_EDGE ( 'NONE', *, *, #61201, .T. ) ;
#10654 = CARTESIAN_POINT ( 'NONE',  ( 14.42525372082709012, 14.76984920709442051, 3.890283033989281769 ) ) ;
#10655 = CARTESIAN_POINT ( 'NONE',  ( 10.00000000000000178, 37.25893115100078745, 9.846743663894594434 ) ) ;
#10657 = AXIS2_PLACEMENT_3D ( 'NONE', #76337, #7853, #75845 ) ;
#10656 = CARTESIAN_POINT ( 'NONE',  ( 6.565887622018943937, 63.08196800326376064, -12.81628187352647608 ) ) ;
#10658 = CARTESIAN_POINT ( 'NONE',  ( -2.816281873526473856, 9.331968003263753531, 3.434112377981055619 ) ) ;
#10659 = CARTESIAN_POINT ( 'NONE',  ( 20.88017736071110875, 60.77201867748817676, -2.915334737309920765 ) ) ;
#10660 = DIRECTION ( 'NONE',  ( 0.9426414910921783186, 0.000000000000000000, -0.3338068592337714025 ) ) ;
#10661 = CIRCLE ( 'NONE', #23392, 2.999999999999999112 ) ;
#10662 = CARTESIAN_POINT ( 'NONE',  ( 2.791683348922240793, 61.63393115100079456, 7.208316651077764092 ) ) ;
#10663 = CARTESIAN_POINT ( 'NONE',  ( -11.92686044187656336, 7.870456701841145986, 3.195792623639540864 ) ) ;
#10664 = VECTOR ( 'NONE', #83581, 999.9999999999998863 ) ;
#10665 = ORIENTED_EDGE ( 'NONE', *, *, #20667, .F. ) ;
#10666 = CARTESIAN_POINT ( 'NONE',  ( 13.79529636645031943, 65.34541550158063217, -14.16423886937409904 ) ) ;
#10667 = DIRECTION ( 'NONE',  ( -0.000000000000000000, 0.000000000000000000, 1.000000000000000000 ) ) ;
#10668 = CARTESIAN_POINT ( 'NONE',  ( 20.88017736071110519, 40.56368534415484106, 2.639326808657452039E-16 ) ) ;
#10670 = CARTESIAN_POINT ( 'NONE',  ( 0.5774900079438607392, 68.48035201082150536, 5.440088680355550821 ) ) ;
#10669 = CARTESIAN_POINT ( 'NONE',  ( 22.81628187352647785, 16.41530133659708923, 3.434112377981063169 ) ) ;
#10671 = LINE ( 'NONE', #41185, #16923 ) ;
#10672 = CARTESIAN_POINT ( 'NONE',  ( -2.120353041430744323, 15.00000000000000000, 14.34413130794943925 ) ) ;
#10673 = CARTESIAN_POINT ( 'NONE',  ( -14.16722289976693894, 14.49999999999999112, 4.928467845925465163 ) ) ;
#10674 = CARTESIAN_POINT ( 'NONE',  ( 2.791683348922240793, 46.63393115100077324, 7.208316651077764092 ) ) ;
#10675 = CARTESIAN_POINT ( 'NONE',  ( 10.00000000000000178, 2.258931151000784787, 9.846743663894594434 ) ) ;
#10676 = CARTESIAN_POINT ( 'NONE',  ( -7.964842623401179544, -32.56131465584516604, -7.964842623401174215 ) ) ;
#10677 = CARTESIAN_POINT ( 'NONE',  ( 0.6178305044545818747, 3.498634669930420049, -9.382169495545419124 ) ) ;
#10679 = CARTESIAN_POINT ( 'NONE',  ( -3.750000000000000000, 0.000000000000000000, -2.500000000000000000 ) ) ;
#10678 = CARTESIAN_POINT ( 'NONE',  ( 17.96484262340118221, 21.18868534415483396, -7.964842623401177768 ) ) ;
#10680 = PRESENTATION_LAYER_ASSIGNMENT (  '', '', ( #79340 ) ) ;
#10681 = CARTESIAN_POINT ( 'NONE',  ( 17.08211943468705840, 30.13708216824730357, -12.26659068614894466 ) ) ;
#10682 = ADVANCED_FACE ( 'NONE', ( #52767 ), #54798, .T. ) ;
#10683 = CIRCLE ( 'NONE', #73047, 0.5000000000000004441 ) ;
#10684 = CARTESIAN_POINT ( 'NONE',  ( -4.164238869374099039, 31.80374883491396432, 8.674139862899312516E-16 ) ) ;
#10685 = CARTESIAN_POINT ( 'NONE',  ( 2.035157376598822676, 12.43868534415483751, -7.964842623401177768 ) ) ;
#10686 = CARTESIAN_POINT ( 'NONE',  ( 12.63842701281683922, 49.55059781766744464, -9.846743663894590881 ) ) ;
#10687 = VECTOR ( 'NONE', #94572, 1000.000000000000114 ) ;
#10688 = CARTESIAN_POINT ( 'NONE',  ( -2.816281873526473856, 44.12363466993042493, 9.499525473075851096E-16 ) ) ;
#10689 = CARTESIAN_POINT ( 'NONE',  ( 4.559911319644449179, 8.897018677488171434, 9.422509992056141925 ) ) ;
#10690 = ORIENTED_EDGE ( 'NONE', *, *, #90022, .T. ) ;
#10691 = CARTESIAN_POINT ( 'NONE',  ( 18.52753015748617571, 38.09226448433412315, 4.923371831947298993 ) ) ;
#10692 = STYLED_ITEM ( 'NONE', ( #65994 ), #38400 ) ;
#10693 = CARTESIAN_POINT ( 'NONE',  ( 7.084665262690076126, 42.02201867748816966, -10.88017736071110164 ) ) ;
#10694 = CARTESIAN_POINT ( 'NONE',  ( 16.40814093676324603, 12.45696800326375353, -11.09922568453594671 ) ) ;
#10696 = FACE_OUTER_BOUND ( 'NONE', #83160, .T. ) ;
#10695 = CARTESIAN_POINT ( 'NONE',  ( 24.16423886937409904, 19.09541550158063927, 3.795296366450317205 ) ) ;
#10697 = CARTESIAN_POINT ( 'NONE',  ( -13.74344568549552825, 14.76984872680916183, -5.860030649990871865 ) ) ;
#10698 = CARTESIAN_POINT ( 'NONE',  ( 1.472469842513823179, 20.59226448433411960, -4.923371831947296329 ) ) ;
#10699 = CARTESIAN_POINT ( 'NONE',  ( 21.09922568453595559, 47.04030133659708923, -6.408140936763230044 ) ) ;
#10700 = CARTESIAN_POINT ( 'NONE',  ( 12.63842701281683922, 49.55059781766744464, -9.846743663894590881 ) ) ;
#10701 = ORIENTED_EDGE ( 'NONE', *, *, #23783, .T. ) ;
#10702 = CARTESIAN_POINT ( 'NONE',  ( 8.880000000000000782, -0.01161165531298087583, -3.750000000000000000 ) ) ;
#10703 = CARTESIAN_POINT ( 'NONE',  ( -0.3689425029237898834, 66.17874883491396076, -10.36894250292378850 ) ) ;
#10704 = CARTESIAN_POINT ( 'NONE',  ( 20.36894250292379738, 4.928748834913967869, -10.36894250292379027 ) ) ;
#10705 = CARTESIAN_POINT ( 'NONE',  ( 7.361572987183169658, -0.03273551566588185635, -9.846743663894592657 ) ) ;
#10706 = CARTESIAN_POINT ( 'NONE',  ( 12.63842701281683922, 49.55059781766744464, -9.846743663894590881 ) ) ;
#10707 = CARTESIAN_POINT ( 'NONE',  ( 20.88017736071110164, 15.35535201082150358, 2.915334737309930979 ) ) ;
#10708 = DIRECTION ( 'NONE',  ( -0.000000000000000000, -0.000000000000000000, 1.000000000000000000 ) ) ;
#10709 = CARTESIAN_POINT ( 'NONE',  ( 18.72515096720609051, 25.05509018479941119, 6.499999999999470646 ) ) ;
#10710 = ORIENTED_EDGE ( 'NONE', *, *, #23751, .F. ) ;
#10711 = ORIENTED_EDGE ( 'NONE', *, *, #731, .F. ) ;
#10712 = ORIENTED_EDGE ( 'NONE', *, *, #32274, .T. ) ;
#10713 = CARTESIAN_POINT ( 'NONE',  ( 3.469446951953614189E-15, 9.171802177851546389, 11.25000000000000355 ) ) ;
#10714 = CARTESIAN_POINT ( 'NONE',  ( 20.36894250292379382, 8.678748834913967869, 10.36894250292379205 ) ) ;
#10715 = DIRECTION ( 'NONE',  ( 0.000000000000000000, 0.000000000000000000, 1.000000000000000000 ) ) ;
#10716 = CARTESIAN_POINT ( 'NONE',  ( 6.204703633549690345, 40.76208216824731778, -14.16423886937410259 ) ) ;
#10717 = CARTESIAN_POINT ( 'NONE',  ( 7.361572987183169658, 54.96726448433413026, -9.846743663894592657 ) ) ;
#10718 = CARTESIAN_POINT ( 'NONE',  ( 12.63842701281683922, 39.55059781766744464, -9.846743663894590881 ) ) ;
#10720 = CARTESIAN_POINT ( 'NONE',  ( 2.791683348922237240, 60.38393115100078745, -7.208316651077763204 ) ) ;
#10719 = CARTESIAN_POINT ( 'NONE',  ( 10.00000000000000000, 26.81368534415484106, -10.88017736071110342 ) ) ;
#10721 = CARTESIAN_POINT ( 'NONE',  ( 20.36894250292379738, 9.928748834913966093, -10.36894250292379027 ) ) ;
#10722 = CARTESIAN_POINT ( 'NONE',  ( 10.00000000000000178, 43.05374883491397497, 14.16423886937410082 ) ) ;
#10723 = CIRCLE ( 'NONE', #42697, 3.799999999999998934 ) ;
#10724 = CARTESIAN_POINT ( 'NONE',  ( 20.88017736071110519, 10.56368534415483929, 2.639326808657452039E-16 ) ) ;
#10725 = CARTESIAN_POINT ( 'NONE',  ( -4.096035146093346846, 4.802464241948007172E-16, -13.90943910019264429 ) ) ;
#10726 = EDGE_CURVE ( 'NONE', #52526, #10914, #21516, .T. ) ;
#10727 = DIRECTION ( 'NONE',  ( 0.000000000000000000, 0.000000000000000000, -1.000000000000000000 ) ) ;
#10728 = CARTESIAN_POINT ( 'NONE',  ( 7.084665262690076126, 64.10535201082150536, 10.88017736071109987 ) ) ;
#10729 = CARTESIAN_POINT ( 'NONE',  ( 10.00000000000000000, 24.75893115100078745, -9.846743663894594434 ) ) ;
#10730 = CARTESIAN_POINT ( 'NONE',  ( -6.581680125707231710, -88.31141629936868753, 2.750000000000000000 ) ) ;
#10731 = EDGE_LOOP ( 'NONE', ( #53157, #25749, #51971, #67230, #5826, #55023 ) ) ;
#10732 =( BOUNDED_SURFACE ( )  B_SPLINE_SURFACE ( 1, 2, ( 
 ( #74521, #51532, #98550, #90999, #44519, #38025, #67030, #36541, #53002, #45507, #21043, #75018, #21538, #60996, #20548, #59027, #51033, #22039, #37033, #6523, #89533, #15034, #67529, #90505, #22530, #45008, #52514, #14538, #82024, #75514, #48, #43528, #5554, #76007, #7534, #36031, #44018, #97060, #28533, #97552, #29014, #30990, #39503, #8986, #24006, #54478, #61489, #47476, #9483, #91994, #46981, #84009, #39986, #40487, #24504, #77976, #15533, #54966, #23525, #84988, #1018, #16504, #53997, #46492, #55483, #84504, #16004, #32473, #70488, #31478, #69992, #76991, #70985, #62467, #85488, #91508, #92972, #46014, #2008, #39007, #47960, #2507, #62968, #8504, #93473, #85984, #17495, #78470, #9984, #23027, #76503, #8017, #38514, #61981, #92481, #65419, #94940, #12425, #50424, #56940, #87442, #42931, #49934, #79939, #73412, #49435, #72429, #4940, #10955, #63464, #3955, #95444, #57435, #80442, #25963, #72927, #57920, #93965, #25491, #55976, #48948, #33439, #86477, #48460, #40978, #63936, #56464, #86950, #18463, #79456, #13922, #14917, #27914, #36416, #75389, #81904, #74399, #28417, #90884, #6398, #5922, #20432, #5443, #66412, #83397, #50919, #97428, #35420, #82898, #43414, #12917, #28894, #59399, #14417, #73914, #89902, #21418, #29390, #51415, #96944, #37419, #44399, #29884, #59892, #58912, #90382, #21920, #65914, #6907, #96444, #98429, #60386, #58407, #81415, #89411, #13413, #60881, #40233, #86225, #78721, #79206, #48702, #26210, #40724, #25249, #38396, #47724, #7901, #70741, #87193, #76386, #32712, #78222, #10716, #91381, #55221, #33205, #45900, #10231, #37913, #63699, #56224, #3222, #68898, #85735, #56703, #41233, #426, #71226, #63210, #15418, #17248, #18716, #7417, #9733, #2257, #33686, #68401, #32217, #18222, #30378, #22909, #62718, #86718, #25732, #93714, #55733, #93218, #83889, #94202, #24742, #21171, #4706, #72189, #81174, #27177, #36169, #28662, #58160, #49679, #42688, #43664, #12674, #89168, #35676, #35169, #43174, #41720, #88671, #57680, #89661, #81657, #73662, #64671, #73167, #5189, #66160, #20179, #59154, #51173, #79702, #96693, #72672, #13166, #50682, #28173, #58666, #19196, #74150, #65669, #96191, #20679, #3718, #11200, #50176, #5684, #27675, #65173, #66669, #97194, #34179, #95181, #26689, #57185, #34677, #11696, #87682, #80183, #42205, #4207, #88176, #95693, #19689, #80686, #12182, #37173, #75147, #45643, #51674, #97684, #82152, #14673, #90637, #60140, #29146, #22661, #98176, #83148, #37660, #75645, #45139, #22162, #59652, #52644, #15162, #44148, #13664, #29632, #60635, #7156, #82652, #53138, #68159, #21673, #98680 ),
 ( #6657, #30129, #90143, #91136, #74656, #83647, #6167, #36671, #44652, #67159, #52159, #14168, #67666, #12989, #65991, #50012, #50503, #66986, #42513, #35496, #12503, #82479, #42039, #80516, #72503, #43485, #58487, #27991, #12014, #6000, #96518, #81486, #28494, #66490, #73986, #88999, #72997, #20505, #59475, #4035, #21493, #43002, #51488, #50991, #4527, #43973, #5511, #34991, #35988, #19515, #97017, #58987, #73486, #5013, #65496, #89491, #21000, #96016, #81983, #34498, #13494, #89976, #74475, #36494, #64989, #97508, #27499, #28972, #20003, #51990, #57994, #88500, #95516, #81001, #27009, #57507, #88004, #22485, #75960, #75469, #92434, #7488, #45967, #54432, #37984, #6481, #76457, #60464, #69450, #61933, #91458, #82975, #68475, #76942, #7972, #23480, #68963, #1, #38471, #74976, #22984, #90952, #23958, #8451, #495, #98005, #30449, #30944, #61442, #53449, #13998, #84459, #44476, #91948, #6985, #38958, #83958, #53951, #969, #14495, #31430, #60949, #36986, #67483, #29458, #59966, #83469, #90459, #21995, #98504, #44966, #37489, #67978, #29958, #52958, #14990, #45461, #16944, #2945, #33394, #78420, #3423, #32423, #39937, #18417, #2458, #94897, #62924, #64386, #93920, #93425, #32915, #63892, #47428, #24947, #17448, #9936, #94406, #63415, #70439, #54921, #84941, #55431, #10915, #40440, #85937, #17929, #70941, #78915, #25446, #26394, #77424, #47914, #25919, #55929, #86428, #77928, #41438, #48412, #10426, #39456, #85435, #9435, #71899, #69946, #40933, #33882, #56422, #92924, #62420, #71431, #86907, #48902, #24455, #79416, #16452, #46931, #1958, #8938, #1466, #31920, #51371, #4897, #26895, #88386, #43368, #74348, #96896, #5875, #19885, #81858, #56895, #3913, #19397, #73867, #11401, #50376, #35378, #96397, #28375, #58864, #36370, #88879, #73370, #87880, #95903, #57389, #80885, #66864, #49884, #12383, #27384, #89368, #41923, #4413, #50879, #95394, #65870, #87400, #81372, #5397, #13369, #80396, #34880, #43854, #20879, #11898, #27873, #42888, #64870, #65374, #97383, #18916, #57874, #58359, #49392, #79893, #42400, #66360, #72385, #34382, #72878, #35871, #20388, #12869, #24574, #76564, #611, #55034, #24073, #84569, #17065, #31055, #7599, #77539, #8080, #47547, #78045, #61555, #92063, #9547, #16569, #16070, #91067, #23591, #39073, #53070, #69566, #38095, #62044, #92544, #9057, #39570, #30559, #70059, #1581, #32030, #62534, #68582, #53562, #113, #84076, #48026, #36978, #66481, #50985, #43965, #97009, #5993, #20994, #90452, #27493, #12982, #82471, #20497, #73980, #35489, #97998, #81975, #5505, #19994, #80993, #12496, #59960, #50496 ) ),
 .UNSPECIFIED., .F., .F., .F. ) 
 B_SPLINE_SURFACE_WITH_KNOTS ( ( 2, 2 ),
 ( 3, 2, 2, 2, 2, 2, 2, 2, 2, 2, 2, 2, 2, 2, 2, 2, 2, 2, 2, 2, 2, 2, 2, 2, 2, 2, 2, 2, 2, 2, 2, 2, 2, 2, 2, 2, 2, 2, 2, 2, 2, 2, 2, 2, 2, 2, 2, 2, 2, 2, 2, 2, 2, 2, 2, 2, 2, 2, 2, 2, 2, 2, 2, 2, 2, 2, 2, 2, 2, 2, 2, 2, 2, 2, 2, 2, 2, 2, 2, 2, 2, 2, 2, 2, 2, 2, 2, 2, 2, 2, 2, 2, 2, 2, 2, 2, 2, 2, 2, 2, 2, 2, 2, 2, 2, 2, 2, 2, 2, 2, 2, 2, 2, 2, 2, 2, 2, 2, 2, 2, 2, 2, 2, 2, 2, 2, 2, 2, 2, 2, 2, 2, 2, 2, 2, 2, 2, 2, 2, 2, 2, 2, 2, 2, 2, 2, 2, 2, 2, 2, 2, 2, 2, 2, 2, 2, 2, 2, 2, 2, 2, 2, 3 ),
 ( 0.000000000000000000, 1.000000000000000000 ),
 ( 0.000000000000000000, 0.005952380952380952051, 0.01190476190476190410, 0.01785714285714285615, 0.02380952380952380820, 0.02976190476190476025, 0.03571428571428571230, 0.04166666666666666435, 0.04761904761904761640, 0.05357142857142856845, 0.05952380952380952051, 0.06547619047619047949, 0.07142857142857142461, 0.07738095238095238360, 0.08333333333333332871, 0.08928571428571428770, 0.09523809523809523281, 0.1011904761904761918, 0.1071428571428571369, 0.1130952380952380959, 0.1190476190476190410, 0.1250000000000000000, 0.1309523809523809590, 0.1369047619047619180, 0.1428571428571428492, 0.1488095238095238082, 0.1547619047619047672, 0.1607142857142857262, 0.1666666666666666574, 0.1726190476190476164, 0.1785714285714285754, 0.1845238095238095344, 0.1904761904761904656, 0.1964285714285714246, 0.2023809523809523836, 0.2083333333333333426, 0.2142857142857142738, 0.2202380952380952328, 0.2261904761904761918, 0.2321428571428571508, 0.2380952380952380820, 0.2440476190476190410, 0.2500000000000000000, 0.2559523809523809312, 0.2619047619047619180, 0.2678571428571428492, 0.2738095238095238360, 0.2797619047619047672, 0.2857142857142856984, 0.2916666666666666852, 0.2976190476190476164, 0.3035714285714285476, 0.3095238095238095344, 0.3154761904761904656, 0.3214285714285714524, 0.3273809523809523836, 0.3333333333333333148, 0.3392857142857143016, 0.3452380952380952328, 0.3511904761904761640, 0.3571428571428571508, 0.3630952380952380820, 0.3690476190476190688, 0.3750000000000000000, 0.3809523809523809312, 0.3869047619047619180, 0.3928571428571428492, 0.3988095238095238360, 0.4047619047619047672, 0.4107142857142856984, 0.4166666666666666852, 0.4226190476190476164, 0.4285714285714285476, 0.4345238095238095344, 0.4404761904761904656, 0.4464285714285714524, 0.4523809523809523836, 0.4583333333333333148, 0.4642857142857143016, 0.4702380952380952328, 0.4761904761904761640, 0.4821428571428571508, 0.4880952380952380820, 0.4940476190476190688, 0.5000000000000000000, 0.5059523809523809312, 0.5119047619047618625, 0.5178571428571429047, 0.5238095238095238360, 0.5297619047619047672, 0.5357142857142856984, 0.5416666666666666297, 0.5476190476190476719, 0.5535714285714286031, 0.5595238095238095344, 0.5654761904761904656, 0.5714285714285713969, 0.5773809523809523281, 0.5833333333333333703, 0.5892857142857143016, 0.5952380952380952328, 0.6011904761904761640, 0.6071428571428570953, 0.6130952380952381375, 0.6190476190476190688, 0.6250000000000000000, 0.6309523809523809312, 0.6369047619047618625, 0.6428571428571429047, 0.6488095238095238360, 0.6547619047619047672, 0.6607142857142856984, 0.6666666666666666297, 0.6726190476190476719, 0.6785714285714286031, 0.6845238095238095344, 0.6904761904761904656, 0.6964285714285713969, 0.7023809523809523281, 0.7083333333333333703, 0.7142857142857143016, 0.7202380952380952328, 0.7261904761904761640, 0.7321428571428570953, 0.7380952380952381375, 0.7440476190476190688, 0.7500000000000000000, 0.7559523809523809312, 0.7619047619047618625, 0.7678571428571429047, 0.7738095238095238360, 0.7797619047619047672, 0.7857142857142856984, 0.7916666666666666297, 0.7976190476190476719, 0.8035714285714286031, 0.8095238095238095344, 0.8154761904761904656, 0.8214285714285713969, 0.8273809523809523281, 0.8333333333333333703, 0.8392857142857143016, 0.8452380952380952328, 0.8511904761904761640, 0.8571428571428570953, 0.8630952380952381375, 0.8690476190476190688, 0.8750000000000000000, 0.8809523809523809312, 0.8869047619047618625, 0.8928571428571429047, 0.8988095238095238360, 0.9047619047619047672, 0.9107142857142856984, 0.9166666666666666297, 0.9226190476190476719, 0.9285714285714286031, 0.9345238095238095344, 0.9404761904761904656, 0.9464285714285713969, 0.9523809523809523281, 0.9583333333333333703, 0.9642857142857143016 ),
 .UNSPECIFIED. ) 
 GEOMETRIC_REPRESENTATION_ITEM ( )  RATIONAL_B_SPLINE_SURFACE ( (
 ( 1.000000000000000000, 0.9659258262890683122, 1.000000000000000000, 0.9659258262890683122, 1.000000000000000000, 0.9659258262890683122, 1.000000000000000000, 0.9659258262890683122, 1.000000000000000000, 0.9659258262890683122, 1.000000000000000000, 0.9659258262890683122, 1.000000000000000000, 0.9659258262890683122, 1.000000000000000000, 0.9659258262890683122, 1.000000000000000000, 0.9659258262890683122, 1.000000000000000000, 0.9659258262890683122, 1.000000000000000000, 0.9659258262890683122, 1.000000000000000000, 0.9659258262890683122, 1.000000000000000000, 0.9659258262890683122, 1.000000000000000000, 0.9659258262890683122, 1.000000000000000000, 0.9659258262890683122, 1.000000000000000000, 0.9659258262890683122, 1.000000000000000000, 0.9659258262890683122, 1.000000000000000000, 0.9659258262890683122, 1.000000000000000000, 0.9659258262890683122, 1.000000000000000000, 0.9659258262890683122, 1.000000000000000000, 0.9659258262890683122, 1.000000000000000000, 0.9659258262890683122, 1.000000000000000000, 0.9659258262890683122, 1.000000000000000000, 0.9659258262890683122, 1.000000000000000000, 0.9659258262890683122, 1.000000000000000000, 0.9659258262890683122, 1.000000000000000000, 0.9659258262890683122, 1.000000000000000000, 0.9659258262890683122, 1.000000000000000000, 0.9659258262890683122, 1.000000000000000000, 0.9659258262890683122, 1.000000000000000000, 0.9659258262890683122, 1.000000000000000000, 0.9659258262890683122, 1.000000000000000000, 0.9659258262890683122, 1.000000000000000000, 0.9659258262890683122, 1.000000000000000000, 0.9659258262890683122, 1.000000000000000000, 0.9659258262890683122, 1.000000000000000000, 0.9659258262890683122, 1.000000000000000000, 0.9659258262890683122, 1.000000000000000000, 0.9659258262890683122, 1.000000000000000000, 0.9659258262890683122, 1.000000000000000000, 0.9659258262890683122, 1.000000000000000000, 0.9659258262890683122, 1.000000000000000000, 0.9659258262890683122, 1.000000000000000000, 0.9659258262890683122, 1.000000000000000000, 0.9659258262890683122, 1.000000000000000000, 0.9659258262890683122, 1.000000000000000000, 0.9659258262890683122, 1.000000000000000000, 0.9659258262890683122, 1.000000000000000000, 0.9659258262890683122, 1.000000000000000000, 0.9659258262890683122, 1.000000000000000000, 0.9659258262890683122, 1.000000000000000000, 0.9659258262890683122, 1.000000000000000000, 0.9659258262890683122, 1.000000000000000000, 0.9659258262890683122, 1.000000000000000000, 0.9659258262890683122, 1.000000000000000000, 0.9659258262890683122, 1.000000000000000000, 0.9659258262890683122, 1.000000000000000000, 0.9659258262890683122, 1.000000000000000000, 0.9659258262890683122, 1.000000000000000000, 0.9659258262890683122, 1.000000000000000000, 0.9659258262890683122, 1.000000000000000000, 0.9659258262890683122, 1.000000000000000000, 0.9659258262890683122, 1.000000000000000000, 0.9659258262890683122, 1.000000000000000000, 0.9659258262890683122, 1.000000000000000000, 0.9659258262890683122, 1.000000000000000000, 0.9659258262890683122, 1.000000000000000000, 0.9659258262890683122, 1.000000000000000000, 0.9659258262890683122, 1.000000000000000000, 0.9659258262890683122, 1.000000000000000000, 0.9659258262890683122, 1.000000000000000000, 0.9659258262890683122, 1.000000000000000000, 0.9659258262890683122, 1.000000000000000000, 0.9659258262890683122, 1.000000000000000000, 0.9659258262890683122, 1.000000000000000000, 0.9659258262890683122, 1.000000000000000000, 0.9659258262890683122, 1.000000000000000000, 0.9659258262890683122, 1.000000000000000000, 0.9659258262890683122, 1.000000000000000000, 0.9659258262890683122, 1.000000000000000000, 0.9659258262890683122, 1.000000000000000000, 0.9659258262890683122, 1.000000000000000000, 0.9659258262890683122, 1.000000000000000000, 0.9659258262890683122, 1.000000000000000000, 0.9659258262890683122, 1.000000000000000000, 0.9659258262890683122, 1.000000000000000000, 0.9659258262890683122, 1.000000000000000000, 0.9659258262890683122, 1.000000000000000000, 0.9659258262890683122, 1.000000000000000000, 0.9659258262890683122, 1.000000000000000000, 0.9659258262890683122, 1.000000000000000000, 0.9659258262890683122, 1.000000000000000000, 0.9659258262890683122, 1.000000000000000000, 0.9659258262890683122, 1.000000000000000000, 0.9659258262890683122, 1.000000000000000000, 0.9659258262890683122, 1.000000000000000000, 0.9659258262890683122, 1.000000000000000000, 0.9659258262890683122, 1.000000000000000000, 0.9659258262890683122, 1.000000000000000000, 0.9659258262890683122, 1.000000000000000000, 0.9659258262890683122, 1.000000000000000000, 0.9659258262890683122, 1.000000000000000000, 0.9659258262890683122, 1.000000000000000000, 0.9659258262890683122, 1.000000000000000000, 0.9659258262890683122, 1.000000000000000000, 0.9659258262890683122, 1.000000000000000000, 0.9659258262890683122, 1.000000000000000000, 0.9659258262890683122, 1.000000000000000000, 0.9659258262890683122, 1.000000000000000000, 0.9659258262890683122, 1.000000000000000000, 0.9659258262890683122, 1.000000000000000000, 0.9659258262890683122, 1.000000000000000000, 0.9659258262890683122, 1.000000000000000000, 0.9659258262890683122, 1.000000000000000000, 0.9659258262890683122, 1.000000000000000000, 0.9659258262890683122, 1.000000000000000000, 0.9659258262890683122, 1.000000000000000000, 0.9659258262890683122, 1.000000000000000000, 0.9659258262890683122, 1.000000000000000000, 0.9659258262890683122, 1.000000000000000000, 0.9659258262890683122, 1.000000000000000000, 0.9659258262890683122, 1.000000000000000000, 0.9659258262890683122, 1.000000000000000000, 0.9659258262890683122, 1.000000000000000000, 0.9659258262890683122, 1.000000000000000000, 0.9659258262890683122, 1.000000000000000000, 0.9659258262890683122, 1.000000000000000000, 0.9659258262890683122, 1.000000000000000000, 0.9659258262890683122, 1.000000000000000000, 0.9659258262890683122, 1.000000000000000000, 0.9659258262890683122, 1.000000000000000000, 0.9659258262890683122, 1.000000000000000000, 0.9659258262890683122, 1.000000000000000000, 0.9659258262890683122, 1.000000000000000000, 0.9659258262890683122, 1.000000000000000000, 0.9659258262890683122, 1.000000000000000000, 0.9659258262890683122, 1.000000000000000000, 0.9659258262890683122, 1.000000000000000000, 0.9659258262890683122, 1.000000000000000000, 0.9659258262890683122, 1.000000000000000000, 0.9659258262890683122, 1.000000000000000000, 0.9659258262890683122, 1.000000000000000000, 0.9659258262890683122, 1.000000000000000000, 0.9659258262890683122, 1.000000000000000000, 0.9659258262890683122, 1.000000000000000000, 0.9659258262890683122, 1.000000000000000000, 0.9659258262890683122, 1.000000000000000000, 0.9659258262890683122, 1.000000000000000000, 0.9659258262890683122, 1.000000000000000000, 0.9659258262890683122, 1.000000000000000000, 0.9659258262890683122, 1.000000000000000000, 0.9659258262890683122, 1.000000000000000000, 0.9659258262890683122, 1.000000000000000000, 0.9659258262890683122, 1.000000000000000000, 0.9659258262890683122, 1.000000000000000000, 0.9659258262890683122, 1.000000000000000000, 0.9659258262890683122, 1.000000000000000000, 0.9659258262890683122, 1.000000000000000000, 0.9659258262890683122, 1.000000000000000000, 0.9659258262890683122, 1.000000000000000000, 0.9659258262890683122, 1.000000000000000000, 0.9659258262890683122, 1.000000000000000000),
 ( 1.000000000000000000, 0.9659258262890683122, 1.000000000000000000, 0.9659258262890683122, 1.000000000000000000, 0.9659258262890683122, 1.000000000000000000, 0.9659258262890683122, 1.000000000000000000, 0.9659258262890683122, 1.000000000000000000, 0.9659258262890683122, 1.000000000000000000, 0.9659258262890683122, 1.000000000000000000, 0.9659258262890683122, 1.000000000000000000, 0.9659258262890683122, 1.000000000000000000, 0.9659258262890683122, 1.000000000000000000, 0.9659258262890683122, 1.000000000000000000, 0.9659258262890683122, 1.000000000000000000, 0.9659258262890683122, 1.000000000000000000, 0.9659258262890683122, 1.000000000000000000, 0.9659258262890683122, 1.000000000000000000, 0.9659258262890683122, 1.000000000000000000, 0.9659258262890683122, 1.000000000000000000, 0.9659258262890683122, 1.000000000000000000, 0.9659258262890683122, 1.000000000000000000, 0.9659258262890683122, 1.000000000000000000, 0.9659258262890683122, 1.000000000000000000, 0.9659258262890683122, 1.000000000000000000, 0.9659258262890683122, 1.000000000000000000, 0.9659258262890683122, 1.000000000000000000, 0.9659258262890683122, 1.000000000000000000, 0.9659258262890683122, 1.000000000000000000, 0.9659258262890683122, 1.000000000000000000, 0.9659258262890683122, 1.000000000000000000, 0.9659258262890683122, 1.000000000000000000, 0.9659258262890683122, 1.000000000000000000, 0.9659258262890683122, 1.000000000000000000, 0.9659258262890683122, 1.000000000000000000, 0.9659258262890683122, 1.000000000000000000, 0.9659258262890683122, 1.000000000000000000, 0.9659258262890683122, 1.000000000000000000, 0.9659258262890683122, 1.000000000000000000, 0.9659258262890683122, 1.000000000000000000, 0.9659258262890683122, 1.000000000000000000, 0.9659258262890683122, 1.000000000000000000, 0.9659258262890683122, 1.000000000000000000, 0.9659258262890683122, 1.000000000000000000, 0.9659258262890683122, 1.000000000000000000, 0.9659258262890683122, 1.000000000000000000, 0.9659258262890683122, 1.000000000000000000, 0.9659258262890683122, 1.000000000000000000, 0.9659258262890683122, 1.000000000000000000, 0.9659258262890683122, 1.000000000000000000, 0.9659258262890683122, 1.000000000000000000, 0.9659258262890683122, 1.000000000000000000, 0.9659258262890683122, 1.000000000000000000, 0.9659258262890683122, 1.000000000000000000, 0.9659258262890683122, 1.000000000000000000, 0.9659258262890683122, 1.000000000000000000, 0.9659258262890683122, 1.000000000000000000, 0.9659258262890683122, 1.000000000000000000, 0.9659258262890683122, 1.000000000000000000, 0.9659258262890683122, 1.000000000000000000, 0.9659258262890683122, 1.000000000000000000, 0.9659258262890683122, 1.000000000000000000, 0.9659258262890683122, 1.000000000000000000, 0.9659258262890683122, 1.000000000000000000, 0.9659258262890683122, 1.000000000000000000, 0.9659258262890683122, 1.000000000000000000, 0.9659258262890683122, 1.000000000000000000, 0.9659258262890683122, 1.000000000000000000, 0.9659258262890683122, 1.000000000000000000, 0.9659258262890683122, 1.000000000000000000, 0.9659258262890683122, 1.000000000000000000, 0.9659258262890683122, 1.000000000000000000, 0.9659258262890683122, 1.000000000000000000, 0.9659258262890683122, 1.000000000000000000, 0.9659258262890683122, 1.000000000000000000, 0.9659258262890683122, 1.000000000000000000, 0.9659258262890683122, 1.000000000000000000, 0.9659258262890683122, 1.000000000000000000, 0.9659258262890683122, 1.000000000000000000, 0.9659258262890683122, 1.000000000000000000, 0.9659258262890683122, 1.000000000000000000, 0.9659258262890683122, 1.000000000000000000, 0.9659258262890683122, 1.000000000000000000, 0.9659258262890683122, 1.000000000000000000, 0.9659258262890683122, 1.000000000000000000, 0.9659258262890683122, 1.000000000000000000, 0.9659258262890683122, 1.000000000000000000, 0.9659258262890683122, 1.000000000000000000, 0.9659258262890683122, 1.000000000000000000, 0.9659258262890683122, 1.000000000000000000, 0.9659258262890683122, 1.000000000000000000, 0.9659258262890683122, 1.000000000000000000, 0.9659258262890683122, 1.000000000000000000, 0.9659258262890683122, 1.000000000000000000, 0.9659258262890683122, 1.000000000000000000, 0.9659258262890683122, 1.000000000000000000, 0.9659258262890683122, 1.000000000000000000, 0.9659258262890683122, 1.000000000000000000, 0.9659258262890683122, 1.000000000000000000, 0.9659258262890683122, 1.000000000000000000, 0.9659258262890683122, 1.000000000000000000, 0.9659258262890683122, 1.000000000000000000, 0.9659258262890683122, 1.000000000000000000, 0.9659258262890683122, 1.000000000000000000, 0.9659258262890683122, 1.000000000000000000, 0.9659258262890683122, 1.000000000000000000, 0.9659258262890683122, 1.000000000000000000, 0.9659258262890683122, 1.000000000000000000, 0.9659258262890683122, 1.000000000000000000, 0.9659258262890683122, 1.000000000000000000, 0.9659258262890683122, 1.000000000000000000, 0.9659258262890683122, 1.000000000000000000, 0.9659258262890683122, 1.000000000000000000, 0.9659258262890683122, 1.000000000000000000, 0.9659258262890683122, 1.000000000000000000, 0.9659258262890683122, 1.000000000000000000, 0.9659258262890683122, 1.000000000000000000, 0.9659258262890683122, 1.000000000000000000, 0.9659258262890683122, 1.000000000000000000, 0.9659258262890683122, 1.000000000000000000, 0.9659258262890683122, 1.000000000000000000, 0.9659258262890683122, 1.000000000000000000, 0.9659258262890683122, 1.000000000000000000, 0.9659258262890683122, 1.000000000000000000, 0.9659258262890683122, 1.000000000000000000, 0.9659258262890683122, 1.000000000000000000, 0.9659258262890683122, 1.000000000000000000, 0.9659258262890683122, 1.000000000000000000, 0.9659258262890683122, 1.000000000000000000, 0.9659258262890683122, 1.000000000000000000, 0.9659258262890683122, 1.000000000000000000, 0.9659258262890683122, 1.000000000000000000, 0.9659258262890683122, 1.000000000000000000, 0.9659258262890683122, 1.000000000000000000, 0.9659258262890683122, 1.000000000000000000, 0.9659258262890683122, 1.000000000000000000, 0.9659258262890683122, 1.000000000000000000, 0.9659258262890683122, 1.000000000000000000, 0.9659258262890683122, 1.000000000000000000, 0.9659258262890683122, 1.000000000000000000, 0.9659258262890683122, 1.000000000000000000, 0.9659258262890683122, 1.000000000000000000, 0.9659258262890683122, 1.000000000000000000, 0.9659258262890683122, 1.000000000000000000, 0.9659258262890683122, 1.000000000000000000, 0.9659258262890683122, 1.000000000000000000, 0.9659258262890683122, 1.000000000000000000, 0.9659258262890683122, 1.000000000000000000, 0.9659258262890683122, 1.000000000000000000, 0.9659258262890683122, 1.000000000000000000, 0.9659258262890683122, 1.000000000000000000, 0.9659258262890683122, 1.000000000000000000, 0.9659258262890683122, 1.000000000000000000, 0.9659258262890683122, 1.000000000000000000, 0.9659258262890683122, 1.000000000000000000, 0.9659258262890683122, 1.000000000000000000, 0.9659258262890683122, 1.000000000000000000, 0.9659258262890683122, 1.000000000000000000, 0.9659258262890683122, 1.000000000000000000, 0.9659258262890683122, 1.000000000000000000, 0.9659258262890683122, 1.000000000000000000, 0.9659258262890683122, 1.000000000000000000, 0.9659258262890683122, 1.000000000000000000, 0.9659258262890683122, 1.000000000000000000, 0.9659258262890683122, 1.000000000000000000) ) ) 
 REPRESENTATION_ITEM ( '' )  SURFACE ( )  );
#10733 = VERTEX_POINT ( 'NONE', #92772 ) ;
#10734 = CARTESIAN_POINT ( 'NONE',  ( 19.84674366389459266, 23.71726448433412315, -2.638427012816827677 ) ) ;
#10735 = VERTEX_POINT ( 'NONE', #342 ) ;
#10736 = CARTESIAN_POINT ( 'NONE',  ( 6.204703633549690345, 32.84541550158063927, 14.16423886937410082 ) ) ;
#10737 = CARTESIAN_POINT ( 'NONE',  ( 7.361572987183170547, 37.05059781766744464, 9.846743663894590881 ) ) ;
#10738 = CARTESIAN_POINT ( 'NONE',  ( -0.8801773607111008646, 48.27201867748816966, 2.915334737309923430 ) ) ;
#10739 = FACE_BOUND ( 'NONE', #63716, .T. ) ;
#10740 = EDGE_CURVE ( 'NONE', #30525, #70565, #16802, .T. ) ;
#10741 = CARTESIAN_POINT ( 'NONE',  ( -0.8801773607111009756, 38.06368534415484106, 1.068504757029289695E-15 ) ) ;
#10742 = B_SPLINE_CURVE_WITH_KNOTS ( 'NONE', 3,
 ( #43523, #67024, #21532, #67523, #60004, #90498 ),
 .UNSPECIFIED., .F., .F.,
 ( 4, 2, 4 ),
 ( 0.000000000000000000, 0.0002100574294231419411, 0.0004201148588462838823 ),
 .UNSPECIFIED. ) ;
#10743 = CIRCLE ( 'NONE', #28294, 15.00000000000000000 ) ;
#10744 = ADVANCED_FACE ( 'NONE', ( #30292 ), #45813, .F. ) ;
#10745 = CARTESIAN_POINT ( 'NONE',  ( 12.81628187352647608, -3.376365330069575066, -2.602085213965210642E-15 ) ) ;
#10746 = VERTEX_POINT ( 'NONE', #68317 ) ;
#10747 = CARTESIAN_POINT ( 'NONE',  ( 20.88017736071110875, 45.77201867748816966, -2.915334737309920765 ) ) ;
#10748 = CARTESIAN_POINT ( 'NONE',  ( -4.164238869374099039, 1.803748834913967647, 8.674139862899312516E-16 ) ) ;
#10749 = ORIENTED_EDGE ( 'NONE', *, *, #28284, .T. ) ;
#10750 = CARTESIAN_POINT ( 'NONE',  ( 19.38216949554541557, 27.24863466993041783, -9.382169495545420901 ) ) ;
#10751 = AXIS2_PLACEMENT_3D ( 'NONE', #9253, #70261, #63226 ) ;
#10752 =( NAMED_UNIT ( * ) PLANE_ANGLE_UNIT ( ) SI_UNIT ( $, .RADIAN. ) );
#10753 = CARTESIAN_POINT ( 'NONE',  ( 14.92337183194729988, 24.34226448433411960, -8.527530157486177487 ) ) ;
#10754 = CARTESIAN_POINT ( 'NONE',  ( 12.25993886608609351, 14.49999999999999112, -8.642563219313673883 ) ) ;
#10755 = CARTESIAN_POINT ( 'NONE',  ( 21.09922568453595559, 47.04030133659708923, -6.408140936763230044 ) ) ;
#10756 = DIRECTION ( 'NONE',  ( -1.000000000000000000, -0.000000000000000000, -0.000000000000000000 ) ) ;
#10757 = CARTESIAN_POINT ( 'NONE',  ( 19.84674366389459621, 23.50893115100078390, 7.409399052514197653E-17 ) ) ;
#10758 = VECTOR ( 'NONE', #8197, 1000.000000000000000 ) ;
#10759 = CIRCLE ( 'NONE', #45887, 0.5000000000000004441 ) ;
#10760 = CARTESIAN_POINT ( 'NONE',  ( 4.559911319644449179, 58.89701867748817676, 9.422509992056141925 ) ) ;
#10761 = EDGE_CURVE ( 'NONE', #15070, #66451, #24301, .T. ) ;
#10762 = DIRECTION ( 'NONE',  ( 0.000000000000000000, 0.000000000000000000, 1.000000000000000000 ) ) ;
#10763 = CARTESIAN_POINT ( 'NONE',  ( 31.00000000000000000, -1.803315223424012063E-15, -7.000000000000000000 ) ) ;
#10764 = CARTESIAN_POINT ( 'NONE',  ( 14.02068044289378967, 0.3639308153356252129, 5.331089937175756077 ) ) ;
#10765 = CARTESIAN_POINT ( 'NONE',  ( 5.076628168052703671, 1.842264484334118047, 8.527530157486179263 ) ) ;
#10766 = CARTESIAN_POINT ( 'NONE',  ( 16.40814093676324603, 12.45696800326375353, -11.09922568453594671 ) ) ;
#10767 = EDGE_CURVE ( 'NONE', #44163, #42904, #55111, .T. ) ;
#10768 = LINE ( 'NONE', #69304, #56290 ) ;
#10769 = CARTESIAN_POINT ( 'NONE',  ( 0.1532563361054083140, 46.00893115100079456, 1.131784320476157264E-15 ) ) ;
#10770 = CARTESIAN_POINT ( 'NONE',  ( -42.94000000000001194, 92.00000000000000000, -8.999999999999998224 ) ) ;
#10771 = CARTESIAN_POINT ( 'NONE',  ( -4.164238869374099039, 1.803748834913967647, 8.674139862899312516E-16 ) ) ;
#10772 = CARTESIAN_POINT ( 'NONE',  ( 19.84674366389459621, 33.50893115100078745, 7.409399052514197653E-17 ) ) ;
#10773 = CARTESIAN_POINT ( 'NONE',  ( 10.00000000000000178, 30.37363466993042138, 12.81628187352647608 ) ) ;
#10774 = FILL_AREA_STYLE ('',( #80242 ) ) ;
#10775 = CARTESIAN_POINT ( 'NONE',  ( 10.00000000000000178, 49.31368534415484106, 10.88017736071110342 ) ) ;
#10776 = CARTESIAN_POINT ( 'NONE',  ( 21.09922568453595559, 2.040301336597086568, -6.408140936763230044 ) ) ;
#10777 = DIRECTION ( 'NONE',  ( 0.3665012267243070720, 0.000000000000000000, -0.9304175679820205769 ) ) ;
#10778 = CARTESIAN_POINT ( 'NONE',  ( 19.84674366389459266, 18.30059781766745175, 2.638427012816836559 ) ) ;
#10779 = CARTESIAN_POINT ( 'NONE',  ( 20.88017736071110164, 25.35535201082150891, 2.915334737309930979 ) ) ;
#10780 = CARTESIAN_POINT ( 'NONE',  ( -2.816281873526471635, 28.91530133659708213, -3.434112377981056508 ) ) ;
#10781 = FILL_AREA_STYLE ('',( #92794 ) ) ;
#10782 = CARTESIAN_POINT ( 'NONE',  ( -0.8218345515126993517, 0.04922511925147192435, -14.72992491912911639 ) ) ;
#10783 = CARTESIAN_POINT ( 'NONE',  ( 10.00000000000000178, 39.31368534415484106, 10.88017736071110342 ) ) ;
#10784 = CIRCLE ( 'NONE', #47465, 15.00000000000000000 ) ;
#10785 = VERTEX_POINT ( 'NONE', #62764 ) ;
#10786 = CARTESIAN_POINT ( 'NONE',  ( 10.00000000000000178, 59.31368534415484106, 10.88017736071110342 ) ) ;
#10787 = B_SPLINE_CURVE_WITH_KNOTS ( 'NONE', 3,
 ( #6384, #67389, #83381, #36900, #90869, #14903 ),
 .UNSPECIFIED., .F., .F.,
 ( 4, 2, 4 ),
 ( 0.000000000000000000, 0.0002626113303185870955, 0.0005252226606371741911 ),
 .UNSPECIFIED. ) ;
#10788 = FILL_AREA_STYLE ('',( #79278 ) ) ;
#10790 = CARTESIAN_POINT ( 'NONE',  ( 4.559911319644449179, 28.89701867748817321, 9.422509992056141925 ) ) ;
#10789 = CARTESIAN_POINT ( 'NONE',  ( 19.84674366389459621, 38.50893115100078745, 7.409399052514197653E-17 ) ) ;
#10791 = PLANE ( 'NONE',  #66361 ) ;
#10792 = CARTESIAN_POINT ( 'NONE',  ( 12.91533473730992121, 44.52201867748816966, 10.88017736071110164 ) ) ;
#10794 = DIRECTION ( 'NONE',  ( 1.000000000000000000, -1.257568779154408793E-17, 0.000000000000000000 ) ) ;
#10793 = CARTESIAN_POINT ( 'NONE',  ( -0.8801773607111008646, 13.27201867748817321, 2.915334737309923430 ) ) ;
#10795 = CARTESIAN_POINT ( 'NONE',  ( 21.92686044187657401, 55.37045670184114954, -3.195792623639525765 ) ) ;
#10796 = CARTESIAN_POINT ( 'NONE',  ( 19.84674366389459266, 33.30059781766744464, 2.638427012816836559 ) ) ;
#10798 = CARTESIAN_POINT ( 'NONE',  ( 1.909764518474428519, 0.000000000000000000, 5.107897229450606424 ) ) ;
#10797 = CARTESIAN_POINT ( 'NONE',  ( 10.00000000000000178, 43.05374883491397497, 14.16423886937410082 ) ) ;
#10799 = CARTESIAN_POINT ( 'NONE',  ( -0.2078280073304304698, 14.95041468192699696, -14.75174119393810557 ) ) ;
#10800 = DIRECTION ( 'NONE',  ( 0.000000000000000000, 0.000000000000000000, 1.000000000000000000 ) ) ;
#10801 = EDGE_CURVE ( 'NONE', #11027, #105, #24802, .T. ) ;
#10803 = CARTESIAN_POINT ( 'NONE',  ( -4.164238869374099039, 26.80374883491397142, 8.674139862899312516E-16 ) ) ;
#10802 =( BOUNDED_CURVE ( )  B_SPLINE_CURVE ( 2, ( #67005, #93939, #61953, #84478, #2477, #55453, #54938, #69965, #48432 ),
 .UNSPECIFIED., .F., .F. ) 
 B_SPLINE_CURVE_WITH_KNOTS ( ( 3, 2, 2, 2, 3 ),
 ( 0.3329980797973742246, 0.3333333333333333703, 0.3392857142857143016, 0.3452380952380952328, 0.3455733487740543786 ),
 .UNSPECIFIED. ) 
 CURVE ( )  GEOMETRIC_REPRESENTATION_ITEM ( )  RATIONAL_B_SPLINE_CURVE ( ( 0.9963778908391760503, 0.9980808541467920403, 1.000000000000000000, 0.9659258262890683122, 1.000000000000000000, 0.9659258262890683122, 1.000000000000000000, 0.9980808541467920403, 0.9963778908391759392 ) ) 
 REPRESENTATION_ITEM ( '' )  );
#10804 = AXIS2_PLACEMENT_3D ( 'NONE', #46508, #9498, #40000 ) ;
#10805 = CARTESIAN_POINT ( 'NONE',  ( 11.62719953690061558, 14.49999999999999112, 9.476720473301933012 ) ) ;
#10806 = CARTESIAN_POINT ( 'NONE',  ( -4.164238869374099039, 66.80374883491396076, 8.674139862899312516E-16 ) ) ;
#10807 = CARTESIAN_POINT ( 'NONE',  ( 5.076628168052703671, 41.84226448433411605, 8.527530157486179263 ) ) ;
#10809 = CARTESIAN_POINT ( 'NONE',  ( -14.71525861348292175, 14.49999999999999822, 2.908807992686482713 ) ) ;
#10808 = CARTESIAN_POINT ( 'NONE',  ( 8.979999999999991545, 27.03929484861771826, -3.000000000000000000 ) ) ;
#10810 = CARTESIAN_POINT ( 'NONE',  ( 20.88017736071110519, 55.56368534415484817, 2.639326808657452039E-16 ) ) ;
#10811 = CARTESIAN_POINT ( 'NONE',  ( 13.43411237798106583, 62.66530133659708923, -12.81628187352647252 ) ) ;
#10812 = CARTESIAN_POINT ( 'NONE',  ( 19.42250999205614193, 35.14701867748816966, 5.440088680355555262 ) ) ;
#10813 = CARTESIAN_POINT ( 'NONE',  ( -2.816281873526473856, 64.12363466993042493, 9.499525473075851096E-16 ) ) ;
#10814 = CARTESIAN_POINT ( 'NONE',  ( 13.43411237798106583, 7.665301336597086568, -12.81628187352647252 ) ) ;
#10815 = CARTESIAN_POINT ( 'NONE',  ( 19.84674366389459266, 13.71726448433411782, -2.638427012816827677 ) ) ;
#10816 = VERTEX_POINT ( 'NONE', #46779 ) ;
#10817 = CARTESIAN_POINT ( 'NONE',  ( -0.1023957841222418036, 20.13377557478296609, 6.340343622311920946 ) ) ;
#10818 = CARTESIAN_POINT ( 'NONE',  ( 7.084665262690076126, 2.022018677488171434, -10.88017736071110164 ) ) ;
#10819 = CARTESIAN_POINT ( 'NONE',  ( 24.16423886937409904, 29.09541550158063572, 3.795296366450317205 ) ) ;
#10820 = CARTESIAN_POINT ( 'NONE',  ( 20.88017736071110164, 35.35535201082150536, 2.915334737309930979 ) ) ;
#10821 = AXIS2_PLACEMENT_3D ( 'NONE', #81189, #72685, #12194 ) ;
#10822 = CARTESIAN_POINT ( 'NONE',  ( 20.88017736071110164, 45.35535201082149115, 2.915334737309930979 ) ) ;
#10823 = DIRECTION ( 'NONE',  ( 0.000000000000000000, 0.000000000000000000, -1.000000000000000000 ) ) ;
#10824 = CARTESIAN_POINT ( 'NONE',  ( 18.52753015748618282, 48.92559781766745886, -4.923371831947291888 ) ) ;
#10825 = CARTESIAN_POINT ( 'NONE',  ( 7.361572987183169658, 4.967264484334119601, -9.846743663894592657 ) ) ;
#10826 =( NAMED_UNIT ( * ) SI_UNIT ( $, .STERADIAN. ) SOLID_ANGLE_UNIT ( ) );
#10827 = CARTESIAN_POINT ( 'NONE',  ( 0.1532563361054083140, 26.00893115100078745, 1.131784320476157264E-15 ) ) ;
#10828 = PRESENTATION_STYLE_ASSIGNMENT (( #56808 ) ) ;
#10829 = CARTESIAN_POINT ( 'NONE',  ( -11.62006642627369146, 15.00000000000000533, 8.881585844847059263 ) ) ;
#10830 = CARTESIAN_POINT ( 'NONE',  ( 7.361572987183169658, 29.96726448433411960, -9.846743663894592657 ) ) ;
#10831 = CARTESIAN_POINT ( 'NONE',  ( 5.076628168052704559, 50.17559781766745886, -8.527530157486179263 ) ) ;
#10832 = CIRCLE ( 'NONE', #49140, 0.2500000000000002220 ) ;
#10833 = CIRCLE ( 'NONE', #49144, 0.4999999999999995559 ) ;
#10834 = VECTOR ( 'NONE', #39641, 1000.000000000000000 ) ;
#10835 = CARTESIAN_POINT ( 'NONE',  ( 21.09922568453594849, 41.20696800326375353, 6.408140936763242479 ) ) ;
#10836 = CARTESIAN_POINT ( 'NONE',  ( 12.91533473730993009, 51.60535201082149825, -10.88017736071109987 ) ) ;
#10837 = CARTESIAN_POINT ( 'NONE',  ( 5.076628168052704559, 25.17559781766745175, -8.527530157486179263 ) ) ;
#10839 = CARTESIAN_POINT ( 'NONE',  ( 12.63842701281683034, 17.46726448433411250, 9.846743663894596210 ) ) ;
#10838 = CARTESIAN_POINT ( 'NONE',  ( 20.36894250292379382, 43.67874883491397497, 10.36894250292379205 ) ) ;
#10840 = CARTESIAN_POINT ( 'NONE',  ( -0.1049300847420624183, 47.21697413083880690, -6.336235997365760930 ) ) ;
#10841 = DIRECTION ( 'NONE',  ( 0.000000000000000000, -1.000000000000000000, 0.000000000000000000 ) ) ;
#10842 = CARTESIAN_POINT ( 'NONE',  ( -2.266590686148945544, 12.22041550158063394, 7.082119434687048631 ) ) ;
#10843 = CARTESIAN_POINT ( 'NONE',  ( 2.917880565312948704, 27.63708216824730357, 12.26659068614894643 ) ) ;
#10844 = CARTESIAN_POINT ( 'NONE',  ( 18.52753015748618282, 23.92559781766745530, -4.923371831947291888 ) ) ;
#10845 = CARTESIAN_POINT ( 'NONE',  ( 8.879999999999991900, 76.07179676972447169, 6.500000000000000888 ) ) ;
#10846 = CARTESIAN_POINT ( 'NONE',  ( 12.91533473730993009, 26.60535201082150536, -10.88017736071109987 ) ) ;
#10847 = CARTESIAN_POINT ( 'NONE',  ( 19.42250999205614548, 40.98035201082150536, -5.440088680355545492 ) ) ;
#10848 = CARTESIAN_POINT ( 'NONE',  ( 19.42250999205614548, 40.98035201082150536, -5.440088680355545492 ) ) ;
#10849 = EDGE_LOOP ( 'NONE', ( #19368, #11104, #75249, #13473 ) ) ;
#10850 = EDGE_CURVE ( 'NONE', #18240, #32841, #31277, .T. ) ;
#10851 = CARTESIAN_POINT ( 'NONE',  ( 15.44008868035555260, 59.73035201082151247, 9.422509992056143702 ) ) ;
#10852 = ORIENTED_EDGE ( 'NONE', *, *, #72663, .F. ) ;
#10853 = DIRECTION ( 'NONE',  ( -0.000000000000000000, -0.000000000000000000, -1.000000000000000000 ) ) ;
#10854 = CARTESIAN_POINT ( 'NONE',  ( 12.91533473730992121, 59.52201867748816966, 10.88017736071110164 ) ) ;
#10855 = EDGE_LOOP ( 'NONE', ( #84912, #81070, #76426, #78136 ) ) ;
#10857 = ADVANCED_FACE ( 'NONE', ( #9280 ), #90227, .F. ) ;
#10856 = CARTESIAN_POINT ( 'NONE',  ( 10.00000000000000000, 66.81368534415484817, -10.88017736071110342 ) ) ;
#10858 = CARTESIAN_POINT ( 'NONE',  ( -12.69000000000001371, 93.50000000000000000, -10.09898361729590199 ) ) ;
#10859 = DIRECTION ( 'NONE',  ( -0.000000000000000000, 1.000000000000000000, -0.000000000000000000 ) ) ;
#10860 = CARTESIAN_POINT ( 'NONE',  ( -0.8801773607110991993, 12.85535201082150358, -2.915334737309923874 ) ) ;
#10861 = CARTESIAN_POINT ( 'NONE',  ( 2.791683348922240793, 11.63393115100078568, 7.208316651077764092 ) ) ;
#10862 = EDGE_CURVE ( 'NONE', #18218, #75294, #52286, .T. ) ;
#10863 = CARTESIAN_POINT ( 'NONE',  ( 5.076628168052703671, 1.842264484334118047, 8.527530157486179263 ) ) ;
#10864 = CARTESIAN_POINT ( 'NONE',  ( -0.8801773607111008646, 8.272018677488171434, 2.915334737309923430 ) ) ;
#10865 = CARTESIAN_POINT ( 'NONE',  ( 10.00000000000000000, 49.75893115100078745, -9.846743663894594434 ) ) ;
#10866 = VERTEX_POINT ( 'NONE', #16790 ) ;
#10867 = CARTESIAN_POINT ( 'NONE',  ( 18.52753015748617571, 48.09226448433412315, 4.923371831947298993 ) ) ;
#10868 = ORIENTED_EDGE ( 'NONE', *, *, #68033, .T. ) ;
#10869 = CARTESIAN_POINT ( 'NONE',  ( -15.00000000000004974, 91.25000000000000000, 8.000000000000000000 ) ) ;
#10870 = CARTESIAN_POINT ( 'NONE',  ( -0.8801773607111009756, 53.06368534415484106, 1.068504757029289695E-15 ) ) ;
#10871 = CARTESIAN_POINT ( 'NONE',  ( 0.1532563361054083140, 51.00893115100078745, 1.131784320476157264E-15 ) ) ;
#10873 = DIRECTION ( 'NONE',  ( 0.000000000000000000, 0.000000000000000000, 1.000000000000000000 ) ) ;
#10872 = SURFACE_SIDE_STYLE ('',( #47379 ) ) ;
#10874 = CARTESIAN_POINT ( 'NONE',  ( -0.8801773607111009756, 53.06368534415484106, 1.068504757029289695E-15 ) ) ;
#10875 = CARTESIAN_POINT ( 'NONE',  ( -4.164238869374098151, 66.59541550158060375, -3.795296366450310543 ) ) ;
#10876 = CARTESIAN_POINT ( 'NONE',  ( 6.565887622018943937, 38.08196800326376064, -12.81628187352647608 ) ) ;
#10877 = CARTESIAN_POINT ( 'NONE',  ( -5.817157072110893168, 15.00000000000000000, 13.82608706751082828 ) ) ;
#10878 = ORIENTED_EDGE ( 'NONE', *, *, #3741, .F. ) ;
#10879 = CARTESIAN_POINT ( 'NONE',  ( 22.81628187352647785, 26.62363466993042138, 6.195893100308588602E-16 ) ) ;
#10880 = CARTESIAN_POINT ( 'NONE',  ( 19.42250999205614193, 30.14701867748817321, 5.440088680355555262 ) ) ;
#10882 = ORIENTED_EDGE ( 'NONE', *, *, #35785, .F. ) ;
#10881 = EDGE_CURVE ( 'NONE', #72857, #14939, #90597, .T. ) ;
#10883 = MECHANICAL_DESIGN_GEOMETRIC_PRESENTATION_REPRESENTATION (  '', ( #55642 ), #73179 ) ;
#10884 = CARTESIAN_POINT ( 'NONE',  ( 0.6178305044545818747, -1.501365330069579951, -9.382169495545419124 ) ) ;
#10886 = CARTESIAN_POINT ( 'NONE',  ( 12.63842701281683922, 44.55059781766745175, -9.846743663894590881 ) ) ;
#10885 = CARTESIAN_POINT ( 'NONE',  ( 12.63842701281683034, 7.467264484334118713, 9.846743663894596210 ) ) ;
#10887 = CARTESIAN_POINT ( 'NONE',  ( -1.354709868695722852, 15.00000000000000000, 14.93870011653150698 ) ) ;
#10888 =( NAMED_UNIT ( * ) PLANE_ANGLE_UNIT ( ) SI_UNIT ( $, .RADIAN. ) );
#10889 = CARTESIAN_POINT ( 'NONE',  ( 7.361572987183169658, 39.96726448433411605, -9.846743663894592657 ) ) ;
#10890 = CARTESIAN_POINT ( 'NONE',  ( 14.35840480524201013, 0.3640475087720984604, -4.340070442838850795 ) ) ;
#10893 = CARTESIAN_POINT ( 'NONE',  ( 15.00000000000000000, 60.50000000000000711, -6.500000000000000888 ) ) ;
#10892 = STYLED_ITEM ( 'NONE', ( #95813 ), #59069 ) ;
#10891 = CARTESIAN_POINT ( 'NONE',  ( 19.84674366389459266, 28.30059781766745886, 2.638427012816836559 ) ) ;
#10894 = DIRECTION ( 'NONE',  ( -1.000000000000000000, 1.257568779154408793E-17, 0.000000000000000000 ) ) ;
#10896 = ORIENTED_EDGE ( 'NONE', *, *, #75848, .T. ) ;
#10895 = CARTESIAN_POINT ( 'NONE',  ( 18.52753015748617571, 63.09226448433412315, 4.923371831947298993 ) ) ;
#10897 = AXIS2_PLACEMENT_3D ( 'NONE', #8528, #23049, #2032 ) ;
#10898 = B_SPLINE_CURVE_WITH_KNOTS ( 'NONE', 3,
 ( #16171, #18504, #48994, #61644, #77151, #69662, #79504, #11003, #64476, #23690, #26488, #56983, #23194, #87488, #49479, #8660, #68682, #210, #53668, #8181, #38678, #69178 ),
 .UNSPECIFIED., .F., .F.,
 ( 4, 2, 2, 2, 2, 2, 2, 2, 2, 2, 4 ),
 ( 0.000000000000000000, 0.002788651922846089107, 0.005577303845692178214, 0.01115460769138435643, 0.02230921538276871285, 0.03346382307415306928, 0.04461843076553742571, 0.06692764614830616632, 0.07808225383969051581, 0.08365955768538271831, 0.08923686153107489305 ),
 .UNSPECIFIED. ) ;
#10899 = SURFACE_SIDE_STYLE ('',( #17911 ) ) ;
#10900 = CARTESIAN_POINT ( 'NONE',  ( -1.099225684535947600, 19.54030133659708568, 6.408140936763237150 ) ) ;
#10901 = CARTESIAN_POINT ( 'NONE',  ( 2.791683348922240793, 41.63393115100078745, 7.208316651077764092 ) ) ;
#10902 = CARTESIAN_POINT ( 'NONE',  ( -13.48255862861931043, 15.00000000000000000, 5.335786055104065895 ) ) ;
#10903 = CARTESIAN_POINT ( 'NONE',  ( -2.266590686148945544, 41.38708216824729647, -7.082119434687050408 ) ) ;
#10904 = CARTESIAN_POINT ( 'NONE',  ( 18.52753015748617571, 23.09226448433411960, 4.923371831947298993 ) ) ;
#10905 = CARTESIAN_POINT ( 'NONE',  ( 19.54746220608152285, 80.97929546852273575, 5.000000000000000000 ) ) ;
#10906 = CARTESIAN_POINT ( 'NONE',  ( -0.3689425029237898834, 61.17874883491396076, -10.36894250292378850 ) ) ;
#10907 = CARTESIAN_POINT ( 'NONE',  ( 5.076628168052703671, 61.84226448433412315, 8.527530157486179263 ) ) ;
#10908 = CARTESIAN_POINT ( 'NONE',  ( 19.42250999205614548, 10.98035201082150536, -5.440088680355545492 ) ) ;
#10909 = CARTESIAN_POINT ( 'NONE',  ( 2.917880565312948704, 32.63708216824730357, 12.26659068614894643 ) ) ;
#10910 = CARTESIAN_POINT ( 'NONE',  ( 24.16423886937410614, 39.51208216824731068, -3.795296366450302550 ) ) ;
#10911 = CARTESIAN_POINT ( 'NONE',  ( 4.600000000000003197, 98.49999999999998579, -8.525133428036873795 ) ) ;
#10913 = CARTESIAN_POINT ( 'NONE',  ( 12.63842701281683922, 54.55059781766745175, -9.846743663894590881 ) ) ;
#10912 = DIRECTION ( 'NONE',  ( -0.000000000000000000, -1.000000000000000000, -0.000000000000000000 ) ) ;
#10914 = VERTEX_POINT ( 'NONE', #98836 ) ;
#10915 = CARTESIAN_POINT ( 'NONE',  ( 20.88017736071110875, 35.77201867748816966, -2.915334737309920765 ) ) ;
#10916 = DIRECTION ( 'NONE',  ( 0.000000000000000000, 0.000000000000000000, 1.000000000000000000 ) ) ;
#10917 = CARTESIAN_POINT ( 'NONE',  ( -1.099225684535947600, 63.70696800326376774, -6.408140936763238038 ) ) ;
#10918 = CARTESIAN_POINT ( 'NONE',  ( -10.36894250292378317, 2.428748834913970089, 10.36894250292379560 ) ) ;
#10919 = CARTESIAN_POINT ( 'NONE',  ( 2.791683348922237240, 55.38393115100078745, -7.208316651077763204 ) ) ;
#10920 = DIRECTION ( 'NONE',  ( -0.9890158633619157147, 0.000000000000000000, -0.1478094111296180124 ) ) ;
#10921 = ORIENTED_EDGE ( 'NONE', *, *, #23303, .F. ) ;
#10922 = CARTESIAN_POINT ( 'NONE',  ( 20.36894250292379382, 33.67874883491396076, 10.36894250292379205 ) ) ;
#10923 = LINE ( 'NONE', #63904, #8748 ) ;
#10924 = CARTESIAN_POINT ( 'NONE',  ( -3.770608837557338333, -6.399801140514261633, -2.750000000000403233 ) ) ;
#10925 = CARTESIAN_POINT ( 'NONE',  ( 4.559911319644449179, 22.23035201082150536, -9.422509992056141925 ) ) ;
#10926 = CARTESIAN_POINT ( 'NONE',  ( -1.099225684535947600, 23.70696800326375708, -6.408140936763238038 ) ) ;
#10927 = CARTESIAN_POINT ( 'NONE',  ( -3.822225673302219739, 0.000000000000000000, -3.889525102760289066 ) ) ;
#10928 = CARTESIAN_POINT ( 'NONE',  ( 10.00000000000000000, 14.75893115100078568, -9.846743663894594434 ) ) ;
#10929 = CARTESIAN_POINT ( 'NONE',  ( -45.94000000000000483, 93.00000000000000000, 9.000000000000000000 ) ) ;
#10930 = CARTESIAN_POINT ( 'NONE',  ( -46.94000000000001194, 100.3306229069515325, -9.153711987617667134 ) ) ;
#10931 = EDGE_CURVE ( 'NONE', #74605, #48230, #83355, .T. ) ;
#10932 = LINE ( 'NONE', #87417, #48695 ) ;
#10933 = CARTESIAN_POINT ( 'NONE',  ( -0.8801773607111009756, 13.06368534415483929, 1.068504757029289695E-15 ) ) ;
#10934 = CARTESIAN_POINT ( 'NONE',  ( 4.096035146093531587, 4.098443466602401877E-16, -13.90943910019259278 ) ) ;
#10935 = CARTESIAN_POINT ( 'NONE',  ( -0.8801773607111008646, 38.27201867748816255, 2.915334737309923430 ) ) ;
#10936 = CARTESIAN_POINT ( 'NONE',  ( 0.5774900079438607392, 33.48035201082150536, 5.440088680355550821 ) ) ;
#10937 = CARTESIAN_POINT ( 'NONE',  ( 2.791683348922240793, 66.63393115100079456, 7.208316651077764092 ) ) ;
#10938 = CARTESIAN_POINT ( 'NONE',  ( 2.791683348922240793, 66.63393115100079456, 7.208316651077764092 ) ) ;
#10939 = CARTESIAN_POINT ( 'NONE',  ( -1.783843307429720415, 13.12729635533385597, 10.00000000000000000 ) ) ;
#10940 = CARTESIAN_POINT ( 'NONE',  ( 10.00000000000000000, 9.758931151000785675, -9.846743663894594434 ) ) ;
#10941 = ORIENTED_EDGE ( 'NONE', *, *, #11090, .T. ) ;
#10942 = ADVANCED_FACE ( 'NONE', ( #73086 ), #31506, .T. ) ;
#10943 = CARTESIAN_POINT ( 'NONE',  ( 10.00000000000000000, 31.81368534415483751, -10.88017736071110342 ) ) ;
#10944 = CIRCLE ( 'NONE', #49263, 1.249999999999987121 ) ;
#10945 = CARTESIAN_POINT ( 'NONE',  ( 19.38216949554541202, 0.9986346699304200492, 9.382169495545424454 ) ) ;
#10946 = CARTESIAN_POINT ( 'NONE',  ( 4.559911319644449179, 63.89701867748817676, 9.422509992056141925 ) ) ;
#10947 = CARTESIAN_POINT ( 'NONE',  ( 5.076628168052703671, 6.842264484334118713, 8.527530157486179263 ) ) ;
#10948 = CARTESIAN_POINT ( 'NONE',  ( -1.099225684535947600, 34.54030133659708923, 6.408140936763237150 ) ) ;
#10949 = CARTESIAN_POINT ( 'NONE',  ( 5.076628168052703671, 6.842264484334118713, 8.527530157486179263 ) ) ;
#10950 = ORIENTED_EDGE ( 'NONE', *, *, #34284, .F. ) ;
#10951 = DIRECTION ( 'NONE',  ( 0.000000000000000000, 0.000000000000000000, -1.000000000000000000 ) ) ;
#10952 = CARTESIAN_POINT ( 'NONE',  ( 2.603489959281591659, 15.43575266056827999, -6.500000000000006217 ) ) ;
#10953 = CARTESIAN_POINT ( 'NONE',  ( 19.42250999205614548, 10.98035201082150358, -5.440088680355545492 ) ) ;
#10955 = CARTESIAN_POINT ( 'NONE',  ( 10.00000000000000178, 23.05374883491397142, 14.16423886937410082 ) ) ;
#10954 = CARTESIAN_POINT ( 'NONE',  ( -1.099225684535947600, 54.54030133659708923, 6.408140936763237150 ) ) ;
#10956 = CARTESIAN_POINT ( 'NONE',  ( 0.1532563361054100626, 20.80059781766744464, -2.638427012816831230 ) ) ;
#10957 =( GEOMETRIC_REPRESENTATION_CONTEXT ( 3 ) GLOBAL_UNCERTAINTY_ASSIGNED_CONTEXT ( ( #2233 ) ) GLOBAL_UNIT_ASSIGNED_CONTEXT ( ( #61801, #46320, #23835 ) ) REPRESENTATION_CONTEXT ( 'NONE', 'WORKASPACE' ) );
#10958 = CARTESIAN_POINT ( 'NONE',  ( 7.361572987183170547, 27.05059781766745175, 9.846743663894590881 ) ) ;
#10959 = CARTESIAN_POINT ( 'NONE',  ( 20.88017736071110875, 5.772018677488170546, -2.915334737309920765 ) ) ;
#10960 = EDGE_LOOP ( 'NONE', ( #92524, #38406, #4272, #9478 ) ) ;
#10961 = CARTESIAN_POINT ( 'NONE',  ( 4.559911319644449179, 13.89701867748817143, 9.422509992056141925 ) ) ;
#10962 = CARTESIAN_POINT ( 'NONE',  ( 15.44008868035555793, 21.39701867748817321, -9.422509992056140149 ) ) ;
#10963 = B_SPLINE_CURVE_WITH_KNOTS ( 'NONE', 3,
 ( #98567, #28552, #37051, #82539, #74040, #74538 ),
 .UNSPECIFIED., .F., .F.,
 ( 4, 2, 4 ),
 ( 0.0002800630492131261874, 0.0006862688956284150425, 0.001092474742043704006 ),
 .UNSPECIFIED. ) ;
#10964 = DIRECTION ( 'NONE',  ( 0.000000000000000000, 0.000000000000000000, -1.000000000000000000 ) ) ;
#10965 = AXIS2_PLACEMENT_3D ( 'NONE', #49244, #43211, #4743 ) ;
#10966 = ORIENTED_EDGE ( 'NONE', *, *, #94485, .F. ) ;
#10967 = CARTESIAN_POINT ( 'NONE',  ( 13.07907619356926610, 0.2301500790491319004, 7.222187741820762064 ) ) ;
#10969 = EDGE_CURVE ( 'NONE', #52027, #91180, #50600, .T. ) ;
#10968 = CARTESIAN_POINT ( 'NONE',  ( 17.96484262340118221, 24.93868534415484461, 7.964842623401181321 ) ) ;
#10970 = CARTESIAN_POINT ( 'NONE',  ( 12.63842701281683034, 62.46726448433410894, 9.846743663894596210 ) ) ;
#10971 = DIRECTION ( 'NONE',  ( -0.000000000000000000, -1.000000000000000000, -0.000000000000000000 ) ) ;
#10972 = CARTESIAN_POINT ( 'NONE',  ( 10.00000000000000178, 50.37363466993042493, 12.81628187352647608 ) ) ;
#10973 = CARTESIAN_POINT ( 'NONE',  ( -3.927832320392339316, -0.03417435944610275333, 13.69797916712101404 ) ) ;
#10974 = CARTESIAN_POINT ( 'NONE',  ( 17.08211943468705130, 38.47041550158063217, 12.26659068614894998 ) ) ;
#10975 = CARTESIAN_POINT ( 'NONE',  ( 0.5774900079438607392, 38.48035201082150536, 5.440088680355550821 ) ) ;
#10976 = CARTESIAN_POINT ( 'NONE',  ( 2.035157376598824452, 13.68868534415483751, 7.964842623401179544 ) ) ;
#10977 = CARTESIAN_POINT ( 'NONE',  ( 17.20831665107776587, 57.88393115100078745, 7.208316651077764980 ) ) ;
#10978 = EDGE_CURVE ( 'NONE', #25147, #92057, #87393, .T. ) ;
#10979 = CARTESIAN_POINT ( 'NONE',  ( 18.18329248733322245, 32.60290668512019607, 6.499999999999997335 ) ) ;
#10980 = CARTESIAN_POINT ( 'NONE',  ( 1.472469842513823179, 40.59226448433411605, -4.923371831947296329 ) ) ;
#10981 = LINE ( 'NONE', #41502, #4780 ) ;
#10982 = CARTESIAN_POINT ( 'NONE',  ( 7.361572987183169658, 9.967264484334119601, -9.846743663894592657 ) ) ;
#10983 = CARTESIAN_POINT ( 'NONE',  ( 3.434112377981060948, -29.41803199673624292, 12.81628187352647430 ) ) ;
#10984 = VERTEX_POINT ( 'NONE', #55266 ) ;
#10985 = VECTOR ( 'NONE', #44694, 999.9999999999998863 ) ;
#10986 = CARTESIAN_POINT ( 'NONE',  ( 10.00000000000000178, 9.313685344154839285, 10.88017736071110342 ) ) ;
#10987 = CARTESIAN_POINT ( 'NONE',  ( 2.791683348922240793, 11.63393115100078568, 7.208316651077764092 ) ) ;
#10988 = CARTESIAN_POINT ( 'NONE',  ( 10.00000000000000000, -2.126365330069579951, -12.81628187352647608 ) ) ;
#10989 = CARTESIAN_POINT ( 'NONE',  ( 0.5774900079438590739, 42.64701867748816966, -5.440088680355550821 ) ) ;
#10991 = CARTESIAN_POINT ( 'NONE',  ( 13.43411237798105340, 50.58196800326375353, 12.81628187352647963 ) ) ;
#10990 = CARTESIAN_POINT ( 'NONE',  ( 4.559911319644449179, 17.23035201082150536, -9.422509992056141925 ) ) ;
#10992 = CARTESIAN_POINT ( 'NONE',  ( 13.79529636645031943, 35.34541550158063927, -14.16423886937409904 ) ) ;
#10993 = CARTESIAN_POINT ( 'NONE',  ( -14.48718990079891888, 4.171500096121077077E-16, -0.6093675230842403590 ) ) ;
#10994 = EDGE_CURVE ( 'NONE', #32864, #85555, #28455, .T. ) ;
#10995 = CARTESIAN_POINT ( 'NONE',  ( 16.40814093676323893, 60.79030133659709634, 11.09922568453595026 ) ) ;
#10996 = EDGE_LOOP ( 'NONE', ( #88322, #32306, #13258, #77937 ) ) ;
#10997 = CARTESIAN_POINT ( 'NONE',  ( 19.84674366389459621, 63.50893115100078745, 7.409399052514197653E-17 ) ) ;
#10998 = DIRECTION ( 'NONE',  ( 0.02617694830788287394, 0.000000000000000000, -0.9996573249755571489 ) ) ;
#10999 = CARTESIAN_POINT ( 'NONE',  ( 17.96484262340118221, 36.18868534415484106, -7.964842623401177768 ) ) ;
#11001 = ORIENTED_EDGE ( 'NONE', *, *, #46255, .T. ) ;
#11000 = EDGE_CURVE ( 'NONE', #5711, #8841, #53600, .T. ) ;
#11003 = CARTESIAN_POINT ( 'NONE',  ( -4.010384638568478266, -13.83464189901984120, 2.500000000000000444 ) ) ;
#11002 = CARTESIAN_POINT ( 'NONE',  ( 17.20831665107776587, 2.883931151000785231, 7.208316651077764980 ) ) ;
#11004 = CARTESIAN_POINT ( 'NONE',  ( 10.32896413005679825, 7.604976035794179801, -5.963430220938286119 ) ) ;
#11005 = AXIS2_PLACEMENT_3D ( 'NONE', #25233, #17720, #23757 ) ;
#11006 = CARTESIAN_POINT ( 'NONE',  ( 10.00000000000000178, 12.25893115100078568, 9.846743663894594434 ) ) ;
#11007 = CARTESIAN_POINT ( 'NONE',  ( 12.63842701281683922, 24.55059781766745175, -9.846743663894590881 ) ) ;
#11008 = CARTESIAN_POINT ( 'NONE',  ( 19.84674366389459621, 8.508931151000785675, 7.409399052514197653E-17 ) ) ;
#11010 = CARTESIAN_POINT ( 'NONE',  ( -5.240693273018903753, 0.04962883216462592173, -13.79102773477921140 ) ) ;
#11009 = CARTESIAN_POINT ( 'NONE',  ( 12.91533473730992121, 54.52201867748816255, 10.88017736071110164 ) ) ;
#11011 = CARTESIAN_POINT ( 'NONE',  ( 10.00000000000000000, 66.81368534415484817, -10.88017736071110342 ) ) ;
#11013 = ORIENTED_EDGE ( 'NONE', *, *, #94952, .F. ) ;
#11012 = CARTESIAN_POINT ( 'NONE',  ( 14.92337183194729988, 19.34226448433411960, -8.527530157486177487 ) ) ;
#11014 = LINE ( 'NONE', #10521, #15112 ) ;
#11015 = CARTESIAN_POINT ( 'NONE',  ( 10.00000000000000178, 57.25893115100078745, 9.846743663894594434 ) ) ;
#11016 = ORIENTED_EDGE ( 'NONE', *, *, #47770, .F. ) ;
#11017 = EDGE_LOOP ( 'NONE', ( #57674, #44219, #55817 ) ) ;
#11018 = DIRECTION ( 'NONE',  ( 0.000000000000000000, -7.806255641895625614E-15, -1.000000000000000000 ) ) ;
#11019 = CARTESIAN_POINT ( 'NONE',  ( -4.164238869374098151, 11.59541550158063217, -3.795296366450310543 ) ) ;
#11020 = CARTESIAN_POINT ( 'NONE',  ( -14.94699059465099822, 0.5000000000000004441, -1.259949270175015013 ) ) ;
#11021 = CARTESIAN_POINT ( 'NONE',  ( 17.08211943468705130, 23.47041550158063572, 12.26659068614894998 ) ) ;
#11022 = CARTESIAN_POINT ( 'NONE',  ( -4.164238869374098151, 26.59541550158063217, -3.795296366450310543 ) ) ;
#11023 = COLOUR_RGB ( '', 0.08235294, 0.09019608, 0.10196078) ;
#11024 = CARTESIAN_POINT ( 'NONE',  ( -4.164238869374099039, 1.803748834913967647, 8.674139862899312516E-16 ) ) ;
#11025 = DIRECTION ( 'NONE',  ( 0.000000000000000000, 1.000000000000000000, -0.000000000000000000 ) ) ;
#11026 = CARTESIAN_POINT ( 'NONE',  ( 17.96484262340118221, 41.18868534415484106, -7.964842623401177768 ) ) ;
#11027 = VERTEX_POINT ( 'NONE', #66082 ) ;
#11028 = CARTESIAN_POINT ( 'NONE',  ( 7.361572987183170547, 12.05059781766744997, 9.846743663894590881 ) ) ;
#11030 = CARTESIAN_POINT ( 'NONE',  ( 0.1532563361054082862, 16.21726448433411960, 2.638427012816831674 ) ) ;
#11029 = CARTESIAN_POINT ( 'NONE',  ( 20.88017736071110519, 60.56368534415484106, 2.639326808657452039E-16 ) ) ;
#11031 = CARTESIAN_POINT ( 'NONE',  ( -2.816281873526471635, 43.91530133659708923, -3.434112377981056508 ) ) ;
#11032 = CARTESIAN_POINT ( 'NONE',  ( 19.84674366389459266, 38.30059781766745175, 2.638427012816836559 ) ) ;
#11033 = CARTESIAN_POINT ( 'NONE',  ( -13.82671409943298357, 0.000000000000000000, 3.447387012295131115 ) ) ;
#11034 = CARTESIAN_POINT ( 'NONE',  ( 0.5774900079438607392, 58.48035201082151247, 5.440088680355550821 ) ) ;
#11035 = CARTESIAN_POINT ( 'NONE',  ( 19.38216949554541202, 25.99863466993042138, 9.382169495545424454 ) ) ;
#11036 = CARTESIAN_POINT ( 'NONE',  ( -14.16423886937409726, -37.98791783175268932, 3.795296366450320757 ) ) ;
#11037 = CARTESIAN_POINT ( 'NONE',  ( 18.52753015748618282, 28.92559781766745175, -4.923371831947291888 ) ) ;
#11038 = CARTESIAN_POINT ( 'NONE',  ( 22.26659068614895176, 14.72041550158063572, -7.082119434687042414 ) ) ;
#11039 = ORIENTED_EDGE ( 'NONE', *, *, #68784, .F. ) ;
#11040 = B_SPLINE_CURVE_WITH_KNOTS ( 'NONE', 3,
 ( #6881, #68870, #84848, #67881, #53860, #15870, #76843 ),
 .UNSPECIFIED., .F., .F.,
 ( 4, 3, 4 ),
 ( 1.788497222143715241E-16, 0.001212392164850256563, 0.002424962242136481996 ),
 .UNSPECIFIED. ) ;
#11041 = CARTESIAN_POINT ( 'NONE',  ( 20.88017736071110164, 40.35535201082150536, 2.915334737309930979 ) ) ;
#11042 = CARTESIAN_POINT ( 'NONE',  ( 10.00000000000000178, 49.31368534415484106, 10.88017736071110342 ) ) ;
#11043 = CARTESIAN_POINT ( 'NONE',  ( -0.3689425029237881626, 52.42874883491396076, 10.36894250292379027 ) ) ;
#11044 = CARTESIAN_POINT ( 'NONE',  ( 2.791683348922240793, 56.63393115100078035, 7.208316651077764092 ) ) ;
#11045 = CARTESIAN_POINT ( 'NONE',  ( 18.52753015748617571, 13.09226448433411960, 4.923371831947298993 ) ) ;
#11047 = CYLINDRICAL_SURFACE ( 'NONE', #73578, 15.00000000000000000 ) ;
#11046 = DIRECTION ( 'NONE',  ( 1.000000000000000000, 0.000000000000000000, 0.000000000000000000 ) ) ;
#11048 = CARTESIAN_POINT ( 'NONE',  ( 2.035157376598824452, 38.68868534415483396, 7.964842623401179544 ) ) ;
#11049 = DIRECTION ( 'NONE',  ( 0.000000000000000000, 0.000000000000000000, -1.000000000000000000 ) ) ;
#11050 = CARTESIAN_POINT ( 'NONE',  ( 0.6178305044545818747, 18.49863466993041428, -9.382169495545419124 ) ) ;
#11051 = CARTESIAN_POINT ( 'NONE',  ( 3.591859063236761518, 19.95696800326375353, 11.09922568453594849 ) ) ;
#11052 = CARTESIAN_POINT ( 'NONE',  ( 17.20831665107776587, 49.13393115100078745, -7.208316651077762316 ) ) ;
#11053 = CARTESIAN_POINT ( 'NONE',  ( 5.440088680355556150, 9.730352010821514241, 9.422509992056138373 ) ) ;
#11054 = CARTESIAN_POINT ( 'NONE',  ( 7.084665262690076126, 4.105352010821503583, 10.88017736071109987 ) ) ;
#11056 = CARTESIAN_POINT ( 'NONE',  ( -10.67057496978640252, -97.55820424041962724, -4.000000000000000000 ) ) ;
#11055 = CARTESIAN_POINT ( 'NONE',  ( -0.8801773607111009756, 68.06368534415484817, 1.068504757029289695E-15 ) ) ;
#11057 = EDGE_CURVE ( 'NONE', #20937, #77207, #66625, .T. ) ;
#11058 = CARTESIAN_POINT ( 'NONE',  ( -13.07751017357375112, 4.831904710033835254E-16, -6.263284095430687870 ) ) ;
#11059 = DIRECTION ( 'NONE',  ( -0.9483236552062001001, 0.000000000000000000, 0.3173046564050899798 ) ) ;
#11060 = CARTESIAN_POINT ( 'NONE',  ( 20.88017736071110164, 65.35535201082150536, 2.915334737309930979 ) ) ;
#11061 = CARTESIAN_POINT ( 'NONE',  ( -0.8801773607111008646, 63.27201867748817676, 2.915334737309923430 ) ) ;
#11062 = CARTESIAN_POINT ( 'NONE',  ( 0.000000000000000000, 14.49999999999999822, 0.000000000000000000 ) ) ;
#11063 = DIRECTION ( 'NONE',  ( -0.000000000000000000, -1.000000000000000000, -0.000000000000000000 ) ) ;
#11064 = CARTESIAN_POINT ( 'NONE',  ( 5.076628168052704559, 25.17559781766745175, -8.527530157486179263 ) ) ;
#11065 = CARTESIAN_POINT ( 'NONE',  ( 7.084665262690076126, 19.10535201082150181, 10.88017736071109987 ) ) ;
#11066 = CARTESIAN_POINT ( 'NONE',  ( 10.00000000000000000, 59.75893115100078745, -9.846743663894594434 ) ) ;
#11068 = CARTESIAN_POINT ( 'NONE',  ( -9.065164099344377391, 14.63595249122790598, -11.95084933600779920 ) ) ;
#11067 = CARTESIAN_POINT ( 'NONE',  ( 12.91533473730993009, 36.60535201082151247, -10.88017736071109987 ) ) ;
#11069 = FILL_AREA_STYLE_COLOUR ( '', #32145 ) ;
#11070 = CARTESIAN_POINT ( 'NONE',  ( -1.099225684535947600, 43.70696800326375353, -6.408140936763238038 ) ) ;
#11071 = ORIENTED_EDGE ( 'NONE', *, *, #35481, .T. ) ;
#11072 = CARTESIAN_POINT ( 'NONE',  ( 7.084665262690076126, 49.10535201082149825, 10.88017736071109987 ) ) ;
#11074 = DIRECTION ( 'NONE',  ( 0.000000000000000000, 1.000000000000000000, 0.000000000000000000 ) ) ;
#11073 = CARTESIAN_POINT ( 'NONE',  ( -2.816281873526473856, 24.12363466993042138, 9.499525473075851096E-16 ) ) ;
#11075 = CARTESIAN_POINT ( 'NONE',  ( 20.88017736071110875, 20.77201867748816611, -2.915334737309920765 ) ) ;
#11076 = CARTESIAN_POINT ( 'NONE',  ( 2.917880565312948704, 52.63708216824730357, 12.26659068614894643 ) ) ;
#11077 = CARTESIAN_POINT ( 'NONE',  ( 1.472469842513823179, 46.42559781766745175, 4.923371831947296329 ) ) ;
#11078 = AXIS2_PLACEMENT_3D ( 'NONE', #14655, #7139, #13642 ) ;
#11079 = CARTESIAN_POINT ( 'NONE',  ( 14.92337183194729633, 2.675597817667451750, 8.527530157486181039 ) ) ;
#11080 = CARTESIAN_POINT ( 'NONE',  ( 4.559911319644449179, 43.89701867748816966, 9.422509992056141925 ) ) ;
#11081 = CARTESIAN_POINT ( 'NONE',  ( -3.750000000000000000, 36.75000000000000000, -2.750000000000000000 ) ) ;
#11082 = CARTESIAN_POINT ( 'NONE',  ( -4.164238869374099039, 21.80374883491396787, 8.674139862899312516E-16 ) ) ;
#11083 = VECTOR ( 'NONE', #33540, 1000.000000000000000 ) ;
#11084 = CARTESIAN_POINT ( 'NONE',  ( -10.14667048435152097, 4.576487713787624877E-16, 10.35833375027034542 ) ) ;
#11085 = DIRECTION ( 'NONE',  ( -0.8526401643540953978, 0.000000000000000000, 0.5224985647159435809 ) ) ;
#11086 = VERTEX_POINT ( 'NONE', #4622 ) ;
#11087 = ORIENTED_EDGE ( 'NONE', *, *, #12326, .F. ) ;
#11088 = CARTESIAN_POINT ( 'NONE',  ( -4.164238869374099039, 46.80374883491397497, 8.674139862899312516E-16 ) ) ;
#11090 = EDGE_CURVE ( 'NONE', #73676, #30064, #79049, .T. ) ;
#11089 = CARTESIAN_POINT ( 'NONE',  ( -4.164238869374099927, 47.01208216824729647, 3.795296366450308767 ) ) ;
#11091 = CARTESIAN_POINT ( 'NONE',  ( 19.84674366389459266, 13.71726448433411782, -2.638427012816827677 ) ) ;
#11092 = CARTESIAN_POINT ( 'NONE',  ( 0.6178305044545818747, 18.49863466993041428, -9.382169495545419124 ) ) ;
#11093 = CARTESIAN_POINT ( 'NONE',  ( -13.51588146042584171, 90.98610341008148339, 7.976019732132908935 ) ) ;
#11094 = CARTESIAN_POINT ( 'NONE',  ( -14.88232117145528655, 15.00000000000000000, -1.875237731503337946 ) ) ;
#11096 = CARTESIAN_POINT ( 'NONE',  ( 22.81628187352647785, 31.62363466993042138, 6.195893100308588602E-16 ) ) ;
#11095 = CARTESIAN_POINT ( 'NONE',  ( -0.8801773607110991993, 67.85535201082151957, -2.915334737309923874 ) ) ;
#11097 = CARTESIAN_POINT ( 'NONE',  ( 10.00000000000000178, 43.05374883491397497, 14.16423886937410082 ) ) ;
#11098 = EDGE_CURVE ( 'NONE', #87486, #22095, #58585, .T. ) ;
#11099 = DIRECTION ( 'NONE',  ( 0.000000000000000000, 0.000000000000000000, -1.000000000000000000 ) ) ;
#11100 = CARTESIAN_POINT ( 'NONE',  ( 2.638427012816829897, -0.4494021823325435872, -9.846743663894592657 ) ) ;
#11101 = VERTEX_POINT ( 'NONE', #9777 ) ;
#11102 = DIRECTION ( 'NONE',  ( 0.000000000000000000, 0.000000000000000000, 1.000000000000000000 ) ) ;
#11103 = CARTESIAN_POINT ( 'NONE',  ( 17.20831665107776587, 17.88393115100078745, 7.208316651077764980 ) ) ;
#11104 = ORIENTED_EDGE ( 'NONE', *, *, #42890, .T. ) ;
#11105 = CARTESIAN_POINT ( 'NONE',  ( -4.164238869374099927, 12.01208216824730357, 3.795296366450308767 ) ) ;
#11107 = CARTESIAN_POINT ( 'NONE',  ( 7.084665262690076126, 9.105352010821503583, 10.88017736071109987 ) ) ;
#11106 = CARTESIAN_POINT ( 'NONE',  ( 10.00000000000000000, 6.813685344154838397, -10.88017736071110342 ) ) ;
#11109 = CARTESIAN_POINT ( 'NONE',  ( -2.816281873526471635, -1.084698663402913210, -3.434112377981056508 ) ) ;
#11108 = CARTESIAN_POINT ( 'NONE',  ( 1.472469842513823179, 46.42559781766745175, 4.923371831947296329 ) ) ;
#11110 = CARTESIAN_POINT ( 'NONE',  ( -29.94000000000001549, 92.00000000000000000, 9.500000000000000000 ) ) ;
#11111 = CARTESIAN_POINT ( 'NONE',  ( -13.75801628063875803, 15.00000000000000000, -4.578972376164643698 ) ) ;
#11112 = CARTESIAN_POINT ( 'NONE',  ( 10.00000000000000178, 20.37363466993042138, 12.81628187352647608 ) ) ;
#11113 = ORIENTED_EDGE ( 'NONE', *, *, #73178, .T. ) ;
#11114 = CARTESIAN_POINT ( 'NONE',  ( 24.16423886937409904, 64.09541550158064638, 3.795296366450317205 ) ) ;
#11115 = ORIENTED_EDGE ( 'NONE', *, *, #64113, .T. ) ;
#11116 = CARTESIAN_POINT ( 'NONE',  ( 17.08211943468705130, 53.47041550158063217, 12.26659068614894998 ) ) ;
#11117 = ORIENTED_EDGE ( 'NONE', *, *, #69915, .F. ) ;
#11118 = CARTESIAN_POINT ( 'NONE',  ( 20.88017736071110164, 35.35535201082150536, 2.915334737309930979 ) ) ;
#11119 = AXIS2_PLACEMENT_3D ( 'NONE', #4436, #4921, #13897 ) ;
#11120 = CARTESIAN_POINT ( 'NONE',  ( 20.88017736071110875, 40.77201867748818387, -2.915334737309920765 ) ) ;
#11121 = CARTESIAN_POINT ( 'NONE',  ( 7.084665262690076126, 39.10535201082150536, 10.88017736071109987 ) ) ;
#11122 = FILL_AREA_STYLE_COLOUR ( '', #98464 ) ;
#11123 = CARTESIAN_POINT ( 'NONE',  ( 20.88017736071110164, 45.35535201082149115, 2.915334737309930979 ) ) ;
#11124 = EDGE_CURVE ( 'NONE', #26718, #87224, #82033, .T. ) ;
#11125 = CIRCLE ( 'NONE', #84577, 2.000000000000000000 ) ;
#11126 = CARTESIAN_POINT ( 'NONE',  ( 9.779999999999990479, 20.99999999999999645, -3.000000000000000000 ) ) ;
#11127 = CARTESIAN_POINT ( 'NONE',  ( 18.52753015748617571, 13.09226448433411960, 4.923371831947298993 ) ) ;
#11128 = ORIENTED_EDGE ( 'NONE', *, *, #5230, .T. ) ;
#11129 = CARTESIAN_POINT ( 'NONE',  ( 10.58840669699852199, -98.14374106289703548, 4.000000000000000000 ) ) ;
#11130 = CARTESIAN_POINT ( 'NONE',  ( 5.076628168052704559, 45.17559781766745175, -8.527530157486179263 ) ) ;
#11131 = CARTESIAN_POINT ( 'NONE',  ( 4.999999999999997335, 16.50982297312470592, 7.000000000000000000 ) ) ;
#11132 = CARTESIAN_POINT ( 'NONE',  ( -3.711005778769052021, -5.293034685380286319, 3.750000000000000444 ) ) ;
#11133 = CARTESIAN_POINT ( 'NONE',  ( -46.43544119129182945, 103.9441758960464455, 5.610234333949799534 ) ) ;
#11134 = CARTESIAN_POINT ( 'NONE',  ( -45.12746704901013572, 105.3510678274659540, 4.910681296974491516 ) ) ;
#11135 = CARTESIAN_POINT ( 'NONE',  ( -3.420591144908350589, 0.5000000000000004441, -14.60477854057960556 ) ) ;
#11136 = CARTESIAN_POINT ( 'NONE',  ( -4.164238869374099039, 56.80374883491397497, 8.674139862899312516E-16 ) ) ;
#11137 = DIRECTION ( 'NONE',  ( -0.000000000000000000, -1.000000000000000000, -0.000000000000000000 ) ) ;
#11138 = EDGE_LOOP ( 'NONE', ( #71022, #22328, #43098, #88809 ) ) ;
#11139 = DIRECTION ( 'NONE',  ( 0.000000000000000000, 1.000000000000000000, 0.000000000000000000 ) ) ;
#11140 = CARTESIAN_POINT ( 'NONE',  ( 2.791683348922240793, 31.63393115100078745, 7.208316651077764092 ) ) ;
#11141 = CARTESIAN_POINT ( 'NONE',  ( 16.40814093676324603, 62.45696800326376064, -11.09922568453594671 ) ) ;
#11142 = CARTESIAN_POINT ( 'NONE',  ( 19.38216949554541557, 7.248634669930421381, -9.382169495545420901 ) ) ;
#11143 = CARTESIAN_POINT ( 'NONE',  ( 15.44008868035555260, 64.73035201082151957, 9.422509992056143702 ) ) ;
#11144 = CARTESIAN_POINT ( 'NONE',  ( 0.000000000000000000, 0.5000000000000004441, 0.000000000000000000 ) ) ;
#11145 = CARTESIAN_POINT ( 'NONE',  ( 17.20831665107776587, 14.13393115100078568, -7.208316651077762316 ) ) ;
#11146 = CARTESIAN_POINT ( 'NONE',  ( 14.92337183194729988, 54.34226448433412315, -8.527530157486177487 ) ) ;
#11147 = DIRECTION ( 'NONE',  ( 0.000000000000000000, 0.000000000000000000, 1.000000000000000000 ) ) ;
#11148 = ORIENTED_EDGE ( 'NONE', *, *, #65570, .T. ) ;
#11149 = CARTESIAN_POINT ( 'NONE',  ( 24.16423886937410614, 59.30374883491397497, 8.672049930838204340E-16 ) ) ;
#11150 = FACE_OUTER_BOUND ( 'NONE', #58326, .T. ) ;
#11151 = CARTESIAN_POINT ( 'NONE',  ( 17.96484262340118221, 36.18868534415484106, -7.964842623401177768 ) ) ;
#11153 = CARTESIAN_POINT ( 'NONE',  ( 8.490309438743736337, 12.94122572292852347, -8.044354728829526735 ) ) ;
#11152 = CARTESIAN_POINT ( 'NONE',  ( -2.816281873526473856, 29.12363466993041783, 9.499525473075851096E-16 ) ) ;
#11154 = SURFACE_SIDE_STYLE ('',( #95134 ) ) ;
#11155 = FACE_OUTER_BOUND ( 'NONE', #52594, .T. ) ;
#11156 = SURFACE_STYLE_USAGE ( .BOTH. , #58625 ) ;
#11157 = CARTESIAN_POINT ( 'NONE',  ( 0.1532563361054082862, 46.21726448433411605, 2.638427012816831674 ) ) ;
#11158 = CARTESIAN_POINT ( 'NONE',  ( 18.52753015748618282, 13.92559781766745175, -4.923371831947291888 ) ) ;
#11159 = CARTESIAN_POINT ( 'NONE',  ( 3.469446951953614189E-15, -20.68631465584515539, 10.88017736071110342 ) ) ;
#11160 = CARTESIAN_POINT ( 'NONE',  ( 13.43411237798106583, 27.66530133659708568, -12.81628187352647252 ) ) ;
#11161 = CARTESIAN_POINT ( 'NONE',  ( -14.43100913236851568, 4.866596497322921311E-16, 1.412789942453065883 ) ) ;
#11163 = CARTESIAN_POINT ( 'NONE',  ( 0.000000000000000000, 91.00000000000000000, 7.750000000000000000 ) ) ;
#11162 = CARTESIAN_POINT ( 'NONE',  ( -0.8801773607111008646, 23.27201867748817676, 2.915334737309923430 ) ) ;
#11164 = CARTESIAN_POINT ( 'NONE',  ( 24.16423886937410614, 39.51208216824731068, -3.795296366450302550 ) ) ;
#11165 = EDGE_CURVE ( 'NONE', #76576, #10735, #89279, .T. ) ;
#11166 = CARTESIAN_POINT ( 'NONE',  ( 20.36894250292379738, 29.92874883491396432, -10.36894250292379027 ) ) ;
#11167 = CARTESIAN_POINT ( 'NONE',  ( 2.035157376598824452, 8.688685344154839285, 7.964842623401179544 ) ) ;
#11168 = CARTESIAN_POINT ( 'NONE',  ( 19.84674366389459266, 48.30059781766745175, 2.638427012816836559 ) ) ;
#11169 = CARTESIAN_POINT ( 'NONE',  ( 6.565887622018943937, 43.08196800326374643, -12.81628187352647608 ) ) ;
#11170 = CARTESIAN_POINT ( 'NONE',  ( 2.035157376598822676, 17.43868534415483751, -7.964842623401177768 ) ) ;
#11171 = CARTESIAN_POINT ( 'NONE',  ( 5.076628168052703671, 41.84226448433411605, 8.527530157486179263 ) ) ;
#11172 = CARTESIAN_POINT ( 'NONE',  ( 20.88017736071110164, 35.35535201082150536, 2.915334737309930979 ) ) ;
#11173 = CARTESIAN_POINT ( 'NONE',  ( 22.81628187352647785, 1.623634669930420271, 6.195893100308588602E-16 ) ) ;
#11174 = CARTESIAN_POINT ( 'NONE',  ( -2.266590686148945544, 22.22041550158063572, 7.082119434687048631 ) ) ;
#11175 = LINE ( 'NONE', #18693, #7309 ) ;
#11176 = UNCERTAINTY_MEASURE_WITH_UNIT (LENGTH_MEASURE( 1.000000000000000082E-05 ), #16772, 'distance_accuracy_value', 'NONE');
#11177 = CARTESIAN_POINT ( 'NONE',  ( 10.00000000000000178, 27.25893115100078390, 9.846743663894594434 ) ) ;
#11178 = CARTESIAN_POINT ( 'NONE',  ( 22.81628187352648496, 56.83196800326374643, -3.434112377981050290 ) ) ;
#11179 = CARTESIAN_POINT ( 'NONE',  ( 0.1532563361054082862, 56.21726448433411605, 2.638427012816831674 ) ) ;
#11180 = ORIENTED_EDGE ( 'NONE', *, *, #32623, .F. ) ;
#11181 = CARTESIAN_POINT ( 'NONE',  ( 0.000000000000000000, 0.5000000000000004441, 0.000000000000000000 ) ) ;
#11182 = FILL_AREA_STYLE_COLOUR ( '', #49122 ) ;
#11183 = MECHANICAL_DESIGN_GEOMETRIC_PRESENTATION_REPRESENTATION (  '', ( #43155 ), #86274 ) ;
#11184 = CARTESIAN_POINT ( 'NONE',  ( -4.164238869374099039, 66.80374883491396076, 8.674139862899312516E-16 ) ) ;
#11185 = CARTESIAN_POINT ( 'NONE',  ( 17.08211943468705130, 8.470415501580635720, 12.26659068614894998 ) ) ;
#11186 = CARTESIAN_POINT ( 'NONE',  ( 10.00000000000000000, 66.81368534415484817, -10.88017736071110342 ) ) ;
#11187 = CARTESIAN_POINT ( 'NONE',  ( 10.00000000000000000, 49.75893115100078745, -9.846743663894594434 ) ) ;
#11188 = CARTESIAN_POINT ( 'NONE',  ( 7.084665262690076126, 37.02201867748817676, -10.88017736071110164 ) ) ;
#11189 = DIRECTION ( 'NONE',  ( -0.000000000000000000, -1.000000000000000000, -0.000000000000000000 ) ) ;
#11190 = CARTESIAN_POINT ( 'NONE',  ( 20.88017736071110164, 25.35535201082150891, 2.915334737309930979 ) ) ;
#11191 = VECTOR ( 'NONE', #66315, 1000.000000000000000 ) ;
#11192 = CIRCLE ( 'NONE', #92633, 2.000000000000001776 ) ;
#11193 = ORIENTED_EDGE ( 'NONE', *, *, #56947, .F. ) ;
#11194 = EDGE_LOOP ( 'NONE', ( #45264, #6200, #82683, #40983 ) ) ;
#11195 = VERTEX_POINT ( 'NONE', #30055 ) ;
#11196 = CARTESIAN_POINT ( 'NONE',  ( 11.24999999999999822, 10.63013551118487143, -3.014428414850134796 ) ) ;
#11197 = CARTESIAN_POINT ( 'NONE',  ( 22.26659068614895176, 9.720415501580633943, -7.082119434687042414 ) ) ;
#11199 = EDGE_CURVE ( 'NONE', #27072, #85384, #550, .T. ) ;
#11198 = CARTESIAN_POINT ( 'NONE',  ( -4.164238869374098151, 16.59541550158063927, -3.795296366450310543 ) ) ;
#11200 = CARTESIAN_POINT ( 'NONE',  ( -0.3689425029237881626, 57.42874883491397497, 10.36894250292379027 ) ) ;
#11201 = CARTESIAN_POINT ( 'NONE',  ( 19.84674366389459266, 58.30059781766745886, 2.638427012816836559 ) ) ;
#11202 = CARTESIAN_POINT ( 'NONE',  ( 7.361572987183169658, 39.96726448433411605, -9.846743663894592657 ) ) ;
#11203 = DIRECTION ( 'NONE',  ( -0.7132504491541847846, 0.000000000000000000, 0.7009092642998475675 ) ) ;
#11205 = CARTESIAN_POINT ( 'NONE',  ( 10.00000000000000178, 57.25893115100078745, 9.846743663894594434 ) ) ;
#11204 = CARTESIAN_POINT ( 'NONE',  ( 10.00000000000000000, 31.81368534415483751, -10.88017736071110342 ) ) ;
#11206 = CARTESIAN_POINT ( 'NONE',  ( -4.164238869374099039, 6.803748834913967869, 8.674139862899312516E-16 ) ) ;
#11207 = CARTESIAN_POINT ( 'NONE',  ( 22.26659068614895176, 39.72041550158063217, -7.082119434687042414 ) ) ;
#11208 = CARTESIAN_POINT ( 'NONE',  ( -0.3689425029237898834, 66.17874883491396076, -10.36894250292378850 ) ) ;
#11209 = CARTESIAN_POINT ( 'NONE',  ( 17.20831665107776587, 64.13393115100079456, -7.208316651077762316 ) ) ;
#11210 = CARTESIAN_POINT ( 'NONE',  ( 0.9082943533637206635, 15.00000000000000000, -14.47152380945584760 ) ) ;
#11211 = CARTESIAN_POINT ( 'NONE',  ( 12.91533473730993009, 66.60535201082150536, -10.88017736071109987 ) ) ;
#11212 = EDGE_CURVE ( 'NONE', #32729, #27101, #24858, .T. ) ;
#11213 = CARTESIAN_POINT ( 'NONE',  ( 14.92337183194729988, 29.34226448433411960, -8.527530157486177487 ) ) ;
#11214 = CARTESIAN_POINT ( 'NONE',  ( 7.208316651077762316, -30.86606884899920900, -7.208316651077764980 ) ) ;
#11215 = ORIENTED_EDGE ( 'NONE', *, *, #5107, .T. ) ;
#11216 = SURFACE_SIDE_STYLE ('',( #26703 ) ) ;
#11217 = ORIENTED_EDGE ( 'NONE', *, *, #55858, .F. ) ;
#11218 = CARTESIAN_POINT ( 'NONE',  ( 0.1532563361054083140, 26.00893115100078745, 1.131784320476157264E-15 ) ) ;
#11219 = ORIENTED_EDGE ( 'NONE', *, *, #72465, .T. ) ;
#11220 = CARTESIAN_POINT ( 'NONE',  ( -2.266590686148945544, 36.38708216824730357, -7.082119434687050408 ) ) ;
#11221 = CARTESIAN_POINT ( 'NONE',  ( 17.20831665107776587, 32.88393115100078745, 7.208316651077764980 ) ) ;
#11222 = CARTESIAN_POINT ( 'NONE',  ( 7.084665262690076126, 54.10535201082151247, 10.88017736071109987 ) ) ;
#11223 = CARTESIAN_POINT ( 'NONE',  ( 14.66196617519557677, 0.2306972965111900586, 2.874856965127918773 ) ) ;
#11224 = B_SPLINE_CURVE_WITH_KNOTS ( 'NONE', 3,
 ( #95378, #3900, #97368, #96383, #58342, #88862 ),
 .UNSPECIFIED., .F., .F.,
 ( 4, 2, 4 ),
 ( 0.000000000000000000, 0.0002565770811491102925, 0.0005131541622982205850 ),
 .UNSPECIFIED. ) ;
#11225 = CARTESIAN_POINT ( 'NONE',  ( 12.91533473730992121, 59.52201867748816966, 10.88017736071110164 ) ) ;
#11226 = CARTESIAN_POINT ( 'NONE',  ( 19.84674366389459621, 48.50893115100078745, 7.409399052514197653E-17 ) ) ;
#11227 = CARTESIAN_POINT ( 'NONE',  ( 3.469446951953614189E-15, -4.626365330069575954, 12.81628187352647608 ) ) ;
#11228 = ORIENTED_EDGE ( 'NONE', *, *, #19347, .T. ) ;
#11229 = CARTESIAN_POINT ( 'NONE',  ( 24.16423886937410614, 24.30374883491396787, 8.672049930838204340E-16 ) ) ;
#11230 = ORIENTED_EDGE ( 'NONE', *, *, #74466, .F. ) ;
#11231 = VERTEX_POINT ( 'NONE', #89583 ) ;
#11232 = CARTESIAN_POINT ( 'NONE',  ( 10.00000000000000000, 32.87363466993042493, -12.81628187352647608 ) ) ;
#11233 = CARTESIAN_POINT ( 'NONE',  ( 0.1532563361054100626, 20.80059781766744464, -2.638427012816831230 ) ) ;
#11234 = CARTESIAN_POINT ( 'NONE',  ( 4.559911319644449179, 3.897018677488170990, 9.422509992056141925 ) ) ;
#11235 = CARTESIAN_POINT ( 'NONE',  ( 19.38216949554541202, 50.99863466993042493, 9.382169495545424454 ) ) ;
#11236 = DIRECTION ( 'NONE',  ( 0.000000000000000000, 0.000000000000000000, -1.000000000000000000 ) ) ;
#11237 = CARTESIAN_POINT ( 'NONE',  ( 18.52753015748617571, 28.09226448433411960, 4.923371831947298993 ) ) ;
#11238 = EDGE_CURVE ( 'NONE', #25147, #12064, #15557, .T. ) ;
#11240 = COLOUR_RGB ( '', 0.72549020, 0.75294118, 0.79215686) ;
#11239 = CARTESIAN_POINT ( 'NONE',  ( 19.42250999205614193, 65.14701867748817676, 5.440088680355555262 ) ) ;
#11241 = CARTESIAN_POINT ( 'NONE',  ( -14.43100913236851568, 15.00000000000000000, 1.412789942453067216 ) ) ;
#11242 = CARTESIAN_POINT ( 'NONE',  ( -0.1503990784575407469, 17.22266099184918531, -6.262539305110056631 ) ) ;
#11243 = CARTESIAN_POINT ( 'NONE',  ( 10.00000000000000178, 2.258931151000784787, 9.846743663894594434 ) ) ;
#11244 = CARTESIAN_POINT ( 'NONE',  ( -1.099225684535947600, 29.54030133659708923, 6.408140936763237150 ) ) ;
#11245 = CIRCLE ( 'NONE', #70371, 0.2500000000000002220 ) ;
#11246 = EDGE_CURVE ( 'NONE', #77672, #49491, #4405, .T. ) ;
#11247 = VECTOR ( 'NONE', #95437, 1000.000000000000000 ) ;
#11248 = CARTESIAN_POINT ( 'NONE',  ( 7.361572987183170547, 47.05059781766745175, 9.846743663894590881 ) ) ;
#11249 = LINE ( 'NONE', #56274, #53697 ) ;
#11250 = CARTESIAN_POINT ( 'NONE',  ( -0.3689425029237881626, 12.42874883491396609, 10.36894250292379027 ) ) ;
#11251 = CARTESIAN_POINT ( 'NONE',  ( 0.1532563361054083140, 31.00893115100078390, 1.131784320476157264E-15 ) ) ;
#11252 = CARTESIAN_POINT ( 'NONE',  ( 13.43411237798105340, 35.58196800326375353, 12.81628187352647963 ) ) ;
#11254 = LINE ( 'NONE', #55786, #60833 ) ;
#11253 = CYLINDRICAL_SURFACE ( 'NONE', #89973, 0.09999999999999982514 ) ;
#11255 = CARTESIAN_POINT ( 'NONE',  ( 20.88017736071110875, 65.77201867748817676, -2.915334737309920765 ) ) ;
#11256 = TOROIDAL_SURFACE ( 'NONE', #94259, 0.7500000000000008882, 0.2500000000000000000 ) ;
#11257 = CARTESIAN_POINT ( 'NONE',  ( -2.816281873526473856, 4.331968003263754419, 3.434112377981055619 ) ) ;
#11258 = CARTESIAN_POINT ( 'NONE',  ( -13.80105244023572197, 90.89655890636302615, 7.750000000000543565 ) ) ;
#11259 = CARTESIAN_POINT ( 'NONE',  ( 1.472469842513823179, 35.59226448433412315, -4.923371831947296329 ) ) ;
#11260 = CARTESIAN_POINT ( 'NONE',  ( 19.42250999205614193, 30.14701867748817321, 5.440088680355555262 ) ) ;
#11261 = CARTESIAN_POINT ( 'NONE',  ( -1.099225684535947600, 23.70696800326375708, -6.408140936763238038 ) ) ;
#11262 = CARTESIAN_POINT ( 'NONE',  ( 10.00000000000000178, 27.25893115100078390, 9.846743663894594434 ) ) ;
#11263 = LINE ( 'NONE', #49744, #90179 ) ;
#11264 = CARTESIAN_POINT ( 'NONE',  ( 0.5774900079438607392, 33.48035201082150536, 5.440088680355550821 ) ) ;
#11265 = EDGE_LOOP ( 'NONE', ( #51939, #25976, #8900, #62737 ) ) ;
#11266 = CARTESIAN_POINT ( 'NONE',  ( 12.91533473730993009, 56.60535201082151247, -10.88017736071109987 ) ) ;
#11267 = CARTESIAN_POINT ( 'NONE',  ( 10.00000000000000178, 4.313685344154837509, 10.88017736071110342 ) ) ;
#11269 = CARTESIAN_POINT ( 'NONE',  ( 7.084665262690076126, 27.02201867748817676, -10.88017736071110164 ) ) ;
#11268 = CARTESIAN_POINT ( 'NONE',  ( 10.00000000000000178, 37.25893115100078745, 9.846743663894594434 ) ) ;
#11270 = DIRECTION ( 'NONE',  ( -0.000000000000000000, -1.000000000000000000, -0.000000000000000000 ) ) ;
#11271 = CARTESIAN_POINT ( 'NONE',  ( 17.96484262340118221, 49.93868534415484106, 7.964842623401181321 ) ) ;
#11273 = CARTESIAN_POINT ( 'NONE',  ( -2.120353041430445895, 3.806229657360874111E-16, -14.34413130794948543 ) ) ;
#11272 = CARTESIAN_POINT ( 'NONE',  ( 4.559911319644449179, 18.89701867748817321, 9.422509992056141925 ) ) ;
#11274 = FACE_OUTER_BOUND ( 'NONE', #56138, .T. ) ;
#11275 = CARTESIAN_POINT ( 'NONE',  ( 7.361572987183169658, 54.96726448433413026, -9.846743663894592657 ) ) ;
#11277 = CARTESIAN_POINT ( 'NONE',  ( -11.94720539484415944, 0.2306972965111586116, 8.972309510150065393 ) ) ;
#11276 = CARTESIAN_POINT ( 'NONE',  ( 13.79529636645031943, 55.34541550158062506, -14.16423886937409904 ) ) ;
#11278 = VECTOR ( 'NONE', #44100, 1000.000000000000000 ) ;
#11279 = CARTESIAN_POINT ( 'NONE',  ( 0.000000000000000000, 15.00000000000000000, 0.000000000000000000 ) ) ;
#11280 = CARTESIAN_POINT ( 'NONE',  ( 6.204703633549690345, 0.7620821682473009062, -14.16423886937410259 ) ) ;
#11281 = EDGE_CURVE ( 'NONE', #11943, #1670, #83072, .T. ) ;
#11282 = CARTESIAN_POINT ( 'NONE',  ( -0.3689425029237881626, 37.42874883491396787, 10.36894250292379027 ) ) ;
#11284 = DIRECTION ( 'NONE',  ( 0.000000000000000000, 0.000000000000000000, 1.000000000000000000 ) ) ;
#11283 = AXIS2_PLACEMENT_3D ( 'NONE', #61068, #6108, #51610 ) ;
#11285 = EDGE_LOOP ( 'NONE', ( #44064, #73161, #81306, #10506 ) ) ;
#11286 = CARTESIAN_POINT ( 'NONE',  ( 13.79529636645031943, 65.34541550158063217, -14.16423886937409904 ) ) ;
#11287 = EDGE_CURVE ( 'NONE', #25163, #7091, #68077, .T. ) ;
#11288 = CARTESIAN_POINT ( 'NONE',  ( 1.472469842513823179, 35.59226448433412315, -4.923371831947296329 ) ) ;
#11290 = CARTESIAN_POINT ( 'NONE',  ( -8.004649405379840488, 84.50413264541204228, -3.999860480131919527 ) ) ;
#11289 = PLANE ( 'NONE',  #57925 ) ;
#11291 = CARTESIAN_POINT ( 'NONE',  ( 0.5774900079438590739, 62.64701867748817676, -5.440088680355550821 ) ) ;
#11292 = CARTESIAN_POINT ( 'NONE',  ( -8.439016546559740206, 3.923478264313957572E-16, -11.79122553964984910 ) ) ;
#11293 = CARTESIAN_POINT ( 'NONE',  ( 7.084665262690076126, 32.02201867748816966, -10.88017736071110164 ) ) ;
#11294 = CARTESIAN_POINT ( 'NONE',  ( -1.099225684535947600, 64.54030133659709634, 6.408140936763237150 ) ) ;
#11295 = CARTESIAN_POINT ( 'NONE',  ( 0.6178305044545838731, 9.748634669930416052, 9.382169495545420901 ) ) ;
#11296 = CARTESIAN_POINT ( 'NONE',  ( 18.52753015748618282, 18.92559781766745175, -4.923371831947291888 ) ) ;
#11297 = ORIENTED_EDGE ( 'NONE', *, *, #24384, .F. ) ;
#11298 = CARTESIAN_POINT ( 'NONE',  ( 3.969999999999999751, 36.75000000000000000, -3.750000000000000000 ) ) ;
#11299 = SURFACE_STYLE_USAGE ( .BOTH. , #28762 ) ;
#11300 = CARTESIAN_POINT ( 'NONE',  ( -0.3689425029237881626, 67.42874883491396076, 10.36894250292379027 ) ) ;
#11301 = CARTESIAN_POINT ( 'NONE',  ( -0.3689425029237898834, 26.17874883491396432, -10.36894250292378850 ) ) ;
#11302 = CARTESIAN_POINT ( 'NONE',  ( 0.5774900079438607392, 38.48035201082150536, 5.440088680355550821 ) ) ;
#11303 = CARTESIAN_POINT ( 'NONE',  ( 12.91533473730992121, 44.52201867748816966, 10.88017736071110164 ) ) ;
#11304 = CARTESIAN_POINT ( 'NONE',  ( -13.07751017358212131, 15.00000000000000000, 6.263284095430918796 ) ) ;
#11305 = CARTESIAN_POINT ( 'NONE',  ( 17.39651004071838614, 47.93575266056826933, 6.500000000000032863 ) ) ;
#11306 = CARTESIAN_POINT ( 'NONE',  ( 12.63842701281683922, 14.55059781766744997, -9.846743663894590881 ) ) ;
#11307 = FILL_AREA_STYLE_COLOUR ( '', #3459 ) ;
#11308 = CARTESIAN_POINT ( 'NONE',  ( -14.64885433386000635, 14.95077488074853456, 1.748475581354107300 ) ) ;
#11309 = DIRECTION ( 'NONE',  ( 0.6246950475544238435, 0.7808688094430307203, 0.000000000000000000 ) ) ;
#11310 = CARTESIAN_POINT ( 'NONE',  ( 5.076628168052703671, 26.84226448433411960, 8.527530157486179263 ) ) ;
#11311 = CARTESIAN_POINT ( 'NONE',  ( 1.472469842513823179, 50.59226448433411605, -4.923371831947296329 ) ) ;
#11312 = ADVANCED_FACE ( 'NONE', ( #53055 ), #21092, .T. ) ;
#11313 = TOROIDAL_SURFACE ( 'NONE', #71981, 99.50000000000000000, 0.5000000000000000000 ) ;
#11314 = CARTESIAN_POINT ( 'NONE',  ( 21.09922568453595559, 47.04030133659708923, -6.408140936763230044 ) ) ;
#11315 = SURFACE_STYLE_USAGE ( .BOTH. , #35788 ) ;
#11316 = CARTESIAN_POINT ( 'NONE',  ( 7.361572987183170547, 2.050597817667451750, 9.846743663894590881 ) ) ;
#11317 = CARTESIAN_POINT ( 'NONE',  ( 17.20831665107776587, 22.88393115100078745, 7.208316651077764980 ) ) ;
#11319 = CARTESIAN_POINT ( 'NONE',  ( 0.1532563361054100626, 20.80059781766744464, -2.638427012816831230 ) ) ;
#11318 = CARTESIAN_POINT ( 'NONE',  ( 6.204703633549690345, 65.76208216824731778, -14.16423886937410259 ) ) ;
#11320 = CARTESIAN_POINT ( 'NONE',  ( -0.03743638938522149406, 44.25197528031021221, -6.399506433553973750 ) ) ;
#11321 = CARTESIAN_POINT ( 'NONE',  ( 1.472469842513823179, 66.42559781766745175, 4.923371831947296329 ) ) ;
#11322 = CARTESIAN_POINT ( 'NONE',  ( 17.08211943468705840, 5.137082168247300906, -12.26659068614894466 ) ) ;
#11323 = CARTESIAN_POINT ( 'NONE',  ( -2.266590686148945544, 37.22041550158063217, 7.082119434687048631 ) ) ;
#11324 = CARTESIAN_POINT ( 'NONE',  ( 5.076628168052704559, 35.17559781766745175, -8.527530157486179263 ) ) ;
#11325 = CARTESIAN_POINT ( 'NONE',  ( -2.393480905993250918, 0.5000000000000004441, 14.80781041047749724 ) ) ;
#11326 = CARTESIAN_POINT ( 'NONE',  ( -0.8801773607110991993, 22.85535201082150181, -2.915334737309923874 ) ) ;
#11327 = ADVANCED_FACE ( 'NONE', ( #61049 ), #15091, .T. ) ;
#11328 = CIRCLE ( 'NONE', #49632, 5.999999999999998224 ) ;
#11329 = CARTESIAN_POINT ( 'NONE',  ( 0.5774900079438590739, 62.64701867748817676, -5.440088680355550821 ) ) ;
#11330 = PRESENTATION_STYLE_ASSIGNMENT (( #12800 ) ) ;
#11331 = ORIENTED_EDGE ( 'NONE', *, *, #50459, .F. ) ;
#11332 = CARTESIAN_POINT ( 'NONE',  ( 10.00000000000000178, 50.37363466993042493, 12.81628187352647608 ) ) ;
#11333 = CARTESIAN_POINT ( 'NONE',  ( 7.084665262690076126, 47.02201867748818387, -10.88017736071110164 ) ) ;
#11334 = VERTEX_POINT ( 'NONE', #30548 ) ;
#11335 = DIRECTION ( 'NONE',  ( 0.000000000000000000, -1.000000000000000000, 0.000000000000000000 ) ) ;
#11336 = EDGE_LOOP ( 'NONE', ( #55541, #47242, #44700, #68412 ) ) ;
#11337 = CARTESIAN_POINT ( 'NONE',  ( 7.084665262690076126, 69.10535201082151957, 10.88017736071109987 ) ) ;
#11338 = CARTESIAN_POINT ( 'NONE',  ( 10.00000000000000000, 6.813685344154838397, -10.88017736071110342 ) ) ;
#11339 = CARTESIAN_POINT ( 'NONE',  ( 0.1532563361054100626, 0.8005978176674514168, -2.638427012816831230 ) ) ;
#11340 = CARTESIAN_POINT ( 'NONE',  ( 14.42956166533737417, 15.00000000000000533, -2.386684097925001247 ) ) ;
#11341 = CARTESIAN_POINT ( 'NONE',  ( 20.88017736071110875, 10.77201867748817143, -2.915334737309920765 ) ) ;
#11342 = CARTESIAN_POINT ( 'NONE',  ( 19.84674366389459266, 13.71726448433411782, -2.638427012816827677 ) ) ;
#11343 = CARTESIAN_POINT ( 'NONE',  ( 22.26659068614894466, 13.88708216824730179, 7.082119434687054849 ) ) ;
#11344 = CARTESIAN_POINT ( 'NONE',  ( 14.92337183194729988, 4.342264484334117824, -8.527530157486177487 ) ) ;
#11345 = CARTESIAN_POINT ( 'NONE',  ( 17.96484262340118221, 29.93868534415484106, 7.964842623401181321 ) ) ;
#11346 = CARTESIAN_POINT ( 'NONE',  ( 1.472469842513823179, 40.59226448433411605, -4.923371831947296329 ) ) ;
#11347 = EDGE_LOOP ( 'NONE', ( #84778, #23603, #43347, #38791 ) ) ;
#11348 = CARTESIAN_POINT ( 'NONE',  ( 2.791683348922240793, 46.63393115100077324, 7.208316651077764092 ) ) ;
#11349 = ORIENTED_EDGE ( 'NONE', *, *, #37081, .T. ) ;
#11350 = CARTESIAN_POINT ( 'NONE',  ( -12.07856007377833407, 15.00000000000000000, 8.022367888854752493 ) ) ;
#11351 = CARTESIAN_POINT ( 'NONE',  ( -0.8801773607110991993, 47.85535201082150536, -2.915334737309923874 ) ) ;
#11352 = CARTESIAN_POINT ( 'NONE',  ( 18.52753015748618282, 48.92559781766745886, -4.923371831947291888 ) ) ;
#11354 = DIRECTION ( 'NONE',  ( -0.000000000000000000, -1.000000000000000000, -0.000000000000000000 ) ) ;
#11353 = CARTESIAN_POINT ( 'NONE',  ( 19.42250999205614548, 5.980352010821504471, -5.440088680355545492 ) ) ;
#11355 = CARTESIAN_POINT ( 'NONE',  ( 4.559911319644449179, 57.23035201082150536, -9.422509992056141925 ) ) ;
#11356 = CARTESIAN_POINT ( 'NONE',  ( 10.00000000000000000, 1.813685344154838175, -10.88017736071110342 ) ) ;
#11357 = VECTOR ( 'NONE', #67869, 1000.000000000000000 ) ;
#11358 = AXIS2_PLACEMENT_3D ( 'NONE', #21497, #24457, #85439 ) ;
#11359 = ADVANCED_FACE ( 'NONE', ( #45563 ), #13587, .F. ) ;
#11360 = CARTESIAN_POINT ( 'NONE',  ( 6.565887622018943937, 40.16530133659708923, 12.81628187352647430 ) ) ;
#11361 = CARTESIAN_POINT ( 'NONE',  ( 20.88017736071110519, 30.56368534415484106, 2.639326808657452039E-16 ) ) ;
#11362 = CARTESIAN_POINT ( 'NONE',  ( -45.94000000000001194, 99.99999999999998579, 12.00000000000000000 ) ) ;
#11363 = VERTEX_POINT ( 'NONE', #21594 ) ;
#11364 = CARTESIAN_POINT ( 'NONE',  ( 6.565887622018943937, 48.08196800326375353, -12.81628187352647608 ) ) ;
#11365 = CARTESIAN_POINT ( 'NONE',  ( 20.88017736071110164, 30.35535201082151247, 2.915334737309930979 ) ) ;
#11366 = VERTEX_POINT ( 'NONE', #52084 ) ;
#11367 = DIRECTION ( 'NONE',  ( 0.000000000000000000, 1.000000000000000000, 0.000000000000000000 ) ) ;
#11368 = VERTEX_POINT ( 'NONE', #82577 ) ;
#11369 = CARTESIAN_POINT ( 'NONE',  ( 18.52753015748618282, 63.92559781766745886, -4.923371831947291888 ) ) ;
#11371 = CARTESIAN_POINT ( 'NONE',  ( 10.00000000000000000, 49.75893115100078745, -9.846743663894594434 ) ) ;
#11370 = CARTESIAN_POINT ( 'NONE',  ( 10.00000000000000178, 7.258931151000785675, 9.846743663894594434 ) ) ;
#11372 = CARTESIAN_POINT ( 'NONE',  ( 17.96484262340118221, 24.93868534415484461, 7.964842623401181321 ) ) ;
#11373 = AXIS2_PLACEMENT_3D ( 'NONE', #11749, #86775, #3274 ) ;
#11374 = CARTESIAN_POINT ( 'NONE',  ( 12.63842701281683034, 37.46726448433411605, 9.846743663894596210 ) ) ;
#11375 = DIRECTION ( 'NONE',  ( -6.938893903907222067E-15, 0.000000000000000000, -1.000000000000000000 ) ) ;
#11376 = DIRECTION ( 'NONE',  ( -0.000000000000000000, -0.000000000000000000, 1.000000000000000000 ) ) ;
#11378 = CARTESIAN_POINT ( 'NONE',  ( 0.1532563361054083140, 11.00893115100078568, 1.131784320476157264E-15 ) ) ;
#11377 = CARTESIAN_POINT ( 'NONE',  ( 0.1532563361054082862, 26.21726448433411605, 2.638427012816831674 ) ) ;
#11379 = CARTESIAN_POINT ( 'NONE',  ( 18.04007052943773104, 28.01528370094808551, 5.767676674365834977 ) ) ;
#11381 = ORIENTED_EDGE ( 'NONE', *, *, #3476, .F. ) ;
#11380 = CARTESIAN_POINT ( 'NONE',  ( 10.00000000000000000, 54.75893115100078745, -9.846743663894594434 ) ) ;
#11382 = VECTOR ( 'NONE', #82121, 1000.000000000000000 ) ;
#11383 = CARTESIAN_POINT ( 'NONE',  ( 0.8952175423694405110, 8.525762395770811963, 5.990408912944244157 ) ) ;
#11384 = CARTESIAN_POINT ( 'NONE',  ( 13.43411237798105340, 20.58196800326374643, 12.81628187352647963 ) ) ;
#11385 = CARTESIAN_POINT ( 'NONE',  ( 7.361572987183170547, 47.05059781766745175, 9.846743663894590881 ) ) ;
#11386 = CARTESIAN_POINT ( 'NONE',  ( -0.1503990784575321704, 8.101585745166424601, 6.262539305110068177 ) ) ;
#11387 = CARTESIAN_POINT ( 'NONE',  ( 24.16423886937410614, 54.30374883491396787, 8.672049930838204340E-16 ) ) ;
#11388 = CARTESIAN_POINT ( 'NONE',  ( 18.52753015748618282, 23.92559781766745530, -4.923371831947291888 ) ) ;
#11389 = STYLED_ITEM ( 'NONE', ( #58029 ), #46610 ) ;
#11390 = CARTESIAN_POINT ( 'NONE',  ( 20.00000000000000711, 79.40087001978916703, 4.999999999999999112 ) ) ;
#11391 = CARTESIAN_POINT ( 'NONE',  ( 6.204703633549690345, 57.84541550158063927, 14.16423886937410082 ) ) ;
#11392 = CARTESIAN_POINT ( 'NONE',  ( 19.84674366389459621, 58.50893115100078745, 7.409399052514197653E-17 ) ) ;
#11393 = CARTESIAN_POINT ( 'NONE',  ( 10.00000000000000000, 1.813685344154838175, -10.88017736071110342 ) ) ;
#11394 = CARTESIAN_POINT ( 'NONE',  ( 22.26659068614895176, 39.72041550158063217, -7.082119434687042414 ) ) ;
#11395 = CARTESIAN_POINT ( 'NONE',  ( 24.16423886937409904, 39.09541550158062506, 3.795296366450317205 ) ) ;
#11396 = DIRECTION ( 'NONE',  ( -0.000000000000000000, -1.000000000000000000, -0.000000000000000000 ) ) ;
#11397 = AXIS2_PLACEMENT_3D ( 'NONE', #93589, #40606, #34056 ) ;
#11399 = CARTESIAN_POINT ( 'NONE',  ( 0.1532563361054083140, 56.00893115100078745, 1.131784320476157264E-15 ) ) ;
#11398 = DIRECTION ( 'NONE',  ( -0.000000000000000000, -1.000000000000000000, -0.000000000000000000 ) ) ;
#11400 = EDGE_LOOP ( 'NONE', ( #95918, #52061, #40696, #77815, #41110 ) ) ;
#11401 = CARTESIAN_POINT ( 'NONE',  ( 12.91533473730993009, 46.60535201082150536, -10.88017736071109987 ) ) ;
#11402 = CARTESIAN_POINT ( 'NONE',  ( 11.10714268220738354, -52.69759663682445705, 3.750000000000000000 ) ) ;
#11403 = CARTESIAN_POINT ( 'NONE',  ( 17.72850354356589619, 33.99078749795493337, -9.999999999999998224 ) ) ;
#11404 = CARTESIAN_POINT ( 'NONE',  ( 12.63842701281683922, 54.55059781766745175, -9.846743663894590881 ) ) ;
#11405 = EDGE_CURVE ( 'NONE', #1162, #31031, #6579, .T. ) ;
#11406 = EDGE_LOOP ( 'NONE', ( #51286, #83677, #74403, #25901, #5133, #59629, #49323, #43801, #43659, #33434 ) ) ;
#11407 = CARTESIAN_POINT ( 'NONE',  ( 6.204703633549690345, 22.84541550158062861, 14.16423886937410082 ) ) ;
#11408 = EDGE_CURVE ( 'NONE', #33129, #96487, #598, .T. ) ;
#11409 = EDGE_CURVE ( 'NONE', #79587, #8141, #42644, .T. ) ;
#11410 = DIRECTION ( 'NONE',  ( 0.000000000000000000, 0.000000000000000000, 1.000000000000000000 ) ) ;
#11412 = CYLINDRICAL_SURFACE ( 'NONE', #2584, 11.92686044187656513 ) ;
#11411 = CARTESIAN_POINT ( 'NONE',  ( -3.500000001558553286, 0.09224605988788428523, -2.499999999999595879 ) ) ;
#11413 = CARTESIAN_POINT ( 'NONE',  ( 0.5774900079438607392, 23.48035201082150536, 5.440088680355550821 ) ) ;
#11414 = CARTESIAN_POINT ( 'NONE',  ( -1.099225684535947600, 19.54030133659708568, 6.408140936763237150 ) ) ;
#11415 = CARTESIAN_POINT ( 'NONE',  ( 20.24186590665277308, 61.76028685723174050, 6.114288769123050749 ) ) ;
#11416 = CARTESIAN_POINT ( 'NONE',  ( 17.20831665107776587, 12.88393115100078390, 7.208316651077764980 ) ) ;
#11417 = ORIENTED_EDGE ( 'NONE', *, *, #62641, .T. ) ;
#11418 = CARTESIAN_POINT ( 'NONE',  ( 6.575338752097509065, -50.90849809615561838, -3.999999999999999556 ) ) ;
#11419 = CARTESIAN_POINT ( 'NONE',  ( 24.16423886937409904, 34.09541550158064638, 3.795296366450317205 ) ) ;
#11420 = CARTESIAN_POINT ( 'NONE',  ( -0.3289641300568005855, 10.10497603579417536, 5.963430220938281678 ) ) ;
#11421 = PRESENTATION_STYLE_ASSIGNMENT (( #42420 ) ) ;
#11422 = CARTESIAN_POINT ( 'NONE',  ( 20.88017736071110164, 5.355352010821503583, 2.915334737309930979 ) ) ;
#11423 = CARTESIAN_POINT ( 'NONE',  ( 0.2751277870542967463, 70.00000000000000000, 6.000000000000000000 ) ) ;
#11424 = CARTESIAN_POINT ( 'NONE',  ( -19.00000000000000000, 75.76920769491739804, -2.900000000000000799 ) ) ;
#11425 = CARTESIAN_POINT ( 'NONE',  ( 15.44008868035555260, 34.73035201082151247, 9.422509992056143702 ) ) ;
#11426 = CARTESIAN_POINT ( 'NONE',  ( 19.42250999205614548, 40.98035201082150536, -5.440088680355545492 ) ) ;
#11427 = CARTESIAN_POINT ( 'NONE',  ( -2.816281873526473856, 19.33196800326375708, 3.434112377981055619 ) ) ;
#11428 = CARTESIAN_POINT ( 'NONE',  ( 0.1532563361054083140, 66.00893115100079456, 1.131784320476157264E-15 ) ) ;
#11429 = CARTESIAN_POINT ( 'NONE',  ( 0.2751277870542979120, 15.30223176428831344, 6.500000000000003553 ) ) ;
#11430 = CARTESIAN_POINT ( 'NONE',  ( 19.84674366389459266, 13.30059781766745353, 2.638427012816836559 ) ) ;
#11431 = VERTEX_POINT ( 'NONE', #47528 ) ;
#11432 = CARTESIAN_POINT ( 'NONE',  ( 18.17829156368509302, 49.16792564121895026, 6.499999999999931610 ) ) ;
#11433 = CARTESIAN_POINT ( 'NONE',  ( 19.42250999205614548, 40.98035201082150536, -5.440088680355545492 ) ) ;
#11434 = UNCERTAINTY_MEASURE_WITH_UNIT (LENGTH_MEASURE( 1.000000000000000082E-05 ), #57163, 'distance_accuracy_value', 'NONE');
#11435 = CARTESIAN_POINT ( 'NONE',  ( -2.816281873526471635, -1.084698663402913210, -3.434112377981056508 ) ) ;
#11436 = CARTESIAN_POINT ( 'NONE',  ( -0.8801773607111008646, 63.27201867748817676, 2.915334737309923430 ) ) ;
#11437 = CARTESIAN_POINT ( 'NONE',  ( 0.1532563361054083140, 31.00893115100078390, 1.131784320476157264E-15 ) ) ;
#11438 = CARTESIAN_POINT ( 'NONE',  ( 6.565887622018943937, 35.16530133659708923, 12.81628187352647430 ) ) ;
#11440 = CARTESIAN_POINT ( 'NONE',  ( -4.856044144387799300, 15.00000000000000888, 13.79699902221156371 ) ) ;
#11439 = CARTESIAN_POINT ( 'NONE',  ( 12.63842701281683922, 9.550597817667449974, -9.846743663894590881 ) ) ;
#11441 = ORIENTED_EDGE ( 'NONE', *, *, #69115, .T. ) ;
#11442 = LINE ( 'NONE', #87438, #78845 ) ;
#11443 = CARTESIAN_POINT ( 'NONE',  ( 2.746530213673227803E-16, 21.83999999999999986, 0.000000000000000000 ) ) ;
#11444 = CARTESIAN_POINT ( 'NONE',  ( 0.5774900079438590739, 12.64701867748817143, -5.440088680355550821 ) ) ;
#11445 = CARTESIAN_POINT ( 'NONE',  ( 16.40814093676324603, 62.45696800326376064, -11.09922568453594671 ) ) ;
#11446 = EDGE_CURVE ( 'NONE', #83367, #22095, #11730, .T. ) ;
#11447 = CARTESIAN_POINT ( 'NONE',  ( 0.1532563361054100626, 35.80059781766745175, -2.638427012816831230 ) ) ;
#11448 = CARTESIAN_POINT ( 'NONE',  ( 12.91533473730993009, 16.60535201082150891, -10.88017736071109987 ) ) ;
#11449 = CARTESIAN_POINT ( 'NONE',  ( 15.44008868035555793, 6.397018677488171434, -9.422509992056140149 ) ) ;
#11450 = VERTEX_POINT ( 'NONE', #1069 ) ;
#11451 = CARTESIAN_POINT ( 'NONE',  ( 4.559911319644449179, 12.23035201082150536, -9.422509992056141925 ) ) ;
#11452 = CARTESIAN_POINT ( 'NONE',  ( 20.88017736071110164, 25.35535201082150891, 2.915334737309930979 ) ) ;
#11453 = EDGE_CURVE ( 'NONE', #83674, #39649, #10032, .T. ) ;
#11454 = LINE ( 'NONE', #96953, #7401 ) ;
#11455 = PRESENTATION_LAYER_ASSIGNMENT (  '', '', ( #49765 ) ) ;
#11456 = ORIENTED_EDGE ( 'NONE', *, *, #8812, .T. ) ;
#11457 = CARTESIAN_POINT ( 'NONE',  ( 2.791683348922240793, 61.63393115100079456, 7.208316651077764092 ) ) ;
#11458 = CARTESIAN_POINT ( 'NONE',  ( -0.8801773607111009756, 23.06368534415484106, 1.068504757029289695E-15 ) ) ;
#11459 = CARTESIAN_POINT ( 'NONE',  ( 10.00000000000000178, 57.25893115100078745, 9.846743663894594434 ) ) ;
#11460 = CARTESIAN_POINT ( 'NONE',  ( -1.099225684535947600, 48.70696800326375353, -6.408140936763238038 ) ) ;
#11461 = FACE_OUTER_BOUND ( 'NONE', #34534, .T. ) ;
#11462 = CARTESIAN_POINT ( 'NONE',  ( 22.26659068614894466, 28.88708216824730357, 7.082119434687054849 ) ) ;
#11463 = CARTESIAN_POINT ( 'NONE',  ( 0.5774900079438590739, 42.64701867748816966, -5.440088680355550821 ) ) ;
#11464 = CARTESIAN_POINT ( 'NONE',  ( 17.96484262340118221, 14.93868534415484106, 7.964842623401181321 ) ) ;
#11465 = CARTESIAN_POINT ( 'NONE',  ( 10.00000000000000000, 49.75893115100078745, -9.846743663894594434 ) ) ;
#11466 = CARTESIAN_POINT ( 'NONE',  ( -11.07344383391687259, -96.04710479529198608, -3.750000000000000888 ) ) ;
#11467 = CARTESIAN_POINT ( 'NONE',  ( 0.1532563361054082862, 56.21726448433411605, 2.638427012816831674 ) ) ;
#11468 = STYLED_ITEM ( 'NONE', ( #91894 ), #47247 ) ;
#11469 = CARTESIAN_POINT ( 'NONE',  ( 20.15039907845753930, 70.00000000000000000, -6.262539305110068177 ) ) ;
#11470 = CARTESIAN_POINT ( 'NONE',  ( 5.076628168052703671, 1.842264484334118047, 8.527530157486179263 ) ) ;
#11471 = CARTESIAN_POINT ( 'NONE',  ( 6.408140936763243367, -34.20969866340291077, 11.09922568453594494 ) ) ;
#11472 = VERTEX_POINT ( 'NONE', #92048 ) ;
#11473 = AXIS2_PLACEMENT_3D ( 'NONE', #66093, #21106, #44080 ) ;
#11474 = CARTESIAN_POINT ( 'NONE',  ( 2.035157376598822676, 12.43868534415483751, -7.964842623401177768 ) ) ;
#11475 = CARTESIAN_POINT ( 'NONE',  ( 5.076628168052704559, 5.175597817667451750, -8.527530157486179263 ) ) ;
#11476 = CARTESIAN_POINT ( 'NONE',  ( 3.591859063236763294, -1.709698663402913210, -11.09922568453595026 ) ) ;
#11477 = CARTESIAN_POINT ( 'NONE',  ( 7.084665262690076126, 62.02201867748816966, -10.88017736071110164 ) ) ;
#11479 = CARTESIAN_POINT ( 'NONE',  ( 6.565887622018943937, 40.16530133659708923, 12.81628187352647430 ) ) ;
#11478 = CARTESIAN_POINT ( 'NONE',  ( 10.00000000000000178, 24.31368534415484106, 10.88017736071110342 ) ) ;
#11480 = CARTESIAN_POINT ( 'NONE',  ( 13.79529636645031943, 25.34541550158063572, -14.16423886937409904 ) ) ;
#11481 = CARTESIAN_POINT ( 'NONE',  ( 6.565887622018943937, 60.16530133659707502, 12.81628187352647430 ) ) ;
#11482 = EDGE_LOOP ( 'NONE', ( #38481, #88483, #86375, #21689, #80007, #90829 ) ) ;
#11483 = CARTESIAN_POINT ( 'NONE',  ( 7.361572987183170547, 67.05059781766746596, 9.846743663894590881 ) ) ;
#11484 = CARTESIAN_POINT ( 'NONE',  ( -3.750000000000000000, 36.75000000000000000, 2.500000000000000000 ) ) ;
#11485 = CARTESIAN_POINT ( 'NONE',  ( -0.8801773607111008646, 28.27201867748817321, 2.915334737309923430 ) ) ;
#11486 = CARTESIAN_POINT ( 'NONE',  ( 7.361572987183169658, 64.96726448433412315, -9.846743663894592657 ) ) ;
#11487 = ORIENTED_EDGE ( 'NONE', *, *, #35113, .T. ) ;
#11488 = CARTESIAN_POINT ( 'NONE',  ( 18.52753015748617571, 8.092264484334117824, 4.923371831947298993 ) ) ;
#11489 = CARTESIAN_POINT ( 'NONE',  ( 14.99847009497944406, 0.5000000000000004441, 0.2142307401081381124 ) ) ;
#11490 = CARTESIAN_POINT ( 'NONE',  ( 17.20831665107776587, 14.13393115100078568, -7.208316651077762316 ) ) ;
#11491 = CARTESIAN_POINT ( 'NONE',  ( 0.1532563361054082862, 21.21726448433412315, 2.638427012816831674 ) ) ;
#11492 = CARTESIAN_POINT ( 'NONE',  ( 7.361572987183170547, 12.05059781766744997, 9.846743663894590881 ) ) ;
#11493 = EDGE_CURVE ( 'NONE', #43585, #18004, #46544, .T. ) ;
#11495 = CARTESIAN_POINT ( 'NONE',  ( 8.879999999999991900, 76.07179676972447169, 6.250000000000000000 ) ) ;
#11494 = CARTESIAN_POINT ( 'NONE',  ( 7.084665262690076126, 52.02201867748816255, -10.88017736071110164 ) ) ;
#11496 = CARTESIAN_POINT ( 'NONE',  ( -0.8801773607111009756, 68.06368534415484817, 1.068504757029289695E-15 ) ) ;
#11498 = EDGE_LOOP ( 'NONE', ( #71210, #1573, #92198 ) ) ;
#11497 = CARTESIAN_POINT ( 'NONE',  ( 17.20831665107776587, 12.88393115100078390, 7.208316651077764980 ) ) ;
#11499 = CIRCLE ( 'NONE', #37075, 0.4999999999999998335 ) ;
#11500 = PLANE ( 'NONE',  #11880 ) ;
#11501 = CARTESIAN_POINT ( 'NONE',  ( 12.63842701281683034, 57.46726448433411605, 9.846743663894596210 ) ) ;
#11502 = ORIENTED_EDGE ( 'NONE', *, *, #67189, .F. ) ;
#11503 = CARTESIAN_POINT ( 'NONE',  ( 17.08211943468705130, 23.47041550158063572, 12.26659068614894998 ) ) ;
#11504 = UNCERTAINTY_MEASURE_WITH_UNIT (LENGTH_MEASURE( 1.000000000000000082E-05 ), #29322, 'distance_accuracy_value', 'NONE');
#11505 = DIRECTION ( 'NONE',  ( -0.000000000000000000, -0.000000000000000000, 1.000000000000000000 ) ) ;
#11506 = CARTESIAN_POINT ( 'NONE',  ( -2.266590686148945544, 11.38708216824730179, -7.082119434687050408 ) ) ;
#11507 = CARTESIAN_POINT ( 'NONE',  ( -2.266590686148945544, 27.22041550158063572, 7.082119434687048631 ) ) ;
#11508 = CARTESIAN_POINT ( 'NONE',  ( -2.999999999999999556, 22.11937003968011695, 0.000000000000000000 ) ) ;
#11509 = FILL_AREA_STYLE_COLOUR ( '', #41828 ) ;
#11510 = CARTESIAN_POINT ( 'NONE',  ( 4.559911319644449179, 33.89701867748817676, 9.422509992056141925 ) ) ;
#11511 = VERTEX_POINT ( 'NONE', #39058 ) ;
#11512 = CARTESIAN_POINT ( 'NONE',  ( 0.1532563361054082862, 16.21726448433411960, 2.638427012816831674 ) ) ;
#11513 = ADVANCED_FACE ( 'NONE', ( #55018 ), #33011, .T. ) ;
#11515 = CARTESIAN_POINT ( 'NONE',  ( 14.92337183194729988, 14.34226448433411782, -8.527530157486177487 ) ) ;
#11514 = CARTESIAN_POINT ( 'NONE',  ( 19.42250999205614193, 60.14701867748817676, 5.440088680355555262 ) ) ;
#11516 = CARTESIAN_POINT ( 'NONE',  ( 0.6178305044545838731, 49.74863466993041072, 9.382169495545420901 ) ) ;
#11517 = CARTESIAN_POINT ( 'NONE',  ( 19.84674366389459266, 38.71726448433412315, -2.638427012816827677 ) ) ;
#11518 = DIRECTION ( 'NONE',  ( 0.000000000000000000, 1.000000000000000000, 0.000000000000000000 ) ) ;
#11519 = CARTESIAN_POINT ( 'NONE',  ( 22.81628187352648496, 31.83196800326375353, -3.434112377981050290 ) ) ;
#11520 = CARTESIAN_POINT ( 'NONE',  ( 14.16423886937410437, -35.90458449841936783, 3.795296366450304770 ) ) ;
#11521 = AXIS2_PLACEMENT_3D ( 'NONE', #35206, #41760, #3260 ) ;
#11522 = CARTESIAN_POINT ( 'NONE',  ( 19.84674366389459266, 23.71726448433412315, -2.638427012816827677 ) ) ;
#11523 = EDGE_CURVE ( 'NONE', #83267, #75676, #84199, .T. ) ;
#11524 = CARTESIAN_POINT ( 'NONE',  ( -4.164238869374099039, 6.803748834913967869, 8.674139862899312516E-16 ) ) ;
#11525 = ORIENTED_EDGE ( 'NONE', *, *, #18796, .F. ) ;
#11526 = ORIENTED_EDGE ( 'NONE', *, *, #9656, .T. ) ;
#11527 = EDGE_CURVE ( 'NONE', #1561, #20489, #38565, .T. ) ;
#11528 = CARTESIAN_POINT ( 'NONE',  ( 4.559911319644449179, 52.23035201082151247, -9.422509992056141925 ) ) ;
#11529 = CARTESIAN_POINT ( 'NONE',  ( 4.559911319644449179, 58.89701867748817676, 9.422509992056141925 ) ) ;
#11530 = CARTESIAN_POINT ( 'NONE',  ( 17.08211943468705130, 43.47041550158063927, 12.26659068614894998 ) ) ;
#11531 = CARTESIAN_POINT ( 'NONE',  ( 17.20831665107776587, 52.88393115100078035, 7.208316651077764980 ) ) ;
#11532 = CARTESIAN_POINT ( 'NONE',  ( 7.361572987183170547, 17.05059781766745530, 9.846743663894590881 ) ) ;
#11533 = AXIS2_PLACEMENT_3D ( 'NONE', #87619, #41656, #86654 ) ;
#11534 = CARTESIAN_POINT ( 'NONE',  ( -2.815433093576914736, 14.49999999999999112, -14.73340885523760413 ) ) ;
#11535 = CARTESIAN_POINT ( 'NONE',  ( 0.5774900079438590739, 37.64701867748817676, -5.440088680355550821 ) ) ;
#11536 =( GEOMETRIC_REPRESENTATION_CONTEXT ( 3 ) GLOBAL_UNCERTAINTY_ASSIGNED_CONTEXT ( ( #41536 ) ) GLOBAL_UNIT_ASSIGNED_CONTEXT ( ( #51555, #6059, #42573 ) ) REPRESENTATION_CONTEXT ( 'NONE', 'WORKASPACE' ) );
#11537 = DIRECTION ( 'NONE',  ( 0.000000000000000000, 0.000000000000000000, 1.000000000000000000 ) ) ;
#11538 = CARTESIAN_POINT ( 'NONE',  ( 12.63842701281683034, 57.46726448433411605, 9.846743663894596210 ) ) ;
#11539 = CARTESIAN_POINT ( 'NONE',  ( 10.88017736071109987, 15.77201867748817854, -2.915334737309928315 ) ) ;
#11540 = CARTESIAN_POINT ( 'NONE',  ( 0.000000000000000000, -97.00000000000000000, -3.750000000000000000 ) ) ;
#11541 = AXIS2_PLACEMENT_3D ( 'NONE', #36507, #82493, #98018 ) ;
#11542 = CARTESIAN_POINT ( 'NONE',  ( 4.559911319644449179, 62.23035201082150536, -9.422509992056141925 ) ) ;
#11543 = SURFACE_STYLE_USAGE ( .BOTH. , #6027 ) ;
#11544 = FACE_OUTER_BOUND ( 'NONE', #37227, .T. ) ;
#11545 = STYLED_ITEM ( 'NONE', ( #14269 ), #73503 ) ;
#11546 = CARTESIAN_POINT ( 'NONE',  ( 10.00000000000000000, -0.2410688489992152128, -9.846743663894594434 ) ) ;
#11547 = CARTESIAN_POINT ( 'NONE',  ( 0.1532563361054100626, 0.8005978176674514168, -2.638427012816831230 ) ) ;
#11548 = CARTESIAN_POINT ( 'NONE',  ( 5.073789285385978509, 0.000000000000000000, -1.998618750576372838 ) ) ;
#11549 = CARTESIAN_POINT ( 'NONE',  ( 12.63842701281683922, 39.55059781766744464, -9.846743663894590881 ) ) ;
#11550 = CARTESIAN_POINT ( 'NONE',  ( 7.084665262690076126, 17.02201867748817676, -10.88017736071110164 ) ) ;
#11551 = CARTESIAN_POINT ( 'NONE',  ( 17.20831665107776587, 64.13393115100079456, -7.208316651077762316 ) ) ;
#11553 = CARTESIAN_POINT ( 'NONE',  ( -0.9940297508538862292, 15.00000000000000000, 14.21528771620248932 ) ) ;
#11552 = CARTESIAN_POINT ( 'NONE',  ( 20.88017736071110875, 30.77201867748816966, -2.915334737309920765 ) ) ;
#11554 = CARTESIAN_POINT ( 'NONE',  ( 18.29284471827482506, 65.40189080397281884, -6.499999999999912070 ) ) ;
#11555 = CARTESIAN_POINT ( 'NONE',  ( -1.099225684535947600, 38.70696800326375353, -6.408140936763238038 ) ) ;
#11556 = VERTEX_POINT ( 'NONE', #9532 ) ;
#11557 = CARTESIAN_POINT ( 'NONE',  ( 10.00000000000000000, 51.81368534415484106, -10.88017736071110342 ) ) ;
#11559 = CARTESIAN_POINT ( 'NONE',  ( 18.04007052943773459, 18.01528370094808196, 5.767676674365826983 ) ) ;
#11558 = CARTESIAN_POINT ( 'NONE',  ( 0.6178305044545818747, 18.49863466993041428, -9.382169495545419124 ) ) ;
#11560 = EDGE_CURVE ( 'NONE', #57214, #57542, #32520, .T. ) ;
#11561 = CARTESIAN_POINT ( 'NONE',  ( 17.96484262340118221, 21.18868534415483396, -7.964842623401177768 ) ) ;
#11562 = CARTESIAN_POINT ( 'NONE',  ( -4.164238869374099927, 67.01208216824728936, 3.795296366450308767 ) ) ;
#11563 = MECHANICAL_DESIGN_GEOMETRIC_PRESENTATION_REPRESENTATION (  '', ( #29182 ), #80218 ) ;
#11564 = CARTESIAN_POINT ( 'NONE',  ( 14.92337183194729633, 37.67559781766745175, 8.527530157486181039 ) ) ;
#11565 = CARTESIAN_POINT ( 'NONE',  ( 10.00000000000000178, 7.258931151000785675, 9.846743663894594434 ) ) ;
#11566 = CARTESIAN_POINT ( 'NONE',  ( 12.91533473730993009, 56.60535201082151247, -10.88017736071109987 ) ) ;
#11567 = B_SPLINE_CURVE_WITH_KNOTS ( 'NONE', 3,
 ( #72851, #94380, #19376, #70913 ),
 .UNSPECIFIED., .F., .F.,
 ( 4, 4 ),
 ( 0.000000000000000000, 0.002657014572711341102 ),
 .UNSPECIFIED. ) ;
#11568 = CARTESIAN_POINT ( 'NONE',  ( 0.000000000000000000, 0.000000000000000000, 0.000000000000000000 ) ) ;
#11569 = CARTESIAN_POINT ( 'NONE',  ( 10.00000000000000000, 35.55374883491396787, -14.16423886937410082 ) ) ;
#11570 = DIRECTION ( 'NONE',  ( -1.000000000000000000, 0.000000000000000000, 0.000000000000000000 ) ) ;
#11571 = DIRECTION ( 'NONE',  ( -0.9975640502598243087, 0.06975647374412544122, 0.000000000000000000 ) ) ;
#11572 = ORIENTED_EDGE ( 'NONE', *, *, #35734, .F. ) ;
#11573 = ORIENTED_EDGE ( 'NONE', *, *, #51593, .T. ) ;
#11574 = TOROIDAL_SURFACE ( 'NONE', #48252, 7.538348415311010520, 7.000000000000000000 ) ;
#11575 = CARTESIAN_POINT ( 'NONE',  ( 24.16423886937410614, 54.51208216824730357, -3.795296366450302550 ) ) ;
#11576 = CARTESIAN_POINT ( 'NONE',  ( -2.266590686148945544, 56.38708216824731068, -7.082119434687050408 ) ) ;
#11577 = CARTESIAN_POINT ( 'NONE',  ( 2.791683348922240793, 11.63393115100078568, 7.208316651077764092 ) ) ;
#11578 = CARTESIAN_POINT ( 'NONE',  ( -1.099225684535947600, 18.70696800326375353, -6.408140936763238038 ) ) ;
#11579 = DIRECTION ( 'NONE',  ( -0.000000000000000000, -1.000000000000000000, -0.000000000000000000 ) ) ;
#11580 = FACE_OUTER_BOUND ( 'NONE', #795, .T. ) ;
#11582 = CARTESIAN_POINT ( 'NONE',  ( 22.81628187352648496, 36.83196800326376064, -3.434112377981050290 ) ) ;
#11581 = CARTESIAN_POINT ( 'NONE',  ( -13.55255535720598026, -0.03417435944610275333, 4.403492169842870396 ) ) ;
#11583 = CARTESIAN_POINT ( 'NONE',  ( 10.00000000000000000, 40.55374883491397497, -14.16423886937410082 ) ) ;
#11584 = CARTESIAN_POINT ( 'NONE',  ( -4.856092091437838043, 14.99999999999808686, -13.79590085421244439 ) ) ;
#11585 = CARTESIAN_POINT ( 'NONE',  ( 18.52753015748617571, 13.09226448433411960, 4.923371831947298993 ) ) ;
#11586 = CARTESIAN_POINT ( 'NONE',  ( 2.638427012816835227, -2.532735515665880843, 9.846743663894590881 ) ) ;
#11587 = VERTEX_POINT ( 'NONE', #48504 ) ;
#11588 = LINE ( 'NONE', #50080, #31643 ) ;
#11589 = CARTESIAN_POINT ( 'NONE',  ( 18.52753015748617571, 18.09226448433411960, 4.923371831947298993 ) ) ;
#11590 = SURFACE_SIDE_STYLE ('',( #35569 ) ) ;
#11591 = ORIENTED_EDGE ( 'NONE', *, *, #72949, .F. ) ;
#11593 = CARTESIAN_POINT ( 'NONE',  ( 7.084665262690076126, 19.10535201082150181, 10.88017736071109987 ) ) ;
#11592 = CARTESIAN_POINT ( 'NONE',  ( 12.91533473730992121, 9.522018677488171434, 10.88017736071110164 ) ) ;
#11595 = CARTESIAN_POINT ( 'NONE',  ( -2.816281873526473856, -0.6680319967362464695, 3.434112377981055619 ) ) ;
#11594 = CARTESIAN_POINT ( 'NONE',  ( 1.472469842513823179, 56.42559781766745886, 4.923371831947296329 ) ) ;
#11596 = CIRCLE ( 'NONE', #40377, 9.999999999999994671 ) ;
#11597 = CARTESIAN_POINT ( 'NONE',  ( 6.565887622018943937, 18.08196800326375708, -12.81628187352647608 ) ) ;
#11598 = ORIENTED_EDGE ( 'NONE', *, *, #17411, .T. ) ;
#11599 = MECHANICAL_DESIGN_GEOMETRIC_PRESENTATION_REPRESENTATION (  '', ( #57913 ), #61135 ) ;
#11600 = CARTESIAN_POINT ( 'NONE',  ( 24.16423886937409904, 59.09541550158063217, 3.795296366450317205 ) ) ;
#11601 = VERTEX_POINT ( 'NONE', #69060 ) ;
#11602 = AXIS2_PLACEMENT_3D ( 'NONE', #77878, #32375, #69904 ) ;
#11603 = CARTESIAN_POINT ( 'NONE',  ( -2.266590686148945544, 62.22041550158063927, 7.082119434687048631 ) ) ;
#11604 = VERTEX_POINT ( 'NONE', #31040 ) ;
#11605 = CARTESIAN_POINT ( 'NONE',  ( -0.8801773607111009756, 28.06368534415484106, 1.068504757029289695E-15 ) ) ;
#11606 = CARTESIAN_POINT ( 'NONE',  ( 15.44008868035555793, 51.39701867748816966, -9.422509992056140149 ) ) ;
#11607 = CARTESIAN_POINT ( 'NONE',  ( 4.559911319644449179, 57.23035201082150536, -9.422509992056141925 ) ) ;
#11608 = AXIS2_PLACEMENT_3D ( 'NONE', #63296, #72276, #79299 ) ;
#11609 = SURFACE_STYLE_FILL_AREA ( #50598 ) ;
#11610 = CARTESIAN_POINT ( 'NONE',  ( 12.91533473730992121, 34.52201867748817676, 10.88017736071110164 ) ) ;
#11611 = EDGE_CURVE ( 'NONE', #5083, #1372, #37957, .T. ) ;
#11612 = VECTOR ( 'NONE', #33566, 1000.000000000000000 ) ;
#11613 = ORIENTED_EDGE ( 'NONE', *, *, #4119, .F. ) ;
#11614 = CARTESIAN_POINT ( 'NONE',  ( 1.472469842513823179, 10.59226448433411782, -4.923371831947296329 ) ) ;
#11615 = ORIENTED_EDGE ( 'NONE', *, *, #9438, .T. ) ;
#11616 = CARTESIAN_POINT ( 'NONE',  ( 10.47195283036333180, -40.28639508448244300, 4.000000000000000000 ) ) ;
#11617 = CARTESIAN_POINT ( 'NONE',  ( 5.076628168052703671, 46.84226448433412315, 8.527530157486179263 ) ) ;
#11618 = DIRECTION ( 'NONE',  ( 1.000000000000000000, 1.049065152435176504E-16, -0.000000000000000000 ) ) ;
#11619 = CARTESIAN_POINT ( 'NONE',  ( 16.40814093676323893, 60.79030133659709634, 11.09922568453595026 ) ) ;
#11620 = VECTOR ( 'NONE', #28950, 1000.000000000000000 ) ;
#11621 = CARTESIAN_POINT ( 'NONE',  ( -7.045329894599615450, -66.66420243593404393, 3.750000000000000444 ) ) ;
#11622 = VERTEX_POINT ( 'NONE', #19007 ) ;
#11623 = CARTESIAN_POINT ( 'NONE',  ( -14.89999999999999680, 98.49999999999998579, -8.525133428036873795 ) ) ;
#11624 = DIRECTION ( 'NONE',  ( -0.7009092642998523415, 0.000000000000000000, 0.7132504491541801217 ) ) ;
#11626 = CARTESIAN_POINT ( 'NONE',  ( 7.361572987183169658, 29.96726448433411960, -9.846743663894592657 ) ) ;
#11625 = DIRECTION ( 'NONE',  ( 0.000000000000000000, 1.000000000000000000, -0.000000000000000000 ) ) ;
#11627 = CARTESIAN_POINT ( 'NONE',  ( 10.00000000000000000, 55.55374883491396787, -14.16423886937410082 ) ) ;
#11628 = CARTESIAN_POINT ( 'NONE',  ( 12.11353679309432785, 14.95037110518055812, 8.421373815019714826 ) ) ;
#11629 = ORIENTED_EDGE ( 'NONE', *, *, #8255, .T. ) ;
#11630 = FACE_OUTER_BOUND ( 'NONE', #8624, .T. ) ;
#11631 = CARTESIAN_POINT ( 'NONE',  ( 1.472469842513823179, 35.59226448433412315, -4.923371831947296329 ) ) ;
#11632 = CARTESIAN_POINT ( 'NONE',  ( 21.09922568453595559, 7.040301336597086568, -6.408140936763230044 ) ) ;
#11633 = CARTESIAN_POINT ( 'NONE',  ( -0.8801773607110991993, 62.85535201082150536, -2.915334737309923874 ) ) ;
#11634 = CARTESIAN_POINT ( 'NONE',  ( -10.58223187590993497, 14.76930270348881002, -10.54772123337545509 ) ) ;
#11635 = B_SPLINE_CURVE_WITH_KNOTS ( 'NONE', 3,
 ( #75432, #20967, #4977, #74938, #51452, #96480, #44436, #59929 ),
 .UNSPECIFIED., .F., .F.,
 ( 4, 2, 2, 4 ),
 ( 0.000000000000000000, 0.001329205578904317682, 0.002658411157808635364, 0.005316822315617270728 ),
 .UNSPECIFIED. ) ;
#11636 = CARTESIAN_POINT ( 'NONE',  ( 19.84674366389459266, 13.30059781766745353, 2.638427012816836559 ) ) ;
#11637 = CARTESIAN_POINT ( 'NONE',  ( 5.076628168052704559, 60.17559781766745175, -8.527530157486179263 ) ) ;
#11638 = CARTESIAN_POINT ( 'NONE',  ( 1.042145700049395884, 19.74216108172003104, -6.499999999999846345 ) ) ;
#11639 = AXIS2_PLACEMENT_3D ( 'NONE', #74193, #5726, #34720 ) ;
#11640 = ADVANCED_FACE ( 'NONE', ( #71993 ), #20956, .T. ) ;
#11641 = ORIENTED_EDGE ( 'NONE', *, *, #86749, .F. ) ;
#11642 = EDGE_CURVE ( 'NONE', #14221, #37192, #46274, .T. ) ;
#11643 = CARTESIAN_POINT ( 'NONE',  ( 15.44008868035555260, 4.730352010821505360, 9.422509992056143702 ) ) ;
#11644 = CARTESIAN_POINT ( 'NONE',  ( -2.266590686148945544, 7.220415501580634832, 7.082119434687048631 ) ) ;
#11645 = CARTESIAN_POINT ( 'NONE',  ( 5.076628168052704559, 15.17559781766745175, -8.527530157486179263 ) ) ;
#11646 = CARTESIAN_POINT ( 'NONE',  ( 0.5774900079438607392, 48.48035201082150536, 5.440088680355550821 ) ) ;
#11648 = CARTESIAN_POINT ( 'NONE',  ( 6.779815635997717749, 13.03986625811624833, -9.668860777447443766 ) ) ;
#11647 = CARTESIAN_POINT ( 'NONE',  ( 21.09922568453595559, 22.04030133659708923, -6.408140936763230044 ) ) ;
#11649 = CARTESIAN_POINT ( 'NONE',  ( 0.5774900079438590739, 7.647018677488171434, -5.440088680355550821 ) ) ;
#11650 = CARTESIAN_POINT ( 'NONE',  ( 64.56412365047461321, 44.99999999999998579, 7.000000000000000000 ) ) ;
#11651 = CARTESIAN_POINT ( 'NONE',  ( -13.86186289918447478, 15.00000000000000888, 4.667665767314873371 ) ) ;
#11652 = CARTESIAN_POINT ( 'NONE',  ( 7.361572987183169658, 54.96726448433413026, -9.846743663894592657 ) ) ;
#11653 = CARTESIAN_POINT ( 'NONE',  ( 0.1532563361054100626, 15.80059781766745353, -2.638427012816831230 ) ) ;
#11654 = CARTESIAN_POINT ( 'NONE',  ( -7.964842623401172439, -31.31131465584515539, 7.964842623401183097 ) ) ;
#11655 = CARTESIAN_POINT ( 'NONE',  ( 3.591859063236763294, 28.29030133659708568, -11.09922568453595026 ) ) ;
#11656 = DIRECTION ( 'NONE',  ( 0.000000000000000000, 0.000000000000000000, -1.000000000000000000 ) ) ;
#11657 = PRODUCT_RELATED_PRODUCT_CATEGORY ( 'part', '', ( #7560 ) ) ;
#11658 = CARTESIAN_POINT ( 'NONE',  ( 7.084665262690076126, 32.02201867748816966, -10.88017736071110164 ) ) ;
#11659 = DIRECTION ( 'NONE',  ( 0.000000000000000000, 0.000000000000000000, 1.000000000000000000 ) ) ;
#11660 = CARTESIAN_POINT ( 'NONE',  ( 10.00000000000000000, 55.55374883491396787, -14.16423886937410082 ) ) ;
#11661 = CARTESIAN_POINT ( 'NONE',  ( 13.79529636645031943, 30.34541550158063927, -14.16423886937409904 ) ) ;
#11662 = CIRCLE ( 'NONE', #59561, 0.5000000000000004441 ) ;
#11663 = CARTESIAN_POINT ( 'NONE',  ( 19.84674366389459621, 43.50893115100078745, 7.409399052514197653E-17 ) ) ;
#11664 = CARTESIAN_POINT ( 'NONE',  ( -2.816281873526473856, 39.33196800326374643, 3.434112377981055619 ) ) ;
#11665 = CARTESIAN_POINT ( 'NONE',  ( 2.035157376598824452, 23.68868534415484461, 7.964842623401179544 ) ) ;
#11666 = CARTESIAN_POINT ( 'NONE',  ( 19.84674366389459621, 53.50893115100078745, 7.409399052514197653E-17 ) ) ;
#11667 = CARTESIAN_POINT ( 'NONE',  ( 4.559911319644449179, 38.89701867748817676, 9.422509992056141925 ) ) ;
#11668 = CARTESIAN_POINT ( 'NONE',  ( 19.38216949554541202, 10.99863466993042138, 9.382169495545424454 ) ) ;
#11669 = CARTESIAN_POINT ( 'NONE',  ( 6.204703633549690345, 30.76208216824730357, -14.16423886937410259 ) ) ;
#11671 = CARTESIAN_POINT ( 'NONE',  ( 17.62281668512003208, 33.28593319516822646, 6.499999999999993783 ) ) ;
#11670 = B_SPLINE_CURVE_WITH_KNOTS ( 'NONE', 3,
 ( #25580, #32060, #56072, #9578, #62070, #10077 ),
 .UNSPECIFIED., .F., .F.,
 ( 4, 2, 4 ),
 ( 0.0002800098398849620428, 0.0006862151655504652656, 0.001092420491215968488 ),
 .UNSPECIFIED. ) ;
#11672 = AXIS2_PLACEMENT_3D ( 'NONE', #42613, #35600, #12600 ) ;
#11673 = AXIS2_PLACEMENT_3D ( 'NONE', #89364, #74344, #19878 ) ;
#11674 = CARTESIAN_POINT ( 'NONE',  ( 0.1532563361054082862, 31.21726448433412315, 2.638427012816831674 ) ) ;
#11675 = CARTESIAN_POINT ( 'NONE',  ( 21.09922568453595559, 62.04030133659709634, -6.408140936763230044 ) ) ;
#11676 = CARTESIAN_POINT ( 'NONE',  ( 2.791683348922240793, 66.63393115100079456, 7.208316651077764092 ) ) ;
#11677 = ORIENTED_EDGE ( 'NONE', *, *, #51375, .T. ) ;
#11678 = AXIS2_PLACEMENT_3D ( 'NONE', #65133, #27138, #88137 ) ;
#11679 = DIRECTION ( 'NONE',  ( 0.000000000000000000, 0.000000000000000000, -1.000000000000000000 ) ) ;
#11680 = CARTESIAN_POINT ( 'NONE',  ( 6.878063601867475008, -66.29791949882819324, 3.750000000000001776 ) ) ;
#11681 = CARTESIAN_POINT ( 'NONE',  ( 2.035157376598822676, 17.43868534415483751, -7.964842623401177768 ) ) ;
#11682 = CARTESIAN_POINT ( 'NONE',  ( 6.204703633549690345, 27.84541550158063217, 14.16423886937410082 ) ) ;
#11683 = CARTESIAN_POINT ( 'NONE',  ( 10.00000000000000178, 7.258931151000785675, 9.846743663894594434 ) ) ;
#11684 = CARTESIAN_POINT ( 'NONE',  ( 14.92337183194729633, 52.67559781766745175, 8.527530157486181039 ) ) ;
#11685 = CARTESIAN_POINT ( 'NONE',  ( 20.88017736071110164, 35.35535201082150536, 2.915334737309930979 ) ) ;
#11686 = AXIS2_PLACEMENT_3D ( 'NONE', #62277, #32271, #40288 ) ;
#11687 = DIRECTION ( 'NONE',  ( -3.375077994860475883E-14, 0.000000000000000000, 1.000000000000000000 ) ) ;
#11688 = CARTESIAN_POINT ( 'NONE',  ( 3.469446951953614189E-15, 10.93830936912750573, 11.92686044187656513 ) ) ;
#11689 = ORIENTED_EDGE ( 'NONE', *, *, #23751, .T. ) ;
#11690 = CARTESIAN_POINT ( 'NONE',  ( 20.15039907845753575, 65.60158574516643171, -6.262539305110073506 ) ) ;
#11691 = ORIENTED_EDGE ( 'NONE', *, *, #45037, .T. ) ;
#11692 = EDGE_LOOP ( 'NONE', ( #12195, #84969, #93478, #57693, #53918, #14624 ) ) ;
#11693 = CARTESIAN_POINT ( 'NONE',  ( -41.70923076923077844, 106.3461538461538396, -9.500000000000000000 ) ) ;
#11694 = CARTESIAN_POINT ( 'NONE',  ( 10.00000000000000178, 13.05374883491396787, 14.16423886937410082 ) ) ;
#11695 = CARTESIAN_POINT ( 'NONE',  ( 22.26659068614895176, 9.720415501580633943, -7.082119434687042414 ) ) ;
#11696 = CARTESIAN_POINT ( 'NONE',  ( 20.36894250292379738, 59.92874883491397497, -10.36894250292379027 ) ) ;
#11697 = CARTESIAN_POINT ( 'NONE',  ( 12.63842701281683034, 52.46726448433413026, 9.846743663894596210 ) ) ;
#11698 = CARTESIAN_POINT ( 'NONE',  ( 5.076628168052703671, 41.84226448433411605, 8.527530157486179263 ) ) ;
#11699 = CARTESIAN_POINT ( 'NONE',  ( 19.72487221294570858, 51.86607318730076344, 6.500000000000000888 ) ) ;
#11701 = CARTESIAN_POINT ( 'NONE',  ( 12.63842701281683034, 62.46726448433410894, 9.846743663894596210 ) ) ;
#11700 = CARTESIAN_POINT ( 'NONE',  ( 20.88017736071110875, 30.77201867748816966, -2.915334737309920765 ) ) ;
#11702 = CARTESIAN_POINT ( 'NONE',  ( -4.164238869374098151, 1.595415501580634388, -3.795296366450310543 ) ) ;
#11703 = CARTESIAN_POINT ( 'NONE',  ( 10.00000000000000178, 9.313685344154839285, 10.88017736071110342 ) ) ;
#11704 = CARTESIAN_POINT ( 'NONE',  ( -0.2418659066527706625, 67.23410085661205926, -6.114288769123047196 ) ) ;
#11705 = CARTESIAN_POINT ( 'NONE',  ( 0.000000000000000000, 14.49999999999999822, 0.000000000000000000 ) ) ;
#11706 = CARTESIAN_POINT ( 'NONE',  ( 7.208316651077764980, -32.11606884899921255, 7.208316651077762316 ) ) ;
#11707 = ORIENTED_EDGE ( 'NONE', *, *, #53507, .T. ) ;
#11708 = ORIENTED_EDGE ( 'NONE', *, *, #78248, .T. ) ;
#11709 = CARTESIAN_POINT ( 'NONE',  ( 14.92337183194729633, 27.67559781766745530, 8.527530157486181039 ) ) ;
#11710 = ORIENTED_EDGE ( 'NONE', *, *, #77235, .T. ) ;
#11711 = CARTESIAN_POINT ( 'NONE',  ( 10.00000000000000178, 38.05374883491396787, 14.16423886937410082 ) ) ;
#11712 = CARTESIAN_POINT ( 'NONE',  ( 14.92337183194729988, 39.34226448433412315, -8.527530157486177487 ) ) ;
#11713 = CARTESIAN_POINT ( 'NONE',  ( 19.42250999205614548, 55.98035201082150536, -5.440088680355545492 ) ) ;
#11714 = AXIS2_PLACEMENT_3D ( 'NONE', #98525, #50144, #22506 ) ;
#11715 = LINE ( 'NONE', #43192, #1723 ) ;
#11716 = CARTESIAN_POINT ( 'NONE',  ( 20.88017736071110875, 50.77201867748817676, -2.915334737309920765 ) ) ;
#11717 = CARTESIAN_POINT ( 'NONE',  ( 16.40814093676324603, 62.45696800326376064, -11.09922568453594671 ) ) ;
#11718 = CARTESIAN_POINT ( 'NONE',  ( -5.204170427930421283E-15, 2.873634669930423602, -12.81628187352647608 ) ) ;
#11719 = EDGE_LOOP ( 'NONE', ( #32422, #4105, #20334, #75297 ) ) ;
#11720 = CARTESIAN_POINT ( 'NONE',  ( -0.8801773607110991993, 47.85535201082150536, -2.915334737309923874 ) ) ;
#11721 = CARTESIAN_POINT ( 'NONE',  ( -4.164238869374099039, 21.80374883491396787, 8.674139862899312516E-16 ) ) ;
#11722 = ORIENTED_EDGE ( 'NONE', *, *, #83097, .T. ) ;
#11723 = CARTESIAN_POINT ( 'NONE',  ( 22.81628187352647785, 46.62363466993041783, 6.195893100308588602E-16 ) ) ;
#11724 = CARTESIAN_POINT ( 'NONE',  ( 17.96484262340118221, 19.93868534415484106, 7.964842623401181321 ) ) ;
#11725 = CARTESIAN_POINT ( 'NONE',  ( 18.52753015748617571, 28.09226448433411960, 4.923371831947298993 ) ) ;
#11726 = CARTESIAN_POINT ( 'NONE',  ( 19.42250999205614548, 15.98035201082150714, -5.440088680355545492 ) ) ;
#11727 = CARTESIAN_POINT ( 'NONE',  ( 21.09922568453595559, 52.04030133659708923, -6.408140936763230044 ) ) ;
#11728 = FACE_OUTER_BOUND ( 'NONE', #76292, .T. ) ;
#11729 = CARTESIAN_POINT ( 'NONE',  ( 5.076628168052704559, 35.17559781766745175, -8.527530157486179263 ) ) ;
#11730 = B_SPLINE_CURVE_WITH_KNOTS ( 'NONE', 3,
 ( #93023, #1566, #70536, #24058, #8557, #40533 ),
 .UNSPECIFIED., .F., .F.,
 ( 4, 2, 4 ),
 ( 3.409110551496096132E-05, 0.0004400426677367851079, 0.0008459942299586093156 ),
 .UNSPECIFIED. ) ;
#11731 = EDGE_CURVE ( 'NONE', #14724, #39677, #80974, .T. ) ;
#11733 = EDGE_LOOP ( 'NONE', ( #92608, #17537, #45978, #27383 ) ) ;
#11732 = CARTESIAN_POINT ( 'NONE',  ( 10.19513985507825993, 0.3640475087720984049, 11.00268709613225049 ) ) ;
#11734 = VECTOR ( 'NONE', #62323, 1000.000000000000000 ) ;
#11735 = CARTESIAN_POINT ( 'NONE',  ( 20.88017736071110875, 65.77201867748817676, -2.915334737309920765 ) ) ;
#11736 = CARTESIAN_POINT ( 'NONE',  ( 0.6076426042653181314, 27.37576471608601025, -6.500000000000012434 ) ) ;
#11737 = CARTESIAN_POINT ( 'NONE',  ( 0.000000000000000000, 0.000000000000000000, 0.000000000000000000 ) ) ;
#11738 = CARTESIAN_POINT ( 'NONE',  ( 7.361572987183170547, 2.050597817667451750, 9.846743663894590881 ) ) ;
#11739 = AXIS2_PLACEMENT_3D ( 'NONE', #28094, #82583, #34599 ) ;
#11740 = CARTESIAN_POINT ( 'NONE',  ( -1.099225684535947600, 28.70696800326375353, -6.408140936763238038 ) ) ;
#11742 = CARTESIAN_POINT ( 'NONE',  ( 3.969999999999999751, 37.00000000000000000, -3.750000000000000000 ) ) ;
#11741 = CIRCLE ( 'NONE', #19733, 15.00000000000000000 ) ;
#11743 = CARTESIAN_POINT ( 'NONE',  ( 0.1532563361054083140, 41.00893115100078745, 1.131784320476157264E-15 ) ) ;
#11744 = CARTESIAN_POINT ( 'NONE',  ( 20.15039907845754286, 14.72266099184918531, 6.262539305110064625 ) ) ;
#11745 = CARTESIAN_POINT ( 'NONE',  ( -2.266590686148945544, 22.22041550158063572, 7.082119434687048631 ) ) ;
#11746 = CARTESIAN_POINT ( 'NONE',  ( 7.361572987183169658, 29.96726448433411960, -9.846743663894592657 ) ) ;
#11747 = CARTESIAN_POINT ( 'NONE',  ( 13.43411237798105340, 30.58196800326374998, 12.81628187352647963 ) ) ;
#11749 = CARTESIAN_POINT ( 'NONE',  ( 0.000000000000000000, 15.00000000000000000, 0.000000000000000000 ) ) ;
#11748 = DIRECTION ( 'NONE',  ( -1.000000000000000000, 0.000000000000000000, -0.000000000000000000 ) ) ;
#11750 = CARTESIAN_POINT ( 'NONE',  ( 2.035157376598824452, 68.68868534415484817, 7.964842623401179544 ) ) ;
#11751 = CARTESIAN_POINT ( 'NONE',  ( 16.40814093676323893, 10.79030133659708923, 11.09922568453595026 ) ) ;
#11752 = CARTESIAN_POINT ( 'NONE',  ( -26.69000000000001194, 92.00000000000000000, -10.09898361729590199 ) ) ;
#11753 = CARTESIAN_POINT ( 'NONE',  ( 12.63842701281683922, 39.55059781766744464, -9.846743663894590881 ) ) ;
#11754 = CARTESIAN_POINT ( 'NONE',  ( 19.42250999205614193, 25.14701867748817321, 5.440088680355555262 ) ) ;
#11755 = CARTESIAN_POINT ( 'NONE',  ( 16.40814093676324603, 27.45696800326375708, -11.09922568453594671 ) ) ;
#11756 = APPLICATION_PROTOCOL_DEFINITION ( 'draft international standard', 'automotive_design', 1998, #83209 ) ;
#11757 = CARTESIAN_POINT ( 'NONE',  ( -13.14228782657349370, 14.63606917158947418, 7.230509711182151023 ) ) ;
#11758 = EDGE_CURVE ( 'NONE', #8161, #43087, #57064, .T. ) ;
#11759 = CARTESIAN_POINT ( 'NONE',  ( 12.91533473730993009, 26.60535201082150536, -10.88017736071109987 ) ) ;
#11760 = VERTEX_POINT ( 'NONE', #24759 ) ;
#11761 = DIRECTION ( 'NONE',  ( 0.000000000000000000, -1.000000000000000000, 0.000000000000000000 ) ) ;
#11762 = CARTESIAN_POINT ( 'NONE',  ( 6.934003561272409577, -73.15726776819576571, 2.750000000000000888 ) ) ;
#11764 = CARTESIAN_POINT ( 'NONE',  ( 20.88017736071110519, 30.56368534415484106, 2.639326808657452039E-16 ) ) ;
#11763 = CARTESIAN_POINT ( 'NONE',  ( 12.63842701281683922, 54.55059781766745175, -9.846743663894590881 ) ) ;
#11765 = DIRECTION ( 'NONE',  ( 1.000000000000000000, 0.000000000000000000, 6.938893903907221278E-15 ) ) ;
#11766 = CARTESIAN_POINT ( 'NONE',  ( 19.42250999205614548, 50.98035201082151247, -5.440088680355545492 ) ) ;
#11767 = CARTESIAN_POINT ( 'NONE',  ( 15.44008868035555793, 26.39701867748817321, -9.422509992056140149 ) ) ;
#11768 = DIRECTION ( 'NONE',  ( 0.6755902076156591329, 0.000000000000000000, -0.7372773368101250835 ) ) ;
#11769 = DIRECTION ( 'NONE',  ( -0.000000000000000000, 1.000000000000000000, -0.000000000000000000 ) ) ;
#11770 = CARTESIAN_POINT ( 'NONE',  ( 7.361572987183170547, 52.05059781766745175, 9.846743663894590881 ) ) ;
#11772 =( NAMED_UNIT ( * ) PLANE_ANGLE_UNIT ( ) SI_UNIT ( $, .RADIAN. ) );
#11771 = CARTESIAN_POINT ( 'NONE',  ( -4.164238869374099927, 47.01208216824729647, 3.795296366450308767 ) ) ;
#11773 = CARTESIAN_POINT ( 'NONE',  ( -29.94000000000001549, 92.00000000000000000, -9.500000000000000000 ) ) ;
#11774 = CARTESIAN_POINT ( 'NONE',  ( -2.266590686148945544, 6.387082168247300906, -7.082119434687050408 ) ) ;
#11775 = CARTESIAN_POINT ( 'NONE',  ( 24.16423886937410614, 39.51208216824731068, -3.795296366450302550 ) ) ;
#11776 = CARTESIAN_POINT ( 'NONE',  ( 3.591859063236761518, 9.956968003263753531, 11.09922568453594849 ) ) ;
#11777 = DIRECTION ( 'NONE',  ( 0.6246950475544237324, 0.7808688094430306093, 0.000000000000000000 ) ) ;
#11778 = VERTEX_POINT ( 'NONE', #39761 ) ;
#11779 = B_SPLINE_CURVE_WITH_KNOTS ( 'NONE', 3,
 ( #19551, #79063, #10577, #80549 ),
 .UNSPECIFIED., .F., .F.,
 ( 4, 4 ),
 ( 0.000000000000000000, 0.002562518741975561461 ),
 .UNSPECIFIED. ) ;
#11780 = CARTESIAN_POINT ( 'NONE',  ( 2.035157376598822676, 2.438685344154838397, -7.964842623401177768 ) ) ;
#11781 = CARTESIAN_POINT ( 'NONE',  ( 18.52753015748617571, 33.09226448433411605, 4.923371831947298993 ) ) ;
#11782 = CARTESIAN_POINT ( 'NONE',  ( 2.035157376598824452, 58.68868534415482685, 7.964842623401179544 ) ) ;
#11783 = CARTESIAN_POINT ( 'NONE',  ( 0.2751277870542967463, 70.00000000000000000, -6.500000000000000888 ) ) ;
#11784 = CARTESIAN_POINT ( 'NONE',  ( -0.8801773607111009756, 28.06368534415484106, 1.068504757029289695E-15 ) ) ;
#11785 = CARTESIAN_POINT ( 'NONE',  ( 6.565887622018943937, 58.08196800326376064, -12.81628187352647608 ) ) ;
#11786 = CARTESIAN_POINT ( 'NONE',  ( 19.38216949554541202, 25.99863466993042138, 9.382169495545424454 ) ) ;
#11787 = CARTESIAN_POINT ( 'NONE',  ( 12.63842701281683034, 22.46726448433411605, 9.846743663894596210 ) ) ;
#11788 = ORIENTED_EDGE ( 'NONE', *, *, #70147, .F. ) ;
#11789 = CARTESIAN_POINT ( 'NONE',  ( -12.50534872682722565, 4.101355178835516792E-16, -7.339363270777700343 ) ) ;
#11790 = CARTESIAN_POINT ( 'NONE',  ( 2.035157376598824452, 3.688685344154837953, 7.964842623401179544 ) ) ;
#11791 = CARTESIAN_POINT ( 'NONE',  ( -4.164238869374098151, 46.59541550158063927, -3.795296366450310543 ) ) ;
#11792 = CARTESIAN_POINT ( 'NONE',  ( -0.8801773607111008646, 33.27201867748817676, 2.915334737309923430 ) ) ;
#11793 = CARTESIAN_POINT ( 'NONE',  ( 7.084665262690076126, 52.02201867748816255, -10.88017736071110164 ) ) ;
#11794 = LINE ( 'NONE', #98661, #71855 ) ;
#11795 = ADVANCED_FACE ( 'NONE', ( #55748 ), #5968, .T. ) ;
#11796 = CARTESIAN_POINT ( 'NONE',  ( 9.479665769771463246, -19.63627307881997908, -4.000000000000000000 ) ) ;
#11797 = CARTESIAN_POINT ( 'NONE',  ( 7.361572987183170547, 7.050597817667451750, 9.846743663894590881 ) ) ;
#11798 = FACE_OUTER_BOUND ( 'NONE', #90761, .T. ) ;
#11799 =( LENGTH_UNIT ( ) NAMED_UNIT ( * ) SI_UNIT ( .MILLI., .METRE. ) );
#11800 = CARTESIAN_POINT ( 'NONE',  ( 12.63842701281683034, 27.46726448433411250, 9.846743663894596210 ) ) ;
#11801 = CARTESIAN_POINT ( 'NONE',  ( 2.791683348922237240, 50.38393115100078035, -7.208316651077763204 ) ) ;
#11802 = EDGE_CURVE ( 'NONE', #51757, #39764, #48228, .T. ) ;
#11803 = ORIENTED_EDGE ( 'NONE', *, *, #40200, .F. ) ;
#11804 = CARTESIAN_POINT ( 'NONE',  ( 22.81628187352647785, 51.41530133659708923, 3.434112377981063169 ) ) ;
#11805 =( NAMED_UNIT ( * ) SI_UNIT ( $, .STERADIAN. ) SOLID_ANGLE_UNIT ( ) );
#11806 = AXIS2_PLACEMENT_3D ( 'NONE', #17734, #61729, #54236 ) ;
#11807 = CARTESIAN_POINT ( 'NONE',  ( 7.084665262690076126, 67.02201867748817676, -10.88017736071110164 ) ) ;
#11808 = CARTESIAN_POINT ( 'NONE',  ( 5.076628168052704559, 35.17559781766745175, -8.527530157486179263 ) ) ;
#11810 = CARTESIAN_POINT ( 'NONE',  ( 12.63842701281683034, 22.46726448433411605, 9.846743663894596210 ) ) ;
#11809 = CARTESIAN_POINT ( 'NONE',  ( -2.266590686148945544, 62.22041550158063927, 7.082119434687048631 ) ) ;
#11811 = CARTESIAN_POINT ( 'NONE',  ( 0.000000000000000000, 0.5000000000000004441, 0.000000000000000000 ) ) ;
#11812 = CARTESIAN_POINT ( 'NONE',  ( 19.84674366389459266, 63.30059781766745886, 2.638427012816836559 ) ) ;
#11813 = CARTESIAN_POINT ( 'NONE',  ( 13.79529636645030344, 18.26208216824730002, 14.16423886937410614 ) ) ;
#11814 = CARTESIAN_POINT ( 'NONE',  ( 6.204703633549690345, 37.84541550158063927, 14.16423886937410082 ) ) ;
#11815 = CARTESIAN_POINT ( 'NONE',  ( 5.076628168052704559, 40.17559781766745175, -8.527530157486179263 ) ) ;
#11816 = LINE ( 'NONE', #73301, #36311 ) ;
#11817 = CARTESIAN_POINT ( 'NONE',  ( 17.96484262340118221, 31.18868534415483751, -7.964842623401177768 ) ) ;
#11818 = COLOUR_RGB ( '', 0.08235294, 0.09019608, 0.10196078) ;
#11819 = CARTESIAN_POINT ( 'NONE',  ( 10.00000000000000178, 64.31368534415483396, 10.88017736071110342 ) ) ;
#11820 = CARTESIAN_POINT ( 'NONE',  ( -0.1310148450194394409, 0.09385736792626404867, 6.293957503965299516 ) ) ;
#11821 = ORIENTED_EDGE ( 'NONE', *, *, #94239, .T. ) ;
#11822 = CARTESIAN_POINT ( 'NONE',  ( 21.09922568453594849, 51.20696800326375353, 6.408140936763242479 ) ) ;
#11823 = CARTESIAN_POINT ( 'NONE',  ( 10.00000000000000000, 51.81368534415484106, -10.88017736071110342 ) ) ;
#11824 = ORIENTED_EDGE ( 'NONE', *, *, #33966, .F. ) ;
#11825 = CARTESIAN_POINT ( 'NONE',  ( 2.618367889266248100E-15, 44.99999999999999289, 7.000000000000000000 ) ) ;
#11826 = FACE_OUTER_BOUND ( 'NONE', #97583, .T. ) ;
#11827 = CARTESIAN_POINT ( 'NONE',  ( 4.559911319644449179, 58.89701867748817676, 9.422509992056141925 ) ) ;
#11828 = ORIENTED_EDGE ( 'NONE', *, *, #97691, .T. ) ;
#11829 = CARTESIAN_POINT ( 'NONE',  ( 0.5774900079438590739, 67.64701867748817676, -5.440088680355550821 ) ) ;
#11830 = CARTESIAN_POINT ( 'NONE',  ( -0.8801773607111008646, 18.27201867748817321, 2.915334737309923430 ) ) ;
#11831 = DIRECTION ( 'NONE',  ( -0.000000000000000000, -1.000000000000000000, -0.000000000000000000 ) ) ;
#11832 = CARTESIAN_POINT ( 'NONE',  ( 20.30776406404399026, 0.000000000000000000, 6.000000000000280664 ) ) ;
#11833 = CARTESIAN_POINT ( 'NONE',  ( 4.559911319644449179, 3.897018677488171434, 9.422509992056141925 ) ) ;
#11834 = CARTESIAN_POINT ( 'NONE',  ( 18.52753015748617571, 13.09226448433411960, 4.923371831947298993 ) ) ;
#11835 = CARTESIAN_POINT ( 'NONE',  ( 24.16423886937410614, 19.30374883491397142, 8.672049930838204340E-16 ) ) ;
#11836 = B_SPLINE_CURVE_WITH_KNOTS ( 'NONE', 3,
 ( #54482, #39507, #30008, #69505 ),
 .UNSPECIFIED., .F., .F.,
 ( 4, 4 ),
 ( 0.000000000000000000, 0.001036303429213355533 ),
 .UNSPECIFIED. ) ;
#11837 = CARTESIAN_POINT ( 'NONE',  ( 17.96484262340118221, 26.18868534415483396, -7.964842623401177768 ) ) ;
#11838 = CARTESIAN_POINT ( 'NONE',  ( 18.52753015748618282, 53.92559781766745175, -4.923371831947291888 ) ) ;
#11839 = ORIENTED_EDGE ( 'NONE', *, *, #89519, .F. ) ;
#11840 = CARTESIAN_POINT ( 'NONE',  ( 1.472469842513823179, 55.59226448433412315, -4.923371831947296329 ) ) ;
#11841 = ORIENTED_EDGE ( 'NONE', *, *, #31140, .F. ) ;
#11842 = CARTESIAN_POINT ( 'NONE',  ( -10.39692778084925173, 0.04962893796709067634, -10.46714871971213334 ) ) ;
#11843 = CARTESIAN_POINT ( 'NONE',  ( 19.42250999205614548, 55.98035201082150536, -5.440088680355545492 ) ) ;
#11844 = CARTESIAN_POINT ( 'NONE',  ( 5.076628168052704559, 45.17559781766745175, -8.527530157486179263 ) ) ;
#11845 = CARTESIAN_POINT ( 'NONE',  ( 21.09922568453595559, 42.04030133659708213, -6.408140936763230044 ) ) ;
#11847 = FACE_OUTER_BOUND ( 'NONE', #45035, .T. ) ;
#11846 = CARTESIAN_POINT ( 'NONE',  ( 15.44008868035555260, 9.730352010821505360, 9.422509992056143702 ) ) ;
#11848 = CARTESIAN_POINT ( 'NONE',  ( 20.88017736071110519, 65.56368534415483396, 2.639326808657452039E-16 ) ) ;
#11849 = CARTESIAN_POINT ( 'NONE',  ( 0.5774900079438607392, 8.480352010821505360, 5.440088680355550821 ) ) ;
#11850 = EDGE_CURVE ( 'NONE', #12076, #31523, #46754, .T. ) ;
#11851 = CARTESIAN_POINT ( 'NONE',  ( 19.38216949554541557, 42.24863466993041783, -9.382169495545420901 ) ) ;
#11852 = CARTESIAN_POINT ( 'NONE',  ( 15.44008868035555793, 26.39701867748817321, -9.422509992056140149 ) ) ;
#11853 = CARTESIAN_POINT ( 'NONE',  ( 19.67388390623025529, 90.60261632297043377, 5.439653449514034733 ) ) ;
#11854 = ADVANCED_FACE ( 'NONE', ( #63715 ), #2766, .T. ) ;
#11855 = VERTEX_POINT ( 'NONE', #62734 ) ;
#11856 = B_SPLINE_CURVE_WITH_KNOTS ( 'NONE', 3,
 ( #34888, #80405, #88889, #19893 ),
 .UNSPECIFIED., .F., .F.,
 ( 4, 4 ),
 ( 0.000000000000000000, 0.001036303429213364423 ),
 .UNSPECIFIED. ) ;
#11857 = CARTESIAN_POINT ( 'NONE',  ( 0.6178305044545818747, 43.49863466993042493, -9.382169495545419124 ) ) ;
#11858 = CARTESIAN_POINT ( 'NONE',  ( 20.88017736071110875, 40.77201867748818387, -2.915334737309920765 ) ) ;
#11859 = CARTESIAN_POINT ( 'NONE',  ( 17.20831665107776587, 62.88393115100078745, 7.208316651077764980 ) ) ;
#11860 = ORIENTED_EDGE ( 'NONE', *, *, #9608, .F. ) ;
#11861 = B_SPLINE_CURVE_WITH_KNOTS ( 'NONE', 3,
 ( #33852, #31206, #267, #75237, #23743, #8235 ),
 .UNSPECIFIED., .F., .F.,
 ( 4, 2, 4 ),
 ( 0.000000000000000000, 0.0002701661927229507859, 0.0005403323854459015719 ),
 .UNSPECIFIED. ) ;
#11862 = CARTESIAN_POINT ( 'NONE',  ( 0.1532563361054082862, 56.21726448433411605, 2.638427012816831674 ) ) ;
#11863 = EDGE_CURVE ( 'NONE', #16892, #82266, #12964, .T. ) ;
#11865 = CARTESIAN_POINT ( 'NONE',  ( 10.00000000000000000, 54.75893115100078745, -9.846743663894594434 ) ) ;
#11864 = CARTESIAN_POINT ( 'NONE',  ( 11.81378540890930751, -0.03417435944610275333, 7.968498874458199488 ) ) ;
#11866 = CARTESIAN_POINT ( 'NONE',  ( 7.084665262690076126, 27.02201867748817676, -10.88017736071110164 ) ) ;
#11867 =( LENGTH_UNIT ( ) NAMED_UNIT ( * ) SI_UNIT ( .MILLI., .METRE. ) );
#11868 = CARTESIAN_POINT ( 'NONE',  ( 5.076628168052704559, 35.17559781766745175, -8.527530157486179263 ) ) ;
#11869 = CARTESIAN_POINT ( 'NONE',  ( -1.180296924652950663, 0.000000000000000000, 5.323975374878045841 ) ) ;
#11870 = DIRECTION ( 'NONE',  ( -1.000000000000000000, 0.000000000000000000, 0.000000000000000000 ) ) ;
#11872 = CARTESIAN_POINT ( 'NONE',  ( 18.52753015748618282, 8.925597817667451750, -4.923371831947291888 ) ) ;
#11871 = CARTESIAN_POINT ( 'NONE',  ( 10.00000000000000178, 37.25893115100078745, 9.846743663894594434 ) ) ;
#11873 = PRESENTATION_STYLE_ASSIGNMENT (( #73352 ) ) ;
#11875 = ORIENTED_EDGE ( 'NONE', *, *, #9604, .T. ) ;
#11874 = CARTESIAN_POINT ( 'NONE',  ( 7.361572987183169658, 64.96726448433412315, -9.846743663894592657 ) ) ;
#11876 = CARTESIAN_POINT ( 'NONE',  ( 0.6178305044545838731, 64.74863466993043914, 9.382169495545420901 ) ) ;
#11877 = CARTESIAN_POINT ( 'NONE',  ( 16.40814093676324603, 32.45696800326375353, -11.09922568453594671 ) ) ;
#11878 = EDGE_CURVE ( 'NONE', #49769, #48349, #96893, .T. ) ;
#11879 = CARTESIAN_POINT ( 'NONE',  ( 18.52753015748618282, 38.92559781766745175, -4.923371831947291888 ) ) ;
#11880 = AXIS2_PLACEMENT_3D ( 'NONE', #25054, #94019, #25542 ) ;
#11881 =( LENGTH_UNIT ( ) NAMED_UNIT ( * ) SI_UNIT ( .MILLI., .METRE. ) );
#11882 = CARTESIAN_POINT ( 'NONE',  ( 20.36894250292379382, 53.67874883491397497, 10.36894250292379205 ) ) ;
#11883 = CARTESIAN_POINT ( 'NONE',  ( 14.92337183194729633, 37.67559781766745175, 8.527530157486181039 ) ) ;
#11884 = EDGE_CURVE ( 'NONE', #64703, #70287, #92748, .T. ) ;
#11885 = DIRECTION ( 'NONE',  ( -0.000000000000000000, 1.000000000000000000, -0.000000000000000000 ) ) ;
#11886 = ADVANCED_FACE ( 'NONE', ( #25748 ), #56241, .F. ) ;
#11887 = VECTOR ( 'NONE', #40073, 1000.000000000000000 ) ;
#11888 = CARTESIAN_POINT ( 'NONE',  ( 17.08211943468705130, 58.47041550158063927, 12.26659068614894998 ) ) ;
#11889 = CARTESIAN_POINT ( 'NONE',  ( 7.640985187756247576, 0.04962896822202483849, -12.62032702733652734 ) ) ;
#11890 = CARTESIAN_POINT ( 'NONE',  ( 4.559911319644449179, 7.230352010821505360, -9.422509992056141925 ) ) ;
#11891 = CARTESIAN_POINT ( 'NONE',  ( 24.16423886937409904, 34.09541550158064638, 3.795296366450317205 ) ) ;
#11893 = CARTESIAN_POINT ( 'NONE',  ( 1.274849032794116210, 8.572280503510292249, 6.499999999999738876 ) ) ;
#11892 = CARTESIAN_POINT ( 'NONE',  ( -0.3689425029237898834, 46.17874883491397497, -10.36894250292378850 ) ) ;
#11894 = CARTESIAN_POINT ( 'NONE',  ( 18.72515096720569971, 5.055090184799359676, 6.500000000000000000 ) ) ;
#11895 = CARTESIAN_POINT ( 'NONE',  ( 18.52753015748617571, 18.09226448433411960, 4.923371831947298993 ) ) ;
#11897 = CARTESIAN_POINT ( 'NONE',  ( 3.591859063236763294, 3.290301336597087012, -11.09922568453595026 ) ) ;
#11896 = CARTESIAN_POINT ( 'NONE',  ( -7.881609424765860794, -3.319945636763228996E-15, -12.32025747423903894 ) ) ;
#11898 = CARTESIAN_POINT ( 'NONE',  ( -0.8801773607111009756, 53.06368534415484106, 1.068504757029289695E-15 ) ) ;
#11899 = FILL_AREA_STYLE ('',( #49885 ) ) ;
#11900 = CARTESIAN_POINT ( 'NONE',  ( 14.92337183194729633, 52.67559781766745175, 8.527530157486181039 ) ) ;
#11901 = PLANE ( 'NONE',  #41104 ) ;
#11902 =( BOUNDED_CURVE ( )  B_SPLINE_CURVE ( 2, ( #1712, #85685, #31682, #77679, #23727, #25685, #24697, #78677, #17205 ),
 .UNSPECIFIED., .F., .T. ) 
 B_SPLINE_CURVE_WITH_KNOTS ( ( 3, 2, 2, 2, 3 ),
 ( 0.9034289457926085731, 0.9047619047619047672, 0.9107142857142856984, 0.9166666666666666297, 0.9179996256359628237 ),
 .UNSPECIFIED. ) 
 CURVE ( )  GEOMETRIC_REPRESENTATION_ITEM ( )  RATIONAL_B_SPLINE_CURVE ( ( 0.9881565478350746723, 0.9923695281211503127, 1.000000000000000000, 0.9659258262890683122, 1.000000000000000000, 0.9659258262890683122, 1.000000000000000000, 0.9923695281211504238, 0.9881565478350746723 ) ) 
 REPRESENTATION_ITEM ( '' )  );
#11903 = CARTESIAN_POINT ( 'NONE',  ( 17.20831665107776587, 54.13393115100079456, -7.208316651077762316 ) ) ;
#11904 = CARTESIAN_POINT ( 'NONE',  ( -0.2851577207221824284, 0.2306972965111893648, 14.93843163678290153 ) ) ;
#11905 = ORIENTED_EDGE ( 'NONE', *, *, #29234, .T. ) ;
#11906 = CARTESIAN_POINT ( 'NONE',  ( 17.08211943468705130, 28.47041550158063572, 12.26659068614894998 ) ) ;
#11907 = CARTESIAN_POINT ( 'NONE',  ( -0.1503990784575280903, 38.10158574516643171, 6.262539305110076171 ) ) ;
#11908 = CARTESIAN_POINT ( 'NONE',  ( 0.000000000000000000, 15.00000000000000000, 0.000000000000000000 ) ) ;
#11909 = CARTESIAN_POINT ( 'NONE',  ( 19.42250999205614193, 25.14701867748817321, 5.440088680355555262 ) ) ;
#11910 = CARTESIAN_POINT ( 'NONE',  ( 6.565887622018943937, 20.16530133659708213, 12.81628187352647430 ) ) ;
#11911 = CARTESIAN_POINT ( 'NONE',  ( -14.29541133317239243, 14.76930270348881002, -4.345028136609722758 ) ) ;
#11912 = CARTESIAN_POINT ( 'NONE',  ( 0.1532563361054083140, 16.00893115100078390, 1.131784320476157264E-15 ) ) ;
#11913 = CARTESIAN_POINT ( 'NONE',  ( 22.81628187352647785, 61.41530133659709634, 3.434112377981063169 ) ) ;
#11914 = VERTEX_POINT ( 'NONE', #69276 ) ;
#11915 = CARTESIAN_POINT ( 'NONE',  ( 6.905642986249669768, -69.45547628558871622, -3.999999999999999556 ) ) ;
#11916 = CARTESIAN_POINT ( 'NONE',  ( 2.917880565312948704, 32.63708216824730357, 12.26659068614894643 ) ) ;
#11917 = CARTESIAN_POINT ( 'NONE',  ( 15.44008868035555793, 11.39701867748817143, -9.422509992056140149 ) ) ;
#11918 = DIRECTION ( 'NONE',  ( -0.000000000000000000, -1.000000000000000000, -0.000000000000000000 ) ) ;
#11919 = DIRECTION ( 'NONE',  ( 0.000000000000000000, 0.000000000000000000, 1.000000000000000000 ) ) ;
#11920 = CARTESIAN_POINT ( 'NONE',  ( 0.5774900079438590739, 37.64701867748817676, -5.440088680355550821 ) ) ;
#11921 = CARTESIAN_POINT ( 'NONE',  ( 2.035157376598822676, 52.43868534415483396, -7.964842623401177768 ) ) ;
#11922 = CARTESIAN_POINT ( 'NONE',  ( 0.6178305044545818747, 13.49863466993041783, -9.382169495545419124 ) ) ;
#11923 = CARTESIAN_POINT ( 'NONE',  ( 19.84674366389459266, 63.71726448433412315, -2.638427012816827677 ) ) ;
#11924 = DIRECTION ( 'NONE',  ( 0.000000000000000000, 0.000000000000000000, -1.000000000000000000 ) ) ;
#11925 = CARTESIAN_POINT ( 'NONE',  ( 10.00000000000000178, 7.258931151000785675, 9.846743663894594434 ) ) ;
#11926 = CARTESIAN_POINT ( 'NONE',  ( 13.14228782657334804, 0.5000000000000004441, 7.230509711182329546 ) ) ;
#11927 = CIRCLE ( 'NONE', #63019, 2.899999999999999911 ) ;
#11928 = CARTESIAN_POINT ( 'NONE',  ( 17.96484262340118221, 49.93868534415484106, 7.964842623401181321 ) ) ;
#11929 = EDGE_CURVE ( 'NONE', #59079, #63992, #797, .T. ) ;
#11930 = CARTESIAN_POINT ( 'NONE',  ( 16.40814093676324603, 7.456968003263754419, -11.09922568453594671 ) ) ;
#11931 = CARTESIAN_POINT ( 'NONE',  ( 19.42250999205614548, 65.98035201082151957, -5.440088680355545492 ) ) ;
#11932 = CARTESIAN_POINT ( 'NONE',  ( 19.84674366389459266, 18.71726448433411960, -2.638427012816827677 ) ) ;
#11933 = CARTESIAN_POINT ( 'NONE',  ( 13.43411237798106583, 52.66530133659708213, -12.81628187352647252 ) ) ;
#11934 = CARTESIAN_POINT ( 'NONE',  ( 7.361572987183169658, -0.03273551566588185635, -9.846743663894592657 ) ) ;
#11935 = ORIENTED_EDGE ( 'NONE', *, *, #70927, .T. ) ;
#11936 = CARTESIAN_POINT ( 'NONE',  ( 1.821708436314942503, 56.66792564121897158, -6.500000000000043521 ) ) ;
#11937 = CARTESIAN_POINT ( 'NONE',  ( 0.2751277870542889192, 28.21833443783938122, 6.499999999999990230 ) ) ;
#11938 = CARTESIAN_POINT ( 'NONE',  ( 17.96484262340118221, 24.93868534415484461, 7.964842623401181321 ) ) ;
#11939 = CARTESIAN_POINT ( 'NONE',  ( 10.00000000000000178, 60.37363466993041783, 12.81628187352647608 ) ) ;
#11940 = CARTESIAN_POINT ( 'NONE',  ( 2.791683348922240793, 36.63393115100078035, 7.208316651077764092 ) ) ;
#11941 = CARTESIAN_POINT ( 'NONE',  ( 2.035157376598824452, 23.68868534415484461, 7.964842623401179544 ) ) ;
#11942 = CARTESIAN_POINT ( 'NONE',  ( 10.00000000000000000, 65.55374883491396076, -14.16423886937410082 ) ) ;
#11943 = VERTEX_POINT ( 'NONE', #92264 ) ;
#11944 = VECTOR ( 'NONE', #45272, 1000.000000000000000 ) ;
#11945 = B_SPLINE_CURVE_WITH_KNOTS ( 'NONE', 3,
 ( #16688, #69683, #18161, #55667, #1214, #40170 ),
 .UNSPECIFIED., .F., .F.,
 ( 4, 2, 4 ),
 ( 0.000000000000000000, 0.0002626113303184855600, 0.0005252226606369711200 ),
 .UNSPECIFIED. ) ;
#11946 = CARTESIAN_POINT ( 'NONE',  ( 2.035157376598822676, 12.43868534415483751, -7.964842623401177768 ) ) ;
#11947 = CARTESIAN_POINT ( 'NONE',  ( 2.035157376598824452, 28.68868534415484106, 7.964842623401179544 ) ) ;
#11949 = CARTESIAN_POINT ( 'NONE',  ( 7.084665262690076126, 32.02201867748816966, -10.88017736071110164 ) ) ;
#11948 = DIRECTION ( 'NONE',  ( 1.000000000000000000, -5.818595309480552676E-17, -0.000000000000000000 ) ) ;
#11950 = ORIENTED_EDGE ( 'NONE', *, *, #91444, .F. ) ;
#11951 = CARTESIAN_POINT ( 'NONE',  ( 0.1532563361054083140, 61.00893115100078745, 1.131784320476157264E-15 ) ) ;
#11952 = CARTESIAN_POINT ( 'NONE',  ( 2.035157376598822676, 27.43868534415483396, -7.964842623401177768 ) ) ;
#11953 = CARTESIAN_POINT ( 'NONE',  ( 18.52753015748618282, 63.92559781766745886, -4.923371831947291888 ) ) ;
#11954 = CARTESIAN_POINT ( 'NONE',  ( 19.72487221294570858, 70.00000000000000000, -6.000000000000000000 ) ) ;
#11955 = CARTESIAN_POINT ( 'NONE',  ( 6.565887622018943937, 58.08196800326376064, -12.81628187352647608 ) ) ;
#11956 = CARTESIAN_POINT ( 'NONE',  ( -4.164238869374099039, 31.80374883491396432, 8.674139862899312516E-16 ) ) ;
#11957 = CARTESIAN_POINT ( 'NONE',  ( 2.035157376598824452, 33.68868534415484106, 7.964842623401179544 ) ) ;
#11958 = CARTESIAN_POINT ( 'NONE',  ( 7.084665262690076126, 17.02201867748817676, -10.88017736071110164 ) ) ;
#11959 = CARTESIAN_POINT ( 'NONE',  ( 3.208591742434494964, 70.37446617634741131, -5.000000000000000000 ) ) ;
#11961 = EDGE_CURVE ( 'NONE', #25626, #70343, #23788, .T. ) ;
#11960 = CARTESIAN_POINT ( 'NONE',  ( 14.92337183194729633, 52.67559781766745175, 8.527530157486181039 ) ) ;
#11962 = CARTESIAN_POINT ( 'NONE',  ( -0.1503990784575247319, 22.22266099184918886, -6.262539305110083276 ) ) ;
#11963 = CARTESIAN_POINT ( 'NONE',  ( 19.84674366389459621, 18.50893115100078745, 7.409399052514197653E-17 ) ) ;
#11964 = CARTESIAN_POINT ( 'NONE',  ( -6.408140936763246032, -31.70969866340291077, -11.09922568453594316 ) ) ;
#11965 = CARTESIAN_POINT ( 'NONE',  ( 7.084665262690076126, 7.022018677488169658, -10.88017736071110164 ) ) ;
#11966 = CARTESIAN_POINT ( 'NONE',  ( 5.076628168052703671, 6.842264484334118713, 8.527530157486179263 ) ) ;
#11967 = CARTESIAN_POINT ( 'NONE',  ( 10.00000000000000178, 15.37363466993042138, 12.81628187352647608 ) ) ;
#11968 = CARTESIAN_POINT ( 'NONE',  ( 12.91533473730992121, 59.52201867748816966, 10.88017736071110164 ) ) ;
#11970 = CARTESIAN_POINT ( 'NONE',  ( 6.565887622018943937, 63.08196800326376064, -12.81628187352647608 ) ) ;
#11969 = CARTESIAN_POINT ( 'NONE',  ( 15.44008868035555793, 21.39701867748817321, -9.422509992056140149 ) ) ;
#11971 = CARTESIAN_POINT ( 'NONE',  ( 10.00000000000000178, 33.05374883491396787, 14.16423886937410082 ) ) ;
#11972 = SURFACE_STYLE_FILL_AREA ( #80474 ) ;
#11973 = ADVANCED_FACE ( 'NONE', ( #79716 ), #88191, .F. ) ;
#11974 = PRESENTATION_LAYER_ASSIGNMENT (  '', '', ( #64618 ) ) ;
#11975 = ADVANCED_FACE ( 'NONE', ( #18237 ), #39593, .T. ) ;
#11976 = CARTESIAN_POINT ( 'NONE',  ( 0.6178305044545818747, 58.49863466993042493, -9.382169495545419124 ) ) ;
#11977 = EDGE_CURVE ( 'NONE', #11450, #37577, #7628, .T. ) ;
#11978 = VERTEX_POINT ( 'NONE', #27689 ) ;
#11979 = CARTESIAN_POINT ( 'NONE',  ( -2.816281873526473856, 4.331968003263754419, 3.434112377981055619 ) ) ;
#11980 = CARTESIAN_POINT ( 'NONE',  ( 19.39188664607694790, 20.83703382326399733, -6.499999999999962697 ) ) ;
#11981 = CARTESIAN_POINT ( 'NONE',  ( -0.8801773607110991993, 32.85535201082151247, -2.915334737309923874 ) ) ;
#11982 = DIRECTION ( 'NONE',  ( -0.000000000000000000, -0.000000000000000000, 1.000000000000000000 ) ) ;
#11983 = EDGE_LOOP ( 'NONE', ( #69157, #33967, #8670, #67433 ) ) ;
#11984 = CARTESIAN_POINT ( 'NONE',  ( 17.20831665107776587, 19.13393115100078035, -7.208316651077762316 ) ) ;
#11985 = CARTESIAN_POINT ( 'NONE',  ( 14.92337183194729633, 7.675597817667451750, 8.527530157486181039 ) ) ;
#11986 = CARTESIAN_POINT ( 'NONE',  ( 0.1532563361054083140, 26.00893115100078745, 1.131784320476157264E-15 ) ) ;
#11987 = CARTESIAN_POINT ( 'NONE',  ( 1.472469842513823179, 15.59226448433411960, -4.923371831947296329 ) ) ;
#11988 = FILL_AREA_STYLE_COLOUR ( '', #12312 ) ;
#11989 = CIRCLE ( 'NONE', #34383, 0.5000000000000004441 ) ;
#11991 = DIRECTION ( 'NONE',  ( 0.000000000000000000, 0.000000000000000000, -1.000000000000000000 ) ) ;
#11990 = CARTESIAN_POINT ( 'NONE',  ( -0.8801773607110991993, 67.85535201082151957, -2.915334737309923874 ) ) ;
#11992 = CARTESIAN_POINT ( 'NONE',  ( 14.92337183194729633, 7.675597817667451750, 8.527530157486181039 ) ) ;
#11994 = VERTEX_POINT ( 'NONE', #72205 ) ;
#11993 = CARTESIAN_POINT ( 'NONE',  ( 0.1532563361054100626, 25.80059781766744820, -2.638427012816831230 ) ) ;
#11995 = CARTESIAN_POINT ( 'NONE',  ( 8.630000000000000782, 1.085138116723527427E-15, 4.000000000000000000 ) ) ;
#11996 = CARTESIAN_POINT ( 'NONE',  ( 19.38216949554541202, 0.9986346699304200492, 9.382169495545424454 ) ) ;
#11997 = EDGE_LOOP ( 'NONE', ( #97474, #92263, #43689, #21668 ) ) ;
#11998 = ORIENTED_EDGE ( 'NONE', *, *, #75508, .F. ) ;
#11999 = CARTESIAN_POINT ( 'NONE',  ( 15.44008868035555793, 6.397018677488170546, -9.422509992056140149 ) ) ;
#12000 = CARTESIAN_POINT ( 'NONE',  ( 17.08211943468705840, 20.13708216824730357, -12.26659068614894466 ) ) ;
#12001 = LINE ( 'NONE', #80000, #15247 ) ;
#12002 = EDGE_CURVE ( 'NONE', #54148, #16083, #49693, .T. ) ;
#12003 = CARTESIAN_POINT ( 'NONE',  ( 10.00000000000000000, 20.55374883491396787, -14.16423886937410082 ) ) ;
#12004 = CARTESIAN_POINT ( 'NONE',  ( -4.164238869374098151, 36.59541550158063217, -3.795296366450310543 ) ) ;
#12006 = CARTESIAN_POINT ( 'NONE',  ( -13.77306509549858760, 90.93909206156975245, -7.896286030156202784 ) ) ;
#12005 = SURFACE_SIDE_STYLE ('',( #87016 ) ) ;
#12007 = CARTESIAN_POINT ( 'NONE',  ( -0.8801773607110991993, 37.85535201082151247, -2.915334737309923874 ) ) ;
#12008 = CARTESIAN_POINT ( 'NONE',  ( -14.40939250469967448, 4.171366831970869137E-16, 1.618458416365661012 ) ) ;
#12009 = CIRCLE ( 'NONE', #95079, 1.000000000000000888 ) ;
#12010 = ORIENTED_EDGE ( 'NONE', *, *, #27413, .F. ) ;
#12011 = CARTESIAN_POINT ( 'NONE',  ( 17.20831665107776587, 19.13393115100078035, -7.208316651077762316 ) ) ;
#12013 = CARTESIAN_POINT ( 'NONE',  ( 1.472469842513823179, 16.42559781766745175, 4.923371831947296329 ) ) ;
#12012 = CARTESIAN_POINT ( 'NONE',  ( 0.5774900079438590739, 62.64701867748817676, -5.440088680355550821 ) ) ;
#12014 = CARTESIAN_POINT ( 'NONE',  ( 0.5774900079438590739, 7.647018677488171434, -5.440088680355550821 ) ) ;
#12015 = CARTESIAN_POINT ( 'NONE',  ( -2.816281873526473856, 49.12363466993042493, 9.499525473075851096E-16 ) ) ;
#12016 = CARTESIAN_POINT ( 'NONE',  ( 1.472469842513823179, 56.42559781766745886, 4.923371831947296329 ) ) ;
#12017 = CARTESIAN_POINT ( 'NONE',  ( 19.84674366389459266, 58.71726448433412315, -2.638427012816827677 ) ) ;
#12018 = CARTESIAN_POINT ( 'NONE',  ( 10.00000000000000000, 32.87363466993042493, -12.81628187352647608 ) ) ;
#12019 = CARTESIAN_POINT ( 'NONE',  ( -7.082119434687058401, -29.02958449841936073, -12.26659068614894110 ) ) ;
#12020 = CARTESIAN_POINT ( 'NONE',  ( 7.361572987183169658, 34.96726448433411605, -9.846743663894592657 ) ) ;
#12021 = CARTESIAN_POINT ( 'NONE',  ( 13.79529636645030344, 8.262082168247300018, 14.16423886937410614 ) ) ;
#12022 = EDGE_LOOP ( 'NONE', ( #18923, #95095, #8757, #7874 ) ) ;
#12023 = FACE_OUTER_BOUND ( 'NONE', #4858, .T. ) ;
#12024 = CIRCLE ( 'NONE', #61479, 14.49999999999999822 ) ;
#12025 = CARTESIAN_POINT ( 'NONE',  ( 4.559911319644449179, 47.23035201082150536, -9.422509992056141925 ) ) ;
#12026 = CARTESIAN_POINT ( 'NONE',  ( 7.084665262690076126, 47.02201867748818387, -10.88017736071110164 ) ) ;
#12027 = CARTESIAN_POINT ( 'NONE',  ( 6.204703633549690345, 45.76208216824729647, -14.16423886937410259 ) ) ;
#12028 = CARTESIAN_POINT ( 'NONE',  ( 0.1532563361054083140, 61.00893115100078745, 1.131784320476157264E-15 ) ) ;
#12029 = CARTESIAN_POINT ( 'NONE',  ( 10.00000000000000000, 62.87363466993042493, -12.81628187352647608 ) ) ;
#12030 = CARTESIAN_POINT ( 'NONE',  ( 4.559911319644449179, 37.23035201082150536, -9.422509992056141925 ) ) ;
#12031 = CARTESIAN_POINT ( 'NONE',  ( -3.638307330400850415, -8.269691488429794290, -2.500000000000000000 ) ) ;
#12032 = CARTESIAN_POINT ( 'NONE',  ( 22.81628187352647785, 21.41530133659708923, 3.434112377981063169 ) ) ;
#12033 = CARTESIAN_POINT ( 'NONE',  ( 19.84674366389459266, 53.30059781766744464, 2.638427012816836559 ) ) ;
#12034 = CARTESIAN_POINT ( 'NONE',  ( 5.440088680355556150, 19.73035201082151602, 9.422509992056138373 ) ) ;
#12035 = CARTESIAN_POINT ( 'NONE',  ( -0.8801773607111008646, 63.27201867748817676, 2.915334737309923430 ) ) ;
#12036 = CARTESIAN_POINT ( 'NONE',  ( -0.8801773607111009756, 3.063685344154837509, 1.068504757029289695E-15 ) ) ;
#12037 = CARTESIAN_POINT ( 'NONE',  ( 1.816707512666844604, 60.10290668512023871, -6.499999999999958256 ) ) ;
#12038 = CARTESIAN_POINT ( 'NONE',  ( 0.1532563361054100626, 0.8005978176674514168, -2.638427012816831230 ) ) ;
#12039 = CARTESIAN_POINT ( 'NONE',  ( -0.8801773607111009756, 68.06368534415484817, 1.068504757029289695E-15 ) ) ;
#12040 = DIRECTION ( 'NONE',  ( 0.3665012267242946375, -0.000000000000000000, 0.9304175679820254619 ) ) ;
#12041 = COLOUR_RGB ( '', 0.66274510, 0.83137255, 0.94901961) ;
#12042 = CARTESIAN_POINT ( 'NONE',  ( 18.52753015748618282, 28.92559781766745175, -4.923371831947291888 ) ) ;
#12043 = CARTESIAN_POINT ( 'NONE',  ( 0.5774900079438590739, 27.64701867748817676, -5.440088680355550821 ) ) ;
#12044 = CARTESIAN_POINT ( 'NONE',  ( 22.81628187352647785, 11.41530133659708390, 3.434112377981063169 ) ) ;
#12046 = CARTESIAN_POINT ( 'NONE',  ( -3.500000000000000888, 0.08935878030161711894, -3.750000000000001776 ) ) ;
#12045 = CARTESIAN_POINT ( 'NONE',  ( 7.084665262690076126, 32.02201867748816966, -10.88017736071110164 ) ) ;
#12047 = CARTESIAN_POINT ( 'NONE',  ( 13.43411237798106583, 32.66530133659708213, -12.81628187352647252 ) ) ;
#12048 = ORIENTED_EDGE ( 'NONE', *, *, #50125, .F. ) ;
#12049 = FACE_OUTER_BOUND ( 'NONE', #23072, .T. ) ;
#12051 = CARTESIAN_POINT ( 'NONE',  ( -12.60874940350953111, 15.00000000000000000, 7.160268045226944267 ) ) ;
#12050 = CARTESIAN_POINT ( 'NONE',  ( 19.38216949554541202, 20.99863466993042138, 9.382169495545424454 ) ) ;
#12052 = CYLINDRICAL_SURFACE ( 'NONE', #51536, 3.999999999999999112 ) ;
#12053 = CARTESIAN_POINT ( 'NONE',  ( -0.8801773607111008646, 28.27201867748817321, 2.915334737309923430 ) ) ;
#12054 = CARTESIAN_POINT ( 'NONE',  ( 24.16423886937409904, 59.09541550158063217, 3.795296366450317205 ) ) ;
#12055 = CARTESIAN_POINT ( 'NONE',  ( 19.84674366389459266, 48.30059781766745175, 2.638427012816836559 ) ) ;
#12056 = CARTESIAN_POINT ( 'NONE',  ( 12.63842701281683922, 9.550597817667449974, -9.846743663894590881 ) ) ;
#12057 = CARTESIAN_POINT ( 'NONE',  ( 17.96484262340118221, 64.93868534415483396, 7.964842623401181321 ) ) ;
#12058 = DIRECTION ( 'NONE',  ( 3.035766082959409260E-14, 1.000000000000000000, 0.000000000000000000 ) ) ;
#12059 = CARTESIAN_POINT ( 'NONE',  ( 10.00000000000000000, 30.55374883491397142, -14.16423886937410082 ) ) ;
#12060 =( GEOMETRIC_REPRESENTATION_CONTEXT ( 3 ) GLOBAL_UNCERTAINTY_ASSIGNED_CONTEXT ( ( #4319 ) ) GLOBAL_UNIT_ASSIGNED_CONTEXT ( ( #64257, #56772, #49271 ) ) REPRESENTATION_CONTEXT ( 'NONE', 'WORKASPACE' ) );
#12061 = DIRECTION ( 'NONE',  ( 0.000000000000000000, 0.000000000000000000, 1.000000000000000000 ) ) ;
#12062 = CARTESIAN_POINT ( 'NONE',  ( -3.772059543480756005, -0.8421633283344439613, -4.000000000000000000 ) ) ;
#12063 = ORIENTED_EDGE ( 'NONE', *, *, #83219, .F. ) ;
#12064 = VERTEX_POINT ( 'NONE', #26224 ) ;
#12065 = CARTESIAN_POINT ( 'NONE',  ( 22.26659068614895176, 54.72041550158063217, -7.082119434687042414 ) ) ;
#12066 = CARTESIAN_POINT ( 'NONE',  ( 17.08211943468705840, 45.13708216824730357, -12.26659068614894466 ) ) ;
#12067 = CARTESIAN_POINT ( 'NONE',  ( 14.92337183194729633, 17.67559781766745175, 8.527530157486181039 ) ) ;
#12069 = CARTESIAN_POINT ( 'NONE',  ( 16.40814093676323893, 30.79030133659708923, 11.09922568453595026 ) ) ;
#12068 = AXIS2_PLACEMENT_3D ( 'NONE', #16233, #14768, #37271 ) ;
#12070 = CARTESIAN_POINT ( 'NONE',  ( 0.000000000000000000, 0.000000000000000000, 0.000000000000000000 ) ) ;
#12071 = DIRECTION ( 'NONE',  ( -0.000000000000000000, -1.000000000000000000, -0.000000000000000000 ) ) ;
#12072 = SURFACE_STYLE_FILL_AREA ( #42574 ) ;
#12073 = CARTESIAN_POINT ( 'NONE',  ( -2.266590686148945544, 37.22041550158063217, 7.082119434687048631 ) ) ;
#12074 = CARTESIAN_POINT ( 'NONE',  ( 10.00000000000000178, 7.258931151000785675, 9.846743663894594434 ) ) ;
#12075 = CARTESIAN_POINT ( 'NONE',  ( -7.208316651077764980, 0.3839311510007899497, -7.208316651077759651 ) ) ;
#12076 = VERTEX_POINT ( 'NONE', #96206 ) ;
#12077 = CARTESIAN_POINT ( 'NONE',  ( 8.979999999999991545, 21.00000000000000000, 0.000000000000000000 ) ) ;
#12078 = ORIENTED_EDGE ( 'NONE', *, *, #67276, .F. ) ;
#12080 = ADVANCED_FACE ( 'NONE', ( #34692 ), #3733, .T. ) ;
#12079 = DIRECTION ( 'NONE',  ( -0.000000000000000000, -1.000000000000000000, -0.000000000000000000 ) ) ;
#12081 = ORIENTED_EDGE ( 'NONE', *, *, #50492, .T. ) ;
#12082 = CARTESIAN_POINT ( 'NONE',  ( -4.164238869374098151, 11.59541550158063217, -3.795296366450310543 ) ) ;
#12084 = CARTESIAN_POINT ( 'NONE',  ( 4.559911319644449179, 22.23035201082150536, -9.422509992056141925 ) ) ;
#12083 = CARTESIAN_POINT ( 'NONE',  ( 15.44008868035555793, 26.39701867748817321, -9.422509992056140149 ) ) ;
#12086 = CARTESIAN_POINT ( 'NONE',  ( -2.816281873526473856, 19.33196800326375708, 3.434112377981055619 ) ) ;
#12085 = CARTESIAN_POINT ( 'NONE',  ( 2.791683348922240793, 51.63393115100078745, 7.208316651077764092 ) ) ;
#12087 = CARTESIAN_POINT ( 'NONE',  ( 9.779999999999988702, 27.00436609429084811, -3.000000000000000000 ) ) ;
#12088 = AXIS2_PLACEMENT_3D ( 'NONE', #39627, #70609, #17127 ) ;
#12089 = ADVANCED_FACE ( 'NONE', ( #20193 ), #58173, .T. ) ;
#12090 = CIRCLE ( 'NONE', #59975, 15.00000000000000000 ) ;
#12092 = CARTESIAN_POINT ( 'NONE',  ( -1.099225684535947600, 14.54030133659708568, 6.408140936763237150 ) ) ;
#12091 = VECTOR ( 'NONE', #75498, 1000.000000000000000 ) ;
#12093 = EDGE_CURVE ( 'NONE', #14429, #43985, #12690, .T. ) ;
#12094 = VERTEX_POINT ( 'NONE', #42703 ) ;
#12095 = CARTESIAN_POINT ( 'NONE',  ( 1.472469842513823179, 26.42559781766745175, 4.923371831947296329 ) ) ;
#12096 = CARTESIAN_POINT ( 'NONE',  ( -4.164238869374099039, 66.80374883491396076, 8.674139862899312516E-16 ) ) ;
#12097 = EDGE_LOOP ( 'NONE', ( #4844, #67880, #1063, #67306 ) ) ;
#12098 = CARTESIAN_POINT ( 'NONE',  ( -0.8801773607111008646, 8.272018677488171434, 2.915334737309923430 ) ) ;
#12099 = ORIENTED_EDGE ( 'NONE', *, *, #23783, .F. ) ;
#12100 = CARTESIAN_POINT ( 'NONE',  ( 19.42250999205614548, 40.98035201082150536, -5.440088680355545492 ) ) ;
#12101 = CARTESIAN_POINT ( 'NONE',  ( 20.88017736071110875, 50.77201867748817676, -2.915334737309920765 ) ) ;
#12102 = CARTESIAN_POINT ( 'NONE',  ( -0.8801773607110991993, 57.85535201082149825, -2.915334737309923874 ) ) ;
#12103 = CARTESIAN_POINT ( 'NONE',  ( 20.03932841506543738, 5.621614419605015733, -6.397827110478957024 ) ) ;
#12104 = CARTESIAN_POINT ( 'NONE',  ( 10.00000000000000178, 39.31368534415484106, 10.88017736071110342 ) ) ;
#12105 = CARTESIAN_POINT ( 'NONE',  ( 0.000000000000000000, 14.49999999999999822, 0.000000000000000000 ) ) ;
#12106 = CARTESIAN_POINT ( 'NONE',  ( -7.750000000000000000, 40.99999999999999289, -6.500000000000000888 ) ) ;
#12107 = AXIS2_PLACEMENT_3D ( 'NONE', #78178, #48166, #62676 ) ;
#12108 = CARTESIAN_POINT ( 'NONE',  ( 0.1532563361054100626, 20.80059781766744464, -2.638427012816831230 ) ) ;
#12109 = ORIENTED_EDGE ( 'NONE', *, *, #85272, .T. ) ;
#12110 = CARTESIAN_POINT ( 'NONE',  ( 1.472469842513823179, 51.42559781766745886, 4.923371831947296329 ) ) ;
#12111 = CARTESIAN_POINT ( 'NONE',  ( 1.274849032794292736, 62.55509018479936145, -6.499999999999977796 ) ) ;
#12112 = EDGE_CURVE ( 'NONE', #89066, #75564, #79484, .T. ) ;
#12113 = CARTESIAN_POINT ( 'NONE',  ( -7.081429851441987999, -84.79152421822195151, 3.750000000000000444 ) ) ;
#12114 =( LENGTH_UNIT ( ) NAMED_UNIT ( * ) SI_UNIT ( .MILLI., .METRE. ) );
#12115 = CARTESIAN_POINT ( 'NONE',  ( -1.175527996596911873, 15.00000000000000711, -14.57931687975697344 ) ) ;
#12117 = CARTESIAN_POINT ( 'NONE',  ( 10.00000000000000178, 32.25893115100078745, 9.846743663894594434 ) ) ;
#12116 = CARTESIAN_POINT ( 'NONE',  ( 17.20831665107776587, 64.13393115100079456, -7.208316651077762316 ) ) ;
#12118 = CARTESIAN_POINT ( 'NONE',  ( -4.164238869374099927, 67.01208216824728936, 3.795296366450308767 ) ) ;
#12119 = DIRECTION ( 'NONE',  ( 0.000000000000000000, 0.000000000000000000, 1.000000000000000000 ) ) ;
#12120 = ORIENTED_EDGE ( 'NONE', *, *, #13330, .F. ) ;
#12121 = CARTESIAN_POINT ( 'NONE',  ( -7.003840667633812522, 2.083701050245578834E-16, 12.84073839985649812 ) ) ;
#12122 = CARTESIAN_POINT ( 'NONE',  ( 5.076628168052703671, 36.84226448433412315, 8.527530157486179263 ) ) ;
#12123 = CARTESIAN_POINT ( 'NONE',  ( -1.099225684535947600, 64.54030133659709634, 6.408140936763237150 ) ) ;
#12124 = CIRCLE ( 'NONE', #34520, 0.2500000000000002220 ) ;
#12125 = CARTESIAN_POINT ( 'NONE',  ( 3.591859063236763294, 3.290301336597087012, -11.09922568453595026 ) ) ;
#12126 = CARTESIAN_POINT ( 'NONE',  ( 17.20831665107776587, 7.883931151000784787, 7.208316651077764980 ) ) ;
#12127 = LINE ( 'NONE', #42150, #55373 ) ;
#12128 = CARTESIAN_POINT ( 'NONE',  ( 2.791683348922237240, 5.383931151000785675, -7.208316651077763204 ) ) ;
#12129 = CARTESIAN_POINT ( 'NONE',  ( 12.63842701281683034, 57.46726448433411605, 9.846743663894596210 ) ) ;
#12130 = ADVANCED_FACE ( 'NONE', ( #19211 ), #35690, .F. ) ;
#12131 = DIRECTION ( 'NONE',  ( 0.000000000000000000, 0.000000000000000000, 1.000000000000000000 ) ) ;
#12132 = ORIENTED_EDGE ( 'NONE', *, *, #67277, .T. ) ;
#12133 = CARTESIAN_POINT ( 'NONE',  ( 20.88017736071110164, 10.35535201082150714, 2.915334737309930979 ) ) ;
#12134 = CARTESIAN_POINT ( 'NONE',  ( 18.52753015748617571, 13.09226448433411960, 4.923371831947298993 ) ) ;
#12135 = CARTESIAN_POINT ( 'NONE',  ( 20.88017736071110164, 45.35535201082149115, 2.915334737309930979 ) ) ;
#12137 = CARTESIAN_POINT ( 'NONE',  ( -12.35505582470280572, -0.03417435944610275333, 10.16021613965622095 ) ) ;
#12136 = CARTESIAN_POINT ( 'NONE',  ( 13.43411237798105340, 25.58196800326374998, 12.81628187352647963 ) ) ;
#12138 = DIRECTION ( 'NONE',  ( -1.000000000000000000, 0.000000000000000000, 0.000000000000000000 ) ) ;
#12139 = CARTESIAN_POINT ( 'NONE',  ( 8.838651438279566008, 0.04922511925147201456, -11.81204219878339323 ) ) ;
#12140 = CARTESIAN_POINT ( 'NONE',  ( 22.81628187352648496, 6.831968003263753531, -3.434112377981050290 ) ) ;
#12141 = CARTESIAN_POINT ( 'NONE',  ( 19.84674366389459621, 63.50893115100078745, 7.409399052514197653E-17 ) ) ;
#12142 = CARTESIAN_POINT ( 'NONE',  ( 10.00000000000000178, 12.25893115100078568, 9.846743663894594434 ) ) ;
#12143 = CARTESIAN_POINT ( 'NONE',  ( 5.440088680355556150, -25.26964798917849109, 9.422509992056138373 ) ) ;
#12144 = CARTESIAN_POINT ( 'NONE',  ( 10.00000000000000000, 22.87363466993042138, -12.81628187352647608 ) ) ;
#12145 = CARTESIAN_POINT ( 'NONE',  ( 1.711636803080569313, 51.84492782695771496, -6.500000000000077272 ) ) ;
#12147 = CARTESIAN_POINT ( 'NONE',  ( -9.402796353260967521, 0.5000000000000004441, -11.68706210897770248 ) ) ;
#12146 = CARTESIAN_POINT ( 'NONE',  ( -0.8801773607111008646, 28.27201867748817321, 2.915334737309923430 ) ) ;
#12148 = DIRECTION ( 'NONE',  ( 0.000000000000000000, 1.000000000000000000, 0.000000000000000000 ) ) ;
#12149 = CARTESIAN_POINT ( 'NONE',  ( -0.3689425029237898834, 51.17874883491397497, -10.36894250292378850 ) ) ;
#12150 = DIRECTION ( 'NONE',  ( 0.9975640502598257520, -0.06975647374410356982, 0.000000000000000000 ) ) ;
#12151 = CARTESIAN_POINT ( 'NONE',  ( 13.43411237798105340, 35.58196800326375353, 12.81628187352647963 ) ) ;
#12152 = CARTESIAN_POINT ( 'NONE',  ( 17.96484262340118221, 21.18868534415483396, -7.964842623401177768 ) ) ;
#12153 = COLOUR_RGB ( '', 0.09019608, 0.27058824, 0.51372549) ;
#12154 = CIRCLE ( 'NONE', #10518, 14.49999999999999822 ) ;
#12155 = CARTESIAN_POINT ( 'NONE',  ( 12.63842701281683922, 54.55059781766745175, -9.846743663894590881 ) ) ;
#12156 = CARTESIAN_POINT ( 'NONE',  ( 12.91533473730992121, 49.52201867748817676, 10.88017736071110164 ) ) ;
#12157 = CARTESIAN_POINT ( 'NONE',  ( -0.3689425029237898834, 36.17874883491396787, -10.36894250292378850 ) ) ;
#12158 = FACE_OUTER_BOUND ( 'NONE', #64512, .T. ) ;
#12159 = CARTESIAN_POINT ( 'NONE',  ( 17.20831665107776587, 27.88393115100078390, 7.208316651077764980 ) ) ;
#12160 = SURFACE_STYLE_FILL_AREA ( #73144 ) ;
#12161 = CARTESIAN_POINT ( 'NONE',  ( 0.6178305044545818747, 3.498634669930420049, -9.382169495545419124 ) ) ;
#12162 = ORIENTED_EDGE ( 'NONE', *, *, #97691, .F. ) ;
#12163 = CARTESIAN_POINT ( 'NONE',  ( 20.15039907845753930, 11.74884699246888964, 6.262539305110064625 ) ) ;
#12164 = CARTESIAN_POINT ( 'NONE',  ( 20.88017736071110164, 15.35535201082150358, 2.915334737309930979 ) ) ;
#12165 = CARTESIAN_POINT ( 'NONE',  ( -4.164238869374098151, 21.59541550158063217, -3.795296366450310543 ) ) ;
#12166 = EDGE_CURVE ( 'NONE', #29547, #3599, #92261, .T. ) ;
#12167 = CARTESIAN_POINT ( 'NONE',  ( 5.076628168052704559, 15.17559781766745175, -8.527530157486179263 ) ) ;
#12168 = CARTESIAN_POINT ( 'NONE',  ( 12.63842701281683922, 64.55059781766745175, -9.846743663894590881 ) ) ;
#12169 = CARTESIAN_POINT ( 'NONE',  ( 20.88017736071110164, 30.35535201082151247, 2.915334737309930979 ) ) ;
#12170 =( BOUNDED_CURVE ( )  B_SPLINE_CURVE ( 2, ( #46006, #52995, #24000, #54959, #84980, #15027, #8979, #7528, #85480 ),
 .UNSPECIFIED., .F., .F. ) 
 B_SPLINE_CURVE_WITH_KNOTS ( ( 3, 2, 2, 2, 3 ),
 ( 0.1891432315068940218, 0.1904761904761904656, 0.1964285714285714246, 0.2023809523809523836, 0.2037139113502489662 ),
 .UNSPECIFIED. ) 
 CURVE ( )  GEOMETRIC_REPRESENTATION_ITEM ( )  RATIONAL_B_SPLINE_CURVE ( ( 0.9881565478350731180, 0.9923695281211488695, 1.000000000000000000, 0.9659258262890683122, 1.000000000000000000, 0.9659258262890683122, 1.000000000000000000, 0.9923695281211482033, 0.9881565478350723408 ) ) 
 REPRESENTATION_ITEM ( '' )  );
#12171 = DIRECTION ( 'NONE',  ( 0.8070303256584299145, -0.5905099943842175847, 0.000000000000000000 ) ) ;
#12172 = CARTESIAN_POINT ( 'NONE',  ( -44.74606106857038412, 105.1870489192399845, -5.398875195867286259 ) ) ;
#12173 = EDGE_CURVE ( 'NONE', #31069, #97822, #30004, .T. ) ;
#12174 = ORIENTED_EDGE ( 'NONE', *, *, #68028, .F. ) ;
#12175 = CARTESIAN_POINT ( 'NONE',  ( 1.472469842513823179, 40.59226448433411605, -4.923371831947296329 ) ) ;
#12176 = ORIENTED_EDGE ( 'NONE', *, *, #24423, .F. ) ;
#12177 = EDGE_LOOP ( 'NONE', ( #30416, #67614, #8549, #63250 ) ) ;
#12178 = CARTESIAN_POINT ( 'NONE',  ( 11.25000000000000355, 10.42180217785154639, -2.602085213965210642E-15 ) ) ;
#12179 = CARTESIAN_POINT ( 'NONE',  ( 10.00000000000000178, 3.053748834913967425, 14.16423886937410082 ) ) ;
#12180 = CARTESIAN_POINT ( 'NONE',  ( 6.204703633549690345, 10.76208216824729824, -14.16423886937410259 ) ) ;
#12181 = CARTESIAN_POINT ( 'NONE',  ( -0.8801773607110991993, 47.85535201082150536, -2.915334737309923874 ) ) ;
#12182 = CARTESIAN_POINT ( 'NONE',  ( -4.164238869374099039, 61.80374883491397497, 8.674139862899312516E-16 ) ) ;
#12183 = CARTESIAN_POINT ( 'NONE',  ( 7.361572987183170547, 67.05059781766746596, 9.846743663894590881 ) ) ;
#12184 = CARTESIAN_POINT ( 'NONE',  ( 7.361572987183169658, 34.96726448433411605, -9.846743663894592657 ) ) ;
#12185 = CARTESIAN_POINT ( 'NONE',  ( -1.783843307429720415, 13.12729635533385597, -9.500000000000000000 ) ) ;
#12187 = CARTESIAN_POINT ( 'NONE',  ( -1.099225684535947600, 8.706968003263753531, -6.408140936763238038 ) ) ;
#12186 = CARTESIAN_POINT ( 'NONE',  ( 20.88017736071110519, 30.56368534415484106, 2.639326808657452039E-16 ) ) ;
#12188 = CARTESIAN_POINT ( 'NONE',  ( 13.79529636645031943, 50.34541550158064638, -14.16423886937409904 ) ) ;
#12189 = CARTESIAN_POINT ( 'NONE',  ( 4.559911319644449179, 7.230352010821505360, -9.422509992056141925 ) ) ;
#12190 = CARTESIAN_POINT ( 'NONE',  ( -0.2002127540270661199, 0.02465945891864366329, 6.181800700214927780 ) ) ;
#12191 = CARTESIAN_POINT ( 'NONE',  ( -6.732636091893172470, -88.11213685669366669, -3.750000000000000000 ) ) ;
#12192 = CARTESIAN_POINT ( 'NONE',  ( -2.638427012816824124, -32.94940218233254825, 9.846743663894596210 ) ) ;
#12193 = VERTEX_POINT ( 'NONE', #51187 ) ;
#12194 = DIRECTION ( 'NONE',  ( 1.000000000000000000, 0.000000000000000000, 0.000000000000000000 ) ) ;
#12195 = ORIENTED_EDGE ( 'NONE', *, *, #21286, .T. ) ;
#12196 = ORIENTED_EDGE ( 'NONE', *, *, #39446, .F. ) ;
#12197 = CIRCLE ( 'NONE', #66518, 15.00000000000000000 ) ;
#12198 = CARTESIAN_POINT ( 'NONE',  ( -4.164238869374098151, 51.59541550158063217, -3.795296366450310543 ) ) ;
#12199 = CARTESIAN_POINT ( 'NONE',  ( 10.00000000000000178, 32.25893115100078745, 9.846743663894594434 ) ) ;
#12200 = CARTESIAN_POINT ( 'NONE',  ( 17.96484262340118221, 56.18868534415484817, -7.964842623401177768 ) ) ;
#12201 = CARTESIAN_POINT ( 'NONE',  ( 19.72487221294570858, 36.86607318730075633, 6.500000000000000888 ) ) ;
#12202 = CARTESIAN_POINT ( 'NONE',  ( 20.88017736071110519, 60.56368534415484106, 2.639326808657452039E-16 ) ) ;
#12203 = PRESENTATION_LAYER_ASSIGNMENT (  '', '', ( #55310 ) ) ;
#12204 = EDGE_CURVE ( 'NONE', #651, #3863, #90651, .T. ) ;
#12205 = CARTESIAN_POINT ( 'NONE',  ( 22.81628187352648496, 56.83196800326374643, -3.434112377981050290 ) ) ;
#12206 = CARTESIAN_POINT ( 'NONE',  ( -6.408140936763246032, 3.290301336597092785, -11.09922568453594316 ) ) ;
#12207 = EDGE_CURVE ( 'NONE', #9538, #27610, #59352, .T. ) ;
#12208 = ORIENTED_EDGE ( 'NONE', *, *, #96632, .T. ) ;
#12209 = CARTESIAN_POINT ( 'NONE',  ( 6.204703633549690345, 22.84541550158062861, 14.16423886937410082 ) ) ;
#12210 = ORIENTED_EDGE ( 'NONE', *, *, #368, .F. ) ;
#12211 = CARTESIAN_POINT ( 'NONE',  ( 3.591859063236763294, 23.29030133659708568, -11.09922568453595026 ) ) ;
#12212 = ORIENTED_EDGE ( 'NONE', *, *, #59192, .T. ) ;
#12213 = CARTESIAN_POINT ( 'NONE',  ( -2.816281873526473856, 49.12363466993042493, 9.499525473075851096E-16 ) ) ;
#12214 = CARTESIAN_POINT ( 'NONE',  ( 14.92337183194729988, 19.34226448433411960, -8.527530157486177487 ) ) ;
#12215 = CARTESIAN_POINT ( 'NONE',  ( 0.5774900079438607392, 18.48035201082150536, 5.440088680355550821 ) ) ;
#12216 = CARTESIAN_POINT ( 'NONE',  ( 3.591859063236761518, 54.95696800326376064, 11.09922568453594849 ) ) ;
#12217 = CARTESIAN_POINT ( 'NONE',  ( 14.92337183194729633, 37.67559781766745175, 8.527530157486181039 ) ) ;
#12218 = COLOUR_RGB ( '', 0.66274510, 0.83137255, 0.94901961) ;
#12220 = EDGE_LOOP ( 'NONE', ( #19228, #69543, #61895, #7567 ) ) ;
#12219 = CARTESIAN_POINT ( 'NONE',  ( -12.50534872682736065, 15.00000000000000000, 7.339363270777414350 ) ) ;
#12221 = CARTESIAN_POINT ( 'NONE',  ( 17.96484262340118221, 66.18868534415483396, -7.964842623401177768 ) ) ;
#12222 = CARTESIAN_POINT ( 'NONE',  ( -9.240973841163453883, 4.157471065789850032E-16, -11.17382667070385160 ) ) ;
#12223 = STYLED_ITEM ( 'NONE', ( #44071 ), #88026 ) ;
#12224 = DIRECTION ( 'NONE',  ( 0.000000000000000000, 0.000000000000000000, 1.000000000000000000 ) ) ;
#12225 = CARTESIAN_POINT ( 'NONE',  ( 17.20831665107776587, 12.88393115100078390, 7.208316651077764980 ) ) ;
#12226 = CARTESIAN_POINT ( 'NONE',  ( 16.40814093676323893, 20.79030133659708923, 11.09922568453595026 ) ) ;
#12227 = CARTESIAN_POINT ( 'NONE',  ( -1.983216688681034068, -0.03417435944610275333, 14.11131997956736406 ) ) ;
#12228 = EDGE_CURVE ( 'NONE', #74162, #87326, #60154, .T. ) ;
#12229 = CARTESIAN_POINT ( 'NONE',  ( 12.63842701281683922, 44.55059781766745175, -9.846743663894590881 ) ) ;
#12230 = DIRECTION ( 'NONE',  ( -0.9887436111420608853, -0.1496197561345335991, 0.000000000000000000 ) ) ;
#12231 = CARTESIAN_POINT ( 'NONE',  ( 2.917880565312948704, 22.63708216824730002, 12.26659068614894643 ) ) ;
#12232 = CARTESIAN_POINT ( 'NONE',  ( 2.791683348922237240, 30.38393115100078390, -7.208316651077763204 ) ) ;
#12233 = CARTESIAN_POINT ( 'NONE',  ( 10.00000000000000000, 47.87363466993042493, -12.81628187352647608 ) ) ;
#12235 = CARTESIAN_POINT ( 'NONE',  ( 1.274849032794199255, 23.57228050351030646, 6.499999999999850786 ) ) ;
#12234 = FACE_OUTER_BOUND ( 'NONE', #14359, .T. ) ;
#12236 = CARTESIAN_POINT ( 'NONE',  ( 15.44008868035555260, 59.73035201082151247, 9.422509992056143702 ) ) ;
#12237 = CARTESIAN_POINT ( 'NONE',  ( 6.565887622018943937, 15.16530133659708568, 12.81628187352647430 ) ) ;
#12238 = CARTESIAN_POINT ( 'NONE',  ( -13.40508947812791796, 15.00000000000000000, -5.527528931052510863 ) ) ;
#12239 = CARTESIAN_POINT ( 'NONE',  ( 7.361572987183170547, 37.05059781766744464, 9.846743663894590881 ) ) ;
#12240 = CARTESIAN_POINT ( 'NONE',  ( 10.00000000000000000, 31.81368534415483751, -10.88017736071110342 ) ) ;
#12241 = CARTESIAN_POINT ( 'NONE',  ( 6.565887622018943937, 35.16530133659708923, 12.81628187352647430 ) ) ;
#12242 = VECTOR ( 'NONE', #66735, 1000.000000000000000 ) ;
#12243 = CARTESIAN_POINT ( 'NONE',  ( 2.791683348922240793, 36.63393115100078035, 7.208316651077764092 ) ) ;
#12244 = AXIS2_PLACEMENT_3D ( 'NONE', #71880, #18893, #77905 ) ;
#12245 = CARTESIAN_POINT ( 'NONE',  ( -216.5314366952507612, -104.0243955020849569, -81.87442926164645485 ) ) ;
#12246 = CARTESIAN_POINT ( 'NONE',  ( -2.258648100792393532, 0.04922511925146987738, 14.57890972981271993 ) ) ;
#12247 = CARTESIAN_POINT ( 'NONE',  ( 20.88017736071110875, 35.77201867748816966, -2.915334737309920765 ) ) ;
#12248 = ORIENTED_EDGE ( 'NONE', *, *, #58466, .T. ) ;
#12249 = DIRECTION ( 'NONE',  ( 0.000000000000000000, 1.000000000000000000, 0.000000000000000000 ) ) ;
#12250 = CARTESIAN_POINT ( 'NONE',  ( 2.035157376598824452, 3.688685344154837953, 7.964842623401179544 ) ) ;
#12252 = CARTESIAN_POINT ( 'NONE',  ( 10.00000000000000000, 26.81368534415484106, -10.88017736071110342 ) ) ;
#12251 = CARTESIAN_POINT ( 'NONE',  ( 7.361572987183169658, 59.96726448433410894, -9.846743663894592657 ) ) ;
#12253 = FACE_OUTER_BOUND ( 'NONE', #50627, .T. ) ;
#12254 = CARTESIAN_POINT ( 'NONE',  ( -0.8801773607111008646, 53.27201867748816966, 2.915334737309923430 ) ) ;
#12255 = CARTESIAN_POINT ( 'NONE',  ( 2.035157376598824452, 23.68868534415484461, 7.964842623401179544 ) ) ;
#12256 = CARTESIAN_POINT ( 'NONE',  ( 19.05914839598885635, 49.96693863883977116, 6.499999999999962697 ) ) ;
#12257 = CARTESIAN_POINT ( 'NONE',  ( 14.92337183194729988, 29.34226448433411960, -8.527530157486177487 ) ) ;
#12258 = LINE ( 'NONE', #74226, #21814 ) ;
#12259 = CARTESIAN_POINT ( 'NONE',  ( 17.20831665107776587, 47.88393115100078745, 7.208316651077764980 ) ) ;
#12261 = FILL_AREA_STYLE_COLOUR ( '', #25031 ) ;
#12260 = CARTESIAN_POINT ( 'NONE',  ( -0.3689425029237881626, 47.42874883491396787, 10.36894250292379027 ) ) ;
#12262 = CARTESIAN_POINT ( 'NONE',  ( 11.22915323889580463, -0.03417435944610275333, -8.773176023390609757 ) ) ;
#12263 = CARTESIAN_POINT ( 'NONE',  ( 2.917880565312950480, 5.970415501580634832, -12.26659068614894821 ) ) ;
#12264 = CARTESIAN_POINT ( 'NONE',  ( 22.26659068614895176, 34.72041550158063927, -7.082119434687042414 ) ) ;
#12265 = STYLED_ITEM ( 'NONE', ( #95921 ), #40986 ) ;
#12266 = CARTESIAN_POINT ( 'NONE',  ( 6.565887622018943937, 10.16530133659708746, 12.81628187352647430 ) ) ;
#12267 = CARTESIAN_POINT ( 'NONE',  ( -10.00000000000007105, 92.00000000000000000, 5.000000000000000000 ) ) ;
#12268 = CARTESIAN_POINT ( 'NONE',  ( 4.559911319644449179, 13.89701867748817321, 9.422509992056141925 ) ) ;
#12269 = CARTESIAN_POINT ( 'NONE',  ( 0.1532563361054082862, 31.21726448433412315, 2.638427012816831674 ) ) ;
#12270 = DIRECTION ( 'NONE',  ( 0.000000000000000000, 0.000000000000000000, 1.000000000000000000 ) ) ;
#12272 = B_SPLINE_CURVE_WITH_KNOTS ( 'NONE', 3,
 ( #14396, #44867, #75370, #41342, #2852, #24365 ),
 .UNSPECIFIED., .F., .F.,
 ( 4, 2, 4 ),
 ( 3.409110551496111039E-05, 0.0004400426677367860295, 0.0008459942299586109419 ),
 .UNSPECIFIED. ) ;
#12271 = CARTESIAN_POINT ( 'NONE',  ( 17.96484262340118221, 61.18868534415482685, -7.964842623401177768 ) ) ;
#12273 = DIRECTION ( 'NONE',  ( 1.000000000000000000, 0.000000000000000000, 0.000000000000000000 ) ) ;
#12274 = CIRCLE ( 'NONE', #90495, 14.49999999999999822 ) ;
#12275 = UNCERTAINTY_MEASURE_WITH_UNIT (LENGTH_MEASURE( 1.000000000000000082E-05 ), #83322, 'distance_accuracy_value', 'NONE');
#12276 =( BOUNDED_SURFACE ( )  B_SPLINE_SURFACE ( 1, 2, ( 
 ( #31508, #9511, #41005, #573, #62009, #56004, #92509, #24037, #40012, #54507, #16534, #47010, #70516, #77501, #93501, #2534, #86507, #9013, #39530, #1547, #63491, #2038, #25026, #73442, #42469, #11965, #72455, #95970, #72952, #4482, #50449, #71974, #20458, #50948, #42961, #94478, #10986, #80956, #79968, #88950, #96471, #49462, #41991, #25995, #87470, #34453, #86979, #3498, #56490, #12455, #65447, #11474, #12944, #57462, #34948, #88454, #33955, #3987, #64945, #95472, #19955, #49962, #56967, #18489, #26962, #63964, #3019, #87955, #19472, #27455, #80466, #41506, #57947, #81443, #4967, #18984, #35449, #65944, #48977, #33468, #64459, #94966, #26468, #79486, #27943, #58435, #71506, #68427, #52910, #13952, #14444, #44425, #74930, #67438, #98949, #73941, #66437, #30405, #81932, #75421, #28923, #13440, #45411, #37443, #89443, #90911, #6429, #36941, #22936, #60907, #6936, #43927, #98454, #67934, #28445, #97959, #44914, #29910, #21949, #53404, #14942, #43440, #7440, #5469, #20957, #60416, #52428, #22439, #74425, #5953, #36445, #29414, #75916, #59427, #82426, #83424, #66937, #59919, #91410, #35941, #37937, #83913, #96972, #51942, #90407, #58942, #82926, #51444, #97458, #89929, #21444, #77876, #77378, #23915, #15913, #68920, #32867, #84897, #55881, #15441, #53907, #8891, #45921, #8407, #38914, #32372, #92877, #47868, #69402, #31385, #16901, #923, #24411, #63367, #76893, #55385, #17400, #61885, #46887, #1421, #70395, #84416, #69901, #448, #46404, #9388, #39892, #93869, #92390, #1913, #54384, #16409, #25396, #39407, #70891, #93375, #76410, #62877, #7925, #47377, #24902, #38422, #85886, #91903, #31873, #62373, #54877, #23428, #85388, #30899, #78373, #9892, #40396, #2408, #61393, #64826, #34831, #48853, #25876, #72827, #27331, #11351, #78870, #87832, #33831, #42840, #35323, #95343, #56377, #73324, #41391, #18865, #86866, #57828, #88337, #71859, #49347, #72335, #42351, #18374, #41871, #71387, #79362, #80346, #49834, #4849, #10870, #4365, #3370, #64339, #96353, #79848, #65818, #65323, #27823, #95846, #86379, #19350, #19834, #48365, #11843, #63844, #3867, #94850, #34330, #94357, #26350, #17881, #50323, #87351, #80836, #26842, #56852, #57337, #12336, #10379, #40882, #2900, #33350, #82301, #50833, #59797, #5827, #14825, #7314, #36820, #28323, #45301, #13322, #89804, #58814, #6811, #21326, #51814, #37817, #75796, #21825, #89323, #14323, #52309, #43320, #13823, #90288, #82801, #67312, #68309, #29790, #58309, #22321, #88825, #35826, #29302, #97837, #75299, #96848, #20831, #51320, #44304, #60302, #74302, #97336, #44794, #81804, #74807, #98831 ),
 ( #37327, #59307, #28809, #6313, #83300, #20337, #81326, #12821, #43807, #67817, #36321, #66814, #90795, #98333, #5347, #73813, #52795, #66312, #17282, #85771, #78256, #91790, #32252, #38793, #1797, #85276, #815, #16781, #68802, #84782, #15321, #333, #24290, #92764, #47758, #30777, #47257, #46289, #23311, #40268, #61767, #9772, #9272, #70776, #77758, #30285, #62258, #39782, #91287, #54756, #7810, #23805, #8295, #92283, #38307, #84305, #60787, #62753, #31267, #70280, #54266, #15804, #8776, #93257, #53790, #61281, #24781, #55257, #16291, #22810, #31764, #76778, #53290, #83799, #39293, #69293, #45803, #46771, #77265, #69784, #76294, #1313, #94736, #80718, #57710, #64706, #71262, #57218, #95216, #86258, #26242, #3753, #26723, #79736, #12214, #72704, #2292, #65205, #32748, #78758, #72223, #11233, #19230, #40759, #63735, #94235, #56735, #4240, #18257, #41271, #87715, #2786, #18750, #88210, #63245, #42238, #19718, #42722, #10753, #87227, #34213, #49234, #71746, #49710, #41752, #25766, #80221, #64219, #3252, #33240, #55766, #50207, #33720, #93750, #25283, #56259, #11725, #17771, #86752, #48734, #34709, #95725, #27209, #79240, #48247, #10265, #66192, #82188, #90675, #35706, #14204, #75180, #28202, #5714, #59187, #6203, #50716, #66700, #51206, #36202, #81209, #58698, #73203, #6692, #74183, #29185, #97228, #89202, #51705, #21707, #96726, #12709, #59683, #44685, #28695, #65701, #74693, #20715, #29669, #22201, #13698, #43203, #60178, #81689, #89692, #73693, #52192, #21207, #44183, #52680, #83181, #36706, #5228, #90177, #67196, #58190, #97721, #82687, #37211, #67699, #14705, #98211, #4735, #35198, #96228, #13203, #27707, #88702, #20212, #43696, #7696, #38192, #699, #47138, #61164, #84182, #69660, #45677, #61642, #1678, #45179, #85156, #32131, #85646, #53666, #31152, #46653, #92163, #15691, #16169, #23688, #68679, #8658, #8179, #46176, #76175, #98714, #62630, #76660, #75678, #7192, #83680, #38675, #37695, #207, #30657, #62135, #54151, #77635, #91672, #23191, #77149, #69176, #84661, #93135, #39171, #16664, #9152, #1186, #31645, #92643, #24168, #15195, #54638, #30165, #39670, #70161, #24662, #55132, #68193, #60669, #91167, #22695, #53174, #49976, #73955, #96485, #66450, #65958, #96985, #50466, #73454, #78141, #47646, #87485, #57962, #9651, #70652, #56980, #95988, #40148, #12470, #27957, #12958, #49475, #95487, #5481, #20473, #79984, #88466, #50960, #19968, #80970, #19484, #42974, #4982, #35462, #58450, #19000, #28462, #58956, #88965, #2175, #11486, #81456, #26978, #35954, #43453, #57477, #87972, #32633, #34468, #80482, #63131, #42006 ) ),
 .UNSPECIFIED., .F., .F., .F. ) 
 B_SPLINE_SURFACE_WITH_KNOTS ( ( 2, 2 ),
 ( 3, 2, 2, 2, 2, 2, 2, 2, 2, 2, 2, 2, 2, 2, 2, 2, 2, 2, 2, 2, 2, 2, 2, 2, 2, 2, 2, 2, 2, 2, 2, 2, 2, 2, 2, 2, 2, 2, 2, 2, 2, 2, 2, 2, 2, 2, 2, 2, 2, 2, 2, 2, 2, 2, 2, 2, 2, 2, 2, 2, 2, 2, 2, 2, 2, 2, 2, 2, 2, 2, 2, 2, 2, 2, 2, 2, 2, 2, 2, 2, 2, 2, 2, 2, 2, 2, 2, 2, 2, 2, 2, 2, 2, 2, 2, 2, 2, 2, 2, 2, 2, 2, 2, 2, 2, 2, 2, 2, 2, 2, 2, 2, 2, 2, 2, 2, 2, 2, 2, 2, 2, 2, 2, 2, 2, 2, 2, 2, 2, 2, 2, 2, 2, 2, 2, 2, 2, 2, 2, 2, 2, 2, 2, 2, 2, 2, 2, 2, 2, 2, 2, 2, 2, 2, 2, 2, 2, 2, 2, 2, 2, 2, 3 ),
 ( 0.000000000000000000, 1.000000000000000000 ),
 ( 0.000000000000000000, 0.005952380952380952051, 0.01190476190476190410, 0.01785714285714285615, 0.02380952380952380820, 0.02976190476190476025, 0.03571428571428571230, 0.04166666666666666435, 0.04761904761904761640, 0.05357142857142856845, 0.05952380952380952051, 0.06547619047619047949, 0.07142857142857142461, 0.07738095238095238360, 0.08333333333333332871, 0.08928571428571428770, 0.09523809523809523281, 0.1011904761904761918, 0.1071428571428571369, 0.1130952380952380959, 0.1190476190476190410, 0.1250000000000000000, 0.1309523809523809590, 0.1369047619047619180, 0.1428571428571428492, 0.1488095238095238082, 0.1547619047619047672, 0.1607142857142857262, 0.1666666666666666574, 0.1726190476190476164, 0.1785714285714285754, 0.1845238095238095344, 0.1904761904761904656, 0.1964285714285714246, 0.2023809523809523836, 0.2083333333333333426, 0.2142857142857142738, 0.2202380952380952328, 0.2261904761904761918, 0.2321428571428571508, 0.2380952380952380820, 0.2440476190476190410, 0.2500000000000000000, 0.2559523809523809312, 0.2619047619047619180, 0.2678571428571428492, 0.2738095238095238360, 0.2797619047619047672, 0.2857142857142856984, 0.2916666666666666852, 0.2976190476190476164, 0.3035714285714285476, 0.3095238095238095344, 0.3154761904761904656, 0.3214285714285714524, 0.3273809523809523836, 0.3333333333333333148, 0.3392857142857143016, 0.3452380952380952328, 0.3511904761904761640, 0.3571428571428571508, 0.3630952380952380820, 0.3690476190476190688, 0.3750000000000000000, 0.3809523809523809312, 0.3869047619047619180, 0.3928571428571428492, 0.3988095238095238360, 0.4047619047619047672, 0.4107142857142856984, 0.4166666666666666852, 0.4226190476190476164, 0.4285714285714285476, 0.4345238095238095344, 0.4404761904761904656, 0.4464285714285714524, 0.4523809523809523836, 0.4583333333333333148, 0.4642857142857143016, 0.4702380952380952328, 0.4761904761904761640, 0.4821428571428571508, 0.4880952380952380820, 0.4940476190476190688, 0.5000000000000000000, 0.5059523809523809312, 0.5119047619047618625, 0.5178571428571429047, 0.5238095238095238360, 0.5297619047619047672, 0.5357142857142856984, 0.5416666666666666297, 0.5476190476190476719, 0.5535714285714286031, 0.5595238095238095344, 0.5654761904761904656, 0.5714285714285713969, 0.5773809523809523281, 0.5833333333333333703, 0.5892857142857143016, 0.5952380952380952328, 0.6011904761904761640, 0.6071428571428570953, 0.6130952380952381375, 0.6190476190476190688, 0.6250000000000000000, 0.6309523809523809312, 0.6369047619047618625, 0.6428571428571429047, 0.6488095238095238360, 0.6547619047619047672, 0.6607142857142856984, 0.6666666666666666297, 0.6726190476190476719, 0.6785714285714286031, 0.6845238095238095344, 0.6904761904761904656, 0.6964285714285713969, 0.7023809523809523281, 0.7083333333333333703, 0.7142857142857143016, 0.7202380952380952328, 0.7261904761904761640, 0.7321428571428570953, 0.7380952380952381375, 0.7440476190476190688, 0.7500000000000000000, 0.7559523809523809312, 0.7619047619047618625, 0.7678571428571429047, 0.7738095238095238360, 0.7797619047619047672, 0.7857142857142856984, 0.7916666666666666297, 0.7976190476190476719, 0.8035714285714286031, 0.8095238095238095344, 0.8154761904761904656, 0.8214285714285713969, 0.8273809523809523281, 0.8333333333333333703, 0.8392857142857143016, 0.8452380952380952328, 0.8511904761904761640, 0.8571428571428570953, 0.8630952380952381375, 0.8690476190476190688, 0.8750000000000000000, 0.8809523809523809312, 0.8869047619047618625, 0.8928571428571429047, 0.8988095238095238360, 0.9047619047619047672, 0.9107142857142856984, 0.9166666666666666297, 0.9226190476190476719, 0.9285714285714286031, 0.9345238095238095344, 0.9404761904761904656, 0.9464285714285713969, 0.9523809523809523281, 0.9583333333333333703, 0.9642857142857143016 ),
 .UNSPECIFIED. ) 
 GEOMETRIC_REPRESENTATION_ITEM ( )  RATIONAL_B_SPLINE_SURFACE ( (
 ( 1.000000000000000000, 0.9659258262890683122, 1.000000000000000000, 0.9659258262890683122, 1.000000000000000000, 0.9659258262890683122, 1.000000000000000000, 0.9659258262890683122, 1.000000000000000000, 0.9659258262890683122, 1.000000000000000000, 0.9659258262890683122, 1.000000000000000000, 0.9659258262890683122, 1.000000000000000000, 0.9659258262890683122, 1.000000000000000000, 0.9659258262890683122, 1.000000000000000000, 0.9659258262890683122, 1.000000000000000000, 0.9659258262890683122, 1.000000000000000000, 0.9659258262890683122, 1.000000000000000000, 0.9659258262890683122, 1.000000000000000000, 0.9659258262890683122, 1.000000000000000000, 0.9659258262890683122, 1.000000000000000000, 0.9659258262890683122, 1.000000000000000000, 0.9659258262890683122, 1.000000000000000000, 0.9659258262890683122, 1.000000000000000000, 0.9659258262890683122, 1.000000000000000000, 0.9659258262890683122, 1.000000000000000000, 0.9659258262890683122, 1.000000000000000000, 0.9659258262890683122, 1.000000000000000000, 0.9659258262890683122, 1.000000000000000000, 0.9659258262890683122, 1.000000000000000000, 0.9659258262890683122, 1.000000000000000000, 0.9659258262890683122, 1.000000000000000000, 0.9659258262890683122, 1.000000000000000000, 0.9659258262890683122, 1.000000000000000000, 0.9659258262890683122, 1.000000000000000000, 0.9659258262890683122, 1.000000000000000000, 0.9659258262890683122, 1.000000000000000000, 0.9659258262890683122, 1.000000000000000000, 0.9659258262890683122, 1.000000000000000000, 0.9659258262890683122, 1.000000000000000000, 0.9659258262890683122, 1.000000000000000000, 0.9659258262890683122, 1.000000000000000000, 0.9659258262890683122, 1.000000000000000000, 0.9659258262890683122, 1.000000000000000000, 0.9659258262890683122, 1.000000000000000000, 0.9659258262890683122, 1.000000000000000000, 0.9659258262890683122, 1.000000000000000000, 0.9659258262890683122, 1.000000000000000000, 0.9659258262890683122, 1.000000000000000000, 0.9659258262890683122, 1.000000000000000000, 0.9659258262890683122, 1.000000000000000000, 0.9659258262890683122, 1.000000000000000000, 0.9659258262890683122, 1.000000000000000000, 0.9659258262890683122, 1.000000000000000000, 0.9659258262890683122, 1.000000000000000000, 0.9659258262890683122, 1.000000000000000000, 0.9659258262890683122, 1.000000000000000000, 0.9659258262890683122, 1.000000000000000000, 0.9659258262890683122, 1.000000000000000000, 0.9659258262890683122, 1.000000000000000000, 0.9659258262890683122, 1.000000000000000000, 0.9659258262890683122, 1.000000000000000000, 0.9659258262890683122, 1.000000000000000000, 0.9659258262890683122, 1.000000000000000000, 0.9659258262890683122, 1.000000000000000000, 0.9659258262890683122, 1.000000000000000000, 0.9659258262890683122, 1.000000000000000000, 0.9659258262890683122, 1.000000000000000000, 0.9659258262890683122, 1.000000000000000000, 0.9659258262890683122, 1.000000000000000000, 0.9659258262890683122, 1.000000000000000000, 0.9659258262890683122, 1.000000000000000000, 0.9659258262890683122, 1.000000000000000000, 0.9659258262890683122, 1.000000000000000000, 0.9659258262890683122, 1.000000000000000000, 0.9659258262890683122, 1.000000000000000000, 0.9659258262890683122, 1.000000000000000000, 0.9659258262890683122, 1.000000000000000000, 0.9659258262890683122, 1.000000000000000000, 0.9659258262890683122, 1.000000000000000000, 0.9659258262890683122, 1.000000000000000000, 0.9659258262890683122, 1.000000000000000000, 0.9659258262890683122, 1.000000000000000000, 0.9659258262890683122, 1.000000000000000000, 0.9659258262890683122, 1.000000000000000000, 0.9659258262890683122, 1.000000000000000000, 0.9659258262890683122, 1.000000000000000000, 0.9659258262890683122, 1.000000000000000000, 0.9659258262890683122, 1.000000000000000000, 0.9659258262890683122, 1.000000000000000000, 0.9659258262890683122, 1.000000000000000000, 0.9659258262890683122, 1.000000000000000000, 0.9659258262890683122, 1.000000000000000000, 0.9659258262890683122, 1.000000000000000000, 0.9659258262890683122, 1.000000000000000000, 0.9659258262890683122, 1.000000000000000000, 0.9659258262890683122, 1.000000000000000000, 0.9659258262890683122, 1.000000000000000000, 0.9659258262890683122, 1.000000000000000000, 0.9659258262890683122, 1.000000000000000000, 0.9659258262890683122, 1.000000000000000000, 0.9659258262890683122, 1.000000000000000000, 0.9659258262890683122, 1.000000000000000000, 0.9659258262890683122, 1.000000000000000000, 0.9659258262890683122, 1.000000000000000000, 0.9659258262890683122, 1.000000000000000000, 0.9659258262890683122, 1.000000000000000000, 0.9659258262890683122, 1.000000000000000000, 0.9659258262890683122, 1.000000000000000000, 0.9659258262890683122, 1.000000000000000000, 0.9659258262890683122, 1.000000000000000000, 0.9659258262890683122, 1.000000000000000000, 0.9659258262890683122, 1.000000000000000000, 0.9659258262890683122, 1.000000000000000000, 0.9659258262890683122, 1.000000000000000000, 0.9659258262890683122, 1.000000000000000000, 0.9659258262890683122, 1.000000000000000000, 0.9659258262890683122, 1.000000000000000000, 0.9659258262890683122, 1.000000000000000000, 0.9659258262890683122, 1.000000000000000000, 0.9659258262890683122, 1.000000000000000000, 0.9659258262890683122, 1.000000000000000000, 0.9659258262890683122, 1.000000000000000000, 0.9659258262890683122, 1.000000000000000000, 0.9659258262890683122, 1.000000000000000000, 0.9659258262890683122, 1.000000000000000000, 0.9659258262890683122, 1.000000000000000000, 0.9659258262890683122, 1.000000000000000000, 0.9659258262890683122, 1.000000000000000000, 0.9659258262890683122, 1.000000000000000000, 0.9659258262890683122, 1.000000000000000000, 0.9659258262890683122, 1.000000000000000000, 0.9659258262890683122, 1.000000000000000000, 0.9659258262890683122, 1.000000000000000000, 0.9659258262890683122, 1.000000000000000000, 0.9659258262890683122, 1.000000000000000000, 0.9659258262890683122, 1.000000000000000000, 0.9659258262890683122, 1.000000000000000000, 0.9659258262890683122, 1.000000000000000000, 0.9659258262890683122, 1.000000000000000000, 0.9659258262890683122, 1.000000000000000000, 0.9659258262890683122, 1.000000000000000000, 0.9659258262890683122, 1.000000000000000000, 0.9659258262890683122, 1.000000000000000000, 0.9659258262890683122, 1.000000000000000000, 0.9659258262890683122, 1.000000000000000000, 0.9659258262890683122, 1.000000000000000000, 0.9659258262890683122, 1.000000000000000000, 0.9659258262890683122, 1.000000000000000000, 0.9659258262890683122, 1.000000000000000000, 0.9659258262890683122, 1.000000000000000000, 0.9659258262890683122, 1.000000000000000000, 0.9659258262890683122, 1.000000000000000000, 0.9659258262890683122, 1.000000000000000000, 0.9659258262890683122, 1.000000000000000000, 0.9659258262890683122, 1.000000000000000000, 0.9659258262890683122, 1.000000000000000000, 0.9659258262890683122, 1.000000000000000000, 0.9659258262890683122, 1.000000000000000000, 0.9659258262890683122, 1.000000000000000000, 0.9659258262890683122, 1.000000000000000000, 0.9659258262890683122, 1.000000000000000000, 0.9659258262890683122, 1.000000000000000000, 0.9659258262890683122, 1.000000000000000000, 0.9659258262890683122, 1.000000000000000000, 0.9659258262890683122, 1.000000000000000000, 0.9659258262890683122, 1.000000000000000000, 0.9659258262890683122, 1.000000000000000000),
 ( 1.000000000000000000, 0.9659258262890683122, 1.000000000000000000, 0.9659258262890683122, 1.000000000000000000, 0.9659258262890683122, 1.000000000000000000, 0.9659258262890683122, 1.000000000000000000, 0.9659258262890683122, 1.000000000000000000, 0.9659258262890683122, 1.000000000000000000, 0.9659258262890683122, 1.000000000000000000, 0.9659258262890683122, 1.000000000000000000, 0.9659258262890683122, 1.000000000000000000, 0.9659258262890683122, 1.000000000000000000, 0.9659258262890683122, 1.000000000000000000, 0.9659258262890683122, 1.000000000000000000, 0.9659258262890683122, 1.000000000000000000, 0.9659258262890683122, 1.000000000000000000, 0.9659258262890683122, 1.000000000000000000, 0.9659258262890683122, 1.000000000000000000, 0.9659258262890683122, 1.000000000000000000, 0.9659258262890683122, 1.000000000000000000, 0.9659258262890683122, 1.000000000000000000, 0.9659258262890683122, 1.000000000000000000, 0.9659258262890683122, 1.000000000000000000, 0.9659258262890683122, 1.000000000000000000, 0.9659258262890683122, 1.000000000000000000, 0.9659258262890683122, 1.000000000000000000, 0.9659258262890683122, 1.000000000000000000, 0.9659258262890683122, 1.000000000000000000, 0.9659258262890683122, 1.000000000000000000, 0.9659258262890683122, 1.000000000000000000, 0.9659258262890683122, 1.000000000000000000, 0.9659258262890683122, 1.000000000000000000, 0.9659258262890683122, 1.000000000000000000, 0.9659258262890683122, 1.000000000000000000, 0.9659258262890683122, 1.000000000000000000, 0.9659258262890683122, 1.000000000000000000, 0.9659258262890683122, 1.000000000000000000, 0.9659258262890683122, 1.000000000000000000, 0.9659258262890683122, 1.000000000000000000, 0.9659258262890683122, 1.000000000000000000, 0.9659258262890683122, 1.000000000000000000, 0.9659258262890683122, 1.000000000000000000, 0.9659258262890683122, 1.000000000000000000, 0.9659258262890683122, 1.000000000000000000, 0.9659258262890683122, 1.000000000000000000, 0.9659258262890683122, 1.000000000000000000, 0.9659258262890683122, 1.000000000000000000, 0.9659258262890683122, 1.000000000000000000, 0.9659258262890683122, 1.000000000000000000, 0.9659258262890683122, 1.000000000000000000, 0.9659258262890683122, 1.000000000000000000, 0.9659258262890683122, 1.000000000000000000, 0.9659258262890683122, 1.000000000000000000, 0.9659258262890683122, 1.000000000000000000, 0.9659258262890683122, 1.000000000000000000, 0.9659258262890683122, 1.000000000000000000, 0.9659258262890683122, 1.000000000000000000, 0.9659258262890683122, 1.000000000000000000, 0.9659258262890683122, 1.000000000000000000, 0.9659258262890683122, 1.000000000000000000, 0.9659258262890683122, 1.000000000000000000, 0.9659258262890683122, 1.000000000000000000, 0.9659258262890683122, 1.000000000000000000, 0.9659258262890683122, 1.000000000000000000, 0.9659258262890683122, 1.000000000000000000, 0.9659258262890683122, 1.000000000000000000, 0.9659258262890683122, 1.000000000000000000, 0.9659258262890683122, 1.000000000000000000, 0.9659258262890683122, 1.000000000000000000, 0.9659258262890683122, 1.000000000000000000, 0.9659258262890683122, 1.000000000000000000, 0.9659258262890683122, 1.000000000000000000, 0.9659258262890683122, 1.000000000000000000, 0.9659258262890683122, 1.000000000000000000, 0.9659258262890683122, 1.000000000000000000, 0.9659258262890683122, 1.000000000000000000, 0.9659258262890683122, 1.000000000000000000, 0.9659258262890683122, 1.000000000000000000, 0.9659258262890683122, 1.000000000000000000, 0.9659258262890683122, 1.000000000000000000, 0.9659258262890683122, 1.000000000000000000, 0.9659258262890683122, 1.000000000000000000, 0.9659258262890683122, 1.000000000000000000, 0.9659258262890683122, 1.000000000000000000, 0.9659258262890683122, 1.000000000000000000, 0.9659258262890683122, 1.000000000000000000, 0.9659258262890683122, 1.000000000000000000, 0.9659258262890683122, 1.000000000000000000, 0.9659258262890683122, 1.000000000000000000, 0.9659258262890683122, 1.000000000000000000, 0.9659258262890683122, 1.000000000000000000, 0.9659258262890683122, 1.000000000000000000, 0.9659258262890683122, 1.000000000000000000, 0.9659258262890683122, 1.000000000000000000, 0.9659258262890683122, 1.000000000000000000, 0.9659258262890683122, 1.000000000000000000, 0.9659258262890683122, 1.000000000000000000, 0.9659258262890683122, 1.000000000000000000, 0.9659258262890683122, 1.000000000000000000, 0.9659258262890683122, 1.000000000000000000, 0.9659258262890683122, 1.000000000000000000, 0.9659258262890683122, 1.000000000000000000, 0.9659258262890683122, 1.000000000000000000, 0.9659258262890683122, 1.000000000000000000, 0.9659258262890683122, 1.000000000000000000, 0.9659258262890683122, 1.000000000000000000, 0.9659258262890683122, 1.000000000000000000, 0.9659258262890683122, 1.000000000000000000, 0.9659258262890683122, 1.000000000000000000, 0.9659258262890683122, 1.000000000000000000, 0.9659258262890683122, 1.000000000000000000, 0.9659258262890683122, 1.000000000000000000, 0.9659258262890683122, 1.000000000000000000, 0.9659258262890683122, 1.000000000000000000, 0.9659258262890683122, 1.000000000000000000, 0.9659258262890683122, 1.000000000000000000, 0.9659258262890683122, 1.000000000000000000, 0.9659258262890683122, 1.000000000000000000, 0.9659258262890683122, 1.000000000000000000, 0.9659258262890683122, 1.000000000000000000, 0.9659258262890683122, 1.000000000000000000, 0.9659258262890683122, 1.000000000000000000, 0.9659258262890683122, 1.000000000000000000, 0.9659258262890683122, 1.000000000000000000, 0.9659258262890683122, 1.000000000000000000, 0.9659258262890683122, 1.000000000000000000, 0.9659258262890683122, 1.000000000000000000, 0.9659258262890683122, 1.000000000000000000, 0.9659258262890683122, 1.000000000000000000, 0.9659258262890683122, 1.000000000000000000, 0.9659258262890683122, 1.000000000000000000, 0.9659258262890683122, 1.000000000000000000, 0.9659258262890683122, 1.000000000000000000, 0.9659258262890683122, 1.000000000000000000, 0.9659258262890683122, 1.000000000000000000, 0.9659258262890683122, 1.000000000000000000, 0.9659258262890683122, 1.000000000000000000, 0.9659258262890683122, 1.000000000000000000, 0.9659258262890683122, 1.000000000000000000, 0.9659258262890683122, 1.000000000000000000, 0.9659258262890683122, 1.000000000000000000, 0.9659258262890683122, 1.000000000000000000, 0.9659258262890683122, 1.000000000000000000, 0.9659258262890683122, 1.000000000000000000, 0.9659258262890683122, 1.000000000000000000, 0.9659258262890683122, 1.000000000000000000, 0.9659258262890683122, 1.000000000000000000, 0.9659258262890683122, 1.000000000000000000, 0.9659258262890683122, 1.000000000000000000, 0.9659258262890683122, 1.000000000000000000, 0.9659258262890683122, 1.000000000000000000, 0.9659258262890683122, 1.000000000000000000, 0.9659258262890683122, 1.000000000000000000, 0.9659258262890683122, 1.000000000000000000, 0.9659258262890683122, 1.000000000000000000, 0.9659258262890683122, 1.000000000000000000, 0.9659258262890683122, 1.000000000000000000, 0.9659258262890683122, 1.000000000000000000, 0.9659258262890683122, 1.000000000000000000, 0.9659258262890683122, 1.000000000000000000, 0.9659258262890683122, 1.000000000000000000, 0.9659258262890683122, 1.000000000000000000, 0.9659258262890683122, 1.000000000000000000, 0.9659258262890683122, 1.000000000000000000) ) ) 
 REPRESENTATION_ITEM ( '' )  SURFACE ( )  );
#12277 = CARTESIAN_POINT ( 'NONE',  ( 16.40814093676323893, 60.79030133659709634, 11.09922568453595026 ) ) ;
#12278 = CARTESIAN_POINT ( 'NONE',  ( 21.09922568453595559, 27.04030133659708568, -6.408140936763230044 ) ) ;
#12279 = CARTESIAN_POINT ( 'NONE',  ( 17.20831665107776587, 27.88393115100078390, 7.208316651077764980 ) ) ;
#12280 = ORIENTED_EDGE ( 'NONE', *, *, #46018, .F. ) ;
#12281 = CARTESIAN_POINT ( 'NONE',  ( 8.673617379884035472E-16, 78.91966277462714174, 5.000000000000000000 ) ) ;
#12282 = CARTESIAN_POINT ( 'NONE',  ( -11.29168986245485051, 0.2301502372707046606, -9.783658503027551134 ) ) ;
#12283 = CARTESIAN_POINT ( 'NONE',  ( 17.08211943468705840, 65.13708216824730357, -12.26659068614894466 ) ) ;
#12284 = CARTESIAN_POINT ( 'NONE',  ( 15.44008868035555260, 19.73035201082150536, 9.422509992056143702 ) ) ;
#12285 = CARTESIAN_POINT ( 'NONE',  ( 20.36894250292379738, 44.92874883491396787, -10.36894250292379027 ) ) ;
#12286 = CARTESIAN_POINT ( 'NONE',  ( 19.42250999205614193, 35.14701867748816966, 5.440088680355555262 ) ) ;
#12287 = CARTESIAN_POINT ( 'NONE',  ( -0.8801773607111009756, 58.06368534415484106, 1.068504757029289695E-15 ) ) ;
#12288 = DIRECTION ( 'NONE',  ( 0.000000000000000000, 0.000000000000000000, 1.000000000000000000 ) ) ;
#12289 = CARTESIAN_POINT ( 'NONE',  ( 19.84674366389459266, 13.30059781766745353, 2.638427012816836559 ) ) ;
#12290 = CARTESIAN_POINT ( 'NONE',  ( 6.284583270191197002, -88.40194713205143273, -4.000000000000000000 ) ) ;
#12291 = CARTESIAN_POINT ( 'NONE',  ( 18.52753015748617571, 13.09226448433411960, 4.923371831947298993 ) ) ;
#12292 = DIRECTION ( 'NONE',  ( 0.000000000000000000, -1.000000000000000000, 0.000000000000000000 ) ) ;
#12293 = CARTESIAN_POINT ( 'NONE',  ( 0.1532563361054083140, 41.00893115100078745, 1.131784320476157264E-15 ) ) ;
#12294 = CARTESIAN_POINT ( 'NONE',  ( 1.472469842513823179, 60.59226448433412315, -4.923371831947296329 ) ) ;
#12295 = ADVANCED_FACE ( 'NONE', ( #89675 ), #30141, .F. ) ;
#12296 = UNCERTAINTY_MEASURE_WITH_UNIT (LENGTH_MEASURE( 1.000000000000000082E-05 ), #72569, 'distance_accuracy_value', 'NONE');
#12297 = ORIENTED_EDGE ( 'NONE', *, *, #61201, .F. ) ;
#12298 = CARTESIAN_POINT ( 'NONE',  ( 3.591859063236763294, 43.29030133659708923, -11.09922568453595026 ) ) ;
#12299 = LINE ( 'NONE', #66785, #92326 ) ;
#12300 = CARTESIAN_POINT ( 'NONE',  ( 20.88017736071110875, 65.77201867748817676, -2.915334737309920765 ) ) ;
#12301 = CARTESIAN_POINT ( 'NONE',  ( 3.591859063236761518, 44.95696800326376064, 11.09922568453594849 ) ) ;
#12303 = CARTESIAN_POINT ( 'NONE',  ( 2.791683348922240793, 41.63393115100078745, 7.208316651077764092 ) ) ;
#12302 = CARTESIAN_POINT ( 'NONE',  ( -0.3689425029237881626, 62.42874883491396787, 10.36894250292379027 ) ) ;
#12304 = CARTESIAN_POINT ( 'NONE',  ( 5.129999999999995453, 43.00000000000000711, -6.250000000000000000 ) ) ;
#12305 = TOROIDAL_SURFACE ( 'NONE', #69777, 14.49999999999999822, 0.5000000000000000000 ) ;
#12306 = CARTESIAN_POINT ( 'NONE',  ( 7.361572987183169658, 64.96726448433412315, -9.846743663894592657 ) ) ;
#12307 = CARTESIAN_POINT ( 'NONE',  ( -4.164238869374099039, 26.80374883491397142, 8.674139862899312516E-16 ) ) ;
#12308 = CARTESIAN_POINT ( 'NONE',  ( 10.00000000000000178, 37.25893115100078745, 9.846743663894594434 ) ) ;
#12309 = DIRECTION ( 'NONE',  ( 0.000000000000000000, 0.000000000000000000, 1.000000000000000000 ) ) ;
#12310 = CARTESIAN_POINT ( 'NONE',  ( 17.96484262340118221, 39.93868534415484106, 7.964842623401181321 ) ) ;
#12311 = CARTESIAN_POINT ( 'NONE',  ( 4.559911319644449179, 57.23035201082150536, -9.422509992056141925 ) ) ;
#12312 = COLOUR_RGB ( '', 0.31764706, 0.68627451, 0.89019608) ;
#12313 = DIRECTION ( 'NONE',  ( 0.000000000000000000, 0.000000000000000000, 1.000000000000000000 ) ) ;
#12314 = ORIENTED_EDGE ( 'NONE', *, *, #53053, .T. ) ;
#12315 = CARTESIAN_POINT ( 'NONE',  ( 3.591859063236761518, 39.95696800326375353, 11.09922568453594849 ) ) ;
#12316 = VECTOR ( 'NONE', #71434, 1000.000000000000000 ) ;
#12317 = CARTESIAN_POINT ( 'NONE',  ( 4.559911319644449179, 47.23035201082150536, -9.422509992056141925 ) ) ;
#12318 = ORIENTED_EDGE ( 'NONE', *, *, #40561, .T. ) ;
#12319 = DIRECTION ( 'NONE',  ( 0.000000000000000000, 0.000000000000000000, -1.000000000000000000 ) ) ;
#12320 = CIRCLE ( 'NONE', #17125, 2.250000000000001332 ) ;
#12321 = DIRECTION ( 'NONE',  ( 0.8038568606172163955, 0.000000000000000000, 0.5948227867513425915 ) ) ;
#12322 = ORIENTED_EDGE ( 'NONE', *, *, #2179, .T. ) ;
#12323 = AXIS2_PLACEMENT_3D ( 'NONE', #5178, #35663, #60625 ) ;
#12324 = CARTESIAN_POINT ( 'NONE',  ( -3.749999999999999112, 78.07179676972445748, 4.250000000000000000 ) ) ;
#12325 = CARTESIAN_POINT ( 'NONE',  ( 20.88017736071110164, 15.35535201082150358, 2.915334737309930979 ) ) ;
#12326 = EDGE_CURVE ( 'NONE', #54753, #75561, #6045, .T. ) ;
#12327 = CARTESIAN_POINT ( 'NONE',  ( -8.731067818237040257, 12.03712336850782094, -8.731067818237033151 ) ) ;
#12328 = CARTESIAN_POINT ( 'NONE',  ( 6.204703633549690345, 67.84541550158060375, 14.16423886937410082 ) ) ;
#12329 = CARTESIAN_POINT ( 'NONE',  ( 6.204703633549690345, 20.76208216824730357, -14.16423886937410259 ) ) ;
#12330 = EDGE_CURVE ( 'NONE', #71973, #36998, #50715, .T. ) ;
#12331 = CARTESIAN_POINT ( 'NONE',  ( 15.44008868035555793, 21.39701867748817321, -9.422509992056140149 ) ) ;
#12332 = CARTESIAN_POINT ( 'NONE',  ( 5.076628168052703671, 61.84226448433412315, 8.527530157486179263 ) ) ;
#12333 = ORIENTED_EDGE ( 'NONE', *, *, #69416, .F. ) ;
#12334 = CARTESIAN_POINT ( 'NONE',  ( 18.52753015748618282, 63.92559781766745886, -4.923371831947291888 ) ) ;
#12335 = EDGE_LOOP ( 'NONE', ( #6302, #79950, #17675, #81704, #27044, #80866 ) ) ;
#12336 = CARTESIAN_POINT ( 'NONE',  ( 4.559911319644449179, 58.89701867748817676, 9.422509992056141925 ) ) ;
#12337 = CARTESIAN_POINT ( 'NONE',  ( 1.472469842513823179, 61.42559781766745175, 4.923371831947296329 ) ) ;
#12339 = DIRECTION ( 'NONE',  ( -0.000000000000000000, -0.000000000000000000, -1.000000000000000000 ) ) ;
#12338 = CARTESIAN_POINT ( 'NONE',  ( 12.91533473730993009, 6.605352010821504471, -10.88017736071109987 ) ) ;
#12340 = CARTESIAN_POINT ( 'NONE',  ( 17.96484262340118221, 66.18868534415483396, -7.964842623401177768 ) ) ;
#12341 = CARTESIAN_POINT ( 'NONE',  ( 0.5774900079438590739, 12.64701867748817321, -5.440088680355550821 ) ) ;
#12342 = CARTESIAN_POINT ( 'NONE',  ( 6.565887622018943937, 53.08196800326374643, -12.81628187352647608 ) ) ;
#12343 = CARTESIAN_POINT ( 'NONE',  ( 4.559911319644449179, 28.89701867748817321, 9.422509992056141925 ) ) ;
#12344 = CARTESIAN_POINT ( 'NONE',  ( -14.89999999999999680, 98.49999999999998579, 8.000000000000000000 ) ) ;
#12345 = CARTESIAN_POINT ( 'NONE',  ( 19.38216949554541202, 45.99863466993041072, 9.382169495545424454 ) ) ;
#12346 = CARTESIAN_POINT ( 'NONE',  ( 2.035157376598822676, 52.43868534415483396, -7.964842623401177768 ) ) ;
#12347 = VECTOR ( 'NONE', #48811, 1000.000000000000114 ) ;
#12348 = CARTESIAN_POINT ( 'NONE',  ( 5.076628168052703671, 61.84226448433412315, 8.527530157486179263 ) ) ;
#12349 = ORIENTED_EDGE ( 'NONE', *, *, #69083, .T. ) ;
#12350 = CARTESIAN_POINT ( 'NONE',  ( 14.02068044289375415, 0.5000000000000004441, 5.331089937175756965 ) ) ;
#12351 = CARTESIAN_POINT ( 'NONE',  ( 10.00000000000000000, -2.126365330069579951, -12.81628187352647608 ) ) ;
#12353 = CARTESIAN_POINT ( 'NONE',  ( 12.63842701281683034, 47.46726448433412315, 9.846743663894596210 ) ) ;
#12352 = DIRECTION ( 'NONE',  ( 0.000000000000000000, -1.000000000000000000, 0.000000000000000000 ) ) ;
#12354 = CARTESIAN_POINT ( 'NONE',  ( 17.96484262340118221, 21.18868534415483396, -7.964842623401177768 ) ) ;
#12355 = CARTESIAN_POINT ( 'NONE',  ( 0.000000000000000000, 0.000000000000000000, 0.000000000000000000 ) ) ;
#12356 = CARTESIAN_POINT ( 'NONE',  ( 14.92337183194729633, 42.67559781766745886, 8.527530157486181039 ) ) ;
#12357 = CARTESIAN_POINT ( 'NONE',  ( -14.04391541078767958, 4.832815575535569023E-16, 3.608107528142744602 ) ) ;
#12358 = PRESENTATION_STYLE_ASSIGNMENT (( #67333 ) ) ;
#12359 = EDGE_CURVE ( 'NONE', #28561, #80817, #66634, .T. ) ;
#12361 = CARTESIAN_POINT ( 'NONE',  ( 1.472469842513823179, 5.592264484334118713, -4.923371831947296329 ) ) ;
#12360 = CARTESIAN_POINT ( 'NONE',  ( 7.361572987183169658, 44.96726448433412315, -9.846743663894592657 ) ) ;
#12362 = DIRECTION ( 'NONE',  ( -0.1822355254921514123, 0.000000000000000000, 0.9832549075639539504 ) ) ;
#12364 = ORIENTED_EDGE ( 'NONE', *, *, #86264, .T. ) ;
#12363 = CARTESIAN_POINT ( 'NONE',  ( 18.52753015748618282, 58.92559781766745886, -4.923371831947291888 ) ) ;
#12365 = CARTESIAN_POINT ( 'NONE',  ( 7.313705784284509903, 14.63595249122788999, 13.09617149020749061 ) ) ;
#12366 = CARTESIAN_POINT ( 'NONE',  ( 22.81628187352647785, 41.41530133659708923, 3.434112377981063169 ) ) ;
#12367 = CARTESIAN_POINT ( 'NONE',  ( 18.52753015748618282, 43.92559781766745175, -4.923371831947291888 ) ) ;
#12368 = LINE ( 'NONE', #95887, #40938 ) ;
#12369 = CARTESIAN_POINT ( 'NONE',  ( 13.79529636645030344, 53.26208216824730357, 14.16423886937410614 ) ) ;
#12370 = CARTESIAN_POINT ( 'NONE',  ( 7.361572987183170547, 32.05059781766745175, 9.846743663894590881 ) ) ;
#12371 = CARTESIAN_POINT ( 'NONE',  ( 20.00000000000000711, 87.41133749856676616, 4.971011742375448073 ) ) ;
#12372 = CARTESIAN_POINT ( 'NONE',  ( 20.36894250292379738, 59.92874883491397497, -10.36894250292379027 ) ) ;
#12373 = CARTESIAN_POINT ( 'NONE',  ( 7.674241358950872005, 0.2301500950314220029, -12.81905807005885123 ) ) ;
#12374 = CARTESIAN_POINT ( 'NONE',  ( 19.42250999205614193, 15.14701867748817143, 5.440088680355555262 ) ) ;
#12376 = AXIS2_PLACEMENT_3D ( 'NONE', #47625, #85629, #17146 ) ;
#12375 = CARTESIAN_POINT ( 'NONE',  ( 2.917880565312950480, 30.97041550158063572, -12.26659068614894821 ) ) ;
#12378 = CARTESIAN_POINT ( 'NONE',  ( 7.850000000000003197, 98.50000000000000000, -8.000000000000000000 ) ) ;
#12377 = CARTESIAN_POINT ( 'NONE',  ( 22.26659068614894466, 48.88708216824730357, 7.082119434687054849 ) ) ;
#12379 = CARTESIAN_POINT ( 'NONE',  ( 7.674241358951006120, 14.76984990496591621, 12.81905807006024922 ) ) ;
#12380 = CARTESIAN_POINT ( 'NONE',  ( 10.00000000000000000, 14.75893115100078568, -9.846743663894594434 ) ) ;
#12381 = CARTESIAN_POINT ( 'NONE',  ( 0.1532563361054100626, 65.80059781766745175, -2.638427012816831230 ) ) ;
#12382 = EDGE_LOOP ( 'NONE', ( #5896, #26599, #22069, #58151, #28062, #90487 ) ) ;
#12383 = CARTESIAN_POINT ( 'NONE',  ( 15.44008868035555260, 49.73035201082150536, 9.422509992056143702 ) ) ;
#12384 = CARTESIAN_POINT ( 'NONE',  ( 0.2751277870542874204, 39.36607318730131055, -6.499999999999984901 ) ) ;
#12386 = CARTESIAN_POINT ( 'NONE',  ( -7.313705784284419309, 15.00000000000000000, -13.09617149020753502 ) ) ;
#12385 = CIRCLE ( 'NONE', #20325, 14.49999999999999822 ) ;
#12387 = AXIS2_PLACEMENT_3D ( 'NONE', #91998, #77479, #83523 ) ;
#12388 = CARTESIAN_POINT ( 'NONE',  ( 0.1532563361054100626, 60.80059781766744464, -2.638427012816831230 ) ) ;
#12389 = SURFACE_SIDE_STYLE ('',( #34884 ) ) ;
#12390 = ORIENTED_EDGE ( 'NONE', *, *, #55445, .T. ) ;
#12391 = CARTESIAN_POINT ( 'NONE',  ( 10.00000000000000178, 23.05374883491397142, 14.16423886937410082 ) ) ;
#12392 = DIRECTION ( 'NONE',  ( 0.000000000000000000, 0.000000000000000000, 1.000000000000000000 ) ) ;
#12393 = CARTESIAN_POINT ( 'NONE',  ( -7.072497013479695838, -84.40007040885043921, -2.500000000001209255 ) ) ;
#12394 = CARTESIAN_POINT ( 'NONE',  ( 12.91533473730992121, 19.52201867748816611, 10.88017736071110164 ) ) ;
#12395 = CARTESIAN_POINT ( 'NONE',  ( -2.816281873526473856, 39.12363466993041783, 9.499525473075851096E-16 ) ) ;
#12396 = CARTESIAN_POINT ( 'NONE',  ( -7.313705784284471711, 14.49999999999999112, -13.09617149020757942 ) ) ;
#12397 = CARTESIAN_POINT ( 'NONE',  ( 64.56412365047461321, 11.99999999999999467, 9.500000000000000000 ) ) ;
#12398 = ORIENTED_EDGE ( 'NONE', *, *, #62351, .F. ) ;
#12399 = DIRECTION ( 'NONE',  ( 0.000000000000000000, 1.000000000000000000, 0.000000000000000000 ) ) ;
#12400 = CARTESIAN_POINT ( 'NONE',  ( 20.36894250292379382, 23.67874883491397142, 10.36894250292379205 ) ) ;
#12401 = CARTESIAN_POINT ( 'NONE',  ( 24.16423886937410614, 4.303748834913967869, 8.672049930838204340E-16 ) ) ;
#12402 = CARTESIAN_POINT ( 'NONE',  ( -6.060849023604186314, -36.09672517615243237, 3.999999999999999112 ) ) ;
#12403 = CARTESIAN_POINT ( 'NONE',  ( 0.5774900079438590739, 22.64701867748817321, -5.440088680355550821 ) ) ;
#12404 = CYLINDRICAL_SURFACE ( 'NONE', #84565, 6.999999999999995559 ) ;
#12405 = CARTESIAN_POINT ( 'NONE',  ( 0.000000000000000000, 14.49999999999999822, 0.000000000000000000 ) ) ;
#12406 = CARTESIAN_POINT ( 'NONE',  ( 7.084665262690076126, 39.10535201082150536, 10.88017736071109987 ) ) ;
#12407 = CARTESIAN_POINT ( 'NONE',  ( 17.96484262340118221, 56.18868534415484817, -7.964842623401177768 ) ) ;
#12408 = CARTESIAN_POINT ( 'NONE',  ( -2.816281873526473856, 9.123634669930421381, 9.499525473075851096E-16 ) ) ;
#12409 = LINE ( 'NONE', #48928, #17082 ) ;
#12410 = CARTESIAN_POINT ( 'NONE',  ( 0.8952175423693563561, 2.601608292538878597, -5.990408912944101161 ) ) ;
#12411 = CARTESIAN_POINT ( 'NONE',  ( 14.92337183194729633, 17.67559781766745175, 8.527530157486181039 ) ) ;
#12412 = CARTESIAN_POINT ( 'NONE',  ( 2.035157376598824452, 38.68868534415483396, 7.964842623401179544 ) ) ;
#12413 = EDGE_CURVE ( 'NONE', #37066, #85540, #5697, .T. ) ;
#12414 = B_SPLINE_CURVE_WITH_KNOTS ( 'NONE', 3,
 ( #87070, #34537, #10584, #96057, #28034, #80557 ),
 .UNSPECIFIED., .F., .F.,
 ( 4, 2, 4 ),
 ( 0.000000000000000000, 0.0002626113303184835542, 0.0005252226606369671084 ),
 .UNSPECIFIED. ) ;
#12415 = CARTESIAN_POINT ( 'NONE',  ( 19.38216949554541557, 7.248634669930421381, -9.382169495545420901 ) ) ;
#12416 = CARTESIAN_POINT ( 'NONE',  ( 17.96484262340118221, 61.18868534415482685, -7.964842623401177768 ) ) ;
#12417 = CARTESIAN_POINT ( 'NONE',  ( 19.84674366389459266, 23.71726448433412315, -2.638427012816827677 ) ) ;
#12418 = CARTESIAN_POINT ( 'NONE',  ( 16.40814093676324603, 42.45696800326375353, -11.09922568453594671 ) ) ;
#12419 = CARTESIAN_POINT ( 'NONE',  ( 5.076628168052704559, 0.1755978176674514724, -8.527530157486179263 ) ) ;
#12420 = EDGE_LOOP ( 'NONE', ( #10024, #12398, #12820, #46629 ) ) ;
#12421 = CARTESIAN_POINT ( 'NONE',  ( 2.550000000000003819, 99.99999999999998579, -8.000000000000000000 ) ) ;
#12422 = DIRECTION ( 'NONE',  ( 0.000000000000000000, 0.000000000000000000, -1.000000000000000000 ) ) ;
#12423 = CARTESIAN_POINT ( 'NONE',  ( 17.96484262340118221, 19.93868534415484106, 7.964842623401181321 ) ) ;
#12425 = CARTESIAN_POINT ( 'NONE',  ( 6.204703633549690345, 20.76208216824730357, -14.16423886937410259 ) ) ;
#12424 = CARTESIAN_POINT ( 'NONE',  ( 22.81628187352647785, 61.62363466993041783, 6.195893100308588602E-16 ) ) ;
#12426 = CARTESIAN_POINT ( 'NONE',  ( 7.361572987183169658, 29.96726448433411960, -9.846743663894592657 ) ) ;
#12427 = CARTESIAN_POINT ( 'NONE',  ( 15.44008868035555260, 14.73035201082150536, 9.422509992056143702 ) ) ;
#12428 = CARTESIAN_POINT ( 'NONE',  ( 4.559911319644449179, 2.230352010821504916, -9.422509992056141925 ) ) ;
#12429 = ORIENTED_EDGE ( 'NONE', *, *, #12204, .F. ) ;
#12430 = CARTESIAN_POINT ( 'NONE',  ( 0.5774900079438590739, 17.64701867748817321, -5.440088680355550821 ) ) ;
#12431 = CARTESIAN_POINT ( 'NONE',  ( 15.44008868035555260, 34.73035201082151247, 9.422509992056143702 ) ) ;
#12433 = CARTESIAN_POINT ( 'NONE',  ( 4.559911319644449179, 42.23035201082151247, -9.422509992056141925 ) ) ;
#12432 = CARTESIAN_POINT ( 'NONE',  ( -12.34597252984343640, 14.95037103437615755, 8.076773567935736864 ) ) ;
#12434 =( GEOMETRIC_REPRESENTATION_CONTEXT ( 3 ) GLOBAL_UNCERTAINTY_ASSIGNED_CONTEXT ( ( #1252 ) ) GLOBAL_UNIT_ASSIGNED_CONTEXT ( ( #79189, #56685, #42669 ) ) REPRESENTATION_CONTEXT ( 'NONE', 'WORKASPACE' ) );
#12435 = ORIENTED_EDGE ( 'NONE', *, *, #36367, .T. ) ;
#12436 = CARTESIAN_POINT ( 'NONE',  ( 19.84674366389459266, 63.71726448433412315, -2.638427012816827677 ) ) ;
#12437 = CARTESIAN_POINT ( 'NONE',  ( 19.42250999205614193, 30.14701867748817321, 5.440088680355555262 ) ) ;
#12438 = CARTESIAN_POINT ( 'NONE',  ( 0.1532563361054082862, 66.21726448433413736, 2.638427012816831674 ) ) ;
#12439 = DIRECTION ( 'NONE',  ( 1.257568779154408793E-17, 1.000000000000000000, -0.000000000000000000 ) ) ;
#12440 = ADVANCED_FACE ( 'NONE', ( #37190 ), #52658, .T. ) ;
#12441 = CARTESIAN_POINT ( 'NONE',  ( 22.81628187352647785, 56.62363466993042493, 6.195893100308588602E-16 ) ) ;
#12442 = CARTESIAN_POINT ( 'NONE',  ( 20.10421743870886147, 30.60736173766201773, -6.337391062633416006 ) ) ;
#12443 = CARTESIAN_POINT ( 'NONE',  ( 17.08211943468705130, 33.47041550158063927, 12.26659068614894998 ) ) ;
#12444 = CARTESIAN_POINT ( 'NONE',  ( 15.44008868035555260, 49.73035201082150536, 9.422509992056143702 ) ) ;
#12445 = CARTESIAN_POINT ( 'NONE',  ( 15.44008868035555793, 36.39701867748816966, -9.422509992056140149 ) ) ;
#12446 = CARTESIAN_POINT ( 'NONE',  ( 5.076628168052703671, 66.84226448433412315, 8.527530157486179263 ) ) ;
#12447 = DIRECTION ( 'NONE',  ( 1.000000000000000000, 0.000000000000000000, -0.000000000000000000 ) ) ;
#12448 = CARTESIAN_POINT ( 'NONE',  ( 19.84674366389459266, 43.71726448433410894, -2.638427012816827677 ) ) ;
#12449 = EDGE_CURVE ( 'NONE', #61453, #8076, #14685, .T. ) ;
#12450 = ORIENTED_EDGE ( 'NONE', *, *, #13305, .F. ) ;
#12451 = CARTESIAN_POINT ( 'NONE',  ( 7.347880794884118750E-16, 17.03999999999999915, 0.000000000000000000 ) ) ;
#12452 = CARTESIAN_POINT ( 'NONE',  ( 2.791683348922240793, 21.63393115100078745, 7.208316651077764092 ) ) ;
#12453 = CARTESIAN_POINT ( 'NONE',  ( -9.382169495545422677, -26.50136533006957151, -9.382169495545417348 ) ) ;
#12454 = AXIS2_PLACEMENT_3D ( 'NONE', #443, #44909, #83908 ) ;
#12455 = CARTESIAN_POINT ( 'NONE',  ( 7.084665262690076126, 12.02201867748817143, -10.88017736071110164 ) ) ;
#12456 = CARTESIAN_POINT ( 'NONE',  ( 10.00000000000000000, 29.75893115100078745, -9.846743663894594434 ) ) ;
#12457 = CARTESIAN_POINT ( 'NONE',  ( 13.43411237798106583, 12.66530133659708746, -12.81628187352647252 ) ) ;
#12459 = CARTESIAN_POINT ( 'NONE',  ( 10.00000000000000000, 51.81368534415484106, -10.88017736071110342 ) ) ;
#12458 = CARTESIAN_POINT ( 'NONE',  ( 0.5774900079438590739, 57.64701867748817676, -5.440088680355550821 ) ) ;
#12461 = CARTESIAN_POINT ( 'NONE',  ( 21.09922568453595559, 52.04030133659708923, -6.408140936763230044 ) ) ;
#12460 = CARTESIAN_POINT ( 'NONE',  ( 19.42250999205614193, 25.14701867748817321, 5.440088680355555262 ) ) ;
#12462 = CARTESIAN_POINT ( 'NONE',  ( 6.204703633549690345, 32.84541550158063927, 14.16423886937410082 ) ) ;
#12463 = AXIS2_PLACEMENT_3D ( 'NONE', #70588, #64042, #25104 ) ;
#12464 = AXIS2_PLACEMENT_3D ( 'NONE', #11705, #48713, #57690 ) ;
#12465 = CARTESIAN_POINT ( 'NONE',  ( 20.24186590665276597, 34.73410085661203084, 6.114288769123062295 ) ) ;
#12466 = ORIENTED_EDGE ( 'NONE', *, *, #54625, .F. ) ;
#12467 = CARTESIAN_POINT ( 'NONE',  ( -1.099225684535947600, -0.4596986634029132657, 6.408140936763237150 ) ) ;
#12468 = CARTESIAN_POINT ( 'NONE',  ( 0.6178305044545838731, 64.74863466993043914, 9.382169495545420901 ) ) ;
#12469 = CARTESIAN_POINT ( 'NONE',  ( 19.42250999205614548, 30.98035201082150536, -5.440088680355545492 ) ) ;
#12470 = CARTESIAN_POINT ( 'NONE',  ( 2.791683348922237240, 60.38393115100078745, -7.208316651077763204 ) ) ;
#12471 = VERTEX_POINT ( 'NONE', #66683 ) ;
#12472 = CARTESIAN_POINT ( 'NONE',  ( 7.361572987183169658, 19.96726448433411960, -9.846743663894592657 ) ) ;
#12473 = CARTESIAN_POINT ( 'NONE',  ( 12.63842701281683034, 7.467264484334118713, 9.846743663894596210 ) ) ;
#12474 = CARTESIAN_POINT ( 'NONE',  ( 0.1532563361054082862, 26.21726448433411605, 2.638427012816831674 ) ) ;
#12475 = CARTESIAN_POINT ( 'NONE',  ( 14.92337183194729988, 14.34226448433411782, -8.527530157486177487 ) ) ;
#12476 = CARTESIAN_POINT ( 'NONE',  ( 7.361572987183169658, -0.03273551566588185635, -9.846743663894592657 ) ) ;
#12477 = CARTESIAN_POINT ( 'NONE',  ( -7.124975165242272368, -78.82169502743931844, 2.750000000000000000 ) ) ;
#12478 = EDGE_CURVE ( 'NONE', #72922, #45554, #3421, .T. ) ;
#12480 = DIRECTION ( 'NONE',  ( -0.09584575252022721481, 0.000000000000000000, 0.9953961983671785196 ) ) ;
#12479 = CARTESIAN_POINT ( 'NONE',  ( 0.1532563361054083140, 1.008931151000784787, 1.131784320476157264E-15 ) ) ;
#12481 = CARTESIAN_POINT ( 'NONE',  ( 2.791683348922237240, 5.383931151000785675, -7.208316651077763204 ) ) ;
#12483 = ORIENTED_EDGE ( 'NONE', *, *, #76081, .T. ) ;
#12482 = CARTESIAN_POINT ( 'NONE',  ( 14.92337183194729988, 24.34226448433411960, -8.527530157486177487 ) ) ;
#12484 = CARTESIAN_POINT ( 'NONE',  ( 5.800000000000003375, 99.99999999999998579, -8.525133428036873795 ) ) ;
#12485 = CARTESIAN_POINT ( 'NONE',  ( 10.00000000000000178, 5.373634669930420493, 12.81628187352647608 ) ) ;
#12486 = ORIENTED_EDGE ( 'NONE', *, *, #21475, .T. ) ;
#12487 = FACE_OUTER_BOUND ( 'NONE', #91149, .T. ) ;
#12488 = CARTESIAN_POINT ( 'NONE',  ( 22.26659068614894466, 18.88708216824730002, 7.082119434687054849 ) ) ;
#12489 = UNCERTAINTY_MEASURE_WITH_UNIT (LENGTH_MEASURE( 1.000000000000000082E-05 ), #17357, 'distance_accuracy_value', 'NONE');
#12490 = DIRECTION ( 'NONE',  ( 1.000000000000000000, 0.000000000000000000, 0.000000000000000000 ) ) ;
#12491 = CARTESIAN_POINT ( 'NONE',  ( -0.3689425029237898834, 21.17874883491396432, -10.36894250292378850 ) ) ;
#12492 = EDGE_CURVE ( 'NONE', #58402, #44777, #18629, .T. ) ;
#12493 = CARTESIAN_POINT ( 'NONE',  ( -4.164238869374099039, 26.80374883491397142, 8.674139862899312516E-16 ) ) ;
#12494 = CARTESIAN_POINT ( 'NONE',  ( 10.00000000000000000, 0.5537488349139675359, -14.16423886937410082 ) ) ;
#12496 = CARTESIAN_POINT ( 'NONE',  ( 4.559911319644449179, 68.89701867748817676, 9.422509992056141925 ) ) ;
#12495 = CARTESIAN_POINT ( 'NONE',  ( 10.00000000000000178, 13.05374883491396787, 14.16423886937410082 ) ) ;
#12497 = CARTESIAN_POINT ( 'NONE',  ( -0.8801773607111008646, 28.27201867748817321, 2.915334737309923430 ) ) ;
#12498 = DIRECTION ( 'NONE',  ( 0.000000000000000000, 1.000000000000000000, 0.000000000000000000 ) ) ;
#12499 = ORIENTED_EDGE ( 'NONE', *, *, #6958, .F. ) ;
#12500 = CARTESIAN_POINT ( 'NONE',  ( 7.361572987183170547, 22.05059781766745530, 9.846743663894590881 ) ) ;
#12502 = CARTESIAN_POINT ( 'NONE',  ( 2.791683348922237240, 35.38393115100079456, -7.208316651077763204 ) ) ;
#12501 = CARTESIAN_POINT ( 'NONE',  ( 19.42250999205614548, 50.98035201082151247, -5.440088680355545492 ) ) ;
#12503 = CARTESIAN_POINT ( 'NONE',  ( 19.42250999205614548, 5.980352010821504471, -5.440088680355545492 ) ) ;
#12504 = CARTESIAN_POINT ( 'NONE',  ( -1.099225684535947600, 44.54030133659708923, 6.408140936763237150 ) ) ;
#12505 = CARTESIAN_POINT ( 'NONE',  ( 12.63842701281683922, 44.55059781766745175, -9.846743663894590881 ) ) ;
#12506 = SURFACE_STYLE_USAGE ( .BOTH. , #29462 ) ;
#12507 = CARTESIAN_POINT ( 'NONE',  ( -1.099225684535947600, 48.70696800326375353, -6.408140936763238038 ) ) ;
#12508 = CARTESIAN_POINT ( 'NONE',  ( -5.204170427930421283E-15, -34.44625116508602503, -14.16423886937410082 ) ) ;
#12509 = CARTESIAN_POINT ( 'NONE',  ( 7.361572987183169658, 44.96726448433412315, -9.846743663894592657 ) ) ;
#12510 = CARTESIAN_POINT ( 'NONE',  ( 6.204703633549690345, 27.84541550158063217, 14.16423886937410082 ) ) ;
#12511 = EDGE_LOOP ( 'NONE', ( #97985, #71298, #56134, #38783 ) ) ;
#12512 = DIRECTION ( 'NONE',  ( 0.000000000000000000, 1.000000000000000000, 0.000000000000000000 ) ) ;
#12513 = CARTESIAN_POINT ( 'NONE',  ( 10.00000000000000178, 49.31368534415484106, 10.88017736071110342 ) ) ;
#12514 = CARTESIAN_POINT ( 'NONE',  ( 0.5774900079438590739, 47.64701867748817676, -5.440088680355550821 ) ) ;
#12515 = CARTESIAN_POINT ( 'NONE',  ( 24.16423886937410614, 44.51208216824730357, -3.795296366450302550 ) ) ;
#12516 = CARTESIAN_POINT ( 'NONE',  ( 0.1532563361054082862, 61.21726448433412315, 2.638427012816831674 ) ) ;
#12517 = CARTESIAN_POINT ( 'NONE',  ( 0.1077916266722667299, 57.24062864464239908, -6.478736007405996311 ) ) ;
#12518 = CARTESIAN_POINT ( 'NONE',  ( 15.44008868035555793, 36.39701867748816966, -9.422509992056140149 ) ) ;
#12519 = CARTESIAN_POINT ( 'NONE',  ( -3.335590168189931592, -2.700456006050038216, -2.500000000000000000 ) ) ;
#12520 = COLOUR_RGB ( '', 0.40784314, 0.44705882, 0.49803922) ;
#12521 = CARTESIAN_POINT ( 'NONE',  ( 16.40814093676323893, 25.79030133659708923, 11.09922568453595026 ) ) ;
#12522 = CARTESIAN_POINT ( 'NONE',  ( 10.00000000000000000, 59.75893115100078745, -9.846743663894594434 ) ) ;
#12523 = CARTESIAN_POINT ( 'NONE',  ( -7.964842623401172439, 13.68868534415483573, 7.964842623401183097 ) ) ;
#12524 = CARTESIAN_POINT ( 'NONE',  ( 0.5774900079438590739, 2.647018677488170990, -5.440088680355550821 ) ) ;
#12525 = CARTESIAN_POINT ( 'NONE',  ( 4.559911319644449179, 68.89701867748817676, 9.422509992056141925 ) ) ;
#12526 = VERTEX_POINT ( 'NONE', #59665 ) ;
#12527 = VECTOR ( 'NONE', #91253, 1000.000000000000000 ) ;
#12528 = FACE_OUTER_BOUND ( 'NONE', #32685, .T. ) ;
#12529 = EDGE_CURVE ( 'NONE', #58088, #39614, #36522, .T. ) ;
#12530 = FACE_OUTER_BOUND ( 'NONE', #97549, .T. ) ;
#12531 = VECTOR ( 'NONE', #95074, 1000.000000000000000 ) ;
#12532 = CARTESIAN_POINT ( 'NONE',  ( 20.88017736071110875, 60.77201867748817676, -2.915334737309920765 ) ) ;
#12533 = CARTESIAN_POINT ( 'NONE',  ( 2.791683348922237240, 5.383931151000785675, -7.208316651077763204 ) ) ;
#12534 = CARTESIAN_POINT ( 'NONE',  ( 0.000000000000000000, 14.49999999999999822, 0.000000000000000000 ) ) ;
#12535 = CARTESIAN_POINT ( 'NONE',  ( 0.1532563361054082862, 36.21726448433410894, 2.638427012816831674 ) ) ;
#12536 = EDGE_CURVE ( 'NONE', #27652, #69653, #87468, .T. ) ;
#12537 = CARTESIAN_POINT ( 'NONE',  ( 17.96484262340118221, 19.93868534415484106, 7.964842623401181321 ) ) ;
#12538 = CARTESIAN_POINT ( 'NONE',  ( -1.099225684535947600, 8.706968003263753531, -6.408140936763238038 ) ) ;
#12540 = CARTESIAN_POINT ( 'NONE',  ( 3.469446951953614189E-15, 8.912123368507815613, 11.92686044187656513 ) ) ;
#12539 = CARTESIAN_POINT ( 'NONE',  ( 0.5774900079438607392, 38.48035201082150536, 5.440088680355550821 ) ) ;
#12541 =( LENGTH_UNIT ( ) NAMED_UNIT ( * ) SI_UNIT ( .MILLI., .METRE. ) );
#12542 = CARTESIAN_POINT ( 'NONE',  ( 13.43411237798106583, 42.66530133659707502, -12.81628187352647252 ) ) ;
#12543 = ORIENTED_EDGE ( 'NONE', *, *, #30838, .T. ) ;
#12544 = CARTESIAN_POINT ( 'NONE',  ( 0.5774900079438590739, 62.64701867748817676, -5.440088680355550821 ) ) ;
#12546 = CARTESIAN_POINT ( 'NONE',  ( 18.52753015748617571, 18.09226448433411960, 4.923371831947298993 ) ) ;
#12545 = CARTESIAN_POINT ( 'NONE',  ( 10.00000000000000000, 22.87363466993042138, -12.81628187352647608 ) ) ;
#12547 = DIRECTION ( 'NONE',  ( 0.000000000000000000, 1.000000000000000000, 0.000000000000000000 ) ) ;
#12548 = CARTESIAN_POINT ( 'NONE',  ( 20.88017736071110519, 35.56368534415484106, 2.639326808657452039E-16 ) ) ;
#12549 = CARTESIAN_POINT ( 'NONE',  ( 17.20831665107776587, 64.13393115100079456, -7.208316651077762316 ) ) ;
#12550 = CARTESIAN_POINT ( 'NONE',  ( -2.266590686148945544, 62.22041550158063927, 7.082119434687048631 ) ) ;
#12551 = CARTESIAN_POINT ( 'NONE',  ( 18.52753015748618282, 48.92559781766745886, -4.923371831947291888 ) ) ;
#12552 = CARTESIAN_POINT ( 'NONE',  ( 19.84674366389459621, 3.508931151000785231, 7.409399052514197653E-17 ) ) ;
#12553 = CARTESIAN_POINT ( 'NONE',  ( 10.00000000000000000, 66.81368534415484817, -10.88017736071110342 ) ) ;
#12554 = CARTESIAN_POINT ( 'NONE',  ( 0.2751277870542980231, 5.302231764288316107, 6.500000000000002665 ) ) ;
#12555 = CARTESIAN_POINT ( 'NONE',  ( -4.164238869374099927, 27.01208216824730357, 3.795296366450308767 ) ) ;
#12556 = ADVANCED_FACE ( 'NONE', ( #62606 ), #8640, .F. ) ;
#12557 = CARTESIAN_POINT ( 'NONE',  ( -3.522141228720374162, -0.8488377518990324333, -4.000000000000000000 ) ) ;
#12558 = ORIENTED_EDGE ( 'NONE', *, *, #93514, .T. ) ;
#12559 = CARTESIAN_POINT ( 'NONE',  ( 10.00000000000000000, 1.813685344154838175, -10.88017736071110342 ) ) ;
#12560 = CARTESIAN_POINT ( 'NONE',  ( 6.204703633549690345, 52.84541550158062506, 14.16423886937410082 ) ) ;
#12561 = CARTESIAN_POINT ( 'NONE',  ( 19.84674366389459621, 28.50893115100078745, 7.409399052514197653E-17 ) ) ;
#12562 = CARTESIAN_POINT ( 'NONE',  ( 22.81628187352647785, 31.41530133659709279, 3.434112377981063169 ) ) ;
#12563 = CARTESIAN_POINT ( 'NONE',  ( -13.65777738219310677, 90.97033672325892439, 7.949049539904468276 ) ) ;
#12564 = SURFACE_SIDE_STYLE ('',( #43066 ) ) ;
#12565 = SURFACE_STYLE_USAGE ( .BOTH. , #4095 ) ;
#12566 = CARTESIAN_POINT ( 'NONE',  ( -4.164238869374098151, 61.59541550158063217, -3.795296366450310543 ) ) ;
#12567 = DIRECTION ( 'NONE',  ( -0.6087614290087131064, 0.000000000000000000, -0.7933533402912409382 ) ) ;
#12568 = CARTESIAN_POINT ( 'NONE',  ( 7.361572987183169658, 4.967264484334119601, -9.846743663894592657 ) ) ;
#12569 = EDGE_CURVE ( 'NONE', #73387, #58242, #32107, .T. ) ;
#12570 = CARTESIAN_POINT ( 'NONE',  ( 8.527530157486179263, 3.092264484334125818, 4.923371831947292776 ) ) ;
#12571 = ORIENTED_EDGE ( 'NONE', *, *, #69001, .F. ) ;
#12572 = VECTOR ( 'NONE', #64166, 1000.000000000000000 ) ;
#12573 = VERTEX_POINT ( 'NONE', #85135 ) ;
#12574 = DIRECTION ( 'NONE',  ( 0.000000000000000000, 1.000000000000000000, 0.000000000000000000 ) ) ;
#12575 = VERTEX_POINT ( 'NONE', #31130 ) ;
#12576 = CARTESIAN_POINT ( 'NONE',  ( 20.36894250292379382, 13.67874883491396965, 10.36894250292379205 ) ) ;
#12578 = CARTESIAN_POINT ( 'NONE',  ( 19.42250999205614193, 20.14701867748817321, 5.440088680355555262 ) ) ;
#12577 = CARTESIAN_POINT ( 'NONE',  ( 12.91533473730992121, 14.52201867748817143, 10.88017736071110164 ) ) ;
#12580 = CARTESIAN_POINT ( 'NONE',  ( 19.38216949554541557, 17.24863466993041783, -9.382169495545420901 ) ) ;
#12579 = CARTESIAN_POINT ( 'NONE',  ( 5.076628168052704559, 45.17559781766745175, -8.527530157486179263 ) ) ;
#12581 = DIRECTION ( 'NONE',  ( 0.000000000000000000, 0.000000000000000000, -1.000000000000000000 ) ) ;
#12582 = CARTESIAN_POINT ( 'NONE',  ( 21.09922568453595559, 27.04030133659708568, -6.408140936763230044 ) ) ;
#12583 = EDGE_LOOP ( 'NONE', ( #75788, #95954, #72667, #77169 ) ) ;
#12584 = CARTESIAN_POINT ( 'NONE',  ( 14.92337183194729633, 37.67559781766745175, 8.527530157486181039 ) ) ;
#12585 = CARTESIAN_POINT ( 'NONE',  ( 20.36894250292379738, 64.92874883491397497, -10.36894250292379027 ) ) ;
#12586 = CARTESIAN_POINT ( 'NONE',  ( -0.8801773607111009756, 8.063685344154837509, 1.068504757029289695E-15 ) ) ;
#12587 = ORIENTED_EDGE ( 'NONE', *, *, #77642, .T. ) ;
#12588 = CARTESIAN_POINT ( 'NONE',  ( 2.035157376598822676, 47.43868534415484817, -7.964842623401177768 ) ) ;
#12589 = CARTESIAN_POINT ( 'NONE',  ( 7.084665262690076126, 44.10535201082151247, 10.88017736071109987 ) ) ;
#12590 = CARTESIAN_POINT ( 'NONE',  ( 10.00000000000000178, 49.31368534415484106, 10.88017736071110342 ) ) ;
#12591 = DIRECTION ( 'NONE',  ( 1.000000000000000000, 0.000000000000000000, 0.000000000000000000 ) ) ;
#12592 = CARTESIAN_POINT ( 'NONE',  ( 20.88017736071110875, 35.77201867748816966, -2.915334737309920765 ) ) ;
#12593 = CARTESIAN_POINT ( 'NONE',  ( -6.090257717040695518, 15.00000000000000178, 13.29726560978565075 ) ) ;
#12594 = VECTOR ( 'NONE', #9132, 1000.000000000000000 ) ;
#12595 = ADVANCED_FACE ( 'NONE', ( #17635 ), #61625, .T. ) ;
#12596 = CARTESIAN_POINT ( 'NONE',  ( -7.750000000000000000, 80.32179676972448590, 3.750000000000000000 ) ) ;
#12597 = CARTESIAN_POINT ( 'NONE',  ( 19.84674366389459621, 23.50893115100078390, 7.409399052514197653E-17 ) ) ;
#12598 = ORIENTED_EDGE ( 'NONE', *, *, #32120, .T. ) ;
#12599 = CARTESIAN_POINT ( 'NONE',  ( 5.076628168052704559, 60.17559781766745175, -8.527530157486179263 ) ) ;
#12600 = DIRECTION ( 'NONE',  ( -1.000000000000000000, 0.000000000000000000, -0.000000000000000000 ) ) ;
#12601 = CARTESIAN_POINT ( 'NONE',  ( -6.560019409699617832, -50.64698701990471363, 2.750000000000000000 ) ) ;
#12602 = ORIENTED_EDGE ( 'NONE', *, *, #3122, .F. ) ;
#12603 = CYLINDRICAL_SURFACE ( 'NONE', #76409, 0.2500000000000002220 ) ;
#12604 = DIRECTION ( 'NONE',  ( 1.000000000000000000, 6.938893903907222067E-15, 0.000000000000000000 ) ) ;
#12605 = CARTESIAN_POINT ( 'NONE',  ( 2.791683348922237240, 65.38393115100078035, -7.208316651077763204 ) ) ;
#12606 = CARTESIAN_POINT ( 'NONE',  ( 24.16423886937409904, 64.09541550158064638, 3.795296366450317205 ) ) ;
#12607 = CARTESIAN_POINT ( 'NONE',  ( 18.72515096720583827, 65.05509018479936856, 6.499999999999810818 ) ) ;
#12608 = ORIENTED_EDGE ( 'NONE', *, *, #85248, .F. ) ;
#12609 = FACE_OUTER_BOUND ( 'NONE', #54185, .T. ) ;
#12610 = CARTESIAN_POINT ( 'NONE',  ( 7.361572987183170547, 32.05059781766745175, 9.846743663894590881 ) ) ;
#12611 = DIRECTION ( 'NONE',  ( -0.000000000000000000, -0.000000000000000000, -1.000000000000000000 ) ) ;
#12612 = CARTESIAN_POINT ( 'NONE',  ( 10.00000000000000000, 7.873634669930421381, -12.81628187352647608 ) ) ;
#12613 = CARTESIAN_POINT ( 'NONE',  ( 12.63842701281683922, 9.550597817667449974, -9.846743663894590881 ) ) ;
#12614 = VECTOR ( 'NONE', #25875, 1000.000000000000000 ) ;
#12615 = DIRECTION ( 'NONE',  ( 0.000000000000000000, -0.000000000000000000, -1.000000000000000000 ) ) ;
#12616 = CARTESIAN_POINT ( 'NONE',  ( 7.361572987183169658, 9.967264484334119601, -9.846743663894592657 ) ) ;
#12617 = CARTESIAN_POINT ( 'NONE',  ( 2.791683348922237240, 60.38393115100078745, -7.208316651077763204 ) ) ;
#12618 = DIRECTION ( 'NONE',  ( 0.000000000000000000, 0.000000000000000000, -1.000000000000000000 ) ) ;
#12619 = ORIENTED_EDGE ( 'NONE', *, *, #49798, .T. ) ;
#12620 = CARTESIAN_POINT ( 'NONE',  ( 0.5774900079438607392, 3.480352010821504916, 5.440088680355550821 ) ) ;
#12621 = CARTESIAN_POINT ( 'NONE',  ( -0.3689425029237898834, 11.17874883491396787, -10.36894250292378850 ) ) ;
#12622 = CARTESIAN_POINT ( 'NONE',  ( 19.84674366389459621, 18.50893115100078745, 7.409399052514197653E-17 ) ) ;
#12623 = CARTESIAN_POINT ( 'NONE',  ( 17.96484262340118221, 54.93868534415484106, 7.964842623401181321 ) ) ;
#12625 =( NAMED_UNIT ( * ) PLANE_ANGLE_UNIT ( ) SI_UNIT ( $, .RADIAN. ) );
#12624 = CARTESIAN_POINT ( 'NONE',  ( -2.816281873526471635, 23.91530133659708568, -3.434112377981056508 ) ) ;
#12626 = CARTESIAN_POINT ( 'NONE',  ( -13.78891971893212443, 0.5000000000000004441, 5.904717858191433244 ) ) ;
#12627 = CARTESIAN_POINT ( 'NONE',  ( -0.1503990784575282014, 57.22266099184919597, -6.262539305110077947 ) ) ;
#12628 = CARTESIAN_POINT ( 'NONE',  ( 9.065164099344530158, 0.5000000000000004441, -11.95084933600767307 ) ) ;
#12629 = VECTOR ( 'NONE', #67649, 1000.000000000000114 ) ;
#12630 = CARTESIAN_POINT ( 'NONE',  ( 3.591859063236763294, -1.709698663402913210, -11.09922568453595026 ) ) ;
#12631 = CARTESIAN_POINT ( 'NONE',  ( 12.63842701281683034, 17.46726448433411250, 9.846743663894596210 ) ) ;
#12632 = CARTESIAN_POINT ( 'NONE',  ( 7.964842623401181321, -25.06131465584515894, 7.964842623401174215 ) ) ;
#12633 = CARTESIAN_POINT ( 'NONE',  ( 13.43411237798106583, 17.66530133659708923, -12.81628187352647252 ) ) ;
#12634 = CARTESIAN_POINT ( 'NONE',  ( -10.67057496914079096, -97.55820424040057048, -4.000000000000000000 ) ) ;
#12635 = ADVANCED_FACE ( 'NONE', ( #1163 ), #70628, .F. ) ;
#12637 = DIRECTION ( 'NONE',  ( -1.000000000000000000, 0.000000000000000000, 0.000000000000000000 ) ) ;
#12636 = CARTESIAN_POINT ( 'NONE',  ( 10.00000000000000000, 26.81368534415484106, -10.88017736071110342 ) ) ;
#12638 = CARTESIAN_POINT ( 'NONE',  ( -10.09792486685175916, 14.95037105583725534, -10.75589247084427136 ) ) ;
#12639 = CARTESIAN_POINT ( 'NONE',  ( 24.16423886937409904, 44.09541550158063927, 3.795296366450317205 ) ) ;
#12640 = CARTESIAN_POINT ( 'NONE',  ( 26.00000000000000355, 35.99999999999997158, -10.00000000000000000 ) ) ;
#12641 = CARTESIAN_POINT ( 'NONE',  ( 15.44008868035555793, 21.39701867748817321, -9.422509992056140149 ) ) ;
#12642 = EDGE_CURVE ( 'NONE', #61749, #68154, #31624, .T. ) ;
#12643 = CARTESIAN_POINT ( 'NONE',  ( 5.076628168052704559, 45.17559781766745175, -8.527530157486179263 ) ) ;
#12644 = CARTESIAN_POINT ( 'NONE',  ( 2.035157376598824452, 58.68868534415482685, 7.964842623401179544 ) ) ;
#12645 = CARTESIAN_POINT ( 'NONE',  ( 17.08211943468705840, 35.13708216824730357, -12.26659068614894466 ) ) ;
#12647 = ADVANCED_FACE ( 'NONE', ( #24147 ), #85901, .F. ) ;
#12646 = DIRECTION ( 'NONE',  ( 1.000000000000000000, 0.000000000000000000, 0.000000000000000000 ) ) ;
#12648 = ADVANCED_FACE ( 'NONE', ( #86124 ), #1658, .T. ) ;
#12649 = CARTESIAN_POINT ( 'NONE',  ( 18.52753015748617571, 33.09226448433411605, 4.923371831947298993 ) ) ;
#12650 = LINE ( 'NONE', #6145, #53550 ) ;
#12651 = CARTESIAN_POINT ( 'NONE',  ( 21.09922568453594849, 1.206968003263753531, 6.408140936763242479 ) ) ;
#12652 = VERTEX_POINT ( 'NONE', #39645 ) ;
#12653 = CARTESIAN_POINT ( 'NONE',  ( 0.5774900079438607392, 23.48035201082150536, 5.440088680355550821 ) ) ;
#12654 = DIRECTION ( 'NONE',  ( -0.000000000000000000, -1.000000000000000000, -0.000000000000000000 ) ) ;
#12655 = FACE_OUTER_BOUND ( 'NONE', #939, .T. ) ;
#12656 = CARTESIAN_POINT ( 'NONE',  ( 2.035157376598824452, 8.688685344154839285, 7.964842623401179544 ) ) ;
#12657 = CARTESIAN_POINT ( 'NONE',  ( 1.472469842513823179, 1.425597817667451528, 4.923371831947296329 ) ) ;
#12658 = VECTOR ( 'NONE', #88805, 1000.000000000000000 ) ;
#12659 = CARTESIAN_POINT ( 'NONE',  ( 6.204703633549690345, 20.76208216824730357, -14.16423886937410259 ) ) ;
#12660 = CARTESIAN_POINT ( 'NONE',  ( 5.076628168052703671, 16.84226448433411960, 8.527530157486179263 ) ) ;
#12661 = CARTESIAN_POINT ( 'NONE',  ( 10.00000000000000000, 59.75893115100078745, -9.846743663894594434 ) ) ;
#12662 = CARTESIAN_POINT ( 'NONE',  ( -0.8801773607110991993, 32.85535201082151247, -2.915334737309923874 ) ) ;
#12663 = DIRECTION ( 'NONE',  ( 0.000000000000000000, 0.000000000000000000, 1.000000000000000000 ) ) ;
#12664 = LINE ( 'NONE', #4695, #76077 ) ;
#12665 = EDGE_LOOP ( 'NONE', ( #34127, #89926, #27157, #30111 ) ) ;
#12666 = DIRECTION ( 'NONE',  ( 1.000000000000000000, -0.000000000000000000, 0.000000000000000000 ) ) ;
#12667 = CARTESIAN_POINT ( 'NONE',  ( 7.361572987183169658, 49.96726448433410894, -9.846743663894592657 ) ) ;
#12668 = ORIENTED_EDGE ( 'NONE', *, *, #43116, .T. ) ;
#12669 = VERTEX_POINT ( 'NONE', #2649 ) ;
#12670 = DIRECTION ( 'NONE',  ( 0.000000000000000000, 1.000000000000000000, 0.000000000000000000 ) ) ;
#12671 = CARTESIAN_POINT ( 'NONE',  ( -2.266590686148945544, 26.38708216824730357, -7.082119434687050408 ) ) ;
#12672 = CARTESIAN_POINT ( 'NONE',  ( -4.164238869374099039, 11.80374883491396965, 8.674139862899312516E-16 ) ) ;
#12673 = CARTESIAN_POINT ( 'NONE',  ( 12.91533473730992121, 59.52201867748816966, 10.88017736071110164 ) ) ;
#12674 = CARTESIAN_POINT ( 'NONE',  ( 2.917880565312950480, 50.97041550158064638, -12.26659068614894821 ) ) ;
#12675 = CARTESIAN_POINT ( 'NONE',  ( 19.38216949554541557, 2.248634669930420049, -9.382169495545420901 ) ) ;
#12676 = CARTESIAN_POINT ( 'NONE',  ( 12.63842701281683034, 32.46726448433412315, 9.846743663894596210 ) ) ;
#12677 = DIRECTION ( 'NONE',  ( 0.8070303256584298035, -0.5905099943842175847, 0.000000000000000000 ) ) ;
#12679 = CARTESIAN_POINT ( 'NONE',  ( 0.6178305044545818747, 3.498634669930420049, -9.382169495545419124 ) ) ;
#12678 = CARTESIAN_POINT ( 'NONE',  ( 4.559911319644449179, 37.23035201082150536, -9.422509992056141925 ) ) ;
#12680 = CARTESIAN_POINT ( 'NONE',  ( 20.36894250292379382, 8.678748834913967869, 10.36894250292379205 ) ) ;
#12681 = CARTESIAN_POINT ( 'NONE',  ( 24.16423886937410614, 49.51208216824730357, -3.795296366450302550 ) ) ;
#12682 = CARTESIAN_POINT ( 'NONE',  ( 17.96484262340118221, 14.93868534415484106, 7.964842623401181321 ) ) ;
#12683 = CARTESIAN_POINT ( 'NONE',  ( 19.39235739573468820, 4.875764716086009365, 6.500000000000002665 ) ) ;
#12684 = CARTESIAN_POINT ( 'NONE',  ( 0.000000000000000000, 0.5000000000000004441, 0.000000000000000000 ) ) ;
#12685 = CARTESIAN_POINT ( 'NONE',  ( 15.44008868035555793, 41.39701867748817676, -9.422509992056140149 ) ) ;
#12686 = EDGE_CURVE ( 'NONE', #35060, #37315, #58697, .T. ) ;
#12687 = AXIS2_PLACEMENT_3D ( 'NONE', #65689, #95715, #42710 ) ;
#12688 = CARTESIAN_POINT ( 'NONE',  ( 9.846743663894594434, -31.49106884899921610, -2.168404344971008868E-15 ) ) ;
#12689 = ORIENTED_EDGE ( 'NONE', *, *, #78395, .F. ) ;
#12690 = LINE ( 'NONE', #71726, #20379 ) ;
#12691 = ORIENTED_EDGE ( 'NONE', *, *, #18470, .T. ) ;
#12692 = VERTEX_POINT ( 'NONE', #77131 ) ;
#12693 = CARTESIAN_POINT ( 'NONE',  ( 2.917880565312948704, 52.63708216824730357, 12.26659068614894643 ) ) ;
#12694 = CARTESIAN_POINT ( 'NONE',  ( 19.84674366389459266, 43.71726448433410894, -2.638427012816827677 ) ) ;
#12695 = CARTESIAN_POINT ( 'NONE',  ( 15.44008868035555793, 61.39701867748817676, -9.422509992056140149 ) ) ;
#12696 = VECTOR ( 'NONE', #24003, 1000.000000000000000 ) ;
#12697 = PLANE ( 'NONE',  #43227 ) ;
#12698 = ADVANCED_FACE ( 'NONE', ( #48106 ), #40128, .F. ) ;
#12699 = CARTESIAN_POINT ( 'NONE',  ( 4.559911319644449179, 58.89701867748817676, 9.422509992056141925 ) ) ;
#12700 = CARTESIAN_POINT ( 'NONE',  ( 16.40814093676324603, 57.45696800326375353, -11.09922568453594671 ) ) ;
#12701 = CARTESIAN_POINT ( 'NONE',  ( 12.81628187352647608, 6.623634669930426710, -2.602085213965210642E-15 ) ) ;
#12702 = VERTEX_POINT ( 'NONE', #40625 ) ;
#12703 = CARTESIAN_POINT ( 'NONE',  ( 4.559911319644449179, 47.23035201082150536, -9.422509992056141925 ) ) ;
#12704 = CARTESIAN_POINT ( 'NONE',  ( 17.08211943468705130, 18.47041550158063572, 12.26659068614894998 ) ) ;
#12705 = CARTESIAN_POINT ( 'NONE',  ( 22.81628187352647785, 26.62363466993042138, 6.195893100308588602E-16 ) ) ;
#12706 = ORIENTED_EDGE ( 'NONE', *, *, #87259, .F. ) ;
#12707 = CARTESIAN_POINT ( 'NONE',  ( 16.40814093676323893, 40.79030133659708923, 11.09922568453595026 ) ) ;
#12708 = CARTESIAN_POINT ( 'NONE',  ( 15.44008868035555793, 16.39701867748817321, -9.422509992056140149 ) ) ;
#12709 = CARTESIAN_POINT ( 'NONE',  ( 2.791683348922237240, 35.38393115100079456, -7.208316651077763204 ) ) ;
#12710 = CARTESIAN_POINT ( 'NONE',  ( 12.91533473730993009, 6.605352010821504471, -10.88017736071109987 ) ) ;
#12711 = CARTESIAN_POINT ( 'NONE',  ( 10.00000000000000178, 50.37363466993042493, 12.81628187352647608 ) ) ;
#12712 = DIRECTION ( 'NONE',  ( 0.000000000000000000, -1.000000000000000000, 0.000000000000000000 ) ) ;
#12713 = CARTESIAN_POINT ( 'NONE',  ( 12.63842701281683034, 42.46726448433412315, 9.846743663894596210 ) ) ;
#12714 = VECTOR ( 'NONE', #54334, 1000.000000000000000 ) ;
#12716 = EDGE_LOOP ( 'NONE', ( #86106, #51577, #17910, #72488, #59666 ) ) ;
#12715 = DIRECTION ( 'NONE',  ( -0.000000000000000000, -1.000000000000000000, -0.000000000000000000 ) ) ;
#12717 = DIRECTION ( 'NONE',  ( -0.000000000000000000, -0.000000000000000000, -1.000000000000000000 ) ) ;
#12718 = DIRECTION ( 'NONE',  ( -0.000000000000000000, 0.000000000000000000, 1.000000000000000000 ) ) ;
#12719 = CARTESIAN_POINT ( 'NONE',  ( 0.000000000000000000, 0.000000000000000000, -2.500000000000000000 ) ) ;
#12720 = CARTESIAN_POINT ( 'NONE',  ( 17.20831665107776587, 24.13393115100078035, -7.208316651077762316 ) ) ;
#12721 = CARTESIAN_POINT ( 'NONE',  ( 10.00000000000000178, 25.37363466993041783, 12.81628187352647608 ) ) ;
#12722 = ORIENTED_EDGE ( 'NONE', *, *, #54641, .F. ) ;
#12723 = CARTESIAN_POINT ( 'NONE',  ( 17.20831665107776587, 62.88393115100078745, 7.208316651077764980 ) ) ;
#12724 = CARTESIAN_POINT ( 'NONE',  ( -9.820682251645251881, 0.2306972965111889484, 11.26020669458352685 ) ) ;
#12725 = CARTESIAN_POINT ( 'NONE',  ( 24.16423886937410614, 14.51208216824730179, -3.795296366450302550 ) ) ;
#12726 = CARTESIAN_POINT ( 'NONE',  ( 14.92337183194729633, 47.67559781766745175, 8.527530157486181039 ) ) ;
#12727 = CARTESIAN_POINT ( 'NONE',  ( -1.099225684535947600, 43.70696800326375353, -6.408140936763238038 ) ) ;
#12728 = DIRECTION ( 'NONE',  ( -0.000000000000000000, -0.000000000000000000, -1.000000000000000000 ) ) ;
#12729 = CARTESIAN_POINT ( 'NONE',  ( 12.91533473730992121, 64.52201867748817676, 10.88017736071110164 ) ) ;
#12730 = CARTESIAN_POINT ( 'NONE',  ( 0.000000000000000000, 0.5000000000000004441, 0.000000000000000000 ) ) ;
#12731 = EDGE_CURVE ( 'NONE', #55238, #44298, #41407, .T. ) ;
#12732 = CARTESIAN_POINT ( 'NONE',  ( 18.52753015748618282, 33.92559781766745886, -4.923371831947291888 ) ) ;
#12733 = CARTESIAN_POINT ( 'NONE',  ( -0.8801773607110991993, 37.85535201082151247, -2.915334737309923874 ) ) ;
#12734 = CARTESIAN_POINT ( 'NONE',  ( -1.099225684535947600, 44.54030133659708923, 6.408140936763237150 ) ) ;
#12735 = CARTESIAN_POINT ( 'NONE',  ( 19.72487221294570858, 70.00000000000000000, -6.000000000000000000 ) ) ;
#12736 = CARTESIAN_POINT ( 'NONE',  ( -0.8801773607111008646, 33.27201867748817676, 2.915334737309923430 ) ) ;
#12737 = VERTEX_POINT ( 'NONE', #70138 ) ;
#12738 = FACE_OUTER_BOUND ( 'NONE', #387, .T. ) ;
#12739 = CARTESIAN_POINT ( 'NONE',  ( 12.91533473730993009, 11.60535201082150536, -10.88017736071109987 ) ) ;
#12741 = CARTESIAN_POINT ( 'NONE',  ( 20.88017736071110519, 50.56368534415484106, 2.639326808657452039E-16 ) ) ;
#12740 = CARTESIAN_POINT ( 'NONE',  ( 0.1532563361054083140, 56.00893115100078745, 1.131784320476157264E-15 ) ) ;
#12742 = DIRECTION ( 'NONE',  ( -1.000000000000000000, 0.000000000000000000, 0.000000000000000000 ) ) ;
#12743 = CARTESIAN_POINT ( 'NONE',  ( 15.44008868035555260, 64.73035201082151957, 9.422509992056143702 ) ) ;
#12744 = VECTOR ( 'NONE', #89391, 1000.000000000000000 ) ;
#12746 = CARTESIAN_POINT ( 'NONE',  ( 0.000000000000000000, 73.93174988520466684, -5.598587842719937591 ) ) ;
#12745 = CARTESIAN_POINT ( 'NONE',  ( 19.42250999205614193, 30.14701867748817321, 5.440088680355555262 ) ) ;
#12747 = CARTESIAN_POINT ( 'NONE',  ( 19.84674366389459266, 23.30059781766745530, 2.638427012816836559 ) ) ;
#12748 = CARTESIAN_POINT ( 'NONE',  ( 0.000000000000000000, 0.000000000000000000, 0.000000000000000000 ) ) ;
#12749 = CARTESIAN_POINT ( 'NONE',  ( 10.36894250292378850, 9.928748834913969645, -10.36894250292379027 ) ) ;
#12750 = CARTESIAN_POINT ( 'NONE',  ( 0.1532563361054082862, 46.21726448433411605, 2.638427012816831674 ) ) ;
#12751 = AXIS2_PLACEMENT_3D ( 'NONE', #91289, #98336, #29794 ) ;
#12753 = CARTESIAN_POINT ( 'NONE',  ( -11.62112565934162767, 2.541098841762901017E-16, 8.881879596174677260 ) ) ;
#12752 = CARTESIAN_POINT ( 'NONE',  ( 20.36894250292379738, 59.92874883491397497, -10.36894250292379027 ) ) ;
#12754 = DIRECTION ( 'NONE',  ( -1.483861936729427615E-16, 1.000000000000000000, -0.000000000000000000 ) ) ;
#12755 = CIRCLE ( 'NONE', #55888, 14.49999999999999822 ) ;
#12756 = CARTESIAN_POINT ( 'NONE',  ( 13.79529636645030344, 8.262082168247300018, 14.16423886937410614 ) ) ;
#12757 = CARTESIAN_POINT ( 'NONE',  ( 10.00000000000000000, 40.55374883491397497, -14.16423886937410082 ) ) ;
#12758 = CARTESIAN_POINT ( 'NONE',  ( 19.38216949554541202, 5.998634669930420493, 9.382169495545424454 ) ) ;
#12759 = ADVANCED_FACE ( 'NONE', ( #91651 ), #92625, .T. ) ;
#12760 = ORIENTED_EDGE ( 'NONE', *, *, #6319, .T. ) ;
#12761 = CARTESIAN_POINT ( 'NONE',  ( -0.8801773607110991993, 12.85535201082150358, -2.915334737309923874 ) ) ;
#12762 = CARTESIAN_POINT ( 'NONE',  ( 2.791683348922240793, 31.63393115100078745, 7.208316651077764092 ) ) ;
#12764 = DIRECTION ( 'NONE',  ( 1.257402221000611116E-16, -1.000000000000000000, -0.000000000000000000 ) ) ;
#12763 = CARTESIAN_POINT ( 'NONE',  ( -0.3689425029237898834, 1.178748834913967869, -10.36894250292378850 ) ) ;
#12765 = DIRECTION ( 'NONE',  ( -1.000000000000000000, 0.000000000000000000, 0.000000000000000000 ) ) ;
#12766 = ADVANCED_FACE ( 'NONE', ( #54129, #46155 ), #76639, .F. ) ;
#12767 = CARTESIAN_POINT ( 'NONE',  ( -11.22915323889586858, 15.00000000000000000, 8.773176023390528044 ) ) ;
#12768 = CARTESIAN_POINT ( 'NONE',  ( 3.591859063236761518, 19.95696800326375353, 11.09922568453594849 ) ) ;
#12769 = CARTESIAN_POINT ( 'NONE',  ( 12.63842701281683034, 27.46726448433411250, 9.846743663894596210 ) ) ;
#12770 = ORIENTED_EDGE ( 'NONE', *, *, #23931, .T. ) ;
#12771 = CARTESIAN_POINT ( 'NONE',  ( 2.791683348922240793, 6.633931151000785675, 7.208316651077764092 ) ) ;
#12772 = CYLINDRICAL_SURFACE ( 'NONE', #17296, 0.5000000000000004441 ) ;
#12773 = CARTESIAN_POINT ( 'NONE',  ( -2.266590686148945544, 66.38708216824730357, -7.082119434687050408 ) ) ;
#12774 = CARTESIAN_POINT ( 'NONE',  ( 20.88017736071110519, 10.56368534415483751, 2.639326808657452039E-16 ) ) ;
#12775 = CARTESIAN_POINT ( 'NONE',  ( 17.08211943468705130, 38.47041550158063217, 12.26659068614894998 ) ) ;
#12776 = CARTESIAN_POINT ( 'NONE',  ( -0.8801773607110991993, 27.85535201082150181, -2.915334737309923874 ) ) ;
#12777 = CARTESIAN_POINT ( 'NONE',  ( 0.5774900079438590739, 62.64701867748817676, -5.440088680355550821 ) ) ;
#12778 = CYLINDRICAL_SURFACE ( 'NONE', #83066, 0.5000000000000004441 ) ;
#12779 = CARTESIAN_POINT ( 'NONE',  ( 7.361572987183169658, 29.96726448433411960, -9.846743663894592657 ) ) ;
#12780 = DIRECTION ( 'NONE',  ( 0.000000000000000000, 0.000000000000000000, -1.000000000000000000 ) ) ;
#12781 = CARTESIAN_POINT ( 'NONE',  ( 19.84674366389459266, 8.300597817667451750, 2.638427012816836559 ) ) ;
#12782 = CARTESIAN_POINT ( 'NONE',  ( 0.1532563361054082862, 31.21726448433412315, 2.638427012816831674 ) ) ;
#12783 = CARTESIAN_POINT ( 'NONE',  ( 7.361572987183170547, 67.05059781766746596, 9.846743663894590881 ) ) ;
#12784 = CARTESIAN_POINT ( 'NONE',  ( 2.035157376598822676, 42.43868534415483396, -7.964842623401177768 ) ) ;
#12785 = VERTEX_POINT ( 'NONE', #57086 ) ;
#12786 = CARTESIAN_POINT ( 'NONE',  ( 0.6178305044545818747, 43.49863466993042493, -9.382169495545419124 ) ) ;
#12787 = CARTESIAN_POINT ( 'NONE',  ( 15.44008868035555793, 61.39701867748817676, -9.422509992056140149 ) ) ;
#12788 = CARTESIAN_POINT ( 'NONE',  ( 10.00000000000000000, 42.87363466993042493, -12.81628187352647608 ) ) ;
#12790 = CARTESIAN_POINT ( 'NONE',  ( 18.52753015748618282, 33.92559781766745886, -4.923371831947291888 ) ) ;
#12789 = CARTESIAN_POINT ( 'NONE',  ( 20.36894250292379382, 58.67874883491396076, 10.36894250292379205 ) ) ;
#12791 = DIRECTION ( 'NONE',  ( 3.907985046680550391E-14, 0.000000000000000000, 1.000000000000000000 ) ) ;
#12792 = CARTESIAN_POINT ( 'NONE',  ( 10.00000000000000000, 59.75893115100078745, -9.846743663894594434 ) ) ;
#12793 = CARTESIAN_POINT ( 'NONE',  ( 2.917880565312948704, 17.63708216824730357, 12.26659068614894643 ) ) ;
#12794 = CARTESIAN_POINT ( 'NONE',  ( 24.16423886937410614, 39.30374883491396787, 8.672049930838204340E-16 ) ) ;
#12795 = CARTESIAN_POINT ( 'NONE',  ( 19.84674366389459266, 48.30059781766745175, 2.638427012816836559 ) ) ;
#12796 = CARTESIAN_POINT ( 'NONE',  ( 12.84737282370068812, -0.03417435944610275333, 9.530079116402468742 ) ) ;
#12797 = CARTESIAN_POINT ( 'NONE',  ( 20.88017736071110875, 35.77201867748816966, -2.915334737309920765 ) ) ;
#12798 = ADVANCED_FACE ( 'NONE', ( #41125 ), #97125, .T. ) ;
#12799 = CARTESIAN_POINT ( 'NONE',  ( 10.00000000000000000, 61.81368534415484106, -10.88017736071110342 ) ) ;
#12800 = SURFACE_STYLE_USAGE ( .BOTH. , #58287 ) ;
#12801 = EDGE_LOOP ( 'NONE', ( #2767, #54205, #2648, #81023 ) ) ;
#12802 = CARTESIAN_POINT ( 'NONE',  ( 13.43411237798106583, 47.66530133659709634, -12.81628187352647252 ) ) ;
#12803 = EDGE_LOOP ( 'NONE', ( #20578, #3029, #84427, #39509, #67087, #68786 ) ) ;
#12804 = CARTESIAN_POINT ( 'NONE',  ( 15.44008868035555260, 64.73035201082151957, 9.422509992056143702 ) ) ;
#12805 = ORIENTED_EDGE ( 'NONE', *, *, #44754, .F. ) ;
#12806 = CARTESIAN_POINT ( 'NONE',  ( 24.16423886937410614, 9.303748834913967869, 8.672049930838204340E-16 ) ) ;
#12807 = CARTESIAN_POINT ( 'NONE',  ( 19.84674366389459266, 8.717264484334116048, -2.638427012816827677 ) ) ;
#12808 = CARTESIAN_POINT ( 'NONE',  ( 1.720799100035159679, 0.1239429031973928452, -6.333916461130630005 ) ) ;
#12809 = ORIENTED_EDGE ( 'NONE', *, *, #8175, .F. ) ;
#12810 = TOROIDAL_SURFACE ( 'NONE', #27216, 0.5000000000000000000, 0.2500000000000000000 ) ;
#12811 = PRESENTATION_STYLE_ASSIGNMENT (( #75661 ) ) ;
#12812 = CARTESIAN_POINT ( 'NONE',  ( 2.035157376598822676, 12.43868534415483751, -7.964842623401177768 ) ) ;
#12813 = CARTESIAN_POINT ( 'NONE',  ( 20.88017736071110519, 60.56368534415484106, 2.639326808657452039E-16 ) ) ;
#12814 = CARTESIAN_POINT ( 'NONE',  ( 24.16423886937410614, 19.51208216824729647, -3.795296366450302550 ) ) ;
#12815 = CARTESIAN_POINT ( 'NONE',  ( 20.88017736071110519, 25.56368534415483751, 2.639326808657452039E-16 ) ) ;
#12816 =( GEOMETRIC_REPRESENTATION_CONTEXT ( 3 ) GLOBAL_UNCERTAINTY_ASSIGNED_CONTEXT ( ( #5433 ) ) GLOBAL_UNIT_ASSIGNED_CONTEXT ( ( #98904, #59874, #53361 ) ) REPRESENTATION_CONTEXT ( 'NONE', 'WORKASPACE' ) );
#12817 = CARTESIAN_POINT ( 'NONE',  ( 17.20831665107776587, 59.13393115100078745, -7.208316651077762316 ) ) ;
#12818 = ORIENTED_EDGE ( 'NONE', *, *, #24306, .T. ) ;
#12819 = CARTESIAN_POINT ( 'NONE',  ( 2.791683348922240793, 61.63393115100079456, 7.208316651077764092 ) ) ;
#12820 = ORIENTED_EDGE ( 'NONE', *, *, #98965, .F. ) ;
#12821 = CARTESIAN_POINT ( 'NONE',  ( 0.1532563361054082862, 1.217264484334117824, 2.638427012816831674 ) ) ;
#12822 = CARTESIAN_POINT ( 'NONE',  ( 18.52753015748618282, 58.92559781766745886, -4.923371831947291888 ) ) ;
#12823 = CARTESIAN_POINT ( 'NONE',  ( 21.09922568453594849, 36.20696800326375353, 6.408140936763242479 ) ) ;
#12825 = DIRECTION ( 'NONE',  ( 0.000000000000000000, 1.000000000000000000, 0.000000000000000000 ) ) ;
#12824 = CARTESIAN_POINT ( 'NONE',  ( 2.035157376598824452, 3.688685344154837953, 7.964842623401179544 ) ) ;
#12826 = CARTESIAN_POINT ( 'NONE',  ( 5.076628168052704559, 5.175597817667451750, -8.527530157486179263 ) ) ;
#12827 = VECTOR ( 'NONE', #29188, 1000.000000000000000 ) ;
#12828 = CARTESIAN_POINT ( 'NONE',  ( -0.8801773607111008646, 23.27201867748817676, 2.915334737309923430 ) ) ;
#12829 = ORIENTED_EDGE ( 'NONE', *, *, #10436, .T. ) ;
#12830 = CARTESIAN_POINT ( 'NONE',  ( -2.816281873526473856, 59.33196800326374643, 3.434112377981055619 ) ) ;
#12831 = CARTESIAN_POINT ( 'NONE',  ( 10.00000000000000178, 44.31368534415484106, 10.88017736071110342 ) ) ;
#12832 = CARTESIAN_POINT ( 'NONE',  ( 1.274849032794292736, 47.55509018479936856, -6.499999999999977796 ) ) ;
#12833 = CARTESIAN_POINT ( 'NONE',  ( 21.09922568453594849, 41.20696800326375353, 6.408140936763242479 ) ) ;
#12834 = CARTESIAN_POINT ( 'NONE',  ( 15.44008868035555260, 44.73035201082151247, 9.422509992056143702 ) ) ;
#12835 = CARTESIAN_POINT ( 'NONE',  ( 7.361572987183170547, 57.05059781766744464, 9.846743663894590881 ) ) ;
#12836 = ORIENTED_EDGE ( 'NONE', *, *, #12173, .F. ) ;
#12837 = CIRCLE ( 'NONE', #81504, 4.000000000000003553 ) ;
#12838 = CARTESIAN_POINT ( 'NONE',  ( 19.84674366389459621, 18.50893115100078745, 7.409399052514197653E-17 ) ) ;
#12839 = CARTESIAN_POINT ( 'NONE',  ( 21.09922568453595559, 12.04030133659708746, -6.408140936763230044 ) ) ;
#12841 = CARTESIAN_POINT ( 'NONE',  ( -7.109031286574947650, 14.95037114371795894, 12.92745085449634246 ) ) ;
#12840 = LINE ( 'NONE', #82322, #43579 ) ;
#12842 = CARTESIAN_POINT ( 'NONE',  ( 2.035157376598824452, 18.68868534415484106, 7.964842623401179544 ) ) ;
#12843 = CARTESIAN_POINT ( 'NONE',  ( 12.63842701281683922, 54.55059781766745175, -9.846743663894590881 ) ) ;
#12844 = CARTESIAN_POINT ( 'NONE',  ( -14.47650479471824880, 0.5000000000000004441, 3.928206833721914482 ) ) ;
#12845 = EDGE_CURVE ( 'NONE', #30525, #21081, #11588, .T. ) ;
#12846 = CARTESIAN_POINT ( 'NONE',  ( 5.076628168052704559, 10.17559781766745175, -8.527530157486179263 ) ) ;
#12847 =( NAMED_UNIT ( * ) PLANE_ANGLE_UNIT ( ) SI_UNIT ( $, .RADIAN. ) );
#12849 = ORIENTED_EDGE ( 'NONE', *, *, #87380, .F. ) ;
#12848 = CARTESIAN_POINT ( 'NONE',  ( 10.00000000000000178, 0.3736346699304200492, 12.81628187352647608 ) ) ;
#12850 = CARTESIAN_POINT ( 'NONE',  ( 9.383624259804008716, 14.76984980006448822, 11.62625599701886792 ) ) ;
#12851 = CARTESIAN_POINT ( 'NONE',  ( -36.44000000000000483, 92.00000000000000000, -10.09898361729590199 ) ) ;
#12852 = VECTOR ( 'NONE', #2195, 1000.000000000000000 ) ;
#12853 = CARTESIAN_POINT ( 'NONE',  ( -1.099225684535947600, 39.54030133659708923, 6.408140936763237150 ) ) ;
#12854 = CARTESIAN_POINT ( 'NONE',  ( 17.20831665107776587, 29.13393115100078390, -7.208316651077762316 ) ) ;
#12855 = CARTESIAN_POINT ( 'NONE',  ( 0.8952175423694743728, 57.60160829253887016, -5.990408912944304554 ) ) ;
#12856 = CARTESIAN_POINT ( 'NONE',  ( 2.917880565312948704, 57.63708216824731068, 12.26659068614894643 ) ) ;
#12857 = CARTESIAN_POINT ( 'NONE',  ( 0.1532563361054100626, 25.80059781766744820, -2.638427012816831230 ) ) ;
#12858 = ORIENTED_EDGE ( 'NONE', *, *, #58474, .F. ) ;
#12859 = CARTESIAN_POINT ( 'NONE',  ( 20.00000000000000711, 85.01043265489317946, 4.826711382686302620 ) ) ;
#12860 = CARTESIAN_POINT ( 'NONE',  ( 17.08211943468705840, 55.13708216824731068, -12.26659068614894466 ) ) ;
#12861 = CARTESIAN_POINT ( 'NONE',  ( -8.646548597236176192, 87.41340560412832872, -4.720830526302458807 ) ) ;
#12862 = CARTESIAN_POINT ( 'NONE',  ( 20.88017736071110519, 25.56368534415483751, 2.639326808657452039E-16 ) ) ;
#12863 = CARTESIAN_POINT ( 'NONE',  ( 6.204703633549690345, 42.84541550158063217, 14.16423886937410082 ) ) ;
#12865 = LINE ( 'NONE', #88874, #74945 ) ;
#12864 = CARTESIAN_POINT ( 'NONE',  ( 2.917880565312950480, 50.97041550158064638, -12.26659068614894821 ) ) ;
#12866 = CARTESIAN_POINT ( 'NONE',  ( 19.84674366389459621, 8.508931151000785675, 7.409399052514197653E-17 ) ) ;
#12867 = CARTESIAN_POINT ( 'NONE',  ( 3.591859063236761518, 4.956968003263753531, 11.09922568453594849 ) ) ;
#12868 = ORIENTED_EDGE ( 'NONE', *, *, #73420, .F. ) ;
#12869 = CARTESIAN_POINT ( 'NONE',  ( 10.00000000000000000, 56.81368534415484106, -10.88017736071110342 ) ) ;
#12870 =( LENGTH_UNIT ( ) NAMED_UNIT ( * ) SI_UNIT ( .MILLI., .METRE. ) );
#12871 = CARTESIAN_POINT ( 'NONE',  ( 18.52753015748618282, 58.92559781766745886, -4.923371831947291888 ) ) ;
#12872 = DIRECTION ( 'NONE',  ( -0.6225146366376237417, 0.000000000000000000, 0.7826081568524104748 ) ) ;
#12873 = CARTESIAN_POINT ( 'NONE',  ( 0.1532563361054083140, 66.00893115100079456, 1.131784320476157264E-15 ) ) ;
#12874 = CARTESIAN_POINT ( 'NONE',  ( 0.000000000000000000, 0.5000000000000004441, 0.000000000000000000 ) ) ;
#12875 =( GEOMETRIC_REPRESENTATION_CONTEXT ( 3 ) GLOBAL_UNCERTAINTY_ASSIGNED_CONTEXT ( ( #32335 ) ) GLOBAL_UNIT_ASSIGNED_CONTEXT ( ( #55165, #63158, #82104 ) ) REPRESENTATION_CONTEXT ( 'NONE', 'WORKASPACE' ) );
#12876 = ADVANCED_FACE ( 'NONE', ( #34076 ), #30063, .T. ) ;
#12877 = FACE_OUTER_BOUND ( 'NONE', #8389, .T. ) ;
#12878 = EDGE_LOOP ( 'NONE', ( #24627, #86208, #50770, #28905 ) ) ;
#12879 = CARTESIAN_POINT ( 'NONE',  ( -2.266590686148945544, 42.22041550158063217, 7.082119434687048631 ) ) ;
#12880 = CARTESIAN_POINT ( 'NONE',  ( -7.079903288604985079, -69.52484394646408816, -2.500000000000000000 ) ) ;
#12881 = CARTESIAN_POINT ( 'NONE',  ( -0.8801773607111009756, 13.06368534415483929, 1.068504757029289695E-15 ) ) ;
#12882 = CARTESIAN_POINT ( 'NONE',  ( -2.816281873526473856, 39.33196800326374643, 3.434112377981055619 ) ) ;
#12883 =( BOUNDED_CURVE ( )  B_SPLINE_CURVE ( 2, ( #21278, #13274, #64048, #68755, #17110, #37773, #2614, #68270, #53247 ),
 .UNSPECIFIED., .F., .T. ) 
 B_SPLINE_CURVE_WITH_KNOTS ( ( 3, 2, 2, 2, 3 ),
 ( 0.1901409369402313476, 0.1904761904761904656, 0.1964285714285713969, 0.2023809523809524391, 0.2027162059169115571 ),
 .UNSPECIFIED. ) 
 CURVE ( )  GEOMETRIC_REPRESENTATION_ITEM ( )  RATIONAL_B_SPLINE_CURVE ( ( 0.9963778908391762723, 0.9980808541467921513, 1.000000000000000000, 0.9659258262890683122, 1.000000000000000000, 0.9659258262890683122, 1.000000000000000000, 0.9980808541467921513, 0.9963778908391762723 ) ) 
 REPRESENTATION_ITEM ( '' )  );
#12884 = ADVANCED_FACE ( 'NONE', ( #95080 ), #64079, .F. ) ;
#12885 = CARTESIAN_POINT ( 'NONE',  ( 12.91533473730992121, 9.522018677488171434, 10.88017736071110164 ) ) ;
#12886 = AXIS2_PLACEMENT_3D ( 'NONE', #8363, #24851, #55333 ) ;
#12887 = CARTESIAN_POINT ( 'NONE',  ( 6.565887622018943937, 23.08196800326375708, -12.81628187352647608 ) ) ;
#12888 = CARTESIAN_POINT ( 'NONE',  ( -3.715841784917612856, 15.00000000000000000, -15.55859621770273193 ) ) ;
#12889 = ORIENTED_EDGE ( 'NONE', *, *, #6776, .F. ) ;
#12890 = CARTESIAN_POINT ( 'NONE',  ( 6.935087012957517949, -80.58470470491535309, -3.750000000000000000 ) ) ;
#12891 = AXIS2_PLACEMENT_3D ( 'NONE', #27041, #42546, #4564 ) ;
#12892 = CARTESIAN_POINT ( 'NONE',  ( -45.94000000000000483, 92.50000000000000000, 9.500000000000000000 ) ) ;
#12893 = CARTESIAN_POINT ( 'NONE',  ( -0.3689425029237898834, 6.178748834913968757, -10.36894250292378850 ) ) ;
#12894 = CARTESIAN_POINT ( 'NONE',  ( -3.750000000000000888, 1.019547802438465212, 4.000000000000000000 ) ) ;
#12895 = CARTESIAN_POINT ( 'NONE',  ( 2.035157376598822676, 27.43868534415483396, -7.964842623401177768 ) ) ;
#12896 = CARTESIAN_POINT ( 'NONE',  ( 5.500000000000000000, 61.00000000000000711, 5.000000000000000000 ) ) ;
#12897 = CARTESIAN_POINT ( 'NONE',  ( 14.47650479471819551, 15.00000000000000000, 3.928206833722108549 ) ) ;
#12898 = CARTESIAN_POINT ( 'NONE',  ( -0.8801773607111008646, 53.27201867748816966, 2.915334737309923430 ) ) ;
#12899 = CARTESIAN_POINT ( 'NONE',  ( 20.88017736071110164, 45.35535201082149115, 2.915334737309930979 ) ) ;
#12900 = CARTESIAN_POINT ( 'NONE',  ( 21.09922568453594849, 11.20696800326375531, 6.408140936763242479 ) ) ;
#12901 = CARTESIAN_POINT ( 'NONE',  ( 0.000000000000000000, 14.49999999999999822, 0.000000000000000000 ) ) ;
#12902 = FACE_OUTER_BOUND ( 'NONE', #40109, .T. ) ;
#12903 = CARTESIAN_POINT ( 'NONE',  ( 19.84674366389459266, 28.30059781766745886, 2.638427012816836559 ) ) ;
#12904 = VECTOR ( 'NONE', #23179, 1000.000000000000000 ) ;
#12905 = CARTESIAN_POINT ( 'NONE',  ( -7.750000000000000000, 41.24999999999999289, 6.250000000000000000 ) ) ;
#12906 = CARTESIAN_POINT ( 'NONE',  ( 2.035157376598822676, 42.43868534415483396, -7.964842623401177768 ) ) ;
#12907 = CARTESIAN_POINT ( 'NONE',  ( -1.099225684535947600, 9.540301336597087456, 6.408140936763237150 ) ) ;
#12908 = CARTESIAN_POINT ( 'NONE',  ( 5.076628168052703671, 1.842264484334118047, 8.527530157486179263 ) ) ;
#12909 = CARTESIAN_POINT ( 'NONE',  ( 17.20831665107776587, 24.13393115100078035, -7.208316651077762316 ) ) ;
#12910 = CARTESIAN_POINT ( 'NONE',  ( -1.099225684535947600, 48.70696800326375353, -6.408140936763238038 ) ) ;
#12911 = CARTESIAN_POINT ( 'NONE',  ( 7.361572987183170547, 2.050597817667451750, 9.846743663894590881 ) ) ;
#12912 = VERTEX_POINT ( 'NONE', #42583 ) ;
#12913 = CARTESIAN_POINT ( 'NONE',  ( 0.000000000000000000, 0.5000000000000004441, 0.000000000000000000 ) ) ;
#12914 = CARTESIAN_POINT ( 'NONE',  ( -11.96291822454885612, 15.00000000000000000, 8.193813980848972278 ) ) ;
#12915 = CARTESIAN_POINT ( 'NONE',  ( 20.88017736071110164, 25.35535201082150891, 2.915334737309930979 ) ) ;
#12917 = CARTESIAN_POINT ( 'NONE',  ( -4.164238869374099039, 31.80374883491396432, 8.674139862899312516E-16 ) ) ;
#12916 = CARTESIAN_POINT ( 'NONE',  ( 19.50000000000000711, 98.59912998021083297, -4.500000000000000888 ) ) ;
#12918 = CARTESIAN_POINT ( 'NONE',  ( 2.791683348922240793, 26.63393115100078745, 7.208316651077764092 ) ) ;
#12919 = CARTESIAN_POINT ( 'NONE',  ( 20.88017736071110519, 20.56368534415484106, 2.639326808657452039E-16 ) ) ;
#12920 = CARTESIAN_POINT ( 'NONE',  ( 7.084665262690076126, 9.105352010821503583, 10.88017736071109987 ) ) ;
#12921 = ORIENTED_EDGE ( 'NONE', *, *, #10931, .T. ) ;
#12922 = AXIS2_PLACEMENT_3D ( 'NONE', #87531, #10070, #26057 ) ;
#12923 = CARTESIAN_POINT ( 'NONE',  ( -0.8801773607111008646, 33.27201867748817676, 2.915334737309923430 ) ) ;
#12924 = ADVANCED_FACE ( 'NONE', ( #65560 ), #56605, .F. ) ;
#12925 = CARTESIAN_POINT ( 'NONE',  ( -0.8801773607111009756, 33.06368534415484106, 1.068504757029289695E-15 ) ) ;
#12927 = CARTESIAN_POINT ( 'NONE',  ( -0.8801773607111008646, 43.27201867748817676, 2.915334737309923430 ) ) ;
#12926 = CARTESIAN_POINT ( 'NONE',  ( -13.74385066382875920, 0.2306972965111898921, -5.860428621090559176 ) ) ;
#12928 = ORIENTED_EDGE ( 'NONE', *, *, #88860, .T. ) ;
#12929 = CARTESIAN_POINT ( 'NONE',  ( 21.92686044187657046, 10.16212336850780673, 4.562052436263912550E-16 ) ) ;
#12930 = CARTESIAN_POINT ( 'NONE',  ( 20.88017736071110519, 40.56368534415484106, 2.639326808657452039E-16 ) ) ;
#12931 = DIRECTION ( 'NONE',  ( 1.224646799147353207E-16, 1.000000000000000000, 0.000000000000000000 ) ) ;
#12932 = CIRCLE ( 'NONE', #96024, 14.49999999999999822 ) ;
#12933 = CARTESIAN_POINT ( 'NONE',  ( 14.16722289976685012, 0.5000000000000004441, -4.928467845925517565 ) ) ;
#12934 = CARTESIAN_POINT ( 'NONE',  ( 3.591859063236763294, 63.29030133659708923, -11.09922568453595026 ) ) ;
#12935 = CARTESIAN_POINT ( 'NONE',  ( 8.979999999999991545, 21.00000000000000000, -3.000000000000000000 ) ) ;
#12936 = CARTESIAN_POINT ( 'NONE',  ( 22.26659068614895176, 34.72041550158063927, -7.082119434687042414 ) ) ;
#12937 = CARTESIAN_POINT ( 'NONE',  ( 12.91533473730992121, 54.52201867748816255, 10.88017736071110164 ) ) ;
#12938 = CARTESIAN_POINT ( 'NONE',  ( 18.00000000000000355, 77.07179676972445748, 4.250000000000000000 ) ) ;
#12939 = CARTESIAN_POINT ( 'NONE',  ( 8.502721643904001425, 14.95037103750703622, 12.05657636697107904 ) ) ;
#12940 = CARTESIAN_POINT ( 'NONE',  ( 12.63842701281683034, 47.46726448433412315, 9.846743663894596210 ) ) ;
#12941 = EDGE_LOOP ( 'NONE', ( #73568, #50893, #81148 ) ) ;
#12942 = CARTESIAN_POINT ( 'NONE',  ( 1.472469842513823179, 20.59226448433411960, -4.923371831947296329 ) ) ;
#12943 = CARTESIAN_POINT ( 'NONE',  ( 11.09922568453594671, -12.95969866340290721, -6.408140936763241591 ) ) ;
#12944 = CARTESIAN_POINT ( 'NONE',  ( 0.5774900079438590739, 12.64701867748817143, -5.440088680355550821 ) ) ;
#12945 = CARTESIAN_POINT ( 'NONE',  ( 1.472469842513823179, 31.42559781766745530, 4.923371831947296329 ) ) ;
#12946 = CARTESIAN_POINT ( 'NONE',  ( 19.38216949554541557, 7.248634669930421381, -9.382169495545420901 ) ) ;
#12947 = CARTESIAN_POINT ( 'NONE',  ( 20.88017736071110519, 60.56368534415484106, 2.639326808657452039E-16 ) ) ;
#12949 = CARTESIAN_POINT ( 'NONE',  ( 3.591859063236761518, 54.95696800326376064, 11.09922568453594849 ) ) ;
#12948 = CARTESIAN_POINT ( 'NONE',  ( 4.559911319644449179, 27.23035201082150536, -9.422509992056141925 ) ) ;
#12950 = CARTESIAN_POINT ( 'NONE',  ( 17.08211943468705840, 45.13708216824730357, -12.26659068614894466 ) ) ;
#12951 = TOROIDAL_SURFACE ( 'NONE', #28930, 14.49999999999999822, 0.5000000000000000000 ) ;
#12952 = CARTESIAN_POINT ( 'NONE',  ( -13.34343830728411184, 0.3639313252796100850, 6.852200678592532235 ) ) ;
#12953 = VERTEX_POINT ( 'NONE', #27568 ) ;
#12954 = CARTESIAN_POINT ( 'NONE',  ( 0.6178305044545818747, -1.501365330069579951, -9.382169495545419124 ) ) ;
#12955 = CARTESIAN_POINT ( 'NONE',  ( 10.00000000000000178, 4.313685344154837509, 10.88017736071110342 ) ) ;
#12956 = CARTESIAN_POINT ( 'NONE',  ( 4.559911319644449179, 48.89701867748817676, 9.422509992056141925 ) ) ;
#12957 = AXIS2_PLACEMENT_3D ( 'NONE', #7529, #97547, #52996 ) ;
#12958 = CARTESIAN_POINT ( 'NONE',  ( 0.1532563361054100626, 60.80059781766744464, -2.638427012816831230 ) ) ;
#12959 = ORIENTED_EDGE ( 'NONE', *, *, #84150, .F. ) ;
#12960 = CARTESIAN_POINT ( 'NONE',  ( 7.361572987183170547, 17.05059781766745530, 9.846743663894590881 ) ) ;
#12961 = CARTESIAN_POINT ( 'NONE',  ( 5.076628168052704559, 10.17559781766745175, -8.527530157486179263 ) ) ;
#12962 = CARTESIAN_POINT ( 'NONE',  ( 1.472469842513823179, 36.42559781766745175, 4.923371831947296329 ) ) ;
#12963 = CARTESIAN_POINT ( 'NONE',  ( 2.791683348922240793, 6.633931151000785675, 7.208316651077764092 ) ) ;
#12964 = B_SPLINE_CURVE_WITH_KNOTS ( 'NONE', 3,
 ( #10246, #70758, #85752, #69764, #17750, #31746 ),
 .UNSPECIFIED., .F., .F.,
 ( 4, 2, 4 ),
 ( 0.0002800267093086770119, 0.0006862322000164198209, 0.001092437690724162467 ),
 .UNSPECIFIED. ) ;
#12965 = CARTESIAN_POINT ( 'NONE',  ( 5.076628168052704559, 20.17559781766745175, -8.527530157486179263 ) ) ;
#12966 = CARTESIAN_POINT ( 'NONE',  ( -6.356892395138682872, -50.94284410517786910, 2.500000000000000000 ) ) ;
#12967 = EDGE_CURVE ( 'NONE', #64078, #85989, #57573, .T. ) ;
#12969 = LINE ( 'NONE', #73964, #11620 ) ;
#12968 = CARTESIAN_POINT ( 'NONE',  ( 12.63842701281683034, 2.467264484334118269, 9.846743663894596210 ) ) ;
#12970 = CARTESIAN_POINT ( 'NONE',  ( 2.791683348922237240, 10.38393115100078390, -7.208316651077763204 ) ) ;
#12972 = ORIENTED_EDGE ( 'NONE', *, *, #27212, .F. ) ;
#12971 = CARTESIAN_POINT ( 'NONE',  ( 19.84674366389459266, 13.71726448433411782, -2.638427012816827677 ) ) ;
#12973 = CARTESIAN_POINT ( 'NONE',  ( 0.1034006766821532752, 4.444999227851523509E-16, 14.49963131600461175 ) ) ;
#12974 = CARTESIAN_POINT ( 'NONE',  ( 10.00000000000000000, 2.873634669930420049, -12.81628187352647608 ) ) ;
#12975 =( NAMED_UNIT ( * ) SI_UNIT ( $, .STERADIAN. ) SOLID_ANGLE_UNIT ( ) );
#12976 = CARTESIAN_POINT ( 'NONE',  ( 22.26659068614895176, 19.72041550158063572, -7.082119434687042414 ) ) ;
#12977 = CARTESIAN_POINT ( 'NONE',  ( 2.962741594153077251, -0.03417435944610275333, -13.93860331045673107 ) ) ;
#12978 = CARTESIAN_POINT ( 'NONE',  ( -0.3689425029237881626, 12.42874883491396609, 10.36894250292379027 ) ) ;
#12979 = CARTESIAN_POINT ( 'NONE',  ( -0.3689425029237898834, 46.17874883491397497, -10.36894250292378850 ) ) ;
#12980 = SURFACE_STYLE_USAGE ( .BOTH. , #27981 ) ;
#12982 = CARTESIAN_POINT ( 'NONE',  ( 10.00000000000000000, 66.81368534415484817, -10.88017736071110342 ) ) ;
#12981 = CARTESIAN_POINT ( 'NONE',  ( 6.204703633549690345, 7.845415501580634832, 14.16423886937410082 ) ) ;
#12983 = CARTESIAN_POINT ( 'NONE',  ( -0.8801773607111009756, 28.06368534415484106, 1.068504757029289695E-15 ) ) ;
#12984 = FACE_OUTER_BOUND ( 'NONE', #76552, .T. ) ;
#12985 = VERTEX_POINT ( 'NONE', #14937 ) ;
#12986 = CARTESIAN_POINT ( 'NONE',  ( 2.791683348922237240, 25.38393115100078390, -7.208316651077763204 ) ) ;
#12988 = CARTESIAN_POINT ( 'NONE',  ( 1.472469842513823179, 31.42559781766745530, 4.923371831947296329 ) ) ;
#12987 = CARTESIAN_POINT ( 'NONE',  ( 4.559911319644449179, 53.89701867748817676, 9.422509992056141925 ) ) ;
#12989 = CARTESIAN_POINT ( 'NONE',  ( 12.91533473730992121, 4.522018677488170546, 10.88017736071110164 ) ) ;
#12990 = CARTESIAN_POINT ( 'NONE',  ( 16.40814093676324603, 57.45696800326375353, -11.09922568453594671 ) ) ;
#12991 = CARTESIAN_POINT ( 'NONE',  ( 7.361572987183169658, 49.96726448433410894, -9.846743663894592657 ) ) ;
#12992 = CYLINDRICAL_SURFACE ( 'NONE', #13910, 0.2500000000000002220 ) ;
#12993 = CARTESIAN_POINT ( 'NONE',  ( 0.6178305044545818747, 43.49863466993042493, -9.382169495545419124 ) ) ;
#12994 = CARTESIAN_POINT ( 'NONE',  ( 3.469446951953614189E-15, -21.94625116508602858, 14.16423886937410259 ) ) ;
#12995 = CARTESIAN_POINT ( 'NONE',  ( 2.035157376598824452, 48.68868534415483396, 7.964842623401179544 ) ) ;
#12996 = CARTESIAN_POINT ( 'NONE',  ( 19.84674366389459266, 38.30059781766745175, 2.638427012816836559 ) ) ;
#12997 = CIRCLE ( 'NONE', #48117, 0.2500000000000002220 ) ;
#12998 = CARTESIAN_POINT ( 'NONE',  ( 6.204703633549690345, 20.76208216824730357, -14.16423886937410259 ) ) ;
#12999 = EDGE_CURVE ( 'NONE', #32841, #15068, #1348, .T. ) ;
#13000 = ORIENTED_EDGE ( 'NONE', *, *, #4764, .T. ) ;
#13001 = CARTESIAN_POINT ( 'NONE',  ( 13.79529636645030344, 3.262082168247301350, 14.16423886937410614 ) ) ;
#13002 = CARTESIAN_POINT ( 'NONE',  ( 15.44008868035555793, 56.39701867748817676, -9.422509992056140149 ) ) ;
#13003 = CARTESIAN_POINT ( 'NONE',  ( 4.559911319644449179, 62.23035201082150536, -9.422509992056141925 ) ) ;
#13004 = CARTESIAN_POINT ( 'NONE',  ( 10.00000000000000178, 48.05374883491396787, 14.16423886937410082 ) ) ;
#13005 = CARTESIAN_POINT ( 'NONE',  ( 22.81628187352648496, 1.831968003263753753, -3.434112377981050290 ) ) ;
#13006 = CARTESIAN_POINT ( 'NONE',  ( 66.56412365047464164, 26.99999999999998224, 9.500000000000000000 ) ) ;
#13007 = CARTESIAN_POINT ( 'NONE',  ( 19.42250999205614193, 60.14701867748817676, 5.440088680355555262 ) ) ;
#13008 = DIRECTION ( 'NONE',  ( 1.000000000000000000, 0.000000000000000000, 0.000000000000000000 ) ) ;
#13009 = CARTESIAN_POINT ( 'NONE',  ( -2.816281873526473856, 24.12363466993042138, 9.499525473075851096E-16 ) ) ;
#13010 = CARTESIAN_POINT ( 'NONE',  ( 14.92337183194729633, 52.67559781766745175, 8.527530157486181039 ) ) ;
#13011 = CARTESIAN_POINT ( 'NONE',  ( -7.964842623401172439, 18.68868534415485172, 7.964842623401183097 ) ) ;
#13012 =( NAMED_UNIT ( * ) PLANE_ANGLE_UNIT ( ) SI_UNIT ( $, .RADIAN. ) );
#13013 = CARTESIAN_POINT ( 'NONE',  ( 0.5774900079438607392, 8.480352010821505360, 5.440088680355550821 ) ) ;
#13014 = CARTESIAN_POINT ( 'NONE',  ( -3.750000000000000000, 36.75000000000000000, -2.500000000000000000 ) ) ;
#13015 = EDGE_LOOP ( 'NONE', ( #32019, #87831, #74247, #2168 ) ) ;
#13016 = CARTESIAN_POINT ( 'NONE',  ( 15.44008868035555793, 6.397018677488170546, -9.422509992056140149 ) ) ;
#13017 =( LENGTH_UNIT ( ) NAMED_UNIT ( * ) SI_UNIT ( .MILLI., .METRE. ) );
#13018 = CARTESIAN_POINT ( 'NONE',  ( 10.00000000000000000, 61.81368534415484106, -10.88017736071110342 ) ) ;
#13019 = CIRCLE ( 'NONE', #92885, 14.49999999999999822 ) ;
#13020 = CARTESIAN_POINT ( 'NONE',  ( 1.472469842513823179, 1.425597817667451528, 4.923371831947296329 ) ) ;
#13021 = CIRCLE ( 'NONE', #16252, 0.4999999999999993894 ) ;
#13023 = B_SPLINE_CURVE_WITH_KNOTS ( 'NONE', 3,
 ( #18573, #72055, #34531, #17598 ),
 .UNSPECIFIED., .F., .F.,
 ( 4, 4 ),
 ( 1.571840398521015072E-16, 0.001060528352561993307 ),
 .UNSPECIFIED. ) ;
#13022 = CARTESIAN_POINT ( 'NONE',  ( 17.20831665107776587, 34.13393115100078745, -7.208316651077762316 ) ) ;
#13024 = CARTESIAN_POINT ( 'NONE',  ( 20.88017736071110164, 40.35535201082150536, 2.915334737309930979 ) ) ;
#13025 = CARTESIAN_POINT ( 'NONE',  ( 0.6178305044545818747, 13.49863466993041783, -9.382169495545419124 ) ) ;
#13027 = DIRECTION ( 'NONE',  ( 0.000000000000000000, -1.000000000000000000, -2.602085213965208275E-15 ) ) ;
#13026 = CARTESIAN_POINT ( 'NONE',  ( 19.42250999205614193, 40.14701867748817676, 5.440088680355555262 ) ) ;
#13028 = CARTESIAN_POINT ( 'NONE',  ( -8.000000000000000000, 79.82179676972448590, -6.250000000000000000 ) ) ;
#13029 = COLOUR_RGB ( '', 0.40784314, 0.44705882, 0.49803922) ;
#13030 = CARTESIAN_POINT ( 'NONE',  ( 6.565887622018943937, 43.08196800326374643, -12.81628187352647608 ) ) ;
#13031 = VERTEX_POINT ( 'NONE', #68915 ) ;
#13032 = CARTESIAN_POINT ( 'NONE',  ( 10.00000000000000178, 64.31368534415483396, 10.88017736071110342 ) ) ;
#13033 = CARTESIAN_POINT ( 'NONE',  ( 13.43411237798106583, 27.66530133659708568, -12.81628187352647252 ) ) ;
#13034 = CARTESIAN_POINT ( 'NONE',  ( 17.96484262340118221, 41.18868534415484106, -7.964842623401177768 ) ) ;
#13035 = CARTESIAN_POINT ( 'NONE',  ( 0.1532563361054100626, 65.80059781766745175, -2.638427012816831230 ) ) ;
#13036 = CARTESIAN_POINT ( 'NONE',  ( -4.164238869374099927, 62.01208216824728936, 3.795296366450308767 ) ) ;
#13037 = CARTESIAN_POINT ( 'NONE',  ( 5.076628168052703671, 56.84226448433412315, 8.527530157486179263 ) ) ;
#13038 = CARTESIAN_POINT ( 'NONE',  ( 4.559911319644449179, 68.89701867748817676, 9.422509992056141925 ) ) ;
#13039 = EDGE_CURVE ( 'NONE', #29252, #23929, #23424, .T. ) ;
#13040 = CARTESIAN_POINT ( 'NONE',  ( 12.91533473730992121, 64.52201867748817676, 10.88017736071110164 ) ) ;
#13041 = DIRECTION ( 'NONE',  ( -1.000000000000000000, 0.000000000000000000, 0.000000000000000000 ) ) ;
#13042 = CARTESIAN_POINT ( 'NONE',  ( -2.266590686148945544, 26.38708216824730357, -7.082119434687050408 ) ) ;
#13043 = PRESENTATION_LAYER_ASSIGNMENT (  '', '', ( #22697 ) ) ;
#13044 = EDGE_CURVE ( 'NONE', #51389, #21190, #84343, .T. ) ;
#13045 =( NAMED_UNIT ( * ) SI_UNIT ( $, .STERADIAN. ) SOLID_ANGLE_UNIT ( ) );
#13046 = PRESENTATION_STYLE_ASSIGNMENT (( #35044 ) ) ;
#13047 = VERTEX_POINT ( 'NONE', #14439 ) ;
#13048 = CARTESIAN_POINT ( 'NONE',  ( 6.204703633549690345, 65.76208216824731778, -14.16423886937410259 ) ) ;
#13049 = CARTESIAN_POINT ( 'NONE',  ( 7.084665262690076126, 2.022018677488171434, -10.88017736071110164 ) ) ;
#13050 = CARTESIAN_POINT ( 'NONE',  ( 14.92337183194729633, 32.67559781766745175, 8.527530157486181039 ) ) ;
#13051 = CARTESIAN_POINT ( 'NONE',  ( -1.099225684535947600, 29.54030133659708923, 6.408140936763237150 ) ) ;
#13052 = SURFACE_SIDE_STYLE ('',( #51554 ) ) ;
#13053 = DIRECTION ( 'NONE',  ( -0.8870108331782244893, 0.000000000000000000, 0.4617486132350284711 ) ) ;
#13054 = CARTESIAN_POINT ( 'NONE',  ( 20.88017736071110875, 10.77201867748817143, -2.915334737309920765 ) ) ;
#13055 = CARTESIAN_POINT ( 'NONE',  ( 20.36894250292379382, 58.67874883491396076, 10.36894250292379205 ) ) ;
#13056 = CARTESIAN_POINT ( 'NONE',  ( 12.63842701281683034, 27.46726448433411250, 9.846743663894596210 ) ) ;
#13057 = CARTESIAN_POINT ( 'NONE',  ( 20.15039907845753220, 19.72266099184918886, 6.262539305110075283 ) ) ;
#13058 = CARTESIAN_POINT ( 'NONE',  ( 19.84674366389459621, 13.50893115100078568, 7.409399052514197653E-17 ) ) ;
#13059 = EDGE_CURVE ( 'NONE', #98886, #87109, #49593, .T. ) ;
#13060 = CARTESIAN_POINT ( 'NONE',  ( 18.06765999051783567, 58.99127512925446837, 6.500000000000043521 ) ) ;
#13061 = CARTESIAN_POINT ( 'NONE',  ( -9.846743663894590881, 11.21726448433411605, 2.638427012816840111 ) ) ;
#13062 = VERTEX_POINT ( 'NONE', #59914 ) ;
#13063 = ORIENTED_EDGE ( 'NONE', *, *, #27562, .F. ) ;
#13064 = VERTEX_POINT ( 'NONE', #98944 ) ;
#13065 = CARTESIAN_POINT ( 'NONE',  ( 17.08211943468705840, 20.13708216824730357, -12.26659068614894466 ) ) ;
#13067 = CARTESIAN_POINT ( 'NONE',  ( 10.00000000000000178, 19.31368534415484106, 10.88017736071110342 ) ) ;
#13066 = CARTESIAN_POINT ( 'NONE',  ( 12.91533473730992121, 24.52201867748816966, 10.88017736071110164 ) ) ;
#13069 = CARTESIAN_POINT ( 'NONE',  ( 13.43411237798106583, 12.66530133659708746, -12.81628187352647252 ) ) ;
#13068 = CARTESIAN_POINT ( 'NONE',  ( 18.52753015748618282, 43.92559781766745175, -4.923371831947291888 ) ) ;
#13070 = CARTESIAN_POINT ( 'NONE',  ( 2.917880565312950480, 10.97041550158063572, -12.26659068614894821 ) ) ;
#13071 = CARTESIAN_POINT ( 'NONE',  ( 18.52753015748618282, 43.92559781766745175, -4.923371831947291888 ) ) ;
#13072 = AXIS2_PLACEMENT_3D ( 'NONE', #2266, #94712, #55230 ) ;
#13073 = CARTESIAN_POINT ( 'NONE',  ( -1.099225684535947600, 29.54030133659708923, 6.408140936763237150 ) ) ;
#13075 = VERTEX_POINT ( 'NONE', #68421 ) ;
#13074 = CARTESIAN_POINT ( 'NONE',  ( 0.1532563361054082862, 1.217264484334117824, 2.638427012816831674 ) ) ;
#13076 = CARTESIAN_POINT ( 'NONE',  ( 10.00000000000000000, 29.75893115100078745, -9.846743663894594434 ) ) ;
#13077 = CARTESIAN_POINT ( 'NONE',  ( 20.36894250292379738, 54.92874883491396076, -10.36894250292379027 ) ) ;
#13078 = EDGE_LOOP ( 'NONE', ( #50318, #15577, #90776, #94491 ) ) ;
#13079 = CARTESIAN_POINT ( 'NONE',  ( 17.96484262340118221, 6.188685344154837509, -7.964842623401177768 ) ) ;
#13080 = ORIENTED_EDGE ( 'NONE', *, *, #16997, .F. ) ;
#13081 = CARTESIAN_POINT ( 'NONE',  ( 0.5774900079438607392, 43.48035201082151247, 5.440088680355550821 ) ) ;
#13082 = CARTESIAN_POINT ( 'NONE',  ( 7.084665262690076126, 49.10535201082149825, 10.88017736071109987 ) ) ;
#13083 = CARTESIAN_POINT ( 'NONE',  ( 20.88017736071110164, 50.35535201082151247, 2.915334737309930979 ) ) ;
#13084 = CARTESIAN_POINT ( 'NONE',  ( 2.035157376598822676, 42.43868534415483396, -7.964842623401177768 ) ) ;
#13085 = CARTESIAN_POINT ( 'NONE',  ( 1.175527996597151903, 2.337810934421868936E-16, -14.57931687975703205 ) ) ;
#13086 = EDGE_CURVE ( 'NONE', #42611, #56730, #20457, .T. ) ;
#13089 = ORIENTED_EDGE ( 'NONE', *, *, #48770, .F. ) ;
#13088 = AXIS2_PLACEMENT_3D ( 'NONE', #97950, #22927, #75908 ) ;
#13087 =( LENGTH_UNIT ( ) NAMED_UNIT ( * ) SI_UNIT ( .MILLI., .METRE. ) );
#13090 = VECTOR ( 'NONE', #77288, 1000.000000000000000 ) ;
#13091 = CARTESIAN_POINT ( 'NONE',  ( 18.52753015748618282, 33.92559781766745886, -4.923371831947291888 ) ) ;
#13092 = VERTEX_POINT ( 'NONE', #30398 ) ;
#13093 = CARTESIAN_POINT ( 'NONE',  ( 12.63842701281683922, 54.55059781766745175, -9.846743663894590881 ) ) ;
#13094 = EDGE_CURVE ( 'NONE', #26759, #17506, #55647, .T. ) ;
#13095 = CARTESIAN_POINT ( 'NONE',  ( 14.47650479471823637, 14.63595249122792907, -3.928206833722017510 ) ) ;
#13096 = AXIS2_PLACEMENT_3D ( 'NONE', #58310, #52310, #82802 ) ;
#13097 = AXIS2_PLACEMENT_3D ( 'NONE', #45527, #60028, #84028 ) ;
#13098 = CARTESIAN_POINT ( 'NONE',  ( -0.3689425029237881626, 2.428748834913967869, 10.36894250292379027 ) ) ;
#13099 = CARTESIAN_POINT ( 'NONE',  ( -10.15753629091561550, 13.12143304556736112, 6.250710446193390446 ) ) ;
#13100 = CARTESIAN_POINT ( 'NONE',  ( -42.50369195530267774, 107.9060299417078426, 4.500000000000000888 ) ) ;
#13101 = CARTESIAN_POINT ( 'NONE',  ( 0.000000000000000000, 14.49999999999999822, 0.000000000000000000 ) ) ;
#13102 = CARTESIAN_POINT ( 'NONE',  ( 22.26659068614894466, 63.88708216824730357, 7.082119434687054849 ) ) ;
#13103 = CARTESIAN_POINT ( 'NONE',  ( 13.82192141328812518, 4.718101003023380916E-16, -4.382292601468683380 ) ) ;
#13104 = ORIENTED_EDGE ( 'NONE', *, *, #11453, .F. ) ;
#13106 = TOROIDAL_SURFACE ( 'NONE', #64202, 14.49999999999999822, 0.5000000000000000000 ) ;
#13105 = CARTESIAN_POINT ( 'NONE',  ( 14.03351048042395632, 0.000000000000000000, 2.474486531753810059 ) ) ;
#13107 = CARTESIAN_POINT ( 'NONE',  ( 2.791683348922240793, 41.63393115100078745, 7.208316651077764092 ) ) ;
#13108 = LINE ( 'NONE', #21615, #21163 ) ;
#13109 = CARTESIAN_POINT ( 'NONE',  ( -1.099225684535947600, 18.70696800326375353, -6.408140936763238038 ) ) ;
#13110 = CARTESIAN_POINT ( 'NONE',  ( 0.1532563361054100626, 15.80059781766745353, -2.638427012816831230 ) ) ;
#13111 = CARTESIAN_POINT ( 'NONE',  ( 8.880000000000020322, 80.07179676972448590, 6.250000000000000000 ) ) ;
#13112 = CARTESIAN_POINT ( 'NONE',  ( 14.92337183194729633, 12.67559781766745353, 8.527530157486181039 ) ) ;
#13113 = CARTESIAN_POINT ( 'NONE',  ( 0.6178305044545818747, -1.501365330069579951, -9.382169495545419124 ) ) ;
#13114 = DIRECTION ( 'NONE',  ( 0.000000000000000000, 1.000000000000000000, 0.000000000000000000 ) ) ;
#13115 = ADVANCED_FACE ( 'NONE', ( #29905 ), #3734, .T. ) ;
#13116 = VERTEX_POINT ( 'NONE', #31172 ) ;
#13117 = CARTESIAN_POINT ( 'NONE',  ( 7.084665262690076126, 14.10535201082150358, 10.88017736071109987 ) ) ;
#13118 = CARTESIAN_POINT ( 'NONE',  ( -4.164238869374099039, 6.803748834913967869, 8.674139862899312516E-16 ) ) ;
#13119 = CARTESIAN_POINT ( 'NONE',  ( 0.1532563361054100626, 25.80059781766744820, -2.638427012816831230 ) ) ;
#13120 = CARTESIAN_POINT ( 'NONE',  ( 0.5774900079438590739, 52.64701867748817676, -5.440088680355550821 ) ) ;
#13122 = CARTESIAN_POINT ( 'NONE',  ( -3.500000000000000444, 1.019547802438453887, -3.750000000000000000 ) ) ;
#13121 = CARTESIAN_POINT ( 'NONE',  ( 6.565887622018943937, 33.08196800326374643, -12.81628187352647608 ) ) ;
#13123 = EDGE_CURVE ( 'NONE', #37045, #83910, #16190, .T. ) ;
#13124 = CYLINDRICAL_SURFACE ( 'NONE', #46921, 0.1000000000000000333 ) ;
#13125 = CARTESIAN_POINT ( 'NONE',  ( 13.43411237798105340, 0.5819680032637533085, 12.81628187352647963 ) ) ;
#13126 = CARTESIAN_POINT ( 'NONE',  ( 7.361572987183170547, 62.05059781766745886, 9.846743663894590881 ) ) ;
#13127 = CARTESIAN_POINT ( 'NONE',  ( 10.00000000000000000, 19.75893115100078390, -9.846743663894594434 ) ) ;
#13128 = CARTESIAN_POINT ( 'NONE',  ( 7.964842623401177768, -23.81131465584515539, -7.964842623401181321 ) ) ;
#13129 = CARTESIAN_POINT ( 'NONE',  ( 16.40814093676324603, 27.45696800326375708, -11.09922568453594671 ) ) ;
#13130 = CARTESIAN_POINT ( 'NONE',  ( -10.77730536144846596, -98.63085534186639336, -3.749999999999994671 ) ) ;
#13131 = CARTESIAN_POINT ( 'NONE',  ( 17.96484262340118221, 44.93868534415483396, 7.964842623401181321 ) ) ;
#13132 = DIRECTION ( 'NONE',  ( -0.000000000000000000, 1.000000000000000000, -0.000000000000000000 ) ) ;
#13133 =( BOUNDED_CURVE ( )  B_SPLINE_CURVE ( 2, ( #97082, #28553, #13553, #57564, #44039, #97570, #29033, #27065, #50071 ),
 .UNSPECIFIED., .F., .T. ) 
 B_SPLINE_CURVE_WITH_KNOTS ( ( 3, 2, 2, 2, 3 ),
 ( 0.3687123655116599230, 0.3690476190476190688, 0.3750000000000000000, 0.3809523809523809312, 0.3812876344883400770 ),
 .UNSPECIFIED. ) 
 CURVE ( )  GEOMETRIC_REPRESENTATION_ITEM ( )  RATIONAL_B_SPLINE_CURVE ( ( 0.9963778908391760503, 0.9980808541467920403, 1.000000000000000000, 0.9659258262890682012, 1.000000000000000000, 0.9659258262890682012, 1.000000000000000000, 0.9980808541467920403, 0.9963778908391760503 ) ) 
 REPRESENTATION_ITEM ( '' )  );
#13134 = CARTESIAN_POINT ( 'NONE',  ( 4.559911319644449179, 32.23035201082150536, -9.422509992056141925 ) ) ;
#13135 = AXIS2_PLACEMENT_3D ( 'NONE', #95354, #3877, #39899 ) ;
#13136 = CARTESIAN_POINT ( 'NONE',  ( 10.00000000000000178, 52.25893115100078745, 9.846743663894594434 ) ) ;
#13137 = CARTESIAN_POINT ( 'NONE',  ( 17.96484262340118221, 56.18868534415484817, -7.964842623401177768 ) ) ;
#13138 = CARTESIAN_POINT ( 'NONE',  ( 20.36894250292379738, 34.92874883491396076, -10.36894250292379027 ) ) ;
#13139 = CARTESIAN_POINT ( 'NONE',  ( 5.000000000000000000, -2.909297654740273256E-16, 7.000000000000000000 ) ) ;
#13140 = UNCERTAINTY_MEASURE_WITH_UNIT (LENGTH_MEASURE( 1.000000000000000082E-05 ), #47808, 'distance_accuracy_value', 'NONE');
#13141 =( BOUNDED_CURVE ( )  B_SPLINE_CURVE ( 2, ( #24966, #62939, #53967, #77945, #70455, #30961, #86444, #8470, #61459 ),
 .UNSPECIFIED., .F., .F. ) 
 B_SPLINE_CURVE_WITH_KNOTS ( ( 3, 2, 2, 2, 3 ),
 ( 0.9044266512259456769, 0.9047619047619047672, 0.9107142857142856984, 0.9166666666666667407, 0.9170019202026259419 ),
 .UNSPECIFIED. ) 
 CURVE ( )  GEOMETRIC_REPRESENTATION_ITEM ( )  RATIONAL_B_SPLINE_CURVE ( ( 0.9963778908391764944, 0.9980808541467923733, 1.000000000000000000, 0.9659258262890683122, 1.000000000000000000, 0.9659258262890683122, 1.000000000000000000, 0.9980808541467917072, 0.9963778908391753841 ) ) 
 REPRESENTATION_ITEM ( '' )  );
#13142 = CARTESIAN_POINT ( 'NONE',  ( 17.20831665107776587, 39.13393115100079456, -7.208316651077762316 ) ) ;
#13143 = CARTESIAN_POINT ( 'NONE',  ( 18.52753015748617571, 63.09226448433412315, 4.923371831947298993 ) ) ;
#13144 = ORIENTED_EDGE ( 'NONE', *, *, #81629, .T. ) ;
#13145 = CARTESIAN_POINT ( 'NONE',  ( 2.035157376598822676, 27.43868534415483396, -7.964842623401177768 ) ) ;
#13146 = CARTESIAN_POINT ( 'NONE',  ( 15.44008868035555793, 6.397018677488170546, -9.422509992056140149 ) ) ;
#13147 = CARTESIAN_POINT ( 'NONE',  ( 7.084665262690076126, 9.105352010821503583, 10.88017736071109987 ) ) ;
#13148 = CARTESIAN_POINT ( 'NONE',  ( 1.472469842513823179, 0.5922644843341181575, -4.923371831947296329 ) ) ;
#13149 = CARTESIAN_POINT ( 'NONE',  ( 24.16423886937409904, 19.09541550158063927, 3.795296366450317205 ) ) ;
#13150 = CARTESIAN_POINT ( 'NONE',  ( 5.076628168052704559, 20.17559781766745175, -8.527530157486179263 ) ) ;
#13151 = CARTESIAN_POINT ( 'NONE',  ( 14.92337183194729633, 57.67559781766745886, 8.527530157486181039 ) ) ;
#13152 = CARTESIAN_POINT ( 'NONE',  ( 7.084665262690076126, 39.10535201082150536, 10.88017736071109987 ) ) ;
#13153 = DIRECTION ( 'NONE',  ( 0.000000000000000000, 1.000000000000000000, 0.000000000000000000 ) ) ;
#13154 = DIRECTION ( 'NONE',  ( 0.000000000000000000, 1.000000000000000000, 0.000000000000000000 ) ) ;
#13155 = EDGE_CURVE ( 'NONE', #64180, #86629, #55149, .T. ) ;
#13156 = ORIENTED_EDGE ( 'NONE', *, *, #43233, .T. ) ;
#13157 = VECTOR ( 'NONE', #97414, 1000.000000000000000 ) ;
#13158 = DIRECTION ( 'NONE',  ( -0.000000000000000000, 1.000000000000000000, 0.000000000000000000 ) ) ;
#13159 = CARTESIAN_POINT ( 'NONE',  ( 19.84674366389459266, 43.30059781766744464, 2.638427012816836559 ) ) ;
#13160 = ORIENTED_EDGE ( 'NONE', *, *, #95536, .F. ) ;
#13161 = ORIENTED_EDGE ( 'NONE', *, *, #78495, .F. ) ;
#13162 = CARTESIAN_POINT ( 'NONE',  ( 6.689969769698871360, 15.00000000000000000, 12.58200319823975022 ) ) ;
#13163 = CARTESIAN_POINT ( 'NONE',  ( 10.00000000000000178, 28.05374883491396787, 14.16423886937410082 ) ) ;
#13164 = CARTESIAN_POINT ( 'NONE',  ( -0.3689425029237898834, 11.17874883491396787, -10.36894250292378850 ) ) ;
#13165 = CARTESIAN_POINT ( 'NONE',  ( 20.88017736071110164, 60.35535201082151957, 2.915334737309930979 ) ) ;
#13166 = CARTESIAN_POINT ( 'NONE',  ( 13.79529636645031943, 55.34541550158062506, -14.16423886937409904 ) ) ;
#13167 = CARTESIAN_POINT ( 'NONE',  ( 6.565887622018943937, -1.918031996736246692, -12.81628187352647608 ) ) ;
#13168 = CARTESIAN_POINT ( 'NONE',  ( 19.84674366389459266, 43.30059781766744464, 2.638427012816836559 ) ) ;
#13169 = CARTESIAN_POINT ( 'NONE',  ( -10.77984007350130469, -96.52126437880588128, 4.000000000000000000 ) ) ;
#13171 = CARTESIAN_POINT ( 'NONE',  ( 6.565887622018943937, 5.165301336597086568, 12.81628187352647430 ) ) ;
#13170 = CARTESIAN_POINT ( 'NONE',  ( 15.44008868035555260, 44.73035201082151247, 9.422509992056143702 ) ) ;
#13172 = CARTESIAN_POINT ( 'NONE',  ( -4.164238869374099927, 22.01208216824730357, 3.795296366450308767 ) ) ;
#13173 = CARTESIAN_POINT ( 'NONE',  ( -0.3689425029237881626, 47.42874883491396787, 10.36894250292379027 ) ) ;
#13174 = COLOUR_RGB ( '', 0.08235294, 0.09019608, 0.10196078) ;
#13175 = CARTESIAN_POINT ( 'NONE',  ( 20.88017736071110875, 20.77201867748816611, -2.915334737309920765 ) ) ;
#13176 = CARTESIAN_POINT ( 'NONE',  ( -2.888614318722246832, 2.439454888092384977E-16, -14.33855829812827665 ) ) ;
#13177 = CIRCLE ( 'NONE', #59419, 0.5000000000000004441 ) ;
#13178 = SURFACE_STYLE_FILL_AREA ( #37184 ) ;
#13179 = CARTESIAN_POINT ( 'NONE',  ( 0.5774900079438607392, 43.48035201082151247, 5.440088680355550821 ) ) ;
#13180 = VECTOR ( 'NONE', #36872, 1000.000000000000000 ) ;
#13181 = CARTESIAN_POINT ( 'NONE',  ( -4.923371831947302546, -39.82440218233254825, -8.527530157486173934 ) ) ;
#13182 = ORIENTED_EDGE ( 'NONE', *, *, #8175, .T. ) ;
#13183 = CARTESIAN_POINT ( 'NONE',  ( 19.72487221294570858, 4.782175860852374782, 6.500000000000002665 ) ) ;
#13184 = VECTOR ( 'NONE', #55820, 1000.000000000000000 ) ;
#13185 = EDGE_LOOP ( 'NONE', ( #92107, #29061, #203, #66150, #22609, #18544 ) ) ;
#13186 = VERTEX_POINT ( 'NONE', #8678 ) ;
#13187 = CARTESIAN_POINT ( 'NONE',  ( 2.917880565312950480, 40.97041550158063217, -12.26659068614894821 ) ) ;
#13188 = CARTESIAN_POINT ( 'NONE',  ( 10.00000000000000178, 42.25893115100078745, 9.846743663894594434 ) ) ;
#13189 = CARTESIAN_POINT ( 'NONE',  ( 20.32896413005680358, 49.74545670184114954, 5.963430220938287007 ) ) ;
#13190 = CARTESIAN_POINT ( 'NONE',  ( 0.000000000000000000, 15.00000000000000000, 0.000000000000000000 ) ) ;
#13191 = VECTOR ( 'NONE', #83248, 1000.000000000000227 ) ;
#13192 = CARTESIAN_POINT ( 'NONE',  ( 15.44008868035555260, 59.73035201082151247, 9.422509992056143702 ) ) ;
#13193 = CARTESIAN_POINT ( 'NONE',  ( 19.38216949554541202, 55.99863466993041072, 9.382169495545424454 ) ) ;
#13194 = CARTESIAN_POINT ( 'NONE',  ( 9.382169495545415572, 12.24863466993041961, -9.382169495545422677 ) ) ;
#13195 = ORIENTED_EDGE ( 'NONE', *, *, #21354, .T. ) ;
#13196 = ADVANCED_FACE ( 'NONE', ( #38694 ), #23210, .T. ) ;
#13197 = CARTESIAN_POINT ( 'NONE',  ( 17.08211943468705840, 20.13708216824730357, -12.26659068614894466 ) ) ;
#13198 = EDGE_LOOP ( 'NONE', ( #27813, #38653, #74289, #83034 ) ) ;
#13199 = CARTESIAN_POINT ( 'NONE',  ( 6.565887622018943937, 18.08196800326375708, -12.81628187352647608 ) ) ;
#13200 = ORIENTED_EDGE ( 'NONE', *, *, #91835, .F. ) ;
#13201 = PRESENTATION_LAYER_ASSIGNMENT (  '', '', ( #67533 ) ) ;
#13202 = CARTESIAN_POINT ( 'NONE',  ( 13.43411237798105340, 45.58196800326374643, 12.81628187352647963 ) ) ;
#13203 = CARTESIAN_POINT ( 'NONE',  ( 12.63842701281683034, 42.46726448433412315, 9.846743663894596210 ) ) ;
#13204 = CARTESIAN_POINT ( 'NONE',  ( 15.44008868035555260, 9.730352010821505360, 9.422509992056143702 ) ) ;
#13205 = CARTESIAN_POINT ( 'NONE',  ( -2.816281873526473856, 59.12363466993042493, 9.499525473075851096E-16 ) ) ;
#13206 = CARTESIAN_POINT ( 'NONE',  ( 0.1532563361054100626, 45.80059781766745886, -2.638427012816831230 ) ) ;
#13207 = CARTESIAN_POINT ( 'NONE',  ( -8.000000000000000000, 83.99999999999994316, 3.750000000000000000 ) ) ;
#13208 = VECTOR ( 'NONE', #21836, 1000.000000000000000 ) ;
#13209 = CARTESIAN_POINT ( 'NONE',  ( 0.000000000000000000, 15.00000000000000000, 0.000000000000000000 ) ) ;
#13210 = DIRECTION ( 'NONE',  ( -0.000000000000000000, -0.000000000000000000, 1.000000000000000000 ) ) ;
#13211 = CARTESIAN_POINT ( 'NONE',  ( 18.17884179759848706, 8.666888798595232757, -6.499999999999968914 ) ) ;
#13212 = EDGE_CURVE ( 'NONE', #4322, #17079, #39190, .T. ) ;
#13213 = CARTESIAN_POINT ( 'NONE',  ( -2.120353041430744323, 4.696395766537044518E-16, 14.34413130794943925 ) ) ;
#13214 = CARTESIAN_POINT ( 'NONE',  ( 17.20831665107776587, 19.13393115100078035, -7.208316651077762316 ) ) ;
#13215 = EDGE_CURVE ( 'NONE', #75354, #79733, #30677, .T. ) ;
#13216 = CARTESIAN_POINT ( 'NONE',  ( 10.00000000000000000, 27.87363466993042138, -12.81628187352647608 ) ) ;
#13217 = CARTESIAN_POINT ( 'NONE',  ( 0.9413316022086131163, 38.45508385108959004, 6.499999999999978684 ) ) ;
#13218 = VERTEX_POINT ( 'NONE', #23708 ) ;
#13219 = CARTESIAN_POINT ( 'NONE',  ( 2.791683348922237240, 60.38393115100078745, -7.208316651077763204 ) ) ;
#13220 = CARTESIAN_POINT ( 'NONE',  ( 17.85158348494336167, 4.737265733804413514, -6.499999999999994671 ) ) ;
#13221 = CARTESIAN_POINT ( 'NONE',  ( 10.00000000000000000, 20.55374883491396787, -14.16423886937410082 ) ) ;
#13222 = CARTESIAN_POINT ( 'NONE',  ( 2.791683348922240793, 46.63393115100077324, 7.208316651077764092 ) ) ;
#13223 = CARTESIAN_POINT ( 'NONE',  ( -2.816281873526473856, 49.12363466993042493, 9.499525473075851096E-16 ) ) ;
#13224 = CARTESIAN_POINT ( 'NONE',  ( 20.32896413005680714, 37.60497603579418069, -5.963430220938276349 ) ) ;
#13225 = CARTESIAN_POINT ( 'NONE',  ( 17.96484262340118221, 59.93868534415484106, 7.964842623401181321 ) ) ;
#13226 = CARTESIAN_POINT ( 'NONE',  ( 20.32896413005680714, 47.60497603579417358, -5.963430220938276349 ) ) ;
#13227 = CARTESIAN_POINT ( 'NONE',  ( 1.472469842513823179, 30.59226448433411960, -4.923371831947296329 ) ) ;
#13228 = CARTESIAN_POINT ( 'NONE',  ( 10.00000000000000178, 44.31368534415484106, 10.88017736071110342 ) ) ;
#13229 = AXIS2_PLACEMENT_3D ( 'NONE', #87305, #12292, #72779 ) ;
#13230 = CARTESIAN_POINT ( 'NONE',  ( 0.1532563361054100626, 30.80059781766744820, -2.638427012816831230 ) ) ;
#13231 = CARTESIAN_POINT ( 'NONE',  ( 14.49440716394870954, 15.00000000000000000, 0.4026921475167317688 ) ) ;
#13232 = ADVANCED_FACE ( 'NONE', ( #47663, #1209 ), #7211, .T. ) ;
#13233 = CARTESIAN_POINT ( 'NONE',  ( 0.5774900079438607392, 43.48035201082151247, 5.440088680355550821 ) ) ;
#13234 =( GEOMETRIC_REPRESENTATION_CONTEXT ( 3 ) GLOBAL_UNCERTAINTY_ASSIGNED_CONTEXT ( ( #86204 ) ) GLOBAL_UNIT_ASSIGNED_CONTEXT ( ( #63143, #55659, #69191 ) ) REPRESENTATION_CONTEXT ( 'NONE', 'WORKASPACE' ) );
#13235 = EDGE_LOOP ( 'NONE', ( #75658, #56590, #97259, #94384 ) ) ;
#13236 = AXIS2_PLACEMENT_3D ( 'NONE', #34378, #11396, #63410 ) ;
#13237 = CARTESIAN_POINT ( 'NONE',  ( -3.836325488035988052, 0.5000000000000004441, -14.50112432709427424 ) ) ;
#13238 = CARTESIAN_POINT ( 'NONE',  ( 17.96484262340118221, 14.93868534415483751, 7.964842623401181321 ) ) ;
#13240 = CARTESIAN_POINT ( 'NONE',  ( 15.44008868035555793, 41.39701867748817676, -9.422509992056140149 ) ) ;
#13239 = CARTESIAN_POINT ( 'NONE',  ( 17.20831665107776587, 52.88393115100078035, 7.208316651077764980 ) ) ;
#13241 = CARTESIAN_POINT ( 'NONE',  ( 9.402796353261051010, 15.00000000000000000, 11.68706210897763320 ) ) ;
#13242 = EDGE_CURVE ( 'NONE', #96688, #52732, #14098, .T. ) ;
#13243 = CARTESIAN_POINT ( 'NONE',  ( 7.084665262690076126, 64.10535201082150536, 10.88017736071109987 ) ) ;
#13245 = CARTESIAN_POINT ( 'NONE',  ( 0.000000000000000000, 70.80332830338373640, -5.000000000000000000 ) ) ;
#13244 = CARTESIAN_POINT ( 'NONE',  ( 20.88017736071110164, 30.35535201082151247, 2.915334737309930979 ) ) ;
#13246 = CARTESIAN_POINT ( 'NONE',  ( 0.1532563361054083140, 1.008931151000784787, 1.131784320476157264E-15 ) ) ;
#13247 = CARTESIAN_POINT ( 'NONE',  ( 19.84674366389459266, 28.71726448433411960, -2.638427012816827677 ) ) ;
#13248 = LINE ( 'NONE', #96274, #44114 ) ;
#13249 = CIRCLE ( 'NONE', #94694, 14.49999999999999822 ) ;
#13250 = CARTESIAN_POINT ( 'NONE',  ( -3.795296366450322534, 10.76208216824729647, -14.16423886937409904 ) ) ;
#13251 = CARTESIAN_POINT ( 'NONE',  ( 0.1532563361054082862, 51.21726448433412315, 2.638427012816831674 ) ) ;
#13253 = FACE_OUTER_BOUND ( 'NONE', #11347, .T. ) ;
#13252 = CARTESIAN_POINT ( 'NONE',  ( 10.00000000000000178, 58.05374883491397497, 14.16423886937410082 ) ) ;
#13254 = CARTESIAN_POINT ( 'NONE',  ( 17.08211943468705130, 13.47041550158063572, 12.26659068614894998 ) ) ;
#13255 = B_SPLINE_CURVE_WITH_KNOTS ( 'NONE', 3,
 ( #80333, #33339, #49823, #11832 ),
 .UNSPECIFIED., .F., .F.,
 ( 4, 4 ),
 ( 0.000000000000000000, 0.0003153491572464160622 ),
 .UNSPECIFIED. ) ;
#13256 = CARTESIAN_POINT ( 'NONE',  ( -2.266590686148945544, 31.38708216824730002, -7.082119434687050408 ) ) ;
#13257 = CARTESIAN_POINT ( 'NONE',  ( -1.099225684535947600, 9.540301336597087456, 6.408140936763237150 ) ) ;
#13258 = ORIENTED_EDGE ( 'NONE', *, *, #28207, .F. ) ;
#13259 = CARTESIAN_POINT ( 'NONE',  ( 19.42250999205614193, 10.14701867748816966, 5.440088680355555262 ) ) ;
#13260 = CARTESIAN_POINT ( 'NONE',  ( 1.472469842513823179, 45.59226448433412315, -4.923371831947296329 ) ) ;
#13262 = DIRECTION ( 'NONE',  ( -0.000000000000000000, -1.000000000000000000, -0.000000000000000000 ) ) ;
#13261 = CARTESIAN_POINT ( 'NONE',  ( -13.64884605730320644, 15.00000000000000000, 8.341846182955681144 ) ) ;
#13263 = CARTESIAN_POINT ( 'NONE',  ( 17.20831665107776587, 4.133931151000785675, -7.208316651077762316 ) ) ;
#13264 = CARTESIAN_POINT ( 'NONE',  ( 10.00000000000000178, 20.37363466993042138, 12.81628187352647608 ) ) ;
#13265 = CARTESIAN_POINT ( 'NONE',  ( 12.63842701281683922, 29.55059781766745175, -9.846743663894590881 ) ) ;
#13266 = ORIENTED_EDGE ( 'NONE', *, *, #43152, .F. ) ;
#13267 = CARTESIAN_POINT ( 'NONE',  ( 1.472469842513823179, 5.592264484334118713, -4.923371831947296329 ) ) ;
#13268 = FACE_OUTER_BOUND ( 'NONE', #29218, .T. ) ;
#13269 = CARTESIAN_POINT ( 'NONE',  ( -12.22506292814009576, 0.2306972965111887819, -8.589871424854882420 ) ) ;
#13270 = CARTESIAN_POINT ( 'NONE',  ( 10.00000000000000000, 16.81368534415483751, -10.88017736071110342 ) ) ;
#13271 = CARTESIAN_POINT ( 'NONE',  ( -0.3689425029237881626, 42.42874883491396787, 10.36894250292379027 ) ) ;
#13272 = CARTESIAN_POINT ( 'NONE',  ( -0.8801773607111009756, 68.06368534415484817, 1.068504757029289695E-15 ) ) ;
#13273 = CARTESIAN_POINT ( 'NONE',  ( 8.470640952597564777, -3.685863869977086348E-15, -11.92295067084766380 ) ) ;
#13274 = CARTESIAN_POINT ( 'NONE',  ( 20.24186590665278018, 52.61633188102327807, -6.114288769123040090 ) ) ;
#13275 = CARTESIAN_POINT ( 'NONE',  ( 5.076628168052704559, 30.17559781766745175, -8.527530157486179263 ) ) ;
#13276 = FILL_AREA_STYLE ('',( #97295 ) ) ;
#13277 = CARTESIAN_POINT ( 'NONE',  ( 18.52753015748618282, 3.925597817667451306, -4.923371831947291888 ) ) ;
#13278 = CARTESIAN_POINT ( 'NONE',  ( -1.066947046745619687, -5.787280142670764339E-16, -1.918137652920613778 ) ) ;
#13279 = CARTESIAN_POINT ( 'NONE',  ( 5.076628168052703671, 31.84226448433412315, 8.527530157486179263 ) ) ;
#13280 = CARTESIAN_POINT ( 'NONE',  ( 18.52753015748618282, 63.92559781766745886, -4.923371831947291888 ) ) ;
#13281 = CIRCLE ( 'NONE', #42062, 0.2500000000000002220 ) ;
#13282 = CARTESIAN_POINT ( 'NONE',  ( 19.42250999205614193, 40.14701867748817676, 5.440088680355555262 ) ) ;
#13283 = ADVANCED_FACE ( 'NONE', ( #53196 ), #24188, .T. ) ;
#13284 = VECTOR ( 'NONE', #11870, 1000.000000000000000 ) ;
#13285 = ORIENTED_EDGE ( 'NONE', *, *, #49353, .F. ) ;
#13286 = CARTESIAN_POINT ( 'NONE',  ( -2.816281873526471635, 58.91530133659707502, -3.434112377981056508 ) ) ;
#13287 = LINE ( 'NONE', #43775, #31651 ) ;
#13288 = CARTESIAN_POINT ( 'NONE',  ( 12.91533473730993009, 61.60535201082150536, -10.88017736071109987 ) ) ;
#13289 = CARTESIAN_POINT ( 'NONE',  ( 0.6178305044545838731, 39.74863466993041072, 9.382169495545420901 ) ) ;
#13291 = CARTESIAN_POINT ( 'NONE',  ( 5.076628168052703671, 31.84226448433412315, 8.527530157486179263 ) ) ;
#13290 = CARTESIAN_POINT ( 'NONE',  ( 10.00000000000000000, 55.55374883491396787, -14.16423886937410082 ) ) ;
#13292 = SURFACE_STYLE_USAGE ( .BOTH. , #91258 ) ;
#13293 = PRESENTATION_STYLE_ASSIGNMENT (( #83275 ) ) ;
#13294 = CARTESIAN_POINT ( 'NONE',  ( 24.16423886937410614, 19.51208216824729647, -3.795296366450302550 ) ) ;
#13295 = CARTESIAN_POINT ( 'NONE',  ( -2.266590686148945544, 42.22041550158063217, 7.082119434687048631 ) ) ;
#13296 = CARTESIAN_POINT ( 'NONE',  ( 1.472469842513823179, 46.42559781766745175, 4.923371831947296329 ) ) ;
#13297 = CARTESIAN_POINT ( 'NONE',  ( 10.00000000000000000, 41.81368534415484106, -10.88017736071110342 ) ) ;
#13298 = CARTESIAN_POINT ( 'NONE',  ( 0.5774900079438607392, 58.48035201082151247, 5.440088680355550821 ) ) ;
#13299 = PRODUCT_DEFINITION_SHAPE ( 'NONE', 'NONE',  #66632 ) ;
#13300 = VERTEX_POINT ( 'NONE', #53684 ) ;
#13301 = CARTESIAN_POINT ( 'NONE',  ( 10.00000000000000178, 40.37363466993042493, 12.81628187352647608 ) ) ;
#13302 = B_SPLINE_CURVE_WITH_KNOTS ( 'NONE', 3,
 ( #5984, #82460, #51973, #96499 ),
 .UNSPECIFIED., .F., .F.,
 ( 4, 4 ),
 ( 0.000000000000000000, 0.002392975128318497631 ),
 .UNSPECIFIED. ) ;
#13303 = CARTESIAN_POINT ( 'NONE',  ( 7.084665262690076126, 67.02201867748817676, -10.88017736071110164 ) ) ;
#13304 = ORIENTED_EDGE ( 'NONE', *, *, #36865, .T. ) ;
#13305 = EDGE_CURVE ( 'NONE', #35666, #48192, #22180, .T. ) ;
#13306 = CARTESIAN_POINT ( 'NONE',  ( 13.79529636645031943, 10.34541550158063394, -14.16423886937409904 ) ) ;
#13307 = CARTESIAN_POINT ( 'NONE',  ( 18.52753015748617571, 13.09226448433411960, 4.923371831947298993 ) ) ;
#13308 = CARTESIAN_POINT ( 'NONE',  ( -0.3289641300568005855, 60.10497603579418069, 5.963430220938281678 ) ) ;
#13309 = ORIENTED_EDGE ( 'NONE', *, *, #91952, .F. ) ;
#13310 = CARTESIAN_POINT ( 'NONE',  ( 4.559911319644449179, 18.89701867748817321, 9.422509992056141925 ) ) ;
#13311 = CARTESIAN_POINT ( 'NONE',  ( 1.472469842513823179, 0.5922644843341181575, -4.923371831947296329 ) ) ;
#13312 = AXIS2_PLACEMENT_3D ( 'NONE', #53354, #66382, #98897 ) ;
#13313 = CARTESIAN_POINT ( 'NONE',  ( 10.00000000000000178, 13.05374883491396787, 14.16423886937410082 ) ) ;
#13314 = VERTEX_POINT ( 'NONE', #79633 ) ;
#13315 = CARTESIAN_POINT ( 'NONE',  ( 0.5774900079438607392, 28.48035201082150891, 5.440088680355550821 ) ) ;
#13316 = CARTESIAN_POINT ( 'NONE',  ( 18.52753015748617571, 53.09226448433412315, 4.923371831947298993 ) ) ;
#13317 = EDGE_LOOP ( 'NONE', ( #80166, #53526, #64662, #79863 ) ) ;
#13318 = VECTOR ( 'NONE', #78913, 1000.000000000000000 ) ;
#13319 = CARTESIAN_POINT ( 'NONE',  ( 2.791683348922237240, 60.38393115100078745, -7.208316651077763204 ) ) ;
#13320 = ORIENTED_EDGE ( 'NONE', *, *, #63943, .T. ) ;
#13321 = AXIS2_PLACEMENT_3D ( 'NONE', #3273, #16803, #10283 ) ;
#13322 = CARTESIAN_POINT ( 'NONE',  ( 10.00000000000000000, 61.81368534415484106, -10.88017736071110342 ) ) ;
#13323 = CARTESIAN_POINT ( 'NONE',  ( 12.63842701281683922, 59.55059781766744464, -9.846743663894590881 ) ) ;
#13324 = EDGE_CURVE ( 'NONE', #30576, #38057, #82757, .T. ) ;
#13325 = CARTESIAN_POINT ( 'NONE',  ( -2.816281873526473856, 39.33196800326374643, 3.434112377981055619 ) ) ;
#13327 = DIRECTION ( 'NONE',  ( 0.000000000000000000, 0.000000000000000000, 1.000000000000000000 ) ) ;
#13326 = CARTESIAN_POINT ( 'NONE',  ( 19.42250999205614193, 5.147018677488171434, 5.440088680355555262 ) ) ;
#13328 = CARTESIAN_POINT ( 'NONE',  ( 10.00000000000000178, 2.258931151000784787, 9.846743663894594434 ) ) ;
#13329 = CARTESIAN_POINT ( 'NONE',  ( 12.91533473730992121, 24.52201867748816966, 10.88017736071110164 ) ) ;
#13330 = EDGE_CURVE ( 'NONE', #97093, #76767, #3647, .T. ) ;
#13331 = ORIENTED_EDGE ( 'NONE', *, *, #78782, .T. ) ;
#13332 = CARTESIAN_POINT ( 'NONE',  ( 16.40814093676324603, 52.45696800326375353, -11.09922568453594671 ) ) ;
#13333 = CARTESIAN_POINT ( 'NONE',  ( 2.035157376598822676, 47.43868534415484817, -7.964842623401177768 ) ) ;
#13334 = DIRECTION ( 'NONE',  ( 0.000000000000000000, -1.000000000000000000, -0.000000000000000000 ) ) ;
#13335 = CARTESIAN_POINT ( 'NONE',  ( 22.81628187352648496, 41.83196800326375353, -3.434112377981050290 ) ) ;
#13336 = CARTESIAN_POINT ( 'NONE',  ( 2.035157376598824452, 43.68868534415484106, 7.964842623401179544 ) ) ;
#13337 = EDGE_CURVE ( 'NONE', #17685, #28441, #92649, .T. ) ;
#13338 = CARTESIAN_POINT ( 'NONE',  ( 17.20831665107776587, 59.13393115100078745, -7.208316651077762316 ) ) ;
#13339 = CARTESIAN_POINT ( 'NONE',  ( -4.862001128006866679, 15.00000000000000000, 13.66056166602454347 ) ) ;
#13340 = CARTESIAN_POINT ( 'NONE',  ( 1.472469842513823179, 16.42559781766745175, 4.923371831947296329 ) ) ;
#13341 = CARTESIAN_POINT ( 'NONE',  ( 6.565887622018943937, 13.08196800326374998, -12.81628187352647608 ) ) ;
#13343 = CARTESIAN_POINT ( 'NONE',  ( 12.63842701281683922, 64.55059781766745175, -9.846743663894590881 ) ) ;
#13342 = CARTESIAN_POINT ( 'NONE',  ( -13.80050776813097002, 90.89648773604355370, -7.753931633032691728 ) ) ;
#13344 = CARTESIAN_POINT ( 'NONE',  ( 12.91533473730992121, 24.52201867748816966, 10.88017736071110164 ) ) ;
#13345 = CARTESIAN_POINT ( 'NONE',  ( 19.84674366389459266, 53.30059781766744464, 2.638427012816836559 ) ) ;
#13346 = DIRECTION ( 'NONE',  ( -0.000000000000000000, -1.000000000000000000, -0.000000000000000000 ) ) ;
#13347 = CARTESIAN_POINT ( 'NONE',  ( 17.20831665107776587, 12.88393115100078390, 7.208316651077764980 ) ) ;
#13348 = CARTESIAN_POINT ( 'NONE',  ( 0.1532563361054082862, 1.217264484334117824, 2.638427012816831674 ) ) ;
#13350 = ORIENTED_EDGE ( 'NONE', *, *, #24010, .F. ) ;
#13349 = CARTESIAN_POINT ( 'NONE',  ( 16.40814093676324603, 2.456968003263753531, -11.09922568453594671 ) ) ;
#13351 = CARTESIAN_POINT ( 'NONE',  ( -40.70923076923077844, 107.8461538461538396, -9.500000000000000000 ) ) ;
#13352 = CARTESIAN_POINT ( 'NONE',  ( 13.43411237798105340, 40.58196800326375353, 12.81628187352647963 ) ) ;
#13353 = CARTESIAN_POINT ( 'NONE',  ( 19.84674366389459266, 28.30059781766745886, 2.638427012816836559 ) ) ;
#13354 = FILL_AREA_STYLE ('',( #81840 ) ) ;
#13355 = CARTESIAN_POINT ( 'NONE',  ( -2.266590686148945544, 57.22041550158063217, 7.082119434687048631 ) ) ;
#13356 = CARTESIAN_POINT ( 'NONE',  ( 0.1532563361054082862, 36.21726448433410894, 2.638427012816831674 ) ) ;
#13357 = ORIENTED_EDGE ( 'NONE', *, *, #57021, .T. ) ;
#13358 = DIRECTION ( 'NONE',  ( 0.000000000000000000, -1.000000000000000000, 0.000000000000000000 ) ) ;
#13359 = CARTESIAN_POINT ( 'NONE',  ( 20.88017736071110164, 10.35535201082150714, 2.915334737309930979 ) ) ;
#13360 = CARTESIAN_POINT ( 'NONE',  ( -42.80192881254231452, 92.20710678118653902, 9.500000000000000000 ) ) ;
#13361 = EDGE_CURVE ( 'NONE', #30230, #43585, #55661, .T. ) ;
#13362 = CARTESIAN_POINT ( 'NONE',  ( 0.5774900079438607392, 13.48035201082150358, 5.440088680355550821 ) ) ;
#13363 = CARTESIAN_POINT ( 'NONE',  ( -2.266590686148945544, 47.22041550158063927, 7.082119434687048631 ) ) ;
#13364 = CARTESIAN_POINT ( 'NONE',  ( 10.00000000000000000, 55.55374883491396787, -14.16423886937410082 ) ) ;
#13365 = DIRECTION ( 'NONE',  ( 0.000000000000000000, 1.000000000000000000, 0.000000000000000000 ) ) ;
#13366 = CARTESIAN_POINT ( 'NONE',  ( 1.472469842513823179, 6.425597817667451750, 4.923371831947296329 ) ) ;
#13367 = CARTESIAN_POINT ( 'NONE',  ( 16.40814093676323893, 0.7903013365970867898, 11.09922568453595026 ) ) ;
#13368 = ORIENTED_EDGE ( 'NONE', *, *, #32527, .T. ) ;
#13369 = CARTESIAN_POINT ( 'NONE',  ( 7.084665262690076126, 52.02201867748816255, -10.88017736071110164 ) ) ;
#13370 = CARTESIAN_POINT ( 'NONE',  ( -2.815433093576927170, 15.00000000000000000, -14.73340885523753663 ) ) ;
#13371 = ADVANCED_FACE ( 'NONE', ( #26621 ), #48633, .T. ) ;
#13372 = CARTESIAN_POINT ( 'NONE',  ( 0.1532563361054100626, 65.80059781766745175, -2.638427012816831230 ) ) ;
#13373 = VERTEX_POINT ( 'NONE', #32651 ) ;
#13374 = CARTESIAN_POINT ( 'NONE',  ( 12.63842701281683034, 32.46726448433412315, 9.846743663894596210 ) ) ;
#13375 = DIRECTION ( 'NONE',  ( 0.000000000000000000, 0.000000000000000000, -1.000000000000000000 ) ) ;
#13376 = ORIENTED_EDGE ( 'NONE', *, *, #78245, .T. ) ;
#13377 = VECTOR ( 'NONE', #69261, 1000.000000000000000 ) ;
#13378 = CARTESIAN_POINT ( 'NONE',  ( 2.917880565312948704, 42.63708216824729647, 12.26659068614894643 ) ) ;
#13379 = ORIENTED_EDGE ( 'NONE', *, *, #47254, .T. ) ;
#13380 = CARTESIAN_POINT ( 'NONE',  ( 18.52753015748618282, 13.92559781766745175, -4.923371831947291888 ) ) ;
#13382 = DIRECTION ( 'NONE',  ( 0.000000000000000000, 0.000000000000000000, 1.000000000000000000 ) ) ;
#13381 = CARTESIAN_POINT ( 'NONE',  ( -7.072497013529895682, -84.40007040885102185, -2.750000000000805578 ) ) ;
#13383 = CARTESIAN_POINT ( 'NONE',  ( 12.91533473730992121, 29.52201867748817321, 10.88017736071110164 ) ) ;
#13384 = CARTESIAN_POINT ( 'NONE',  ( 22.81628187352648496, 31.83196800326375353, -3.434112377981050290 ) ) ;
#13385 = CARTESIAN_POINT ( 'NONE',  ( 3.591859063236763294, 38.29030133659708923, -11.09922568453595026 ) ) ;
#13386 = CARTESIAN_POINT ( 'NONE',  ( 13.43411237798106583, 57.66530133659708923, -12.81628187352647252 ) ) ;
#13387 = EDGE_LOOP ( 'NONE', ( #24565, #42596, #63901, #80699, #98621, #42716 ) ) ;
#13388 = AXIS2_PLACEMENT_3D ( 'NONE', #64139, #41676, #70692 ) ;
#13389 = CARTESIAN_POINT ( 'NONE',  ( 17.75000000000000711, 43.00000000000000000, 6.250000000000000000 ) ) ;
#13390 = CARTESIAN_POINT ( 'NONE',  ( -11.23890517442507075, -88.22482801187260293, -4.000000000000000888 ) ) ;
#13391 = CARTESIAN_POINT ( 'NONE',  ( 24.16423886937409904, 24.09541550158063927, 3.795296366450317205 ) ) ;
#13392 = FILL_AREA_STYLE ('',( #50397 ) ) ;
#13393 =( LENGTH_UNIT ( ) NAMED_UNIT ( * ) SI_UNIT ( .MILLI., .METRE. ) );
#13394 = CARTESIAN_POINT ( 'NONE',  ( 2.035157376598824452, 23.68868534415484461, 7.964842623401179544 ) ) ;
#13395 = CARTESIAN_POINT ( 'NONE',  ( -4.000000000000000000, 10.25000000000000000, -2.750000000000000000 ) ) ;
#13396 = DIRECTION ( 'NONE',  ( 0.000000000000000000, 0.000000000000000000, -1.000000000000000000 ) ) ;
#13397 = CARTESIAN_POINT ( 'NONE',  ( -0.8801773607110991993, 47.85535201082150536, -2.915334737309923874 ) ) ;
#13398 = CARTESIAN_POINT ( 'NONE',  ( -0.8801773607110991993, 52.85535201082151247, -2.915334737309923874 ) ) ;
#13399 = CARTESIAN_POINT ( 'NONE',  ( 3.591859063236763294, 13.29030133659708746, -11.09922568453595026 ) ) ;
#13400 = DIRECTION ( 'NONE',  ( -4.085620730620576069E-14, 0.000000000000000000, 1.000000000000000000 ) ) ;
#13401 = CARTESIAN_POINT ( 'NONE',  ( 2.933660812629996339, 15.00000000000000000, -15.72485391577589731 ) ) ;
#13402 = CARTESIAN_POINT ( 'NONE',  ( 5.076628168052703671, 21.84226448433411960, 8.527530157486179263 ) ) ;
#13403 = CARTESIAN_POINT ( 'NONE',  ( 10.00000000000000000, 46.81368534415484106, -10.88017736071110342 ) ) ;
#13404 = CARTESIAN_POINT ( 'NONE',  ( -2.816281873526473856, 14.33196800326375531, 3.434112377981055619 ) ) ;
#13405 = CARTESIAN_POINT ( 'NONE',  ( 2.791683348922237240, 0.3839311510007847872, -7.208316651077763204 ) ) ;
#13406 = CARTESIAN_POINT ( 'NONE',  ( 0.1532563361054083140, 21.00893115100078745, 1.131784320476157264E-15 ) ) ;
#13407 = CARTESIAN_POINT ( 'NONE',  ( 3.591859063236763294, 48.29030133659708923, -11.09922568453595026 ) ) ;
#13408 = CARTESIAN_POINT ( 'NONE',  ( 5.076628168052704559, 25.17559781766745175, -8.527530157486179263 ) ) ;
#13409 = ORIENTED_EDGE ( 'NONE', *, *, #24949, .T. ) ;
#13410 = CARTESIAN_POINT ( 'NONE',  ( 22.26659068614894466, 3.887082168247300906, 7.082119434687054849 ) ) ;
#13411 = DIRECTION ( 'NONE',  ( 0.000000000000000000, 0.000000000000000000, 1.000000000000000000 ) ) ;
#13412 = CARTESIAN_POINT ( 'NONE',  ( -0.8801773607111008646, 23.27201867748817676, 2.915334737309923430 ) ) ;
#13413 = CARTESIAN_POINT ( 'NONE',  ( -4.164238869374099927, 37.01208216824731068, 3.795296366450308767 ) ) ;
#13414 = CARTESIAN_POINT ( 'NONE',  ( 5.076628168052704559, 35.17559781766745175, -8.527530157486179263 ) ) ;
#13415 = CARTESIAN_POINT ( 'NONE',  ( -0.8801773607111008646, 23.27201867748817676, 2.915334737309923430 ) ) ;
#13416 = EDGE_CURVE ( 'NONE', #42599, #63730, #29422, .T. ) ;
#13417 = CARTESIAN_POINT ( 'NONE',  ( 2.035157376598822676, 22.43868534415483396, -7.964842623401177768 ) ) ;
#13418 = ORIENTED_EDGE ( 'NONE', *, *, #35938, .F. ) ;
#13419 = CARTESIAN_POINT ( 'NONE',  ( 2.035157376598824452, 23.68868534415484461, 7.964842623401179544 ) ) ;
#13420 = EDGE_CURVE ( 'NONE', #33129, #22102, #49133, .T. ) ;
#13421 = CARTESIAN_POINT ( 'NONE',  ( 21.09922568453594849, 41.20696800326375353, 6.408140936763242479 ) ) ;
#13422 = CARTESIAN_POINT ( 'NONE',  ( 19.42250999205614548, 35.98035201082151247, -5.440088680355545492 ) ) ;
#13424 = CARTESIAN_POINT ( 'NONE',  ( 12.91533473730993009, 36.60535201082151247, -10.88017736071109987 ) ) ;
#13423 = CARTESIAN_POINT ( 'NONE',  ( 7.551349515323185990, -0.03417435944610275333, -12.08468537022906020 ) ) ;
#13425 = ORIENTED_EDGE ( 'NONE', *, *, #93354, .F. ) ;
#13426 = CARTESIAN_POINT ( 'NONE',  ( 10.00000000000000178, 52.25893115100078745, 9.846743663894594434 ) ) ;
#13427 = CARTESIAN_POINT ( 'NONE',  ( 15.44008868035555793, 41.39701867748817676, -9.422509992056140149 ) ) ;
#13428 = FILL_AREA_STYLE ('',( #51929 ) ) ;
#13429 = CARTESIAN_POINT ( 'NONE',  ( -0.03743638938523772414, 9.251975280310178462, -6.399506433553937335 ) ) ;
#13430 = CARTESIAN_POINT ( 'NONE',  ( -4.164238869374099927, 47.01208216824729647, 3.795296366450308767 ) ) ;
#13431 = CARTESIAN_POINT ( 'NONE',  ( 17.96484262340118221, 49.93868534415484106, 7.964842623401181321 ) ) ;
#13432 = CARTESIAN_POINT ( 'NONE',  ( 0.2751277870542911397, 50.30223176428831522, 6.499999999999992006 ) ) ;
#13433 = CARTESIAN_POINT ( 'NONE',  ( 0.000000000000000000, 0.5000000000000000000, -5.999999999999999112 ) ) ;
#13434 = CARTESIAN_POINT ( 'NONE',  ( 18.52753015748618282, 48.92559781766745886, -4.923371831947291888 ) ) ;
#13435 = CARTESIAN_POINT ( 'NONE',  ( 5.076628168052704559, 5.175597817667451750, -8.527530157486179263 ) ) ;
#13436 = CARTESIAN_POINT ( 'NONE',  ( 7.361572987183169658, 24.96726448433412315, -9.846743663894592657 ) ) ;
#13437 = ORIENTED_EDGE ( 'NONE', *, *, #20763, .T. ) ;
#13438 = CARTESIAN_POINT ( 'NONE',  ( 2.791683348922237240, 15.38393115100078212, -7.208316651077763204 ) ) ;
#13439 = CARTESIAN_POINT ( 'NONE',  ( 11.09922568453594671, -17.95969866340290721, -6.408140936763241591 ) ) ;
#13440 = CARTESIAN_POINT ( 'NONE',  ( -0.8801773607110991993, 22.85535201082150181, -2.915334737309923874 ) ) ;
#13441 = CARTESIAN_POINT ( 'NONE',  ( 1.472469842513823179, 25.59226448433412315, -4.923371831947296329 ) ) ;
#13442 = CARTESIAN_POINT ( 'NONE',  ( 0.6178305044545838731, 9.748634669930416052, 9.382169495545420901 ) ) ;
#13444 = CARTESIAN_POINT ( 'NONE',  ( 20.88017736071110519, 50.56368534415484106, 2.639326808657452039E-16 ) ) ;
#13443 = CARTESIAN_POINT ( 'NONE',  ( 4.559911319644449179, 63.89701867748817676, 9.422509992056141925 ) ) ;
#13446 = CARTESIAN_POINT ( 'NONE',  ( 19.38216949554541202, 50.99863466993042493, 9.382169495545424454 ) ) ;
#13445 = CARTESIAN_POINT ( 'NONE',  ( 15.44008868035555793, 31.39701867748817676, -9.422509992056140149 ) ) ;
#13447 = CARTESIAN_POINT ( 'NONE',  ( 17.08211943468705840, 40.13708216824731068, -12.26659068614894466 ) ) ;
#13448 = ADVANCED_FACE ( 'NONE', ( #34604 ), #55573, .T. ) ;
#13449 = VECTOR ( 'NONE', #91442, 999.9999999999998863 ) ;
#13450 = DIRECTION ( 'NONE',  ( 0.000000000000000000, 0.000000000000000000, -1.000000000000000000 ) ) ;
#13451 = ORIENTED_EDGE ( 'NONE', *, *, #92279, .T. ) ;
#13452 = CARTESIAN_POINT ( 'NONE',  ( -2.816281873526471635, 3.915301336597087456, -3.434112377981056508 ) ) ;
#13453 = CARTESIAN_POINT ( 'NONE',  ( 4.559911319644449179, 3.897018677488170990, 9.422509992056141925 ) ) ;
#13454 = ADVANCED_FACE ( 'NONE', ( #19616 ), #49606, .F. ) ;
#13455 = CARTESIAN_POINT ( 'NONE',  ( 20.88017736071110875, 50.77201867748817676, -2.915334737309920765 ) ) ;
#13456 = SURFACE_SIDE_STYLE ('',( #37458 ) ) ;
#13457 = CIRCLE ( 'NONE', #69354, 14.49999999999999822 ) ;
#13458 = EDGE_LOOP ( 'NONE', ( #51419, #49191, #84612, #40562, #30478, #1403, #37948, #27953 ) ) ;
#13460 = CARTESIAN_POINT ( 'NONE',  ( -12.54397927573574378, 0.2306972965111899199, 8.117058495688928232 ) ) ;
#13459 = CARTESIAN_POINT ( 'NONE',  ( 0.1532563361054082862, 11.21726448433411605, 2.638427012816831674 ) ) ;
#13461 = FACE_OUTER_BOUND ( 'NONE', #26684, .T. ) ;
#13462 = CARTESIAN_POINT ( 'NONE',  ( 2.035157376598824452, 58.68868534415482685, 7.964842623401179544 ) ) ;
#13463 = CARTESIAN_POINT ( 'NONE',  ( 5.076628168052704559, 30.17559781766745175, -8.527530157486179263 ) ) ;
#13464 = PRODUCT_RELATED_PRODUCT_CATEGORY ( 'part', '', ( #36462 ) ) ;
#13465 = CARTESIAN_POINT ( 'NONE',  ( 14.92337183194729988, 29.34226448433411960, -8.527530157486177487 ) ) ;
#13466 = CARTESIAN_POINT ( 'NONE',  ( 19.84674366389459266, 8.300597817667451750, 2.638427012816836559 ) ) ;
#13468 = CARTESIAN_POINT ( 'NONE',  ( -1.099225684535947600, 43.70696800326375353, -6.408140936763238038 ) ) ;
#13467 = CARTESIAN_POINT ( 'NONE',  ( 14.76100041229769744, 14.76930270348882068, 2.313205896730931244 ) ) ;
#13470 = CARTESIAN_POINT ( 'NONE',  ( 10.58840669699852199, -98.14374106289703548, -3.750000000000000000 ) ) ;
#13469 = CARTESIAN_POINT ( 'NONE',  ( 7.084665262690076126, 67.02201867748817676, -10.88017736071110164 ) ) ;
#13471 = CARTESIAN_POINT ( 'NONE',  ( 11.10646695662408767, -65.08356741887227770, 4.000000000000000000 ) ) ;
#13473 = ORIENTED_EDGE ( 'NONE', *, *, #734, .T. ) ;
#13472 = CARTESIAN_POINT ( 'NONE',  ( 5.076628168052704559, 35.17559781766745175, -8.527530157486179263 ) ) ;
#13474 = CARTESIAN_POINT ( 'NONE',  ( 6.565887622018943937, 55.16530133659709634, 12.81628187352647430 ) ) ;
#13475 = LINE ( 'NONE', #43467, #58182 ) ;
#13476 = CARTESIAN_POINT ( 'NONE',  ( 1.472469842513823179, 65.59226448433412315, -4.923371831947296329 ) ) ;
#13477 = CARTESIAN_POINT ( 'NONE',  ( 0.000000000000000000, 14.49999999999999822, 0.000000000000000000 ) ) ;
#13478 = EDGE_CURVE ( 'NONE', #11027, #66682, #86650, .T. ) ;
#13479 = CARTESIAN_POINT ( 'NONE',  ( 20.36894250292379382, 13.67874883491396965, 10.36894250292379205 ) ) ;
#13480 = B_SPLINE_CURVE_WITH_KNOTS ( 'NONE', 3,
 ( #53551, #37585, #52085, #22585, #83573, #45566, #601, #45063, #29071, #104, #75572, #82578, #68572, #84066, #97612, #74577, #67590, #76061, #30550, #15092, #60567, #38083, #44576, #7085 ),
 .UNSPECIFIED., .F., .F.,
 ( 4, 2, 2, 2, 2, 2, 2, 2, 2, 2, 2, 4 ),
 ( 0.000000000000000000, 0.003099737161558395546, 0.006199474323116791093, 0.01239894864623362208, 0.02479789729246732743, 0.03719684593870102585, 0.04959579458493475201, 0.07439369187740220435, 0.08679264052363593052, 0.09299211484675279360, 0.09609185200831121820, 0.09919158916986964281 ),
 .UNSPECIFIED. ) ;
#13481 = UNCERTAINTY_MEASURE_WITH_UNIT (LENGTH_MEASURE( 1.000000000000000082E-05 ), #48766, 'distance_accuracy_value', 'NONE');
#13482 = CARTESIAN_POINT ( 'NONE',  ( 2.603489959281588995, 40.43575266056827644, -6.500000000000003553 ) ) ;
#13483 = CARTESIAN_POINT ( 'NONE',  ( -2.266590686148945544, 26.38708216824730357, -7.082119434687050408 ) ) ;
#13484 = CARTESIAN_POINT ( 'NONE',  ( -2.266590686148945544, 41.38708216824729647, -7.082119434687050408 ) ) ;
#13485 = CARTESIAN_POINT ( 'NONE',  ( 20.36894250292379738, 9.928748834913966093, -10.36894250292379027 ) ) ;
#13487 = FACE_OUTER_BOUND ( 'NONE', #25345, .T. ) ;
#13486 = CARTESIAN_POINT ( 'NONE',  ( -0.3689425029237881626, 7.428748834913967869, 10.36894250292379027 ) ) ;
#13488 = CARTESIAN_POINT ( 'NONE',  ( 10.00000000000000178, 54.31368534415484106, 10.88017736071110342 ) ) ;
#13489 = CARTESIAN_POINT ( 'NONE',  ( -5.056330833731841778, 4.586016791640643039E-16, 13.58983143750696421 ) ) ;
#13490 = ORIENTED_EDGE ( 'NONE', *, *, #11929, .T. ) ;
#13491 = CARTESIAN_POINT ( 'NONE',  ( 17.20831665107776587, 27.88393115100078390, 7.208316651077764980 ) ) ;
#13493 = CARTESIAN_POINT ( 'NONE',  ( 17.20831665107776587, 27.88393115100078390, 7.208316651077764980 ) ) ;
#13492 = CARTESIAN_POINT ( 'NONE',  ( 17.96484262340118221, 66.18868534415483396, -7.964842623401177768 ) ) ;
#13494 = CARTESIAN_POINT ( 'NONE',  ( 10.00000000000000178, 14.31368534415483929, 10.88017736071110342 ) ) ;
#13495 = CARTESIAN_POINT ( 'NONE',  ( 10.00000000000000000, 52.87363466993041783, -12.81628187352647608 ) ) ;
#13496 = CARTESIAN_POINT ( 'NONE',  ( 19.84674366389459621, 53.50893115100078745, 7.409399052514197653E-17 ) ) ;
#13497 = DIRECTION ( 'NONE',  ( -0.000000000000000000, -1.000000000000000000, -0.000000000000000000 ) ) ;
#13498 = CARTESIAN_POINT ( 'NONE',  ( 19.84674366389459621, 33.50893115100078745, 7.409399052514197653E-17 ) ) ;
#13499 = CARTESIAN_POINT ( 'NONE',  ( 22.81628187352647785, 36.62363466993041783, 6.195893100308588602E-16 ) ) ;
#13500 = CARTESIAN_POINT ( 'NONE',  ( 3.795296366450314540, -16.73791783175269998, 14.16423886937410082 ) ) ;
#13501 = CARTESIAN_POINT ( 'NONE',  ( 12.91533473730992121, 49.52201867748817676, 10.88017736071110164 ) ) ;
#13502 = CARTESIAN_POINT ( 'NONE',  ( 10.00000000000000178, 42.25893115100078745, 9.846743663894594434 ) ) ;
#13503 = CARTESIAN_POINT ( 'NONE',  ( 2.917880565312950480, 25.97041550158063572, -12.26659068614894821 ) ) ;
#13504 = ORIENTED_EDGE ( 'NONE', *, *, #62767, .F. ) ;
#13505 =( LENGTH_UNIT ( ) NAMED_UNIT ( * ) SI_UNIT ( .MILLI., .METRE. ) );
#13506 = CARTESIAN_POINT ( 'NONE',  ( 7.084665262690076126, 47.02201867748818387, -10.88017736071110164 ) ) ;
#13507 = CARTESIAN_POINT ( 'NONE',  ( 4.559911319644449179, 67.23035201082150536, -9.422509992056141925 ) ) ;
#13508 = CARTESIAN_POINT ( 'NONE',  ( 22.26659068614895176, 54.72041550158063217, -7.082119434687042414 ) ) ;
#13509 = CARTESIAN_POINT ( 'NONE',  ( -1.099225684535947600, -0.4596986634029132657, 6.408140936763237150 ) ) ;
#13510 = DIRECTION ( 'NONE',  ( -0.000000000000000000, -1.000000000000000000, -0.000000000000000000 ) ) ;
#13511 = CARTESIAN_POINT ( 'NONE',  ( 7.084665262690076126, 59.10535201082150536, 10.88017736071109987 ) ) ;
#13512 = CARTESIAN_POINT ( 'NONE',  ( -1.926860441876563801, 27.66212336850780673, 1.004413902775740978E-15 ) ) ;
#13513 = CARTESIAN_POINT ( 'NONE',  ( 22.81628187352648496, 31.83196800326375353, -3.434112377981050290 ) ) ;
#13514 = CARTESIAN_POINT ( 'NONE',  ( 2.791683348922240793, 61.63393115100079456, 7.208316651077764092 ) ) ;
#13515 = CARTESIAN_POINT ( 'NONE',  ( 10.88017736071110164, 30.35535201082151957, 2.915334737309921209 ) ) ;
#13516 = CARTESIAN_POINT ( 'NONE',  ( -0.8801773607111008646, 8.272018677488171434, 2.915334737309923430 ) ) ;
#13517 = CARTESIAN_POINT ( 'NONE',  ( 7.084665262690076126, 7.022018677488170546, -10.88017736071110164 ) ) ;
#13518 = CARTESIAN_POINT ( 'NONE',  ( 1.472469842513823179, 45.59226448433412315, -4.923371831947296329 ) ) ;
#13519 = CARTESIAN_POINT ( 'NONE',  ( 17.39651004071838614, 62.93575266056827644, 6.500000000000032863 ) ) ;
#13520 = ORIENTED_EDGE ( 'NONE', *, *, #70897, .F. ) ;
#13521 = CARTESIAN_POINT ( 'NONE',  ( 10.00000000000000178, 9.313685344154839285, 10.88017736071110342 ) ) ;
#13522 = CARTESIAN_POINT ( 'NONE',  ( 22.81628187352648496, 11.83196800326375531, -3.434112377981050290 ) ) ;
#13523 = DIRECTION ( 'NONE',  ( 0.000000000000000000, 0.000000000000000000, 1.000000000000000000 ) ) ;
#13524 = CARTESIAN_POINT ( 'NONE',  ( 19.84674366389459266, 13.30059781766745353, 2.638427012816836559 ) ) ;
#13525 = CARTESIAN_POINT ( 'NONE',  ( 2.791683348922237240, 40.38393115100078035, -7.208316651077763204 ) ) ;
#13526 = CARTESIAN_POINT ( 'NONE',  ( 4.559911319644449179, 42.23035201082151247, -9.422509992056141925 ) ) ;
#13527 = VECTOR ( 'NONE', #77439, 1000.000000000000000 ) ;
#13528 = CARTESIAN_POINT ( 'NONE',  ( 22.81628187352648496, 6.831968003263753531, -3.434112377981050290 ) ) ;
#13530 = DIRECTION ( 'NONE',  ( -0.000000000000000000, 1.000000000000000000, -0.000000000000000000 ) ) ;
#13529 = CARTESIAN_POINT ( 'NONE',  ( 20.88017736071110164, 50.35535201082151247, 2.915334737309930979 ) ) ;
#13531 = CARTESIAN_POINT ( 'NONE',  ( 19.38216949554541557, 57.24863466993042493, -9.382169495545420901 ) ) ;
#13532 = ORIENTED_EDGE ( 'NONE', *, *, #75556, .F. ) ;
#13533 = CARTESIAN_POINT ( 'NONE',  ( 0.5774900079438607392, 68.48035201082150536, 5.440088680355550821 ) ) ;
#13534 = CARTESIAN_POINT ( 'NONE',  ( 6.565887622018943937, 30.16530133659708568, 12.81628187352647430 ) ) ;
#13535 = CARTESIAN_POINT ( 'NONE',  ( 20.24186590665276597, 31.76028685723174405, 6.114288769123062295 ) ) ;
#13536 = CARTESIAN_POINT ( 'NONE',  ( 17.96484262340118221, 36.18868534415484106, -7.964842623401177768 ) ) ;
#13537 = CARTESIAN_POINT ( 'NONE',  ( 10.00000000000000178, 62.25893115100078745, 9.846743663894594434 ) ) ;
#13538 = CARTESIAN_POINT ( 'NONE',  ( 7.361572987183169658, 59.96726448433410894, -9.846743663894592657 ) ) ;
#13539 = CARTESIAN_POINT ( 'NONE',  ( 19.84674366389459266, 18.71726448433411960, -2.638427012816827677 ) ) ;
#13540 = CARTESIAN_POINT ( 'NONE',  ( 2.791683348922240793, 6.633931151000785675, 7.208316651077764092 ) ) ;
#13541 = CARTESIAN_POINT ( 'NONE',  ( -0.1023957841222509352, 5.133775574782962536, 6.340343622311908511 ) ) ;
#13542 = CARTESIAN_POINT ( 'NONE',  ( 17.08211943468705840, 30.13708216824730357, -12.26659068614894466 ) ) ;
#13543 = CARTESIAN_POINT ( 'NONE',  ( 14.17193700899789022, 15.00000000000000000, 1.489530601564113654 ) ) ;
#13544 = EDGE_CURVE ( 'NONE', #57586, #93536, #72604, .T. ) ;
#13545 = CARTESIAN_POINT ( 'NONE',  ( 9.512243806915856581, -15.51051116580330635, -3.750000000000000888 ) ) ;
#13546 = CARTESIAN_POINT ( 'NONE',  ( -3.500000000000000444, 1.019547802438453887, -3.750000000000000000 ) ) ;
#13547 = ORIENTED_EDGE ( 'NONE', *, *, #54303, .F. ) ;
#13548 = CARTESIAN_POINT ( 'NONE',  ( -0.3689425029237898834, 56.17874883491396076, -10.36894250292378850 ) ) ;
#13549 = CARTESIAN_POINT ( 'NONE',  ( -0.3689425029237898834, 66.17874883491396076, -10.36894250292378850 ) ) ;
#13550 = CARTESIAN_POINT ( 'NONE',  ( 0.1532563361054083140, 36.00893115100078745, 1.131784320476157264E-15 ) ) ;
#13551 = CARTESIAN_POINT ( 'NONE',  ( 21.09922568453595559, 32.04030133659708923, -6.408140936763230044 ) ) ;
#13552 = DIRECTION ( 'NONE',  ( 1.000000000000000000, 0.000000000000000000, 0.000000000000000000 ) ) ;
#13553 = CARTESIAN_POINT ( 'NONE',  ( -0.3289641300567998083, 43.07879003517447813, 5.963430220938281678 ) ) ;
#13554 = CARTESIAN_POINT ( 'NONE',  ( -0.8801773607111009756, 18.06368534415484106, 1.068504757029289695E-15 ) ) ;
#13555 = CARTESIAN_POINT ( 'NONE',  ( 10.00000000000000000, 50.55374883491396787, -14.16423886937410082 ) ) ;
#13556 = CARTESIAN_POINT ( 'NONE',  ( 18.52753015748618282, 28.92559781766745175, -4.923371831947291888 ) ) ;
#13557 = CARTESIAN_POINT ( 'NONE',  ( 12.11331110855140736, 14.95077488074852923, -8.421032842869449198 ) ) ;
#13558 = CARTESIAN_POINT ( 'NONE',  ( 0.1532563361054083140, 16.00893115100078390, 1.131784320476157264E-15 ) ) ;
#13559 = CARTESIAN_POINT ( 'NONE',  ( 18.72515096720578853, 60.05509018479938277, 6.499999999999877431 ) ) ;
#13560 = CARTESIAN_POINT ( 'NONE',  ( -2.638427012816824124, 12.05059781766744997, 9.846743663894596210 ) ) ;
#13561 = ORIENTED_EDGE ( 'NONE', *, *, #38726, .F. ) ;
#13562 = ORIENTED_EDGE ( 'NONE', *, *, #15724, .T. ) ;
#13563 = ORIENTED_EDGE ( 'NONE', *, *, #77125, .F. ) ;
#13564 = CARTESIAN_POINT ( 'NONE',  ( 10.00000000000000000, 44.75893115100078745, -9.846743663894594434 ) ) ;
#13566 = CARTESIAN_POINT ( 'NONE',  ( 2.035157376598822676, 27.43868534415483396, -7.964842623401177768 ) ) ;
#13565 = CARTESIAN_POINT ( 'NONE',  ( 12.91533473730993009, 16.60535201082150891, -10.88017736071109987 ) ) ;
#13568 = CARTESIAN_POINT ( 'NONE',  ( 19.38216949554541557, 22.24863466993041428, -9.382169495545420901 ) ) ;
#13567 = CARTESIAN_POINT ( 'NONE',  ( 7.361572987183170547, 57.05059781766744464, 9.846743663894590881 ) ) ;
#13569 = CARTESIAN_POINT ( 'NONE',  ( -2.266590686148945544, 1.387082168247301128, -7.082119434687050408 ) ) ;
#13570 = VECTOR ( 'NONE', #79110, 999.9999999999998863 ) ;
#13571 = DIRECTION ( 'NONE',  ( -1.000000000000000000, 0.000000000000000000, 0.000000000000000000 ) ) ;
#13572 = ADVANCED_FACE ( 'NONE', ( #88107 ), #51609, .T. ) ;
#13573 = CARTESIAN_POINT ( 'NONE',  ( 10.00000000000000000, 37.87363466993041783, -12.81628187352647608 ) ) ;
#13574 = ORIENTED_EDGE ( 'NONE', *, *, #40068, .F. ) ;
#13575 = CARTESIAN_POINT ( 'NONE',  ( 19.84674366389459266, 33.71726448433410894, -2.638427012816827677 ) ) ;
#13576 = EDGE_CURVE ( 'NONE', #68711, #11943, #81100, .T. ) ;
#13577 = CARTESIAN_POINT ( 'NONE',  ( -0.8801773607111008646, 3.272018677488171434, 2.915334737309923430 ) ) ;
#13578 = ORIENTED_EDGE ( 'NONE', *, *, #70114, .T. ) ;
#13579 = CARTESIAN_POINT ( 'NONE',  ( 0.5774900079438590739, 2.647018677488171434, -5.440088680355550821 ) ) ;
#13580 = ORIENTED_EDGE ( 'NONE', *, *, #942, .T. ) ;
#13581 = CARTESIAN_POINT ( 'NONE',  ( 10.00000000000000000, 51.81368534415484106, -10.88017736071110342 ) ) ;
#13582 = CARTESIAN_POINT ( 'NONE',  ( 10.00000000000000000, 56.81368534415484106, -10.88017736071110342 ) ) ;
#13583 = CARTESIAN_POINT ( 'NONE',  ( 12.91533473730993009, 46.60535201082150536, -10.88017736071109987 ) ) ;
#13584 = CIRCLE ( 'NONE', #67836, 14.49999999999999822 ) ;
#13585 = CARTESIAN_POINT ( 'NONE',  ( 5.076628168052703671, 1.842264484334118047, 8.527530157486179263 ) ) ;
#13586 = CARTESIAN_POINT ( 'NONE',  ( 7.084665262690076126, 52.02201867748816255, -10.88017736071110164 ) ) ;
#13587 = PLANE ( 'NONE',  #34707 ) ;
#13588 = SURFACE_STYLE_USAGE ( .BOTH. , #21093 ) ;
#13589 = CARTESIAN_POINT ( 'NONE',  ( -5.625000000000007994, 9.284700295649319202, -9.742785792574931492 ) ) ;
#13590 = CARTESIAN_POINT ( 'NONE',  ( 19.84674366389459266, 33.71726448433410894, -2.638427012816827677 ) ) ;
#13591 = ORIENTED_EDGE ( 'NONE', *, *, #9489, .F. ) ;
#13592 = CARTESIAN_POINT ( 'NONE',  ( 7.361572987183170547, 57.05059781766744464, 9.846743663894590881 ) ) ;
#13593 = MECHANICAL_DESIGN_GEOMETRIC_PRESENTATION_REPRESENTATION (  '', ( #63121 ), #48710 ) ;
#13594 = DIRECTION ( 'NONE',  ( 0.000000000000000000, 0.000000000000000000, -1.000000000000000000 ) ) ;
#13595 = CARTESIAN_POINT ( 'NONE',  ( -0.3689425029237881626, 12.42874883491396609, 10.36894250292379027 ) ) ;
#13596 = ORIENTED_EDGE ( 'NONE', *, *, #10179, .F. ) ;
#13597 = EDGE_CURVE ( 'NONE', #48019, #25948, #40660, .T. ) ;
#13598 = FILL_AREA_STYLE ('',( #66091 ) ) ;
#13599 = CARTESIAN_POINT ( 'NONE',  ( -7.116236362341394006, -80.68324313941631942, 3.750000000000001332 ) ) ;
#13600 = DIRECTION ( 'NONE',  ( 1.000000000000000000, 0.000000000000000000, 0.000000000000000000 ) ) ;
#13601 = CARTESIAN_POINT ( 'NONE',  ( 2.035157376598822676, 7.438685344154837509, -7.964842623401177768 ) ) ;
#13602 = CARTESIAN_POINT ( 'NONE',  ( 5.845017550302928022, 15.00000000000000000, 14.89003580495037582 ) ) ;
#13603 = ORIENTED_EDGE ( 'NONE', *, *, #81198, .T. ) ;
#13604 = CARTESIAN_POINT ( 'NONE',  ( 9.240973841163597768, 15.00000000000000000, -11.17382667070370061 ) ) ;
#13605 = CARTESIAN_POINT ( 'NONE',  ( 7.361572987183169658, 49.96726448433410894, -9.846743663894592657 ) ) ;
#13606 = CARTESIAN_POINT ( 'NONE',  ( 10.00000000000000178, 70.00000000000000000, 0.000000000000000000 ) ) ;
#13607 = CARTESIAN_POINT ( 'NONE',  ( 22.81628187352648496, 16.83196800326374998, -3.434112377981050290 ) ) ;
#13609 = EDGE_CURVE ( 'NONE', #58939, #10027, #4633, .T. ) ;
#13608 = CARTESIAN_POINT ( 'NONE',  ( 0.1532563361054100626, 10.80059781766745175, -2.638427012816831230 ) ) ;
#13610 = LINE ( 'NONE', #97138, #98515 ) ;
#13611 = CARTESIAN_POINT ( 'NONE',  ( 19.84674366389459266, 18.30059781766745175, 2.638427012816836559 ) ) ;
#13612 = CARTESIAN_POINT ( 'NONE',  ( 21.09922568453595559, 2.040301336597086568, -6.408140936763230044 ) ) ;
#13613 = TOROIDAL_SURFACE ( 'NONE', #51951, 14.49999999999999822, 0.5000000000000000000 ) ;
#13614 = VERTEX_POINT ( 'NONE', #74083 ) ;
#13615 = CARTESIAN_POINT ( 'NONE',  ( 12.91533473730992121, 9.522018677488171434, 10.88017736071110164 ) ) ;
#13616 = CARTESIAN_POINT ( 'NONE',  ( 17.20831665107776587, 29.13393115100078390, -7.208316651077762316 ) ) ;
#13617 = CARTESIAN_POINT ( 'NONE',  ( 17.96484262340118221, 51.18868534415483396, -7.964842623401177768 ) ) ;
#13619 = CARTESIAN_POINT ( 'NONE',  ( 0.000000000000000000, 91.00000000000000000, 8.000000000000000000 ) ) ;
#13618 = CARTESIAN_POINT ( 'NONE',  ( 19.38216949554541557, 37.24863466993041783, -9.382169495545420901 ) ) ;
#13620 = CARTESIAN_POINT ( 'NONE',  ( 19.42250999205614193, 15.14701867748817143, 5.440088680355555262 ) ) ;
#13621 = CARTESIAN_POINT ( 'NONE',  ( 15.00000000000000000, 77.07179676972447169, 4.250000000000000000 ) ) ;
#13622 = CARTESIAN_POINT ( 'NONE',  ( 13.16767742306549493, 14.95037115937769912, 6.653539137818540006 ) ) ;
#13623 = CARTESIAN_POINT ( 'NONE',  ( 10.00000000000000000, 64.75893115100078035, -9.846743663894594434 ) ) ;
#13624 = CARTESIAN_POINT ( 'NONE',  ( 14.92337183194729633, 27.67559781766745530, 8.527530157486181039 ) ) ;
#13625 = CARTESIAN_POINT ( 'NONE',  ( -10.88017736071109987, -11.72798132251182501, 2.915334737309934532 ) ) ;
#13626 = CARTESIAN_POINT ( 'NONE',  ( 16.40814093676323893, 40.79030133659708923, 11.09922568453595026 ) ) ;
#13627 = CARTESIAN_POINT ( 'NONE',  ( 13.40508947812166873, 4.119406375368599477E-16, -5.527528931046103544 ) ) ;
#13629 = CARTESIAN_POINT ( 'NONE',  ( 13.14228782657344219, 14.63606917158947418, -7.230509711182243393 ) ) ;
#13628 = CARTESIAN_POINT ( 'NONE',  ( 20.88017736071110875, 45.77201867748816966, -2.915334737309920765 ) ) ;
#13630 = CIRCLE ( 'NONE', #58293, 10.09999999999999787 ) ;
#13631 = CARTESIAN_POINT ( 'NONE',  ( 1.847237859018642459, 14.95037103927854538, 14.63711110085122158 ) ) ;
#13632 = CARTESIAN_POINT ( 'NONE',  ( 2.035157376598824452, 43.68868534415484106, 7.964842623401179544 ) ) ;
#13633 = CARTESIAN_POINT ( 'NONE',  ( 2.035157376598822676, 27.43868534415483396, -7.964842623401177768 ) ) ;
#13634 = CARTESIAN_POINT ( 'NONE',  ( 2.603489959281590771, 46.58210964143328425, 6.500000000000003553 ) ) ;
#13635 = CARTESIAN_POINT ( 'NONE',  ( 20.88017736071110164, 60.35535201082151957, 2.915334737309930979 ) ) ;
#13636 = VECTOR ( 'NONE', #51143, 1000.000000000000000 ) ;
#13637 = CARTESIAN_POINT ( 'NONE',  ( 19.84674366389459266, 43.71726448433410894, -2.638427012816827677 ) ) ;
#13638 = CARTESIAN_POINT ( 'NONE',  ( 6.565887622018943937, 60.16530133659707502, 12.81628187352647430 ) ) ;
#13639 = CARTESIAN_POINT ( 'NONE',  ( -1.099225684535947600, 9.540301336597087456, 6.408140936763237150 ) ) ;
#13640 = VERTEX_POINT ( 'NONE', #90080 ) ;
#13641 = CARTESIAN_POINT ( 'NONE',  ( 20.88017736071110164, 25.35535201082150891, 2.915334737309930979 ) ) ;
#13642 = DIRECTION ( 'NONE',  ( 0.000000000000000000, 0.000000000000000000, -1.000000000000000000 ) ) ;
#13643 = CARTESIAN_POINT ( 'NONE',  ( 4.559911319644449179, 13.89701867748817321, 9.422509992056141925 ) ) ;
#13644 = CARTESIAN_POINT ( 'NONE',  ( 0.5774900079438590739, 67.64701867748817676, -5.440088680355550821 ) ) ;
#13645 = CARTESIAN_POINT ( 'NONE',  ( 17.08211943468705840, 20.13708216824730357, -12.26659068614894466 ) ) ;
#13646 = CARTESIAN_POINT ( 'NONE',  ( 0.1532563361054100626, 15.80059781766745353, -2.638427012816831230 ) ) ;
#13647 = CARTESIAN_POINT ( 'NONE',  ( 10.00000000000000178, 57.25893115100078745, 9.846743663894594434 ) ) ;
#13648 = CARTESIAN_POINT ( 'NONE',  ( 19.42250999205614193, 50.14701867748817676, 5.440088680355555262 ) ) ;
#13649 = AXIS2_PLACEMENT_3D ( 'NONE', #97606, #29067, #23078 ) ;
#13650 = DIRECTION ( 'NONE',  ( -0.000000000000000000, 0.000000000000000000, 1.000000000000000000 ) ) ;
#13651 = DIRECTION ( 'NONE',  ( -0.5664062369248259454, 0.000000000000000000, -0.8241261886220204724 ) ) ;
#13652 = EDGE_CURVE ( 'NONE', #87109, #76776, #7694, .T. ) ;
#13653 = VERTEX_POINT ( 'NONE', #61430 ) ;
#13654 = CIRCLE ( 'NONE', #47188, 0.2500000000000002220 ) ;
#13655 = CARTESIAN_POINT ( 'NONE',  ( 8.209432707284774366, 0.5000000000000004441, 12.55409154915492032 ) ) ;
#13656 = CARTESIAN_POINT ( 'NONE',  ( 12.63842701281683034, 42.46726448433412315, 9.846743663894596210 ) ) ;
#13657 =( BOUNDED_CURVE ( )  B_SPLINE_CURVE ( 2, ( #93661, #24690, #16202, #25197, #16694, #25677, #48647, #55673, #86173 ),
 .UNSPECIFIED., .F., .T. ) 
 B_SPLINE_CURVE_WITH_KNOTS ( ( 3, 2, 2, 2, 3 ),
 ( 0.7615695083688026612, 0.7619047619047618625, 0.7678571428571429047, 0.7738095238095238360, 0.7741447773454829262 ),
 .UNSPECIFIED. ) 
 CURVE ( )  GEOMETRIC_REPRESENTATION_ITEM ( )  RATIONAL_B_SPLINE_CURVE ( ( 0.9963778908391753841, 0.9980808541467917072, 1.000000000000000000, 0.9659258262890682012, 1.000000000000000000, 0.9659258262890682012, 1.000000000000000000, 0.9980808541467922623, 0.9963778908391764944 ) ) 
 REPRESENTATION_ITEM ( '' )  );
#13658 = ORIENTED_EDGE ( 'NONE', *, *, #88708, .T. ) ;
#13659 = ORIENTED_EDGE ( 'NONE', *, *, #86431, .F. ) ;
#13660 = VECTOR ( 'NONE', #36857, 1000.000000000000000 ) ;
#13661 = CARTESIAN_POINT ( 'NONE',  ( 13.79529636645031943, 20.34541550158063572, -14.16423886937409904 ) ) ;
#13662 = CARTESIAN_POINT ( 'NONE',  ( 22.26659068614895176, 29.72041550158063572, -7.082119434687042414 ) ) ;
#13663 = CARTESIAN_POINT ( 'NONE',  ( -0.8801773607111008646, 58.27201867748816966, 2.915334737309923430 ) ) ;
#13664 = CARTESIAN_POINT ( 'NONE',  ( -2.266590686148945544, 66.38708216824730357, -7.082119434687050408 ) ) ;
#13665 = CARTESIAN_POINT ( 'NONE',  ( 13.43411237798106583, 2.665301336597086568, -12.81628187352647252 ) ) ;
#13666 = CARTESIAN_POINT ( 'NONE',  ( 2.791683348922237240, 50.38393115100078035, -7.208316651077763204 ) ) ;
#13667 = CARTESIAN_POINT ( 'NONE',  ( -11.17376097873395047, -90.29818107661104420, 4.000000000000000000 ) ) ;
#13669 = CARTESIAN_POINT ( 'NONE',  ( 3.591859063236761518, 9.956968003263753531, 11.09922568453594849 ) ) ;
#13668 = CARTESIAN_POINT ( 'NONE',  ( 20.88017736071110875, 45.77201867748816966, -2.915334737309920765 ) ) ;
#13670 = CARTESIAN_POINT ( 'NONE',  ( 13.79529636645030344, 23.26208216824730002, 14.16423886937410614 ) ) ;
#13671 = CARTESIAN_POINT ( 'NONE',  ( -4.164238869374098151, 56.59541550158063927, -3.795296366450310543 ) ) ;
#13672 = MECHANICAL_DESIGN_GEOMETRIC_PRESENTATION_REPRESENTATION (  '', ( #16894 ), #95089 ) ;
#13673 = CARTESIAN_POINT ( 'NONE',  ( 12.91533473730992121, 19.52201867748816611, 10.88017736071110164 ) ) ;
#13674 = CARTESIAN_POINT ( 'NONE',  ( 17.39651004071838969, 54.08210964143329846, -6.500000000000027534 ) ) ;
#13675 = CARTESIAN_POINT ( 'NONE',  ( 10.00000000000000178, 39.31368534415484106, 10.88017736071110342 ) ) ;
#13676 = CARTESIAN_POINT ( 'NONE',  ( 7.208316651077764980, -27.11606884899921255, 7.208316651077762316 ) ) ;
#13677 = ORIENTED_EDGE ( 'NONE', *, *, #88960, .T. ) ;
#13678 = CARTESIAN_POINT ( 'NONE',  ( 20.10493008474206178, 34.71697413083879269, 6.336235997365760930 ) ) ;
#13679 = ORIENTED_EDGE ( 'NONE', *, *, #25432, .T. ) ;
#13680 = ORIENTED_EDGE ( 'NONE', *, *, #61404, .F. ) ;
#13681 = PRESENTATION_STYLE_ASSIGNMENT (( #80827 ) ) ;
#13682 = CARTESIAN_POINT ( 'NONE',  ( -4.164238869374099039, 46.80374883491397497, 8.674139862899312516E-16 ) ) ;
#13684 = CARTESIAN_POINT ( 'NONE',  ( 18.52753015748618282, 48.92559781766745886, -4.923371831947291888 ) ) ;
#13683 = CARTESIAN_POINT ( 'NONE',  ( 10.00000000000000000, 19.75893115100078390, -9.846743663894594434 ) ) ;
#13685 = CARTESIAN_POINT ( 'NONE',  ( -3.799999999999998934, 1.839999999999999636, 0.000000000000000000 ) ) ;
#13686 = CYLINDRICAL_SURFACE ( 'NONE', #55806, 15.00000000000000000 ) ;
#13687 = CARTESIAN_POINT ( 'NONE',  ( 17.20831665107776587, 2.883931151000785231, 7.208316651077764980 ) ) ;
#13688 = VECTOR ( 'NONE', #38718, 1000.000000000000000 ) ;
#13689 = EDGE_CURVE ( 'NONE', #65696, #4144, #24889, .T. ) ;
#13690 = CARTESIAN_POINT ( 'NONE',  ( -2.816281873526471635, 53.91530133659709634, -3.434112377981056508 ) ) ;
#13691 = CARTESIAN_POINT ( 'NONE',  ( 12.81628187352647252, 26.83196800326376419, -3.434112377981059172 ) ) ;
#13692 = ORIENTED_EDGE ( 'NONE', *, *, #83031, .T. ) ;
#13693 = CARTESIAN_POINT ( 'NONE',  ( 2.917880565312948704, 32.63708216824730357, 12.26659068614894643 ) ) ;
#13694 = EDGE_CURVE ( 'NONE', #21520, #10378, #10520, .T. ) ;
#13695 = CARTESIAN_POINT ( 'NONE',  ( 19.38216949554541557, 27.24863466993041783, -9.382169495545420901 ) ) ;
#13696 = ORIENTED_EDGE ( 'NONE', *, *, #23853, .F. ) ;
#13697 = CARTESIAN_POINT ( 'NONE',  ( -2.816281873526471635, 43.91530133659708923, -3.434112377981056508 ) ) ;
#13698 = CARTESIAN_POINT ( 'NONE',  ( 10.00000000000000178, 37.25893115100078745, 9.846743663894594434 ) ) ;
#13699 = CARTESIAN_POINT ( 'NONE',  ( 0.5774900079438590739, 17.64701867748817321, -5.440088680355550821 ) ) ;
#13700 = CARTESIAN_POINT ( 'NONE',  ( 6.565887622018943937, 60.16530133659707502, 12.81628187352647430 ) ) ;
#13701 = CARTESIAN_POINT ( 'NONE',  ( 9.065164099344453774, 0.5000000000000004441, 11.95084933600773169 ) ) ;
#13702 = CARTESIAN_POINT ( 'NONE',  ( 2.791683348922240793, 46.63393115100077324, 7.208316651077764092 ) ) ;
#13703 = CARTESIAN_POINT ( 'NONE',  ( 0.1532563361054082862, 51.21726448433412315, 2.638427012816831674 ) ) ;
#13704 = AXIS2_PLACEMENT_3D ( 'NONE', #38714, #69213, #739 ) ;
#13706 = ORIENTED_EDGE ( 'NONE', *, *, #66616, .T. ) ;
#13705 = DIRECTION ( 'NONE',  ( -0.9537169507482278208, 0.000000000000000000, 0.3007057995042701770 ) ) ;
#13707 = EDGE_LOOP ( 'NONE', ( #12858, #35700, #64064, #38559 ) ) ;
#13708 = MECHANICAL_DESIGN_GEOMETRIC_PRESENTATION_REPRESENTATION (  '', ( #66149 ), #74356 ) ;
#13709 = CYLINDRICAL_SURFACE ( 'NONE', #23786, 15.00000000000000000 ) ;
#13710 = DIRECTION ( 'NONE',  ( 0.000000000000000000, 0.000000000000000000, 1.000000000000000000 ) ) ;
#13711 = CARTESIAN_POINT ( 'NONE',  ( 17.39651004071841456, 9.082109641433294911, -6.500000000000003553 ) ) ;
#13712 = CARTESIAN_POINT ( 'NONE',  ( -9.000000000000001776, 80.99999999999994316, 2.900000000000001243 ) ) ;
#13713 = CARTESIAN_POINT ( 'NONE',  ( 2.791683348922240793, 16.63393115100078745, 7.208316651077764092 ) ) ;
#13714 = CARTESIAN_POINT ( 'NONE',  ( 19.38216949554541557, 32.24863466993041783, -9.382169495545420901 ) ) ;
#13715 = CARTESIAN_POINT ( 'NONE',  ( 10.70613742633613796, 15.00000000000000000, 9.778988772292906972 ) ) ;
#13716 = ORIENTED_EDGE ( 'NONE', *, *, #38119, .T. ) ;
#13717 = CARTESIAN_POINT ( 'NONE',  ( 12.63842701281683922, 54.55059781766745175, -9.846743663894590881 ) ) ;
#13718 = CARTESIAN_POINT ( 'NONE',  ( 20.15039907845753220, 52.62777174578612716, -6.262539305110077947 ) ) ;
#13719 = CARTESIAN_POINT ( 'NONE',  ( 6.204703633549690345, 20.76208216824730357, -14.16423886937410259 ) ) ;
#13720 = CARTESIAN_POINT ( 'NONE',  ( 14.92337183194729633, 52.67559781766745175, 8.527530157486181039 ) ) ;
#13721 = CARTESIAN_POINT ( 'NONE',  ( 19.38216949554541202, 45.99863466993041072, 9.382169495545424454 ) ) ;
#13723 = PRESENTATION_STYLE_ASSIGNMENT (( #97745 ) ) ;
#13722 = CARTESIAN_POINT ( 'NONE',  ( 12.60589901313222505, 14.49999999999999112, 8.129656208642151327 ) ) ;
#13724 = CARTESIAN_POINT ( 'NONE',  ( 7.361572987183170547, 12.05059781766744997, 9.846743663894590881 ) ) ;
#13725 = CARTESIAN_POINT ( 'NONE',  ( 12.83294900548058415, 0.5000000000000004441, 7.766300266068450142 ) ) ;
#13726 = CARTESIAN_POINT ( 'NONE',  ( 2.791683348922237240, 45.38393115100079456, -7.208316651077763204 ) ) ;
#13728 = ADVANCED_FACE ( 'NONE', ( #59086 ), #12603, .F. ) ;
#13727 = CARTESIAN_POINT ( 'NONE',  ( 15.44008868035555793, 46.39701867748817676, -9.422509992056140149 ) ) ;
#13729 = AXIS2_PLACEMENT_3D ( 'NONE', #71416, #48885, #85421 ) ;
#13730 = CARTESIAN_POINT ( 'NONE',  ( 7.361572987183169658, 34.96726448433411605, -9.846743663894592657 ) ) ;
#13731 = PRODUCT_CONTEXT ( 'NONE', #52544, 'mechanical' ) ;
#13732 = CARTESIAN_POINT ( 'NONE',  ( -10.32896413005680536, 7.245456701841145097, -5.963430220938272797 ) ) ;
#13733 = AXIS2_PLACEMENT_3D ( 'NONE', #86856, #4355, #93858 ) ;
#13734 = CARTESIAN_POINT ( 'NONE',  ( 17.96484262340118221, 46.18868534415484106, -7.964842623401177768 ) ) ;
#13735 = AXIS2_PLACEMENT_3D ( 'NONE', #91284, #22317, #22806 ) ;
#13736 = EDGE_LOOP ( 'NONE', ( #81771, #25165, #44601, #52316, #16114, #93082 ) ) ;
#13737 = CARTESIAN_POINT ( 'NONE',  ( 64.56412365047462742, 26.99999999999999645, -9.500000000000000000 ) ) ;
#13738 = CARTESIAN_POINT ( 'NONE',  ( 10.00000000000000178, 9.313685344154839285, 10.88017736071110342 ) ) ;
#13740 = CARTESIAN_POINT ( 'NONE',  ( 0.5774900079438607392, 48.48035201082150536, 5.440088680355550821 ) ) ;
#13739 = CARTESIAN_POINT ( 'NONE',  ( 19.84674366389459621, 58.50893115100078745, 7.409399052514197653E-17 ) ) ;
#13741 = CARTESIAN_POINT ( 'NONE',  ( 12.84737282370068812, 15.00000000000000000, 9.530079116402468742 ) ) ;
#13742 = CARTESIAN_POINT ( 'NONE',  ( 20.88017736071110519, 60.56368534415484106, 2.639326808657452039E-16 ) ) ;
#13743 = CARTESIAN_POINT ( 'NONE',  ( -13.74344568549460455, 0.2301512731879738205, 5.860030649989552920 ) ) ;
#13745 = FACE_OUTER_BOUND ( 'NONE', #68575, .T. ) ;
#13744 = CARTESIAN_POINT ( 'NONE',  ( 2.035157376598822676, 32.43868534415483396, -7.964842623401177768 ) ) ;
#13746 = CARTESIAN_POINT ( 'NONE',  ( 2.791683348922237240, 10.38393115100078390, -7.208316651077763204 ) ) ;
#13747 = CARTESIAN_POINT ( 'NONE',  ( 14.92337183194729633, 22.67559781766745175, 8.527530157486181039 ) ) ;
#13748 = DIRECTION ( 'NONE',  ( 0.000000000000000000, 0.000000000000000000, 1.000000000000000000 ) ) ;
#13749 = CARTESIAN_POINT ( 'NONE',  ( -12.26659068614894110, 12.22041550158064283, 7.082119434687058401 ) ) ;
#13750 = CARTESIAN_POINT ( 'NONE',  ( 10.00000000000000178, 67.25893115100079456, 9.846743663894594434 ) ) ;
#13751 = CARTESIAN_POINT ( 'NONE',  ( -0.3689425029237881626, 62.42874883491396787, 10.36894250292379027 ) ) ;
#13752 = CARTESIAN_POINT ( 'NONE',  ( -0.3689425029237881626, 12.42874883491396609, 10.36894250292379027 ) ) ;
#13753 = CARTESIAN_POINT ( 'NONE',  ( -0.3689425029237881626, 57.42874883491397497, 10.36894250292379027 ) ) ;
#13754 = CARTESIAN_POINT ( 'NONE',  ( 22.81628187352648496, 1.831968003263753753, -3.434112377981050290 ) ) ;
#13755 = VERTEX_POINT ( 'NONE', #59584 ) ;
#13756 = CARTESIAN_POINT ( 'NONE',  ( 7.361572987183169658, 14.96726448433411960, -9.846743663894592657 ) ) ;
#13757 = CARTESIAN_POINT ( 'NONE',  ( 12.91533473730993009, 16.60535201082150891, -10.88017736071109987 ) ) ;
#13758 = CARTESIAN_POINT ( 'NONE',  ( 18.52753015748618282, 43.92559781766745175, -4.923371831947291888 ) ) ;
#13760 = CARTESIAN_POINT ( 'NONE',  ( -11.82883858055346415, 90.33605471726345115, -7.015824399821311452 ) ) ;
#13759 = CARTESIAN_POINT ( 'NONE',  ( 15.08495336817614607, -0.03417435944610275333, -5.321802168063438643 ) ) ;
#13761 = CARTESIAN_POINT ( 'NONE',  ( 0.000000000000000000, 0.5000000000000004441, 0.000000000000000000 ) ) ;
#13762 = CARTESIAN_POINT ( 'NONE',  ( 2.791683348922240793, 1.633931151000784565, 7.208316651077764092 ) ) ;
#13763 = CARTESIAN_POINT ( 'NONE',  ( 6.565887622018943937, 23.08196800326375708, -12.81628187352647608 ) ) ;
#13764 = CARTESIAN_POINT ( 'NONE',  ( 12.63842701281683034, 32.46726448433412315, 9.846743663894596210 ) ) ;
#13765 = VERTEX_POINT ( 'NONE', #42616 ) ;
#13766 = CARTESIAN_POINT ( 'NONE',  ( 2.791683348922240793, 11.63393115100078568, 7.208316651077764092 ) ) ;
#13767 = B_SPLINE_CURVE_WITH_KNOTS ( 'NONE', 3,
 ( #34618, #80634, #11638, #42153 ),
 .UNSPECIFIED., .F., .F.,
 ( 4, 4 ),
 ( 0.000000000000000000, 0.002562518741975322069 ),
 .UNSPECIFIED. ) ;
#13768 = CARTESIAN_POINT ( 'NONE',  ( 11.35644985441411059, -65.08036738588863557, -4.000000000000000000 ) ) ;
#13769 = DIRECTION ( 'NONE',  ( 0.000000000000000000, 0.000000000000000000, 1.000000000000000000 ) ) ;
#13770 = CARTESIAN_POINT ( 'NONE',  ( -0.8801773607110991993, 7.855352010821504471, -2.915334737309923874 ) ) ;
#13771 = CARTESIAN_POINT ( 'NONE',  ( -0.3689425029237898834, 41.17874883491397497, -10.36894250292378850 ) ) ;
#13772 = CARTESIAN_POINT ( 'NONE',  ( -0.8801773607111009756, 43.06368534415484106, 1.068504757029289695E-15 ) ) ;
#13773 = CARTESIAN_POINT ( 'NONE',  ( 4.559911319644449179, 63.89701867748817676, 9.422509992056141925 ) ) ;
#13774 = CARTESIAN_POINT ( 'NONE',  ( 20.32896413005680714, 40.57879003517447103, -5.963430220938276349 ) ) ;
#13775 = CARTESIAN_POINT ( 'NONE',  ( 10.00000000000000000, 19.75893115100078390, -9.846743663894594434 ) ) ;
#13776 = CARTESIAN_POINT ( 'NONE',  ( 5.076628168052703671, 6.842264484334118713, 8.527530157486179263 ) ) ;
#13777 = CARTESIAN_POINT ( 'NONE',  ( -1.372027372252927480, 1.950157826164670856E-16, -0.5557468924052827441 ) ) ;
#13778 = CARTESIAN_POINT ( 'NONE',  ( 18.52753015748618282, 38.92559781766745175, -4.923371831947291888 ) ) ;
#13779 = AXIS2_PLACEMENT_3D ( 'NONE', #27530, #26547, #72528 ) ;
#13780 = CARTESIAN_POINT ( 'NONE',  ( 17.96484262340118221, 34.93868534415482685, 7.964842623401181321 ) ) ;
#13781 = EDGE_CURVE ( 'NONE', #15284, #16048, #73591, .T. ) ;
#13782 = VERTEX_POINT ( 'NONE', #21104 ) ;
#13783 = CARTESIAN_POINT ( 'NONE',  ( -2.816281873526473856, 64.33196800326376774, 3.434112377981055619 ) ) ;
#13784 = CYLINDRICAL_SURFACE ( 'NONE', #76339, 0.2500000000000002220 ) ;
#13785 = CARTESIAN_POINT ( 'NONE',  ( 14.92337183194729633, 12.67559781766745353, 8.527530157486181039 ) ) ;
#13786 = CARTESIAN_POINT ( 'NONE',  ( 13.43411237798105340, 45.58196800326374643, 12.81628187352647963 ) ) ;
#13788 = CARTESIAN_POINT ( 'NONE',  ( 18.52753015748617571, 33.09226448433411605, 4.923371831947298993 ) ) ;
#13787 = CARTESIAN_POINT ( 'NONE',  ( 17.96484262340118221, 6.188685344154837509, -7.964842623401177768 ) ) ;
#13790 = ADVANCED_FACE ( 'NONE', ( #51603 ), #44583, .T. ) ;
#13789 = FILL_AREA_STYLE ('',( #7287 ) ) ;
#13791 = EDGE_CURVE ( 'NONE', #95455, #75433, #63881, .T. ) ;
#13792 = LINE ( 'NONE', #14298, #11944 ) ;
#13793 = CARTESIAN_POINT ( 'NONE',  ( 10.00000000000000000, 20.55374883491396787, -14.16423886937410082 ) ) ;
#13794 = CARTESIAN_POINT ( 'NONE',  ( 22.26659068614894466, 38.88708216824731068, 7.082119434687054849 ) ) ;
#13795 = CARTESIAN_POINT ( 'NONE',  ( 2.791683348922237240, 40.38393115100078035, -7.208316651077763204 ) ) ;
#13796 = CARTESIAN_POINT ( 'NONE',  ( 8.880000000000000782, 1.116573172248542834E-15, 3.750000000000000000 ) ) ;
#13797 = CARTESIAN_POINT ( 'NONE',  ( 7.084665262690076126, 34.10535201082151247, 10.88017736071109987 ) ) ;
#13798 = CARTESIAN_POINT ( 'NONE',  ( 14.92337183194729633, 7.675597817667451750, 8.527530157486181039 ) ) ;
#13799 = CARTESIAN_POINT ( 'NONE',  ( -3.500000000000000444, 0.08393865084445589764, 3.750000000000000000 ) ) ;
#13800 = VERTEX_POINT ( 'NONE', #77916 ) ;
#13801 = CARTESIAN_POINT ( 'NONE',  ( 6.565887622018943937, 53.08196800326374643, -12.81628187352647608 ) ) ;
#13802 = ORIENTED_EDGE ( 'NONE', *, *, #49376, .T. ) ;
#13803 = ADVANCED_FACE ( 'NONE', ( #15947 ), #61814, .T. ) ;
#13804 = CARTESIAN_POINT ( 'NONE',  ( -0.8801773607110991993, 67.85535201082151957, -2.915334737309923874 ) ) ;
#13805 = COLOUR_RGB ( '', 0.08235294, 0.09019608, 0.10196078) ;
#13806 = EDGE_LOOP ( 'NONE', ( #57212, #74554, #80511, #59788 ) ) ;
#13807 = CARTESIAN_POINT ( 'NONE',  ( -2.266590686148945544, 7.220415501580634832, 7.082119434687048631 ) ) ;
#13808 = CARTESIAN_POINT ( 'NONE',  ( 14.92337183194729633, 7.675597817667451750, 8.527530157486181039 ) ) ;
#13809 = LINE ( 'NONE', #19819, #96837 ) ;
#13810 =( GEOMETRIC_REPRESENTATION_CONTEXT ( 3 ) GLOBAL_UNCERTAINTY_ASSIGNED_CONTEXT ( ( #60114 ) ) GLOBAL_UNIT_ASSIGNED_CONTEXT ( ( #66745, #88752, #35750 ) ) REPRESENTATION_CONTEXT ( 'NONE', 'WORKASPACE' ) );
#13811 = ORIENTED_EDGE ( 'NONE', *, *, #2089, .F. ) ;
#13812 = AXIS2_PLACEMENT_3D ( 'NONE', #30275, #8767, #31754 ) ;
#13813 = CARTESIAN_POINT ( 'NONE',  ( 4.559911319644449179, 12.23035201082150536, -9.422509992056141925 ) ) ;
#13814 = EDGE_CURVE ( 'NONE', #32242, #29178, #47535, .T. ) ;
#13815 = VECTOR ( 'NONE', #72593, 1000.000000000000000 ) ;
#13816 = ORIENTED_EDGE ( 'NONE', *, *, #55674, .F. ) ;
#13817 = CARTESIAN_POINT ( 'NONE',  ( 4.559911319644449179, 38.89701867748817676, 9.422509992056141925 ) ) ;
#13818 = LINE ( 'NONE', #15800, #55269 ) ;
#13819 = ORIENTED_EDGE ( 'NONE', *, *, #88208, .F. ) ;
#13820 = EDGE_CURVE ( 'NONE', #37993, #58317, #28408, .T. ) ;
#13821 = CARTESIAN_POINT ( 'NONE',  ( 17.20831665107776587, 64.13393115100079456, -7.208316651077762316 ) ) ;
#13822 = ORIENTED_EDGE ( 'NONE', *, *, #80963, .T. ) ;
#13823 = CARTESIAN_POINT ( 'NONE',  ( 12.91533473730992121, 64.52201867748817676, 10.88017736071110164 ) ) ;
#13824 = FACE_OUTER_BOUND ( 'NONE', #98594, .T. ) ;
#13825 = CARTESIAN_POINT ( 'NONE',  ( 13.43411237798105340, 35.58196800326375353, 12.81628187352647963 ) ) ;
#13827 = CARTESIAN_POINT ( 'NONE',  ( -0.1503990784575275907, 58.10158574516644592, 6.262539305110076171 ) ) ;
#13826 = CARTESIAN_POINT ( 'NONE',  ( 2.035157376598822676, 27.43868534415483396, -7.964842623401177768 ) ) ;
#13828 = CARTESIAN_POINT ( 'NONE',  ( 17.20831665107776587, 2.883931151000785231, 7.208316651077764980 ) ) ;
#13829 = CARTESIAN_POINT ( 'NONE',  ( 2.035157376598822676, 12.43868534415483751, -7.964842623401177768 ) ) ;
#13830 = TOROIDAL_SURFACE ( 'NONE', #61772, 14.49999999999999822, 0.5000000000000000000 ) ;
#13831 = ORIENTED_EDGE ( 'NONE', *, *, #45198, .F. ) ;
#13832 = STYLED_ITEM ( 'NONE', ( #92071 ), #38078 ) ;
#13833 = CARTESIAN_POINT ( 'NONE',  ( -2.816281873526471635, 48.91530133659708213, -3.434112377981056508 ) ) ;
#13834 = CARTESIAN_POINT ( 'NONE',  ( 7.084665262690076126, 49.10535201082149825, 10.88017736071109987 ) ) ;
#13835 = CARTESIAN_POINT ( 'NONE',  ( 19.50000000000000355, 98.59912998021083297, 5.000000000000000000 ) ) ;
#13836 = CARTESIAN_POINT ( 'NONE',  ( 3.591859063236761518, 59.95696800326375353, 11.09922568453594849 ) ) ;
#13837 = CARTESIAN_POINT ( 'NONE',  ( -0.8801773607111008646, 43.27201867748817676, 2.915334737309923430 ) ) ;
#13838 = CARTESIAN_POINT ( 'NONE',  ( 14.92337183194729988, 59.34226448433412315, -8.527530157486177487 ) ) ;
#13839 = DIRECTION ( 'NONE',  ( 0.7009092642998574485, 0.000000000000000000, -0.7132504491541751257 ) ) ;
#13840 = CARTESIAN_POINT ( 'NONE',  ( 10.00000000000000000, 14.75893115100078568, -9.846743663894594434 ) ) ;
#13841 = CARTESIAN_POINT ( 'NONE',  ( -2.816281873526473856, 9.123634669930421381, 9.499525473075851096E-16 ) ) ;
#13843 = CARTESIAN_POINT ( 'NONE',  ( 10.00000000000000000, 64.75893115100078035, -9.846743663894594434 ) ) ;
#13842 = CARTESIAN_POINT ( 'NONE',  ( -13.79358826900837265, 90.89928960263274860, -7.799418555803335984 ) ) ;
#13844 = CARTESIAN_POINT ( 'NONE',  ( 0.5774900079438607392, 38.48035201082150536, 5.440088680355550821 ) ) ;
#13845 = CARTESIAN_POINT ( 'NONE',  ( 0.1532563361054100626, 50.80059781766745175, -2.638427012816831230 ) ) ;
#13846 = TOROIDAL_SURFACE ( 'NONE', #69742, 2.250000000000001332, 0.2500000000000000000 ) ;
#13847 =( NAMED_UNIT ( * ) SI_UNIT ( $, .STERADIAN. ) SOLID_ANGLE_UNIT ( ) );
#13848 = CARTESIAN_POINT ( 'NONE',  ( 0.1532563361054100626, 15.80059781766745353, -2.638427012816831230 ) ) ;
#13849 = CARTESIAN_POINT ( 'NONE',  ( 17.20831665107776587, 7.883931151000784787, 7.208316651077764980 ) ) ;
#13850 = EDGE_CURVE ( 'NONE', #7375, #32515, #70213, .T. ) ;
#13852 = ORIENTED_EDGE ( 'NONE', *, *, #48083, .T. ) ;
#13851 = CARTESIAN_POINT ( 'NONE',  ( -2.816281873526473856, -0.6680319967362464695, 3.434112377981055619 ) ) ;
#13853 = CARTESIAN_POINT ( 'NONE',  ( -10.76493118081697276, 15.00000000000000711, 9.902252441915640802 ) ) ;
#13854 = CARTESIAN_POINT ( 'NONE',  ( 5.076628168052704559, 60.17559781766745175, -8.527530157486179263 ) ) ;
#13855 = CARTESIAN_POINT ( 'NONE',  ( 22.81628187352648496, 41.83196800326375353, -3.434112377981050290 ) ) ;
#13856 = CARTESIAN_POINT ( 'NONE',  ( 0.1532563361054100626, 35.80059781766745175, -2.638427012816831230 ) ) ;
#13857 = CARTESIAN_POINT ( 'NONE',  ( -45.94000000000000483, 103.7452903794826824, -5.529860068218139801 ) ) ;
#13858 = CARTESIAN_POINT ( 'NONE',  ( 6.204703633549690345, 67.84541550158060375, 14.16423886937410082 ) ) ;
#13859 = CARTESIAN_POINT ( 'NONE',  ( 7.361572987183169658, 34.96726448433411605, -9.846743663894592657 ) ) ;
#13860 = VECTOR ( 'NONE', #49916, 1000.000000000000000 ) ;
#13861 = ORIENTED_EDGE ( 'NONE', *, *, #90819, .T. ) ;
#13862 = LINE ( 'NONE', #29827, #83968 ) ;
#13863 = CARTESIAN_POINT ( 'NONE',  ( -0.8801773607111009756, 8.063685344154837509, 1.068504757029289695E-15 ) ) ;
#13864 = DIRECTION ( 'NONE',  ( 0.000000000000000000, 0.000000000000000000, 1.000000000000000000 ) ) ;
#13865 = CARTESIAN_POINT ( 'NONE',  ( 17.96484262340118221, 21.18868534415483396, -7.964842623401177768 ) ) ;
#13866 = CARTESIAN_POINT ( 'NONE',  ( 22.26659068614895176, 54.72041550158063217, -7.082119434687042414 ) ) ;
#13868 = LINE ( 'NONE', #38837, #47884 ) ;
#13867 = CARTESIAN_POINT ( 'NONE',  ( -4.164238869374098151, 56.59541550158063927, -3.795296366450310543 ) ) ;
#13869 = FACE_OUTER_BOUND ( 'NONE', #97836, .T. ) ;
#13870 = CARTESIAN_POINT ( 'NONE',  ( 19.84674366389459266, 13.30059781766745353, 2.638427012816836559 ) ) ;
#13871 = CARTESIAN_POINT ( 'NONE',  ( 21.09922568453594849, 6.206968003263753531, 6.408140936763242479 ) ) ;
#13872 = EDGE_LOOP ( 'NONE', ( #80023, #45997, #3507, #3237 ) ) ;
#13873 = DIRECTION ( 'NONE',  ( -0.000000000000000000, 0.000000000000000000, 1.000000000000000000 ) ) ;
#13874 = CARTESIAN_POINT ( 'NONE',  ( 18.52753015748617571, 58.09226448433411605, 4.923371831947298993 ) ) ;
#13875 = CARTESIAN_POINT ( 'NONE',  ( 8.731067818237031375, 2.813309369127509285, -8.731067818237036704 ) ) ;
#13876 = CARTESIAN_POINT ( 'NONE',  ( 10.00000000000000000, 64.75893115100078035, -9.846743663894594434 ) ) ;
#13877 = CARTESIAN_POINT ( 'NONE',  ( 24.16423886937409904, 9.095415501580633943, 3.795296366450317205 ) ) ;
#13878 = CARTESIAN_POINT ( 'NONE',  ( 10.00000000000000000, 19.75893115100078390, -9.846743663894594434 ) ) ;
#13879 = FACE_OUTER_BOUND ( 'NONE', #94221, .T. ) ;
#13880 = ORIENTED_EDGE ( 'NONE', *, *, #42450, .T. ) ;
#13881 = CARTESIAN_POINT ( 'NONE',  ( 24.16423886937409904, 34.09541550158064638, 3.795296366450317205 ) ) ;
#13882 = CIRCLE ( 'NONE', #31417, 3.000000000000000888 ) ;
#13883 = CARTESIAN_POINT ( 'NONE',  ( 1.472469842513823179, 5.592264484334118713, -4.923371831947296329 ) ) ;
#13885 = CARTESIAN_POINT ( 'NONE',  ( -11.25000000000000178, 7.921802177851544613, 3.951965214266261022E-15 ) ) ;
#13884 = CARTESIAN_POINT ( 'NONE',  ( -7.232415441807423129, -88.12698951299773853, -3.750000000000000000 ) ) ;
#13886 = CARTESIAN_POINT ( 'NONE',  ( 4.559911319644449179, 37.23035201082150536, -9.422509992056141925 ) ) ;
#13887 = CARTESIAN_POINT ( 'NONE',  ( 6.565887622018943937, 40.16530133659708923, 12.81628187352647430 ) ) ;
#13888 = CARTESIAN_POINT ( 'NONE',  ( 2.035157376598822676, 7.438685344154837509, -7.964842623401177768 ) ) ;
#13889 = CARTESIAN_POINT ( 'NONE',  ( -2.816281873526473856, 34.12363466993042493, 9.499525473075851096E-16 ) ) ;
#13890 = CARTESIAN_POINT ( 'NONE',  ( 22.81628187352648496, 56.83196800326374643, -3.434112377981050290 ) ) ;
#13891 = ORIENTED_EDGE ( 'NONE', *, *, #92635, .F. ) ;
#13892 = CARTESIAN_POINT ( 'NONE',  ( -14.26139399674456776, 15.00000000000000000, 2.619664342929695966 ) ) ;
#13893 = DIRECTION ( 'NONE',  ( 0.000000000000000000, 0.000000000000000000, 1.000000000000000000 ) ) ;
#13894 = CARTESIAN_POINT ( 'NONE',  ( 24.16423886937410614, 34.30374883491396787, 8.672049930838204340E-16 ) ) ;
#13895 = CARTESIAN_POINT ( 'NONE',  ( 4.559911319644449179, 7.230352010821504471, -9.422509992056141925 ) ) ;
#13896 = CARTESIAN_POINT ( 'NONE',  ( 17.96484262340118221, 24.93868534415484461, 7.964842623401181321 ) ) ;
#13897 = DIRECTION ( 'NONE',  ( 0.9999619230641714207, 0.000000000000000000, -0.008726535498360278933 ) ) ;
#13898 = SURFACE_STYLE_USAGE ( .BOTH. , #51894 ) ;
#13899 = CARTESIAN_POINT ( 'NONE',  ( 12.91533473730993009, 56.60535201082151247, -10.88017736071109987 ) ) ;
#13900 = CARTESIAN_POINT ( 'NONE',  ( -0.8801773607111009756, 53.06368534415484106, 1.068504757029289695E-15 ) ) ;
#13901 = CARTESIAN_POINT ( 'NONE',  ( 16.40814093676324603, 32.45696800326375353, -11.09922568453594671 ) ) ;
#13902 = CARTESIAN_POINT ( 'NONE',  ( 0.000000000000000000, 2.500000000000005773, 0.000000000000000000 ) ) ;
#13903 = CARTESIAN_POINT ( 'NONE',  ( -14.29730467489535428, 3.987535082655999417E-16, 2.416004766803123260 ) ) ;
#13904 = CARTESIAN_POINT ( 'NONE',  ( 12.63842701281683034, 17.46726448433411250, 9.846743663894596210 ) ) ;
#13905 = EDGE_CURVE ( 'NONE', #41505, #21427, #73244, .T. ) ;
#13906 =( GEOMETRIC_REPRESENTATION_CONTEXT ( 3 ) GLOBAL_UNCERTAINTY_ASSIGNED_CONTEXT ( ( #83121 ) ) GLOBAL_UNIT_ASSIGNED_CONTEXT ( ( #64268, #86802, #77803 ) ) REPRESENTATION_CONTEXT ( 'NONE', 'WORKASPACE' ) );
#13907 = CARTESIAN_POINT ( 'NONE',  ( 0.5774900079438607392, 58.48035201082151247, 5.440088680355550821 ) ) ;
#13908 = VECTOR ( 'NONE', #3110, 1000.000000000000000 ) ;
#13909 = ADVANCED_FACE ( 'NONE', ( #82332 ), #82260, .T. ) ;
#13910 = AXIS2_PLACEMENT_3D ( 'NONE', #51491, #74979, #27994 ) ;
#13911 = CARTESIAN_POINT ( 'NONE',  ( 22.81628187352647785, 21.62363466993041783, 6.195893100308588602E-16 ) ) ;
#13912 = SURFACE_STYLE_USAGE ( .BOTH. , #67396 ) ;
#13913 = CARTESIAN_POINT ( 'NONE',  ( 12.91533473730992121, 14.52201867748817143, 10.88017736071110164 ) ) ;
#13914 = EDGE_CURVE ( 'NONE', #25080, #83450, #39734, .T. ) ;
#13915 = CARTESIAN_POINT ( 'NONE',  ( 1.472469842513823179, 36.42559781766745175, 4.923371831947296329 ) ) ;
#13916 = CARTESIAN_POINT ( 'NONE',  ( -2.816281873526473856, 54.12363466993041783, 9.499525473075851096E-16 ) ) ;
#13917 = CARTESIAN_POINT ( 'NONE',  ( 2.791683348922237240, 20.38393115100078745, -7.208316651077763204 ) ) ;
#13918 = CARTESIAN_POINT ( 'NONE',  ( -2.266590686148945544, 11.38708216824730179, -7.082119434687050408 ) ) ;
#13919 = CARTESIAN_POINT ( 'NONE',  ( 18.18329248733315140, 27.60290668512023515, 6.499999999999997335 ) ) ;
#13920 = CARTESIAN_POINT ( 'NONE',  ( 0.5774900079438607392, 23.48035201082150536, 5.440088680355550821 ) ) ;
#13922 = CARTESIAN_POINT ( 'NONE',  ( 2.917880565312948704, 27.63708216824730357, 12.26659068614894643 ) ) ;
#13921 =( NAMED_UNIT ( * ) SI_UNIT ( $, .STERADIAN. ) SOLID_ANGLE_UNIT ( ) );
#13923 = CARTESIAN_POINT ( 'NONE',  ( 2.791683348922237240, 50.38393115100078035, -7.208316651077763204 ) ) ;
#13924 = CARTESIAN_POINT ( 'NONE',  ( -0.8801773607111008646, 33.27201867748817676, 2.915334737309923430 ) ) ;
#13925 = CARTESIAN_POINT ( 'NONE',  ( 17.96484262340118221, 19.93868534415484106, 7.964842623401181321 ) ) ;
#13926 = ORIENTED_EDGE ( 'NONE', *, *, #85924, .T. ) ;
#13927 = COLOUR_RGB ( '', 0.72549020, 0.75294118, 0.79215686) ;
#13928 = CARTESIAN_POINT ( 'NONE',  ( 4.559911319644449179, 22.23035201082150536, -9.422509992056141925 ) ) ;
#13929 = EDGE_CURVE ( 'NONE', #71042, #96104, #92487, .T. ) ;
#13930 = CARTESIAN_POINT ( 'NONE',  ( 6.565887622018943937, 48.08196800326375353, -12.81628187352647608 ) ) ;
#13931 = CARTESIAN_POINT ( 'NONE',  ( 0.5774900079438590739, 32.64701867748816966, -5.440088680355550821 ) ) ;
#13933 = CARTESIAN_POINT ( 'NONE',  ( 17.96484262340118221, 39.93868534415484106, 7.964842623401181321 ) ) ;
#13932 = CARTESIAN_POINT ( 'NONE',  ( 0.1532563361054083140, 46.00893115100079456, 1.131784320476157264E-15 ) ) ;
#13934 = EDGE_LOOP ( 'NONE', ( #95048, #38925, #90566, #3895, #10493, #91293 ) ) ;
#13935 = CARTESIAN_POINT ( 'NONE',  ( 18.52753015748617571, 58.09226448433411605, 4.923371831947298993 ) ) ;
#13936 = CARTESIAN_POINT ( 'NONE',  ( 0.5774900079438607392, 43.48035201082151247, 5.440088680355550821 ) ) ;
#13937 = FACE_OUTER_BOUND ( 'NONE', #41254, .T. ) ;
#13938 = DIRECTION ( 'NONE',  ( 0.000000000000000000, 1.000000000000000000, 0.000000000000000000 ) ) ;
#13939 = CARTESIAN_POINT ( 'NONE',  ( 20.36894250292379738, 49.92874883491396787, -10.36894250292379027 ) ) ;
#13940 = CARTESIAN_POINT ( 'NONE',  ( -0.8801773607110991993, 52.85535201082151247, -2.915334737309923874 ) ) ;
#13941 = CARTESIAN_POINT ( 'NONE',  ( 0.1532563361054083140, 66.00893115100079456, 1.131784320476157264E-15 ) ) ;
#13942 = TOROIDAL_SURFACE ( 'NONE', #28337, 14.49999999999999822, 0.5000000000000000000 ) ;
#13943 = CARTESIAN_POINT ( 'NONE',  ( 26.00000000000000355, 35.99999999999997158, -10.00000000000000000 ) ) ;
#13944 = CARTESIAN_POINT ( 'NONE',  ( 5.076628168052704559, 65.17559781766745175, -8.527530157486179263 ) ) ;
#13945 =( NAMED_UNIT ( * ) SI_UNIT ( $, .STERADIAN. ) SOLID_ANGLE_UNIT ( ) );
#13946 = CARTESIAN_POINT ( 'NONE',  ( 1.472469842513823179, 15.59226448433411960, -4.923371831947296329 ) ) ;
#13947 = VERTEX_POINT ( 'NONE', #50433 ) ;
#13948 = EDGE_CURVE ( 'NONE', #25434, #31259, #13951, .T. ) ;
#13949 = CARTESIAN_POINT ( 'NONE',  ( 18.52753015748617571, 28.09226448433411960, 4.923371831947298993 ) ) ;
#13950 = CARTESIAN_POINT ( 'NONE',  ( -11.09922568453595382, -16.29303199673624292, -6.408140936763226492 ) ) ;
#13951 =( BOUNDED_CURVE ( )  B_SPLINE_CURVE ( 2, ( #19455, #65431, #95955, #33452, #12929, #27436, #19940, #80942, #35431 ),
 .UNSPECIFIED., .F., .T. ) 
 B_SPLINE_CURVE_WITH_KNOTS ( ( 3, 2, 2, 2, 3 ),
 ( 0.8329980797973741691, 0.8333333333333333703, 0.8392857142857143016, 0.8452380952380952328, 0.8455733487740543231 ),
 .UNSPECIFIED. ) 
 CURVE ( )  GEOMETRIC_REPRESENTATION_ITEM ( )  RATIONAL_B_SPLINE_CURVE ( ( 0.9963778908391753841, 0.9980808541467917072, 1.000000000000000000, 0.9659258262890682012, 1.000000000000000000, 0.9659258262890682012, 1.000000000000000000, 0.9980808541467922623, 0.9963778908391764944 ) ) 
 REPRESENTATION_ITEM ( '' )  );
#13952 = CARTESIAN_POINT ( 'NONE',  ( 20.88017736071110164, 20.35535201082150891, 2.915334737309930979 ) ) ;
#13953 = CARTESIAN_POINT ( 'NONE',  ( 2.791683348922237240, 25.38393115100078390, -7.208316651077763204 ) ) ;
#13954 = CARTESIAN_POINT ( 'NONE',  ( -1.099225684535947600, 8.706968003263753531, -6.408140936763238038 ) ) ;
#13956 = CARTESIAN_POINT ( 'NONE',  ( -0.8801773607111009756, 63.06368534415484106, 1.068504757029289695E-15 ) ) ;
#13955 = CARTESIAN_POINT ( 'NONE',  ( -0.8801773607111008646, 68.27201867748817676, 2.915334737309923430 ) ) ;
#13958 = CARTESIAN_POINT ( 'NONE',  ( -2.816281873526473856, 59.33196800326374643, 3.434112377981055619 ) ) ;
#13957 = CARTESIAN_POINT ( 'NONE',  ( -0.8801773607111009756, 33.06368534415484106, 1.068504757029289695E-15 ) ) ;
#13959 = CARTESIAN_POINT ( 'NONE',  ( -2.266590686148945544, 51.38708216824730357, -7.082119434687050408 ) ) ;
#13960 = EDGE_CURVE ( 'NONE', #13640, #1529, #3003, .T. ) ;
#13961 = CARTESIAN_POINT ( 'NONE',  ( 20.15039907845753220, 34.72266099184918176, 6.262539305110077059 ) ) ;
#13962 = ORIENTED_EDGE ( 'NONE', *, *, #91312, .F. ) ;
#13963 = CARTESIAN_POINT ( 'NONE',  ( 0.6178305044545838731, 14.74863466993041783, 9.382169495545420901 ) ) ;
#13964 = CARTESIAN_POINT ( 'NONE',  ( 2.035157376598824452, 8.688685344154839285, 7.964842623401179544 ) ) ;
#13965 = CARTESIAN_POINT ( 'NONE',  ( -0.8801773607111009756, 43.06368534415484106, 1.068504757029289695E-15 ) ) ;
#13966 = B_SPLINE_CURVE_WITH_KNOTS ( 'NONE', 3,
 ( #47919, #11403, #78424, #64390, #49396, #32919 ),
 .UNSPECIFIED., .F., .F.,
 ( 4, 2, 4 ),
 ( -2.009308255747123417E-05, 0.0003744380149044849223, 0.0007689691123664410110 ),
 .UNSPECIFIED. ) ;
#13967 = LINE ( 'NONE', #68445, #77690 ) ;
#13968 = ORIENTED_EDGE ( 'NONE', *, *, #86479, .T. ) ;
#13969 = CARTESIAN_POINT ( 'NONE',  ( 19.42250999205614548, 60.98035201082151247, -5.440088680355545492 ) ) ;
#13970 = CARTESIAN_POINT ( 'NONE',  ( 5.076628168052703671, 31.84226448433412315, 8.527530157486179263 ) ) ;
#13971 = CARTESIAN_POINT ( 'NONE',  ( 10.00000000000000000, 19.75893115100078390, -9.846743663894594434 ) ) ;
#13972 = CARTESIAN_POINT ( 'NONE',  ( 14.92337183194729633, 12.67559781766745353, 8.527530157486181039 ) ) ;
#13974 = CARTESIAN_POINT ( 'NONE',  ( -2.816281873526471635, 38.91530133659708213, -3.434112377981056508 ) ) ;
#13973 = CARTESIAN_POINT ( 'NONE',  ( -7.121341127240343738, -73.24353698637879972, 2.500000000000000000 ) ) ;
#13977 = CARTESIAN_POINT ( 'NONE',  ( 0.1089645850228807833, 23.16234555792570760, 6.479102184480781013 ) ) ;
#13976 = TOROIDAL_SURFACE ( 'NONE', #95397, 14.49999999999999822, 0.5000000000000000000 ) ;
#13975 = CARTESIAN_POINT ( 'NONE',  ( 14.92337183194729988, 4.342264484334117824, -8.527530157486177487 ) ) ;
#13978 = CARTESIAN_POINT ( 'NONE',  ( 11.29389914936710859, -89.89072489378423825, 3.750000000000000000 ) ) ;
#13980 = VERTEX_POINT ( 'NONE', #94459 ) ;
#13979 = CARTESIAN_POINT ( 'NONE',  ( 2.791683348922237240, 30.38393115100078390, -7.208316651077763204 ) ) ;
#13981 = CIRCLE ( 'NONE', #28313, 3.690000000000000391 ) ;
#13982 = CARTESIAN_POINT ( 'NONE',  ( 6.565887622018943937, 58.08196800326376064, -12.81628187352647608 ) ) ;
#13983 = CARTESIAN_POINT ( 'NONE',  ( 4.645843784090632589, -0.8374430341443435122, 3.999999999999999112 ) ) ;
#13984 = CARTESIAN_POINT ( 'NONE',  ( 12.63842701281683034, 62.46726448433410894, 9.846743663894596210 ) ) ;
#13985 = CARTESIAN_POINT ( 'NONE',  ( -2.266590686148945544, 27.22041550158063572, 7.082119434687048631 ) ) ;
#13986 = CARTESIAN_POINT ( 'NONE',  ( 11.36220558718857099, 4.586546245355948473E-16, 9.008345252845320061 ) ) ;
#13987 = CARTESIAN_POINT ( 'NONE',  ( 13.79529636645031943, 25.34541550158063572, -14.16423886937409904 ) ) ;
#13988 = CARTESIAN_POINT ( 'NONE',  ( 13.79529636645030344, 48.26208216824728936, 14.16423886937410614 ) ) ;
#13989 = EDGE_CURVE ( 'NONE', #62860, #26361, #59386, .T. ) ;
#13990 = CARTESIAN_POINT ( 'NONE',  ( -2.266590686148945544, 12.22041550158063394, 7.082119434687048631 ) ) ;
#13992 = CARTESIAN_POINT ( 'NONE',  ( -13.73837289480035651, 90.95369347093435408, -7.920836650016501501 ) ) ;
#13991 = CARTESIAN_POINT ( 'NONE',  ( 2.917880565312948704, 17.63708216824730357, 12.26659068614894643 ) ) ;
#13993 = CARTESIAN_POINT ( 'NONE',  ( 15.44008868035555260, 49.73035201082150536, 9.422509992056143702 ) ) ;
#13994 = CARTESIAN_POINT ( 'NONE',  ( 14.88232117145529720, 0.5000000000000004441, 1.875237731503240024 ) ) ;
#13995 = CARTESIAN_POINT ( 'NONE',  ( 0.1532563361054100626, 30.80059781766744820, -2.638427012816831230 ) ) ;
#13997 = CARTESIAN_POINT ( 'NONE',  ( 18.52753015748617571, 33.09226448433411605, 4.923371831947298993 ) ) ;
#13996 = CARTESIAN_POINT ( 'NONE',  ( 2.035157376598822676, 67.43868534415484817, -7.964842623401177768 ) ) ;
#13998 = CARTESIAN_POINT ( 'NONE',  ( 15.44008868035555260, 24.73035201082150891, 9.422509992056143702 ) ) ;
#13999 = CARTESIAN_POINT ( 'NONE',  ( 3.591859063236761518, 59.95696800326375353, 11.09922568453594849 ) ) ;
#14000 = CARTESIAN_POINT ( 'NONE',  ( 5.076628168052704559, 55.17559781766745175, -8.527530157486179263 ) ) ;
#14001 = EDGE_CURVE ( 'NONE', #72372, #80582, #4444, .T. ) ;
#14002 = CARTESIAN_POINT ( 'NONE',  ( 22.81628187352648496, 46.83196800326376064, -3.434112377981050290 ) ) ;
#14003 = CARTESIAN_POINT ( 'NONE',  ( -10.36894250292378317, -17.57125116508602503, 10.36894250292379560 ) ) ;
#14004 = CARTESIAN_POINT ( 'NONE',  ( -0.8801773607110991993, 37.85535201082151247, -2.915334737309923874 ) ) ;
#14005 = CARTESIAN_POINT ( 'NONE',  ( 2.791683348922237240, 35.38393115100079456, -7.208316651077763204 ) ) ;
#14006 = CARTESIAN_POINT ( 'NONE',  ( -2.266590686148945544, 21.38708216824730357, -7.082119434687050408 ) ) ;
#14007 = ORIENTED_EDGE ( 'NONE', *, *, #85898, .T. ) ;
#14008 = CARTESIAN_POINT ( 'NONE',  ( 20.88017736071110875, 60.77201867748817676, -2.915334737309920765 ) ) ;
#14009 = CARTESIAN_POINT ( 'NONE',  ( 2.035157376598824452, 63.68868534415484106, 7.964842623401179544 ) ) ;
#14010 = CARTESIAN_POINT ( 'NONE',  ( 24.16423886937410614, 54.30374883491396787, 8.672049930838204340E-16 ) ) ;
#14011 = CARTESIAN_POINT ( 'NONE',  ( 7.361572987183169658, 64.96726448433412315, -9.846743663894592657 ) ) ;
#14012 = CARTESIAN_POINT ( 'NONE',  ( -12.34086200392816757, 15.00000000000000000, -7.125000000000143885 ) ) ;
#14013 = CARTESIAN_POINT ( 'NONE',  ( 2.035157376598824452, 48.68868534415483396, 7.964842623401179544 ) ) ;
#14014 = CARTESIAN_POINT ( 'NONE',  ( -0.9082943533638283551, 15.00000000000000000, 14.47152380945581918 ) ) ;
#14015 = AXIS2_PLACEMENT_3D ( 'NONE', #89720, #46206, #30198 ) ;
#14016 = CARTESIAN_POINT ( 'NONE',  ( 22.81628187352647785, 31.62363466993042138, 6.195893100308588602E-16 ) ) ;
#14017 = CARTESIAN_POINT ( 'NONE',  ( -2.915334737309917656, 24.10535201082151247, 10.88017736071110164 ) ) ;
#14018 = CARTESIAN_POINT ( 'NONE',  ( -0.8801773607111009756, 13.06368534415483929, 1.068504757029289695E-15 ) ) ;
#14019 = CARTESIAN_POINT ( 'NONE',  ( 15.44008868035555260, 14.73035201082150536, 9.422509992056143702 ) ) ;
#14020 = CARTESIAN_POINT ( 'NONE',  ( 0.1532563361054100626, 45.80059781766745886, -2.638427012816831230 ) ) ;
#14021 = CARTESIAN_POINT ( 'NONE',  ( 21.09922568453595559, 52.04030133659708923, -6.408140936763230044 ) ) ;
#14022 = SURFACE_SIDE_STYLE ('',( #37013 ) ) ;
#14023 = ORIENTED_EDGE ( 'NONE', *, *, #98651, .F. ) ;
#14024 = CARTESIAN_POINT ( 'NONE',  ( -0.8801773607111009756, 23.06368534415484106, 1.068504757029289695E-15 ) ) ;
#14025 = CARTESIAN_POINT ( 'NONE',  ( -1.099225684535947600, -0.4596986634029132657, 6.408140936763237150 ) ) ;
#14026 = CARTESIAN_POINT ( 'NONE',  ( -13.40508947812168827, 15.00000000000000000, 5.527528931045992522 ) ) ;
#14027 = CARTESIAN_POINT ( 'NONE',  ( 12.63842701281683034, 7.467264484334118713, 9.846743663894596210 ) ) ;
#14028 = AXIS2_PLACEMENT_3D ( 'NONE', #84152, #15658, #46141 ) ;
#14029 = EDGE_CURVE ( 'NONE', #92036, #16571, #65899, .T. ) ;
#14030 = CARTESIAN_POINT ( 'NONE',  ( 19.84674366389459266, 53.30059781766744464, 2.638427012816836559 ) ) ;
#14031 = CARTESIAN_POINT ( 'NONE',  ( 19.42250999205614193, 35.14701867748816966, 5.440088680355555262 ) ) ;
#14032 = EDGE_CURVE ( 'NONE', #76760, #1168, #87599, .T. ) ;
#14033 = CARTESIAN_POINT ( 'NONE',  ( -1.099225684535947600, 4.540301336597087456, 6.408140936763237150 ) ) ;
#14035 = CARTESIAN_POINT ( 'NONE',  ( 11.92686044187657224, 9.953790035174483464, 3.195792623639526209 ) ) ;
#14034 = CARTESIAN_POINT ( 'NONE',  ( 20.88017736071110519, 45.56368534415484106, 2.639326808657452039E-16 ) ) ;
#14036 = CARTESIAN_POINT ( 'NONE',  ( 19.38216949554541202, 55.99863466993041072, 9.382169495545424454 ) ) ;
#14037 = EDGE_LOOP ( 'NONE', ( #18427, #52784, #70332, #4044 ) ) ;
#14038 = CARTESIAN_POINT ( 'NONE',  ( 12.91533473730992121, 59.52201867748816966, 10.88017736071110164 ) ) ;
#14039 = CARTESIAN_POINT ( 'NONE',  ( -1.099225684535947600, 38.70696800326375353, -6.408140936763238038 ) ) ;
#14040 = CARTESIAN_POINT ( 'NONE',  ( 10.00000000000000178, 39.31368534415484106, 10.88017736071110342 ) ) ;
#14041 = CARTESIAN_POINT ( 'NONE',  ( 7.361572987183170547, 67.05059781766746596, 9.846743663894590881 ) ) ;
#14042 = CARTESIAN_POINT ( 'NONE',  ( 10.00000000000000000, 54.75893115100078745, -9.846743663894594434 ) ) ;
#14043 = CARTESIAN_POINT ( 'NONE',  ( 5.076628168052704559, 15.17559781766745175, -8.527530157486179263 ) ) ;
#14044 = CARTESIAN_POINT ( 'NONE',  ( 19.84674366389459266, 3.300597817667451750, 2.638427012816836559 ) ) ;
#14045 = CARTESIAN_POINT ( 'NONE',  ( 17.08211943468705130, 38.47041550158063217, 12.26659068614894998 ) ) ;
#14046 = CARTESIAN_POINT ( 'NONE',  ( -14.97653319723434073, 15.00000000000000000, -5.619684139539446122 ) ) ;
#14047 =( GEOMETRIC_REPRESENTATION_CONTEXT ( 3 ) GLOBAL_UNCERTAINTY_ASSIGNED_CONTEXT ( ( #57301 ) ) GLOBAL_UNIT_ASSIGNED_CONTEXT ( ( #3153, #49131, #67091 ) ) REPRESENTATION_CONTEXT ( 'NONE', 'WORKASPACE' ) );
#14048 = CARTESIAN_POINT ( 'NONE',  ( 11.35674113183028311, -65.10122143319173915, -3.750000000000000000 ) ) ;
#14049 = CARTESIAN_POINT ( 'NONE',  ( -7.072388532688812290, -84.40601219567531643, -4.000000000001612932 ) ) ;
#14050 = COLOUR_RGB ( '', 0.40784314, 0.44705882, 0.49803922) ;
#14051 = ORIENTED_EDGE ( 'NONE', *, *, #17478, .F. ) ;
#14052 = VERTEX_POINT ( 'NONE', #95932 ) ;
#14053 = CARTESIAN_POINT ( 'NONE',  ( 13.79529636645031943, 55.34541550158062506, -14.16423886937409904 ) ) ;
#14054 = CARTESIAN_POINT ( 'NONE',  ( 6.204703633549690345, 57.84541550158063927, 14.16423886937410082 ) ) ;
#14055 = CARTESIAN_POINT ( 'NONE',  ( 7.361572987183169658, 29.96726448433411960, -9.846743663894592657 ) ) ;
#14056 = CARTESIAN_POINT ( 'NONE',  ( 6.565887622018943937, 28.08196800326375353, -12.81628187352647608 ) ) ;
#14058 = CARTESIAN_POINT ( 'NONE',  ( -2.266590686148945544, 2.220415501580634388, 7.082119434687048631 ) ) ;
#14057 = CARTESIAN_POINT ( 'NONE',  ( 2.148416515056672971, 22.23726573380438509, 6.499999999999995559 ) ) ;
#14059 = CARTESIAN_POINT ( 'NONE',  ( 4.559911319644449179, 12.23035201082150536, -9.422509992056141925 ) ) ;
#14060 = CARTESIAN_POINT ( 'NONE',  ( -4.164238869374099039, 51.80374883491396787, 8.674139862899312516E-16 ) ) ;
#14061 = EDGE_CURVE ( 'NONE', #11195, #35060, #70056, .T. ) ;
#14062 = CARTESIAN_POINT ( 'NONE',  ( 2.791683348922240793, 31.63393115100078745, 7.208316651077764092 ) ) ;
#14063 = LINE ( 'NONE', #51560, #66782 ) ;
#14064 = CARTESIAN_POINT ( 'NONE',  ( 10.00000000000000178, 17.25893115100078745, 9.846743663894594434 ) ) ;
#14065 = ADVANCED_FACE ( 'NONE', ( #5430 ), #72414, .F. ) ;
#14066 = FACE_OUTER_BOUND ( 'NONE', #83762, .T. ) ;
#14067 = CARTESIAN_POINT ( 'NONE',  ( -7.208316651077756099, 16.63393115100079100, 7.208316651077766757 ) ) ;
#14068 = EDGE_LOOP ( 'NONE', ( #75499, #37847, #35216, #45589 ) ) ;
#14069 = B_SPLINE_CURVE_WITH_KNOTS ( 'NONE', 3,
 ( #48744, #41761, #64228, #49243, #55773, #56743, #24792, #47267 ),
 .UNSPECIFIED., .F., .F.,
 ( 4, 2, 2, 4 ),
 ( 0.000000000000000000, 0.002750327629744753200, 0.004125491444617137606, 0.005500655259489521144 ),
 .UNSPECIFIED. ) ;
#14070 = ORIENTED_EDGE ( 'NONE', *, *, #42833, .F. ) ;
#14071 = SURFACE_STYLE_USAGE ( .BOTH. , #75545 ) ;
#14072 = ORIENTED_EDGE ( 'NONE', *, *, #86749, .T. ) ;
#14073 = CARTESIAN_POINT ( 'NONE',  ( 14.92337183194729988, 44.34226448433412315, -8.527530157486177487 ) ) ;
#14075 = CARTESIAN_POINT ( 'NONE',  ( 15.44008868035555793, 36.39701867748816966, -9.422509992056140149 ) ) ;
#14074 = CARTESIAN_POINT ( 'NONE',  ( -0.8801773607110991993, 22.85535201082150181, -2.915334737309923874 ) ) ;
#14077 = CARTESIAN_POINT ( 'NONE',  ( 6.565887622018943937, 23.08196800326375708, -12.81628187352647608 ) ) ;
#14076 = CARTESIAN_POINT ( 'NONE',  ( 19.84674366389459266, 63.30059781766745886, 2.638427012816836559 ) ) ;
#14078 = CARTESIAN_POINT ( 'NONE',  ( 17.08211943468705130, 8.470415501580635720, 12.26659068614894998 ) ) ;
#14079 = CARTESIAN_POINT ( 'NONE',  ( 20.88017736071110164, 65.35535201082150536, 2.915334737309930979 ) ) ;
#14080 = CARTESIAN_POINT ( 'NONE',  ( 13.43411237798105340, 25.58196800326374998, 12.81628187352647963 ) ) ;
#14081 = ORIENTED_EDGE ( 'NONE', *, *, #33950, .T. ) ;
#14082 = CARTESIAN_POINT ( 'NONE',  ( 2.791683348922237240, 25.38393115100078390, -7.208316651077763204 ) ) ;
#14083 = CARTESIAN_POINT ( 'NONE',  ( 2.035157376598822676, 7.438685344154837509, -7.964842623401177768 ) ) ;
#14084 = VERTEX_POINT ( 'NONE', #26923 ) ;
#14085 = CARTESIAN_POINT ( 'NONE',  ( 7.084665262690076126, 9.105352010821503583, 10.88017736071109987 ) ) ;
#14086 = VERTEX_POINT ( 'NONE', #58392 ) ;
#14087 = CARTESIAN_POINT ( 'NONE',  ( -0.8801773607111008646, 43.27201867748817676, 2.915334737309923430 ) ) ;
#14088 = CARTESIAN_POINT ( 'NONE',  ( -0.8801773607111009756, 58.06368534415484106, 1.068504757029289695E-15 ) ) ;
#14089 = CARTESIAN_POINT ( 'NONE',  ( 7.361572987183170547, 2.050597817667451750, 9.846743663894590881 ) ) ;
#14090 = CARTESIAN_POINT ( 'NONE',  ( 12.91533473730993009, 51.60535201082149825, -10.88017736071109987 ) ) ;
#14092 = AXIS2_PLACEMENT_3D ( 'NONE', #73429, #90900, #21433 ) ;
#14091 = DIRECTION ( 'NONE',  ( -0.8433914458128813907, 0.000000000000000000, -0.5372996083468306594 ) ) ;
#14093 = CARTESIAN_POINT ( 'NONE',  ( 0.1532563361054082862, 26.21726448433411605, 2.638427012816831674 ) ) ;
#14094 = VERTEX_POINT ( 'NONE', #88910 ) ;
#14095 = CARTESIAN_POINT ( 'NONE',  ( 20.15039907845753220, 19.72266099184918886, 6.262539305110075283 ) ) ;
#14096 = DIRECTION ( 'NONE',  ( 0.9366721892483971246, 0.000000000000000000, 0.3502073812594685975 ) ) ;
#14097 = CARTESIAN_POINT ( 'NONE',  ( 6.204703633549690345, 0.7620821682473009062, -14.16423886937410259 ) ) ;
#14098 = CIRCLE ( 'NONE', #92316, 2.900000000000002576 ) ;
#14099 = ORIENTED_EDGE ( 'NONE', *, *, #97807, .F. ) ;
#14100 = DIRECTION ( 'NONE',  ( 1.000000000000000000, 0.000000000000000000, 0.000000000000000000 ) ) ;
#14101 = CARTESIAN_POINT ( 'NONE',  ( -9.997910040112678587, 4.195612547371048347E-16, 10.50199004140710812 ) ) ;
#14102 = CARTESIAN_POINT ( 'NONE',  ( -3.750000000000000000, 36.75000000000000000, -2.750000000000000000 ) ) ;
#14103 = CARTESIAN_POINT ( 'NONE',  ( 20.88017736071110519, 5.563685344154838397, 2.639326808657452039E-16 ) ) ;
#14104 = DIRECTION ( 'NONE',  ( 1.000000000000000000, 0.000000000000000000, -0.000000000000000000 ) ) ;
#14105 = VERTEX_POINT ( 'NONE', #57420 ) ;
#14106 = FILL_AREA_STYLE ('',( #90086 ) ) ;
#14107 = CARTESIAN_POINT ( 'NONE',  ( 0.1532563361054083140, 46.00893115100079456, 1.131784320476157264E-15 ) ) ;
#14108 = CARTESIAN_POINT ( 'NONE',  ( 6.767445849361252819, 14.49999999999999112, -13.38662304974503492 ) ) ;
#14109 = CARTESIAN_POINT ( 'NONE',  ( 0.6178305044545818747, 23.49863466993041783, -9.382169495545419124 ) ) ;
#14110 = CARTESIAN_POINT ( 'NONE',  ( 19.84674366389459621, 8.508931151000785675, 7.409399052514197653E-17 ) ) ;
#14111 = EDGE_CURVE ( 'NONE', #43572, #39677, #17398, .T. ) ;
#14112 = AXIS2_PLACEMENT_3D ( 'NONE', #21290, #34289, #95304 ) ;
#14113 = PLANE ( 'NONE',  #87260 ) ;
#14114 = CARTESIAN_POINT ( 'NONE',  ( 21.09922568453595559, 7.040301336597086568, -6.408140936763230044 ) ) ;
#14115 = AXIS2_PLACEMENT_3D ( 'NONE', #66558, #97086, #59052 ) ;
#14116 = CARTESIAN_POINT ( 'NONE',  ( 6.879999999999995453, 43.00000000000000000, 6.500000000000000888 ) ) ;
#14117 = B_SPLINE_CURVE_WITH_KNOTS ( 'NONE', 3,
 ( #81920, #15904, #67421, #32854, #64325, #77368 ),
 .UNSPECIFIED., .F., .F.,
 ( 4, 2, 4 ),
 ( 3.409110551496146276E-05, 0.0004400426677367891737, 0.0008459942299586169050 ),
 .UNSPECIFIED. ) ;
#14118 = ORIENTED_EDGE ( 'NONE', *, *, #44340, .T. ) ;
#14119 = ORIENTED_EDGE ( 'NONE', *, *, #96580, .F. ) ;
#14120 = CARTESIAN_POINT ( 'NONE',  ( 7.084665262690076126, 22.02201867748817321, -10.88017736071110164 ) ) ;
#14121 = CARTESIAN_POINT ( 'NONE',  ( 13.79529636645031943, 25.34541550158063572, -14.16423886937409904 ) ) ;
#14122 = CARTESIAN_POINT ( 'NONE',  ( 5.076628168052703671, 31.84226448433412315, 8.527530157486179263 ) ) ;
#14123 = CARTESIAN_POINT ( 'NONE',  ( 20.88017736071110164, 60.35535201082151957, 2.915334737309930979 ) ) ;
#14124 = CARTESIAN_POINT ( 'NONE',  ( 3.591859063236761518, 34.95696800326375353, 11.09922568453594849 ) ) ;
#14125 = CARTESIAN_POINT ( 'NONE',  ( 15.44008868035555260, 14.73035201082150536, 9.422509992056143702 ) ) ;
#14126 = CARTESIAN_POINT ( 'NONE',  ( 0.9413316022086124502, 43.45508385108959004, 6.499999999999978684 ) ) ;
#14127 = CARTESIAN_POINT ( 'NONE',  ( -8.813102413619921194, -0.03417435944610275333, -13.34940531570976496 ) ) ;
#14128 = CARTESIAN_POINT ( 'NONE',  ( 16.40814093676323893, 15.79030133659708746, 11.09922568453595026 ) ) ;
#14129 = CARTESIAN_POINT ( 'NONE',  ( 12.63842701281683922, 59.55059781766744464, -9.846743663894590881 ) ) ;
#14130 = CARTESIAN_POINT ( 'NONE',  ( 1.472469842513823179, 26.42559781766745175, 4.923371831947296329 ) ) ;
#14131 = CARTESIAN_POINT ( 'NONE',  ( 2.915334737309921209, -8.394647989178491088, -10.88017736071110164 ) ) ;
#14132 = CARTESIAN_POINT ( 'NONE',  ( 13.43411237798105340, 35.58196800326375353, 12.81628187352647963 ) ) ;
#14133 = CARTESIAN_POINT ( 'NONE',  ( 18.61655166652077042, 24.87718327197429602, 6.499999999999981348 ) ) ;
#14135 = CARTESIAN_POINT ( 'NONE',  ( 12.60874940350947959, 4.146618495107105809E-16, -7.160268045227032196 ) ) ;
#14134 = CARTESIAN_POINT ( 'NONE',  ( -0.8801773607111008646, 38.27201867748816255, 2.915334737309923430 ) ) ;
#14136 = DIRECTION ( 'NONE',  ( -0.9723699203976758909, 0.000000000000000000, -0.2334453638559087496 ) ) ;
#14137 = B_SPLINE_CURVE_WITH_KNOTS ( 'NONE', 3,
 ( #22011, #14511, #83977, #97034, #37999, #15502 ),
 .UNSPECIFIED., .F., .F.,
 ( 4, 2, 4 ),
 ( 0.0002800039672440436710, 0.0006862092354666161648, 0.001092414503689188550 ),
 .UNSPECIFIED. ) ;
#14138 =( NAMED_UNIT ( * ) PLANE_ANGLE_UNIT ( ) SI_UNIT ( $, .RADIAN. ) );
#14139 = CARTESIAN_POINT ( 'NONE',  ( 20.88017736071110875, 35.77201867748816966, -2.915334737309920765 ) ) ;
#14140 = CARTESIAN_POINT ( 'NONE',  ( 7.084665262690076126, 44.10535201082151247, 10.88017736071109987 ) ) ;
#14141 = CARTESIAN_POINT ( 'NONE',  ( 19.84674366389459621, 63.50893115100078745, 7.409399052514197653E-17 ) ) ;
#14142 = EDGE_CURVE ( 'NONE', #26894, #85540, #42933, .T. ) ;
#14143 = CARTESIAN_POINT ( 'NONE',  ( 2.035157376598822676, 47.43868534415484817, -7.964842623401177768 ) ) ;
#14144 = EDGE_CURVE ( 'NONE', #6265, #33986, #3364, .T. ) ;
#14145 = CARTESIAN_POINT ( 'NONE',  ( 12.63842701281683922, 44.55059781766745175, -9.846743663894590881 ) ) ;
#14146 = CARTESIAN_POINT ( 'NONE',  ( 2.035157376598822676, 12.43868534415483751, -7.964842623401177768 ) ) ;
#14147 = CARTESIAN_POINT ( 'NONE',  ( 13.43411237798106583, 12.66530133659708746, -12.81628187352647252 ) ) ;
#14148 = ORIENTED_EDGE ( 'NONE', *, *, #28799, .F. ) ;
#14149 = CARTESIAN_POINT ( 'NONE',  ( -0.8801773607111008646, 18.27201867748817321, 2.915334737309923430 ) ) ;
#14150 = B_SPLINE_CURVE_WITH_KNOTS ( 'NONE', 3,
 ( #44305, #35324, #43321, #89324, #20832, #29303 ),
 .UNSPECIFIED., .F., .F.,
 ( 4, 2, 4 ),
 ( 0.0002800364959418023825, 0.0006862420824208962733, 0.001092447668899990164 ),
 .UNSPECIFIED. ) ;
#14151 = CARTESIAN_POINT ( 'NONE',  ( -13.82671409943291785, -0.03417435944610275333, -3.447387012295409114 ) ) ;
#14152 = CARTESIAN_POINT ( 'NONE',  ( 2.035157376598824452, 3.688685344154837953, 7.964842623401179544 ) ) ;
#14153 = CARTESIAN_POINT ( 'NONE',  ( 10.00000000000000000, 31.81368534415483751, -10.88017736071110342 ) ) ;
#14154 = CARTESIAN_POINT ( 'NONE',  ( 0.1532563361054083140, 1.008931151000784787, 1.131784320476157264E-15 ) ) ;
#14155 = CARTESIAN_POINT ( 'NONE',  ( 22.26659068614894466, 38.88708216824731068, 7.082119434687054849 ) ) ;
#14156 = CARTESIAN_POINT ( 'NONE',  ( 12.63842701281683034, 17.46726448433411250, 9.846743663894596210 ) ) ;
#14157 = AXIS2_PLACEMENT_3D ( 'NONE', #96794, #80290, #50781 ) ;
#14158 = CARTESIAN_POINT ( 'NONE',  ( 4.559911319644449179, 47.23035201082150536, -9.422509992056141925 ) ) ;
#14159 = CARTESIAN_POINT ( 'NONE',  ( 19.05866839779139355, 45.95508385108959715, -6.499999999999974243 ) ) ;
#14160 = ORIENTED_EDGE ( 'NONE', *, *, #6682, .F. ) ;
#14161 = CARTESIAN_POINT ( 'NONE',  ( 6.324651560463742328, -50.88858560574520595, 2.500000000000000000 ) ) ;
#14162 = CARTESIAN_POINT ( 'NONE',  ( 7.361572987183169658, 64.96726448433412315, -9.846743663894592657 ) ) ;
#14163 = ORIENTED_EDGE ( 'NONE', *, *, #6008, .T. ) ;
#14164 = ORIENTED_EDGE ( 'NONE', *, *, #63561, .T. ) ;
#14165 = CARTESIAN_POINT ( 'NONE',  ( 6.204703633549690345, 22.84541550158062861, 14.16423886937410082 ) ) ;
#14166 = CARTESIAN_POINT ( 'NONE',  ( 24.16423886937409904, 24.09541550158063927, 3.795296366450317205 ) ) ;
#14167 = CARTESIAN_POINT ( 'NONE',  ( 2.035157376598822676, 62.43868534415483396, -7.964842623401177768 ) ) ;
#14168 = CARTESIAN_POINT ( 'NONE',  ( 7.084665262690076126, 4.105352010821503583, 10.88017736071109987 ) ) ;
#14169 = CARTESIAN_POINT ( 'NONE',  ( 3.591859063236761518, 4.956968003263753531, 11.09922568453594849 ) ) ;
#14170 = CARTESIAN_POINT ( 'NONE',  ( 14.92337183194729988, 44.34226448433412315, -8.527530157486177487 ) ) ;
#14171 = CARTESIAN_POINT ( 'NONE',  ( -10.67064208003667325, -97.55764508345595232, 4.000000000000000000 ) ) ;
#14173 = CARTESIAN_POINT ( 'NONE',  ( 16.40814093676323893, 0.7903013365970867898, 11.09922568453595026 ) ) ;
#14172 = CARTESIAN_POINT ( 'NONE',  ( 20.88017736071110164, 40.35535201082150536, 2.915334737309930979 ) ) ;
#14174 = CARTESIAN_POINT ( 'NONE',  ( 24.16423886937410614, 19.30374883491397142, 8.672049930838204340E-16 ) ) ;
#14175 = CARTESIAN_POINT ( 'NONE',  ( 10.00000000000000178, 9.313685344154839285, 10.88017736071110342 ) ) ;
#14176 = CARTESIAN_POINT ( 'NONE',  ( 7.084665262690076126, 17.02201867748817676, -10.88017736071110164 ) ) ;
#14177 = CARTESIAN_POINT ( 'NONE',  ( 18.52753015748617571, 53.09226448433412315, 4.923371831947298993 ) ) ;
#14178 = CARTESIAN_POINT ( 'NONE',  ( 17.96484262340118221, 39.93868534415484106, 7.964842623401181321 ) ) ;
#14179 = AXIS2_PLACEMENT_3D ( 'NONE', #88417, #27412, #65407 ) ;
#14180 = CARTESIAN_POINT ( 'NONE',  ( -8.527530157486173934, -23.57440218233254470, 4.923371831947302546 ) ) ;
#14181 = ORIENTED_EDGE ( 'NONE', *, *, #3643, .F. ) ;
#14182 = CARTESIAN_POINT ( 'NONE',  ( 1.460619146402132233E-15, 35.00000000000000000, 11.92686044187656513 ) ) ;
#14183 = ORIENTED_EDGE ( 'NONE', *, *, #72465, .F. ) ;
#14184 = CARTESIAN_POINT ( 'NONE',  ( 2.791683348922240793, 31.63393115100078745, 7.208316651077764092 ) ) ;
#14185 = ORIENTED_EDGE ( 'NONE', *, *, #93607, .T. ) ;
#14186 = CARTESIAN_POINT ( 'NONE',  ( -46.94000000000001194, 103.0000000000000000, -5.997726559847240679 ) ) ;
#14188 = CARTESIAN_POINT ( 'NONE',  ( 7.084665262690076126, 4.105352010821503583, 10.88017736071109987 ) ) ;
#14187 = CARTESIAN_POINT ( 'NONE',  ( 22.26659068614894466, 48.88708216824730357, 7.082119434687054849 ) ) ;
#14190 = CARTESIAN_POINT ( 'NONE',  ( 14.92337183194729633, 47.67559781766745175, 8.527530157486181039 ) ) ;
#14189 = CARTESIAN_POINT ( 'NONE',  ( 18.52753015748617571, 28.09226448433411960, 4.923371831947298993 ) ) ;
#14191 = CARTESIAN_POINT ( 'NONE',  ( 21.92686044187657046, 50.16212336850781384, 4.562052436263912550E-16 ) ) ;
#14192 = ADVANCED_FACE ( 'NONE', ( #61764 ), #22242, .T. ) ;
#14193 = VECTOR ( 'NONE', #90653, 1000.000000000000000 ) ;
#14194 = CARTESIAN_POINT ( 'NONE',  ( 9.879999999999990123, 18.09999999999999787, 0.000000000000000000 ) ) ;
#14195 =( GEOMETRIC_REPRESENTATION_CONTEXT ( 3 ) GLOBAL_UNCERTAINTY_ASSIGNED_CONTEXT ( ( #32211 ) ) GLOBAL_UNIT_ASSIGNED_CONTEXT ( ( #85381, #60409, #22432 ) ) REPRESENTATION_CONTEXT ( 'NONE', 'WORKASPACE' ) );
#14196 = CARTESIAN_POINT ( 'NONE',  ( 0.1532563361054100626, 0.8005978176674514168, -2.638427012816831230 ) ) ;
#14197 = CARTESIAN_POINT ( 'NONE',  ( 12.81628187352647608, 16.62363466993042849, -2.602085213965210642E-15 ) ) ;
#14198 = EDGE_LOOP ( 'NONE', ( #60443, #95638, #75663, #17396 ) ) ;
#14199 = CARTESIAN_POINT ( 'NONE',  ( -0.3689425029237898834, 36.17874883491396787, -10.36894250292378850 ) ) ;
#14200 = CARTESIAN_POINT ( 'NONE',  ( 16.40814093676323893, 20.79030133659708923, 11.09922568453595026 ) ) ;
#14201 = ORIENTED_EDGE ( 'NONE', *, *, #52504, .T. ) ;
#14202 = CARTESIAN_POINT ( 'NONE',  ( -2.816281873526471635, 58.91530133659707502, -3.434112377981056508 ) ) ;
#14203 = CARTESIAN_POINT ( 'NONE',  ( -0.8801773607110991993, 27.85535201082150181, -2.915334737309923874 ) ) ;
#14204 = CARTESIAN_POINT ( 'NONE',  ( 0.1532563361054083140, 31.00893115100078390, 1.131784320476157264E-15 ) ) ;
#14205 = CARTESIAN_POINT ( 'NONE',  ( -0.8801773607111008646, 28.27201867748817321, 2.915334737309923430 ) ) ;
#14206 = CARTESIAN_POINT ( 'NONE',  ( 20.15039907845753575, 32.62777174578613426, -6.262539305110076171 ) ) ;
#14207 = DIRECTION ( 'NONE',  ( -0.7489557207890037427, 0.000000000000000000, 0.6626200482157358351 ) ) ;
#14208 = CARTESIAN_POINT ( 'NONE',  ( 17.20831665107776587, 37.88393115100078745, 7.208316651077764980 ) ) ;
#14209 = CARTESIAN_POINT ( 'NONE',  ( 14.92337183194729633, 52.67559781766745175, 8.527530157486181039 ) ) ;
#14210 = CIRCLE ( 'NONE', #70090, 0.2500000000000002220 ) ;
#14211 = CARTESIAN_POINT ( 'NONE',  ( 0.6178305044545838731, 29.74863466993042138, 9.382169495545420901 ) ) ;
#14213 = ORIENTED_EDGE ( 'NONE', *, *, #61171, .F. ) ;
#14212 = CARTESIAN_POINT ( 'NONE',  ( 17.39651004071842166, 27.93575266056828355, 6.499999999999998224 ) ) ;
#14214 = CARTESIAN_POINT ( 'NONE',  ( 0.000000000000000000, 14.49999999999999822, 0.000000000000000000 ) ) ;
#14215 = CARTESIAN_POINT ( 'NONE',  ( 0.000000000000000000, 0.5000000000000004441, 0.000000000000000000 ) ) ;
#14216 = CARTESIAN_POINT ( 'NONE',  ( 18.72515096720590577, 61.07228050351029935, -6.499999999999718447 ) ) ;
#14217 = DIRECTION ( 'NONE',  ( 0.000000000000000000, -1.000000000000000000, 0.000000000000000000 ) ) ;
#14218 = CARTESIAN_POINT ( 'NONE',  ( 17.20831665107776587, 17.88393115100078745, 7.208316651077764980 ) ) ;
#14219 = CARTESIAN_POINT ( 'NONE',  ( 10.00000000000000178, 35.37363466993042493, 12.81628187352647608 ) ) ;
#14220 = CARTESIAN_POINT ( 'NONE',  ( -4.000000000000000000, 36.75000000000000000, 3.750000000000000000 ) ) ;
#14221 = VERTEX_POINT ( 'NONE', #6431 ) ;
#14222 = CARTESIAN_POINT ( 'NONE',  ( 15.00000000000000178, 73.00000000000000000, 6.250000000000000000 ) ) ;
#14223 = CARTESIAN_POINT ( 'NONE',  ( 1.472469842513823179, 36.42559781766745175, 4.923371831947296329 ) ) ;
#14224 = CARTESIAN_POINT ( 'NONE',  ( 2.917880565312950480, 40.97041550158063217, -12.26659068614894821 ) ) ;
#14225 = CARTESIAN_POINT ( 'NONE',  ( 1.472469842513823179, 45.59226448433412315, -4.923371831947296329 ) ) ;
#14226 = CARTESIAN_POINT ( 'NONE',  ( 16.40814093676324603, 52.45696800326375353, -11.09922568453594671 ) ) ;
#14228 = CARTESIAN_POINT ( 'NONE',  ( 9.065164099344483972, 0.3639310782753644169, 11.95084933600775301 ) ) ;
#14227 = CYLINDRICAL_SURFACE ( 'NONE', #14527, 11.92686044187656513 ) ;
#14229 = CARTESIAN_POINT ( 'NONE',  ( 5.076628168052703671, 11.84226448433411960, 8.527530157486179263 ) ) ;
#14230 = SURFACE_STYLE_FILL_AREA ( #22230 ) ;
#14231 = CARTESIAN_POINT ( 'NONE',  ( 19.84674366389459266, 48.71726448433413026, -2.638427012816827677 ) ) ;
#14232 = CARTESIAN_POINT ( 'NONE',  ( 10.00000000000000178, 39.31368534415484106, 10.88017736071110342 ) ) ;
#14233 = EDGE_CURVE ( 'NONE', #86850, #56243, #87180, .T. ) ;
#14234 = CARTESIAN_POINT ( 'NONE',  ( 19.84674366389459266, 38.71726448433412315, -2.638427012816827677 ) ) ;
#14235 = CARTESIAN_POINT ( 'NONE',  ( 0.000000000000000000, 15.00000000000000000, 0.000000000000000000 ) ) ;
#14236 = CARTESIAN_POINT ( 'NONE',  ( 12.91533473730993009, 46.60535201082150536, -10.88017736071109987 ) ) ;
#14237 = ORIENTED_EDGE ( 'NONE', *, *, #47439, .F. ) ;
#14238 = CARTESIAN_POINT ( 'NONE',  ( -12.83294900548052730, 15.00000000000000000, -7.766300266068542513 ) ) ;
#14239 = CARTESIAN_POINT ( 'NONE',  ( 17.96484262340118221, 21.18868534415483396, -7.964842623401177768 ) ) ;
#14241 = CARTESIAN_POINT ( 'NONE',  ( 7.084665262690076126, 49.10535201082149825, 10.88017736071109987 ) ) ;
#14240 = CARTESIAN_POINT ( 'NONE',  ( 0.6178305044545838731, -0.2513653300695798953, 9.382169495545420901 ) ) ;
#14242 = CARTESIAN_POINT ( 'NONE',  ( 7.084665262690076126, 62.02201867748816966, -10.88017736071110164 ) ) ;
#14243 =( NAMED_UNIT ( * ) SI_UNIT ( $, .STERADIAN. ) SOLID_ANGLE_UNIT ( ) );
#14244 = STYLED_ITEM ( 'NONE', ( #45279 ), #14513 ) ;
#14246 = CARTESIAN_POINT ( 'NONE',  ( 4.879999999999991900, 76.07179676972444327, 6.500000000000000888 ) ) ;
#14245 = CARTESIAN_POINT ( 'NONE',  ( 20.88017736071110875, 40.77201867748818387, -2.915334737309920765 ) ) ;
#14247 = CARTESIAN_POINT ( 'NONE',  ( 0.1532563361054082862, 11.21726448433411605, 2.638427012816831674 ) ) ;
#14248 = CARTESIAN_POINT ( 'NONE',  ( 0.1532563361054100626, 25.80059781766744820, -2.638427012816831230 ) ) ;
#14249 = CARTESIAN_POINT ( 'NONE',  ( -1.881370533971388870, 15.00000000000000888, 14.50512983964824620 ) ) ;
#14250 = CARTESIAN_POINT ( 'NONE',  ( -14.16423886937409726, 17.01208216824730357, 3.795296366450320757 ) ) ;
#14251 = CARTESIAN_POINT ( 'NONE',  ( 14.92337183194729633, 62.67559781766745886, 8.527530157486181039 ) ) ;
#14252 = CARTESIAN_POINT ( 'NONE',  ( 20.36894250292379382, 63.67874883491396787, 10.36894250292379205 ) ) ;
#14253 = CARTESIAN_POINT ( 'NONE',  ( -4.000000000000000000, 37.00000000000000000, -2.750000000000000000 ) ) ;
#14255 = CARTESIAN_POINT ( 'NONE',  ( 10.00000000000000178, 28.05374883491396787, 14.16423886937410082 ) ) ;
#14254 = STYLED_ITEM ( 'NONE', ( #42585 ), #60195 ) ;
#14256 = VECTOR ( 'NONE', #77649, 1000.000000000000000 ) ;
#14257 = CARTESIAN_POINT ( 'NONE',  ( -4.164238869374098151, 46.59541550158063927, -3.795296366450310543 ) ) ;
#14258 =( LENGTH_UNIT ( ) NAMED_UNIT ( * ) SI_UNIT ( .MILLI., .METRE. ) );
#14259 = B_SPLINE_CURVE_WITH_KNOTS ( 'NONE', 3,
 ( #87322, #35800, #66287, #28298, #20809, #51297 ),
 .UNSPECIFIED., .F., .F.,
 ( 4, 2, 4 ),
 ( 3.409110551496091388E-05, 0.0004400426677367852164, 0.0008459942299586095324 ),
 .UNSPECIFIED. ) ;
#14260 = EDGE_LOOP ( 'NONE', ( #81308, #17652, #76152, #48684, #18193, #48717 ) ) ;
#14261 = CARTESIAN_POINT ( 'NONE',  ( 1.472469842513823179, 25.59226448433412315, -4.923371831947296329 ) ) ;
#14262 = EDGE_CURVE ( 'NONE', #62525, #25445, #65158, .T. ) ;
#14263 = CARTESIAN_POINT ( 'NONE',  ( 2.035157376598824452, 18.68868534415484106, 7.964842623401179544 ) ) ;
#14264 = CARTESIAN_POINT ( 'NONE',  ( 0.1532563361054082862, 51.21726448433412315, 2.638427012816831674 ) ) ;
#14266 = CARTESIAN_POINT ( 'NONE',  ( 20.15039907845753575, 16.74884699246888431, 6.262539305110077059 ) ) ;
#14265 = FACE_OUTER_BOUND ( 'NONE', #65559, .T. ) ;
#14267 = CARTESIAN_POINT ( 'NONE',  ( -11.36220558718869711, 4.706058445226104967E-16, 9.008345252845160189 ) ) ;
#14268 = UNCERTAINTY_MEASURE_WITH_UNIT (LENGTH_MEASURE( 1.000000000000000082E-05 ), #6832, 'distance_accuracy_value', 'NONE');
#14269 = PRESENTATION_STYLE_ASSIGNMENT (( #89749 ) ) ;
#14270 = CARTESIAN_POINT ( 'NONE',  ( 16.40814093676324603, 32.45696800326375353, -11.09922568453594671 ) ) ;
#14271 = CARTESIAN_POINT ( 'NONE',  ( 7.361572987183170547, 47.05059781766745175, 9.846743663894590881 ) ) ;
#14273 = ORIENTED_EDGE ( 'NONE', *, *, #75562, .T. ) ;
#14272 = EDGE_CURVE ( 'NONE', #32382, #17988, #66910, .T. ) ;
#14274 = CARTESIAN_POINT ( 'NONE',  ( 10.00000000000000178, 7.258931151000785675, 9.846743663894594434 ) ) ;
#14275 = CARTESIAN_POINT ( 'NONE',  ( 11.20666035741388278, -56.81027457019842331, -3.750000000000000000 ) ) ;
#14276 = CARTESIAN_POINT ( 'NONE',  ( -12.25993886608593897, 0.3640475087720980163, -8.642563219313796452 ) ) ;
#14277 = CARTESIAN_POINT ( 'NONE',  ( -0.8801773607110991993, 12.85535201082150358, -2.915334737309923874 ) ) ;
#14278 = CARTESIAN_POINT ( 'NONE',  ( 20.36894250292379738, 59.92874883491397497, -10.36894250292379027 ) ) ;
#14279 = CARTESIAN_POINT ( 'NONE',  ( 15.44008868035555793, 46.39701867748817676, -9.422509992056140149 ) ) ;
#14280 = CARTESIAN_POINT ( 'NONE',  ( 15.44008868035555793, 66.39701867748817676, -9.422509992056140149 ) ) ;
#14281 = DIRECTION ( 'NONE',  ( 0.000000000000000000, 1.000000000000000000, 0.000000000000000000 ) ) ;
#14282 = CARTESIAN_POINT ( 'NONE',  ( 19.84674366389459621, 18.50893115100078745, 7.409399052514197653E-17 ) ) ;
#14283 = CARTESIAN_POINT ( 'NONE',  ( 7.084665262690076126, 7.022018677488169658, -10.88017736071110164 ) ) ;
#14284 = CARTESIAN_POINT ( 'NONE',  ( 10.00000000000000178, 12.25893115100078568, 9.846743663894594434 ) ) ;
#14285 = CARTESIAN_POINT ( 'NONE',  ( 0.000000000000000000, 0.000000000000000000, 0.000000000000000000 ) ) ;
#14286 = CARTESIAN_POINT ( 'NONE',  ( 1.472469842513823179, 31.42559781766745530, 4.923371831947296329 ) ) ;
#14287 = VECTOR ( 'NONE', #18955, 1000.000000000000114 ) ;
#14288 = CARTESIAN_POINT ( 'NONE',  ( 4.559911319644449179, 32.23035201082150536, -9.422509992056141925 ) ) ;
#14289 = UNCERTAINTY_MEASURE_WITH_UNIT (LENGTH_MEASURE( 1.000000000000000082E-05 ), #40489, 'distance_accuracy_value', 'NONE');
#14290 = EDGE_LOOP ( 'NONE', ( #16276, #19106, #82937, #51062 ) ) ;
#14291 = CARTESIAN_POINT ( 'NONE',  ( 3.591859063236761518, 64.95696800326376774, 11.09922568453594849 ) ) ;
#14292 = DIRECTION ( 'NONE',  ( 0.000000000000000000, 0.000000000000000000, 1.000000000000000000 ) ) ;
#14293 = CARTESIAN_POINT ( 'NONE',  ( 5.076628168052704559, 15.17559781766745175, -8.527530157486179263 ) ) ;
#14294 = CARTESIAN_POINT ( 'NONE',  ( 6.565887622018943937, 50.16530133659708213, 12.81628187352647430 ) ) ;
#14296 = CARTESIAN_POINT ( 'NONE',  ( 14.92337183194729988, 29.34226448433411960, -8.527530157486177487 ) ) ;
#14295 = CARTESIAN_POINT ( 'NONE',  ( 12.91533473730992121, 9.522018677488171434, 10.88017736071110164 ) ) ;
#14297 = DIRECTION ( 'NONE',  ( -0.8320502943378437211, 0.5547001962252290364, 0.000000000000000000 ) ) ;
#14298 = CARTESIAN_POINT ( 'NONE',  ( -1.899999999999997247, 98.49999999999998579, -8.525133428036873795 ) ) ;
#14299 = CARTESIAN_POINT ( 'NONE',  ( 17.08211943468705130, 33.47041550158063927, 12.26659068614894998 ) ) ;
#14300 = CARTESIAN_POINT ( 'NONE',  ( 20.36894250292379738, 39.92874883491396787, -10.36894250292379027 ) ) ;
#14301 = CARTESIAN_POINT ( 'NONE',  ( 19.84674366389459266, 53.71726448433411605, -2.638427012816827677 ) ) ;
#14302 = DIRECTION ( 'NONE',  ( 0.5075383629606904368, 0.000000000000000000, 0.8616291604415338146 ) ) ;
#14303 = CARTESIAN_POINT ( 'NONE',  ( 2.035157376598824452, 38.68868534415483396, 7.964842623401179544 ) ) ;
#14304 = CARTESIAN_POINT ( 'NONE',  ( 7.084665262690076126, 67.02201867748817676, -10.88017736071110164 ) ) ;
#14305 = CIRCLE ( 'NONE', #49389, 0.2500000000000000000 ) ;
#14306 = FILL_AREA_STYLE ('',( #83776 ) ) ;
#14307 = ORIENTED_EDGE ( 'NONE', *, *, #84150, .T. ) ;
#14308 = CARTESIAN_POINT ( 'NONE',  ( -1.099225684535947600, 58.70696800326375353, -6.408140936763238038 ) ) ;
#14309 = ORIENTED_EDGE ( 'NONE', *, *, #52388, .T. ) ;
#14310 = CARTESIAN_POINT ( 'NONE',  ( 2.791683348922237240, 0.3839311510007847872, -7.208316651077763204 ) ) ;
#14311 = ORIENTED_EDGE ( 'NONE', *, *, #39425, .F. ) ;
#14312 = CARTESIAN_POINT ( 'NONE',  ( 2.917880565312950480, 10.97041550158063572, -12.26659068614894821 ) ) ;
#14313 = CARTESIAN_POINT ( 'NONE',  ( 2.791683348922240793, 11.63393115100078568, 7.208316651077764092 ) ) ;
#14314 = CARTESIAN_POINT ( 'NONE',  ( -0.8801773607111009756, 33.06368534415484106, 1.068504757029289695E-15 ) ) ;
#14315 = EDGE_CURVE ( 'NONE', #96219, #19780, #16473, .T. ) ;
#14316 = CARTESIAN_POINT ( 'NONE',  ( 1.152268111383477178, 1.024801820426059406E-17, -6.000000000000281553 ) ) ;
#14317 = VERTEX_POINT ( 'NONE', #93319 ) ;
#14318 = CARTESIAN_POINT ( 'NONE',  ( 10.00000000000000178, 34.31368534415484106, 10.88017736071110342 ) ) ;
#14319 = ORIENTED_EDGE ( 'NONE', *, *, #93755, .T. ) ;
#14320 = LINE ( 'NONE', #92277, #72819 ) ;
#14321 = ORIENTED_EDGE ( 'NONE', *, *, #94726, .T. ) ;
#14322 = ORIENTED_EDGE ( 'NONE', *, *, #16304, .F. ) ;
#14323 = CARTESIAN_POINT ( 'NONE',  ( 4.559911319644449179, 63.89701867748817676, 9.422509992056141925 ) ) ;
#14324 = CARTESIAN_POINT ( 'NONE',  ( 24.50000000000000000, 35.99999999999997158, -7.000000000000000000 ) ) ;
#14326 = CARTESIAN_POINT ( 'NONE',  ( -4.873787042390612001, 0.000000000000000000, -13.39061984619925916 ) ) ;
#14325 = CARTESIAN_POINT ( 'NONE',  ( 12.91533473730992121, 14.52201867748817143, 10.88017736071110164 ) ) ;
#14327 = CARTESIAN_POINT ( 'NONE',  ( 1.472469842513823179, 0.5922644843341181575, -4.923371831947296329 ) ) ;
#14328 = CARTESIAN_POINT ( 'NONE',  ( 7.084665262690076126, 14.10535201082150358, 10.88017736071109987 ) ) ;
#14329 = VERTEX_POINT ( 'NONE', #24841 ) ;
#14330 = CARTESIAN_POINT ( 'NONE',  ( 21.09922568453594849, 51.20696800326375353, 6.408140936763242479 ) ) ;
#14331 = CARTESIAN_POINT ( 'NONE',  ( 4.559911319644449179, 42.23035201082151247, -9.422509992056141925 ) ) ;
#14332 = CARTESIAN_POINT ( 'NONE',  ( 2.746530213673227803E-16, 21.83999999999999986, 0.000000000000000000 ) ) ;
#14333 = CARTESIAN_POINT ( 'NONE',  ( 19.38216949554541202, 60.99863466993042493, 9.382169495545424454 ) ) ;
#14334 = CARTESIAN_POINT ( 'NONE',  ( 2.035157376598822676, 42.43868534415483396, -7.964842623401177768 ) ) ;
#14335 = CARTESIAN_POINT ( 'NONE',  ( 22.81628187352647785, 6.415301336597088344, 3.434112377981063169 ) ) ;
#14336 = PLANE ( 'NONE',  #29078 ) ;
#14337 = CARTESIAN_POINT ( 'NONE',  ( 14.92337183194729988, 14.34226448433411782, -8.527530157486177487 ) ) ;
#14338 = CARTESIAN_POINT ( 'NONE',  ( 4.656465524211139240, -8.255743748965677753, -3.750000000000000444 ) ) ;
#14339 = CARTESIAN_POINT ( 'NONE',  ( 3.591859063236763294, 8.290301336597087456, -11.09922568453595026 ) ) ;
#14341 = CARTESIAN_POINT ( 'NONE',  ( -8.099999999999999645, 80.99999999999994316, 2.900000000000001243 ) ) ;
#14340 = FILL_AREA_STYLE_COLOUR ( '', #96352 ) ;
#14342 = CARTESIAN_POINT ( 'NONE',  ( 19.42250999205614193, 40.14701867748817676, 5.440088680355555262 ) ) ;
#14343 = VECTOR ( 'NONE', #51819, 1000.000000000000000 ) ;
#14344 = CARTESIAN_POINT ( 'NONE',  ( 7.361572987183170547, 47.05059781766745175, 9.846743663894590881 ) ) ;
#14345 =( NAMED_UNIT ( * ) PLANE_ANGLE_UNIT ( ) SI_UNIT ( $, .RADIAN. ) );
#14346 = CARTESIAN_POINT ( 'NONE',  ( 5.076628168052703671, 16.84226448433411960, 8.527530157486179263 ) ) ;
#14347 = CARTESIAN_POINT ( 'NONE',  ( 7.361572987183170547, 2.050597817667451750, 9.846743663894590881 ) ) ;
#14348 = ADVANCED_FACE ( 'NONE', ( #42768 ), #73250, .T. ) ;
#14350 = ORIENTED_EDGE ( 'NONE', *, *, #62428, .T. ) ;
#14349 = CARTESIAN_POINT ( 'NONE',  ( 7.361572987183170547, 67.05059781766746596, 9.846743663894590881 ) ) ;
#14351 = CARTESIAN_POINT ( 'NONE',  ( 20.88017736071110164, 5.355352010821502695, 2.915334737309930979 ) ) ;
#14352 = PRESENTATION_STYLE_ASSIGNMENT (( #69320 ) ) ;
#14353 = CARTESIAN_POINT ( 'NONE',  ( 19.84674366389459266, 58.71726448433411605, -2.638427012816827677 ) ) ;
#14354 = CARTESIAN_POINT ( 'NONE',  ( 19.84674366389459266, 28.71726448433411960, -2.638427012816827677 ) ) ;
#14355 =( NAMED_UNIT ( * ) PLANE_ANGLE_UNIT ( ) SI_UNIT ( $, .RADIAN. ) );
#14357 = EDGE_CURVE ( 'NONE', #61681, #31263, #24170, .T. ) ;
#14356 = CARTESIAN_POINT ( 'NONE',  ( 10.00000000000000000, 6.813685344154838397, -10.88017736071110342 ) ) ;
#14358 = CARTESIAN_POINT ( 'NONE',  ( 14.92337183194729633, 47.67559781766745175, 8.527530157486181039 ) ) ;
#14359 = EDGE_LOOP ( 'NONE', ( #185, #82800, #58560, #60681 ) ) ;
#14360 = CARTESIAN_POINT ( 'NONE',  ( 3.927832320392247389, 15.00000000000000000, -13.69797916712104602 ) ) ;
#14361 = CARTESIAN_POINT ( 'NONE',  ( 2.035157376598822676, 2.438685344154838397, -7.964842623401177768 ) ) ;
#14362 = CARTESIAN_POINT ( 'NONE',  ( 0.5774900079438607392, 13.48035201082150358, 5.440088680355550821 ) ) ;
#14363 = CARTESIAN_POINT ( 'NONE',  ( 0.5774900079438607392, 18.48035201082150536, 5.440088680355550821 ) ) ;
#14364 = CARTESIAN_POINT ( 'NONE',  ( 24.16423886937410614, 54.51208216824730357, -3.795296366450302550 ) ) ;
#14366 = CYLINDRICAL_SURFACE ( 'NONE', #59032, 0.5000000000000004441 ) ;
#14365 = CARTESIAN_POINT ( 'NONE',  ( 6.204703633549690345, 57.84541550158063927, 14.16423886937410082 ) ) ;
#14367 = CARTESIAN_POINT ( 'NONE',  ( 7.361572987183170547, 2.050597817667451750, 9.846743663894590881 ) ) ;
#14368 = B_SPLINE_CURVE_WITH_KNOTS ( 'NONE', 3,
 ( #41904, #16929, #72365, #26875, #3896, #93407 ),
 .UNSPECIFIED., .F., .F.,
 ( 4, 2, 4 ),
 ( 0.000000000000000000, 0.0002701661927229378839, 0.0005403323854458757678 ),
 .UNSPECIFIED. ) ;
#14369 = CARTESIAN_POINT ( 'NONE',  ( 7.361572987183170547, 22.05059781766745530, 9.846743663894590881 ) ) ;
#14370 = EDGE_CURVE ( 'NONE', #18862, #77856, #28583, .T. ) ;
#14371 = CARTESIAN_POINT ( 'NONE',  ( -1.099225684535947600, 13.70696800326375353, -6.408140936763238038 ) ) ;
#14372 = ORIENTED_EDGE ( 'NONE', *, *, #44400, .F. ) ;
#14373 = PLANE ( 'NONE',  #19358 ) ;
#14374 = CARTESIAN_POINT ( 'NONE',  ( 1.472469842513823179, 56.42559781766745886, 4.923371831947296329 ) ) ;
#14375 = CARTESIAN_POINT ( 'NONE',  ( 11.92686044187655980, 2.396642702460846319, -3.195792623639533314 ) ) ;
#14376 = DIRECTION ( 'NONE',  ( -0.000000000000000000, -0.000000000000000000, 1.000000000000000000 ) ) ;
#14377 = CARTESIAN_POINT ( 'NONE',  ( 24.16423886937410614, 4.303748834913967869, 8.672049930838204340E-16 ) ) ;
#14378 = CARTESIAN_POINT ( 'NONE',  ( 2.791683348922237240, 25.38393115100078390, -7.208316651077763204 ) ) ;
#14379 = ORIENTED_EDGE ( 'NONE', *, *, #76214, .T. ) ;
#14380 = ADVANCED_FACE ( 'NONE', ( #42820 ), #38167, .T. ) ;
#14381 = CARTESIAN_POINT ( 'NONE',  ( -2.266590686148945544, 41.38708216824729647, -7.082119434687050408 ) ) ;
#14382 = CARTESIAN_POINT ( 'NONE',  ( 12.63842701281683034, 2.467264484334118269, 9.846743663894596210 ) ) ;
#14383 = PLANE ( 'NONE',  #83423 ) ;
#14384 = CARTESIAN_POINT ( 'NONE',  ( 19.42250999205614548, 30.98035201082150536, -5.440088680355545492 ) ) ;
#14385 = CARTESIAN_POINT ( 'NONE',  ( 6.565887622018943937, 43.08196800326374643, -12.81628187352647608 ) ) ;
#14386 = CARTESIAN_POINT ( 'NONE',  ( 2.035157376598824452, 8.688685344154839285, 7.964842623401179544 ) ) ;
#14387 = CARTESIAN_POINT ( 'NONE',  ( 16.40814093676323893, 30.79030133659708923, 11.09922568453595026 ) ) ;
#14388 = CARTESIAN_POINT ( 'NONE',  ( 5.076628168052704559, 5.175597817667451750, -8.527530157486179263 ) ) ;
#14390 = ORIENTED_EDGE ( 'NONE', *, *, #87839, .T. ) ;
#14389 = EDGE_CURVE ( 'NONE', #49831, #32093, #73793, .T. ) ;
#14391 = CARTESIAN_POINT ( 'NONE',  ( -11.22915323889586858, -0.03417435944610275333, 8.773176023390528044 ) ) ;
#14392 = CARTESIAN_POINT ( 'NONE',  ( -7.778994393464220281, -1.060811710757841198, -4.000000000000000000 ) ) ;
#14393 = CARTESIAN_POINT ( 'NONE',  ( -2.266590686148945544, 36.38708216824730357, -7.082119434687050408 ) ) ;
#14394 = CARTESIAN_POINT ( 'NONE',  ( 19.42250999205614548, 5.980352010821504471, -5.440088680355545492 ) ) ;
#14395 = CARTESIAN_POINT ( 'NONE',  ( 20.88017736071110519, 25.56368534415483751, 2.639326808657452039E-16 ) ) ;
#14396 = CARTESIAN_POINT ( 'NONE',  ( -13.14228782657345107, 0.5000000000000004441, 7.230509711182143917 ) ) ;
#14397 = DIRECTION ( 'NONE',  ( 0.000000000000000000, 0.000000000000000000, -1.000000000000000000 ) ) ;
#14398 = CARTESIAN_POINT ( 'NONE',  ( 19.42250999205614193, 50.14701867748817676, 5.440088680355555262 ) ) ;
#14399 = CARTESIAN_POINT ( 'NONE',  ( 2.035157376598824452, 63.68868534415484106, 7.964842623401179544 ) ) ;
#14400 = CARTESIAN_POINT ( 'NONE',  ( 0.6178305044545838731, 24.74863466993042493, 9.382169495545420901 ) ) ;
#14401 = CARTESIAN_POINT ( 'NONE',  ( -36.44000000000001194, 92.00000000000000000, -10.09898361729590199 ) ) ;
#14402 = CARTESIAN_POINT ( 'NONE',  ( -0.1503990784575328643, 30.12777174578613781, 6.262539305110068177 ) ) ;
#14403 = CARTESIAN_POINT ( 'NONE',  ( 19.84674366389459621, 23.50893115100078390, 7.409399052514197653E-17 ) ) ;
#14404 = CARTESIAN_POINT ( 'NONE',  ( 20.88017736071110875, 55.77201867748816966, -2.915334737309920765 ) ) ;
#14405 = CARTESIAN_POINT ( 'NONE',  ( 3.591859063236761518, 24.95696800326375353, 11.09922568453594849 ) ) ;
#14406 = B_SPLINE_CURVE_WITH_KNOTS ( 'NONE', 3,
 ( #54087, #69595, #84109, #46110 ),
 .UNSPECIFIED., .F., .F.,
 ( 4, 4 ),
 ( 0.000000000000000000, 0.001036303429213365941 ),
 .UNSPECIFIED. ) ;
#14407 = CARTESIAN_POINT ( 'NONE',  ( 0.1532563361054100626, 0.8005978176674514168, -2.638427012816831230 ) ) ;
#14408 = CARTESIAN_POINT ( 'NONE',  ( 17.96484262340118221, 11.18868534415483929, -7.964842623401177768 ) ) ;
#14409 = CARTESIAN_POINT ( 'NONE',  ( 19.84674366389459621, 43.50893115100078745, 7.409399052514197653E-17 ) ) ;
#14410 = CARTESIAN_POINT ( 'NONE',  ( 21.09922568453595559, 57.04030133659708923, -6.408140936763230044 ) ) ;
#14412 = CARTESIAN_POINT ( 'NONE',  ( -0.3689425029237881626, 2.428748834913967869, 10.36894250292379027 ) ) ;
#14411 = CARTESIAN_POINT ( 'NONE',  ( 18.52753015748618282, 18.92559781766745175, -4.923371831947291888 ) ) ;
#14413 = CARTESIAN_POINT ( 'NONE',  ( 10.00000000000000000, 0.5537488349139675359, -14.16423886937410082 ) ) ;
#14414 = DIRECTION ( 'NONE',  ( 0.000000000000000000, 1.000000000000000000, 0.000000000000000000 ) ) ;
#14415 = CARTESIAN_POINT ( 'NONE',  ( 10.00000000000000178, 39.31368534415484106, 10.88017736071110342 ) ) ;
#14417 = CARTESIAN_POINT ( 'NONE',  ( -0.3689425029237881626, 32.42874883491395366, 10.36894250292379027 ) ) ;
#14416 = FILL_AREA_STYLE ('',( #67404 ) ) ;
#14418 = CARTESIAN_POINT ( 'NONE',  ( 2.791683348922237240, 40.38393115100078035, -7.208316651077763204 ) ) ;
#14419 = CARTESIAN_POINT ( 'NONE',  ( 20.88017736071110875, 30.77201867748816966, -2.915334737309920765 ) ) ;
#14420 = CARTESIAN_POINT ( 'NONE',  ( 0.5774900079438590739, 17.64701867748817321, -5.440088680355550821 ) ) ;
#14421 = EDGE_LOOP ( 'NONE', ( #82401, #48232, #61079, #36600, #31018, #86483, #54097, #97718, #95483, #13962, #98341, #41268, #96085, #36314, #7777, #26625, #78238, #46671, #53088, #430, #12429, #5732, #95324, #17056, #24789, #92005, #73090, #29411, #18057, #81583, #52999, #8641, #72437 ) ) ;
#14422 = AXIS2_PLACEMENT_3D ( 'NONE', #51338, #11367, #34346 ) ;
#14423 = CARTESIAN_POINT ( 'NONE',  ( 17.96484262340118221, 31.18868534415483751, -7.964842623401177768 ) ) ;
#14424 = CARTESIAN_POINT ( 'NONE',  ( -1.099225684535947600, 48.70696800326375353, -6.408140936763238038 ) ) ;
#14425 = EDGE_CURVE ( 'NONE', #11778, #93697, #34349, .T. ) ;
#14426 = CARTESIAN_POINT ( 'NONE',  ( 19.42250999205614193, 45.14701867748817676, 5.440088680355555262 ) ) ;
#14428 = CARTESIAN_POINT ( 'NONE',  ( 4.559911319644449179, 38.89701867748817676, 9.422509992056141925 ) ) ;
#14427 = CARTESIAN_POINT ( 'NONE',  ( 12.99999999999999822, 75.00000000000000000, -6.500000000000000888 ) ) ;
#14429 = VERTEX_POINT ( 'NONE', #4339 ) ;
#14430 = CARTESIAN_POINT ( 'NONE',  ( 2.791683348922240793, 51.63393115100078745, 7.208316651077764092 ) ) ;
#14431 = CARTESIAN_POINT ( 'NONE',  ( 2.035157376598822676, 37.43868534415484106, -7.964842623401177768 ) ) ;
#14432 = CARTESIAN_POINT ( 'NONE',  ( 6.935087012957517949, -80.58470470491535309, 3.750000000000000000 ) ) ;
#14433 = CARTESIAN_POINT ( 'NONE',  ( -7.750355510519348456, 84.07179676972448590, 4.000000000000000000 ) ) ;
#14434 = CARTESIAN_POINT ( 'NONE',  ( 20.36894250292379382, 43.67874883491397497, 10.36894250292379205 ) ) ;
#14435 = CARTESIAN_POINT ( 'NONE',  ( -0.8801773607110991993, 47.85535201082150536, -2.915334737309923874 ) ) ;
#14436 = FACE_OUTER_BOUND ( 'NONE', #709, .T. ) ;
#14437 = CARTESIAN_POINT ( 'NONE',  ( -10.77730536144846596, -98.63085534186639336, -3.750000000000000000 ) ) ;
#14438 = CARTESIAN_POINT ( 'NONE',  ( 2.791683348922240793, 61.63393115100079456, 7.208316651077764092 ) ) ;
#14439 = CARTESIAN_POINT ( 'NONE',  ( -25.69000000000001194, 93.50000000000000000, 9.500000000000000000 ) ) ;
#14440 = CARTESIAN_POINT ( 'NONE',  ( 7.361572987183169658, 29.96726448433411960, -9.846743663894592657 ) ) ;
#14441 = ORIENTED_EDGE ( 'NONE', *, *, #45534, .T. ) ;
#14442 = CARTESIAN_POINT ( 'NONE',  ( 2.791683348922240793, 36.63393115100078035, 7.208316651077764092 ) ) ;
#14443 = CARTESIAN_POINT ( 'NONE',  ( -11.09922568453595382, -21.29303199673624292, -6.408140936763226492 ) ) ;
#14444 = CARTESIAN_POINT ( 'NONE',  ( 20.88017736071110519, 20.56368534415484106, 2.639326808657452039E-16 ) ) ;
#14445 = CARTESIAN_POINT ( 'NONE',  ( 17.20831665107776587, 27.88393115100078390, 7.208316651077764980 ) ) ;
#14446 = CARTESIAN_POINT ( 'NONE',  ( -1.099225684535947600, 19.54030133659708568, 6.408140936763237150 ) ) ;
#14448 = CARTESIAN_POINT ( 'NONE',  ( 12.91533473730993009, 61.60535201082150536, -10.88017736071109987 ) ) ;
#14447 = CARTESIAN_POINT ( 'NONE',  ( 18.72515096720569971, 5.055090184799359676, 6.500000000000000000 ) ) ;
#14450 = SURFACE_SIDE_STYLE ('',( #76898 ) ) ;
#14449 = CARTESIAN_POINT ( 'NONE',  ( 15.44008868035555260, 34.73035201082151247, 9.422509992056143702 ) ) ;
#14451 = CARTESIAN_POINT ( 'NONE',  ( -2.266590686148945544, 41.38708216824729647, -7.082119434687050408 ) ) ;
#14452 = B_SPLINE_CURVE_WITH_KNOTS ( 'NONE', 3,
 ( #29207, #44206, #21226, #84207, #51730, #97744 ),
 .UNSPECIFIED., .F., .F.,
 ( 4, 2, 4 ),
 ( 0.0002800630492218076652, 0.0006862688956327564049, 0.001092474742043705090 ),
 .UNSPECIFIED. ) ;
#14453 = CARTESIAN_POINT ( 'NONE',  ( -14.37657372141817724, 15.00000000000000888, 2.693041920167245529 ) ) ;
#14454 = ORIENTED_EDGE ( 'NONE', *, *, #1891, .F. ) ;
#14455 = CARTESIAN_POINT ( 'NONE',  ( 21.09922568453594849, 16.20696800326375353, 6.408140936763242479 ) ) ;
#14456 = CARTESIAN_POINT ( 'NONE',  ( 17.96484262340118221, 6.188685344154836621, -7.964842623401177768 ) ) ;
#14457 = CARTESIAN_POINT ( 'NONE',  ( 0.5774900079438607392, 53.48035201082151247, 5.440088680355550821 ) ) ;
#14458 =( NAMED_UNIT ( * ) PLANE_ANGLE_UNIT ( ) SI_UNIT ( $, .RADIAN. ) );
#14459 = VERTEX_POINT ( 'NONE', #3845 ) ;
#14460 = CARTESIAN_POINT ( 'NONE',  ( 10.00000000000000178, 59.31368534415484106, 10.88017736071110342 ) ) ;
#14461 = CARTESIAN_POINT ( 'NONE',  ( 19.84674366389459266, 38.30059781766745175, 2.638427012816836559 ) ) ;
#14462 = CARTESIAN_POINT ( 'NONE',  ( 2.791683348922237240, 20.38393115100078745, -7.208316651077763204 ) ) ;
#14463 = CARTESIAN_POINT ( 'NONE',  ( 10.00000000000000000, 9.758931151000785675, -9.846743663894594434 ) ) ;
#14465 = CARTESIAN_POINT ( 'NONE',  ( 3.591859063236763294, 38.29030133659708923, -11.09922568453595026 ) ) ;
#14464 = CARTESIAN_POINT ( 'NONE',  ( -7.037799269745396380, -86.25965645050762021, 2.499999999998388400 ) ) ;
#14467 = DIRECTION ( 'NONE',  ( 0.000000000000000000, 0.000000000000000000, 1.000000000000000000 ) ) ;
#14466 = CARTESIAN_POINT ( 'NONE',  ( 17.20831665107776587, 17.88393115100078745, 7.208316651077764980 ) ) ;
#14468 = DIRECTION ( 'NONE',  ( 0.000000000000000000, 0.000000000000000000, 1.000000000000000000 ) ) ;
#14470 = ORIENTED_EDGE ( 'NONE', *, *, #5361, .F. ) ;
#14469 = CARTESIAN_POINT ( 'NONE',  ( 12.63842701281683922, 29.55059781766745175, -9.846743663894590881 ) ) ;
#14471 = VECTOR ( 'NONE', #83756, 1000.000000000000000 ) ;
#14472 = EDGE_CURVE ( 'NONE', #6265, #21520, #18331, .T. ) ;
#14473 = CARTESIAN_POINT ( 'NONE',  ( -1.099225684535947600, 54.54030133659708923, 6.408140936763237150 ) ) ;
#14474 = DIRECTION ( 'NONE',  ( -0.000000000000000000, -1.000000000000000000, -0.000000000000000000 ) ) ;
#14475 = CARTESIAN_POINT ( 'NONE',  ( 10.00000000000000000, 12.87363466993042138, -12.81628187352647608 ) ) ;
#14476 = ADVANCED_FACE ( 'NONE', ( #96329 ), #27804, .F. ) ;
#14477 = CARTESIAN_POINT ( 'NONE',  ( 17.96484262340118221, 46.18868534415484106, -7.964842623401177768 ) ) ;
#14479 = ADVANCED_FACE ( 'NONE', ( #95825 ), #53768, .F. ) ;
#14478 = CARTESIAN_POINT ( 'NONE',  ( 20.36894250292379738, 34.92874883491396076, -10.36894250292379027 ) ) ;
#14480 = AXIS2_PLACEMENT_3D ( 'NONE', #22394, #13396, #43879 ) ;
#14481 = UNCERTAINTY_MEASURE_WITH_UNIT (LENGTH_MEASURE( 1.000000000000000082E-05 ), #4762, 'distance_accuracy_value', 'NONE');
#14482 = CARTESIAN_POINT ( 'NONE',  ( 1.932340009482166776, 41.49127512925448258, -6.500000000000040856 ) ) ;
#14483 = CARTESIAN_POINT ( 'NONE',  ( 24.16423886937409904, 24.09541550158063927, 3.795296366450317205 ) ) ;
#14484 = CARTESIAN_POINT ( 'NONE',  ( 22.26659068614895176, 39.72041550158063217, -7.082119434687042414 ) ) ;
#14485 = CARTESIAN_POINT ( 'NONE',  ( 13.79529636645030344, 3.262082168247301350, 14.16423886937410614 ) ) ;
#14487 = CARTESIAN_POINT ( 'NONE',  ( -1.926860441876564023, 37.87045670184114954, 3.195792623639529761 ) ) ;
#14486 = CARTESIAN_POINT ( 'NONE',  ( -2.266590686148945544, 12.22041550158063394, 7.082119434687048631 ) ) ;
#14488 = CARTESIAN_POINT ( 'NONE',  ( 2.035157376598822676, 47.43868534415484817, -7.964842623401177768 ) ) ;
#14489 = CARTESIAN_POINT ( 'NONE',  ( -3.897244926436033374, 15.00000000000000000, -13.96644127841335958 ) ) ;
#14490 = CARTESIAN_POINT ( 'NONE',  ( 18.52753015748618282, 23.92559781766745530, -4.923371831947291888 ) ) ;
#14493 = VECTOR ( 'NONE', #85145, 1000.000000000000000 ) ;
#14492 = CARTESIAN_POINT ( 'NONE',  ( 1.472469842513823179, 26.42559781766745175, 4.923371831947296329 ) ) ;
#14491 = DIRECTION ( 'NONE',  ( 1.000000000000000000, 0.000000000000000000, 0.000000000000000000 ) ) ;
#14494 = EDGE_CURVE ( 'NONE', #59039, #26330, #52563, .T. ) ;
#14495 = CARTESIAN_POINT ( 'NONE',  ( 12.91533473730993009, 26.60535201082150536, -10.88017736071109987 ) ) ;
#14496 = CARTESIAN_POINT ( 'NONE',  ( 16.40814093676323893, 60.79030133659709634, 11.09922568453595026 ) ) ;
#14497 = LINE ( 'NONE', #92436, #76131 ) ;
#14498 =( NAMED_UNIT ( * ) PLANE_ANGLE_UNIT ( ) SI_UNIT ( $, .RADIAN. ) );
#14499 = CARTESIAN_POINT ( 'NONE',  ( 10.00000000000000000, 24.75893115100078745, -9.846743663894594434 ) ) ;
#14500 = CARTESIAN_POINT ( 'NONE',  ( 16.40814093676324603, 47.45696800326375353, -11.09922568453594671 ) ) ;
#14501 = CARTESIAN_POINT ( 'NONE',  ( -5.204170427930421283E-15, -14.44625116508602858, -14.16423886937410082 ) ) ;
#14502 = CARTESIAN_POINT ( 'NONE',  ( 19.42250999205614193, 40.14701867748817676, 5.440088680355555262 ) ) ;
#14503 = CARTESIAN_POINT ( 'NONE',  ( 19.84674366389459266, 53.71726448433411605, -2.638427012816827677 ) ) ;
#14504 = CARTESIAN_POINT ( 'NONE',  ( -4.164238869374099039, 21.80374883491396787, 8.674139862899312516E-16 ) ) ;
#14505 = VERTEX_POINT ( 'NONE', #30264 ) ;
#14506 = LINE ( 'NONE', #74489, #77903 ) ;
#14507 = CARTESIAN_POINT ( 'NONE',  ( -0.8801773607111008646, 68.27201867748817676, 2.915334737309923430 ) ) ;
#14508 = CARTESIAN_POINT ( 'NONE',  ( -0.9940297508535884674, 15.00000000000000000, -14.21528771620250886 ) ) ;
#14509 = CARTESIAN_POINT ( 'NONE',  ( -2.266590686148945544, 62.22041550158063927, 7.082119434687048631 ) ) ;
#14510 = CARTESIAN_POINT ( 'NONE',  ( -1.099225684535947600, 4.540301336597087456, 6.408140936763237150 ) ) ;
#14511 = CARTESIAN_POINT ( 'NONE',  ( 2.888814634336697829, 15.00000000000000711, 14.33747749179070752 ) ) ;
#14512 = CARTESIAN_POINT ( 'NONE',  ( 17.96484262340118221, 51.18868534415483396, -7.964842623401177768 ) ) ;
#14513 = ADVANCED_FACE ( 'NONE', ( #37306 ), #28544, .T. ) ;
#14514 = CARTESIAN_POINT ( 'NONE',  ( 6.000000000000000000, 10.49999999999999822, 6.500000000000000888 ) ) ;
#14515 = CARTESIAN_POINT ( 'NONE',  ( 6.204703633549690345, 55.76208216824730357, -14.16423886937410259 ) ) ;
#14516 = CARTESIAN_POINT ( 'NONE',  ( 7.964842623401181321, 29.93868534415484461, 7.964842623401174215 ) ) ;
#14517 = CARTESIAN_POINT ( 'NONE',  ( 20.88017736071110519, 10.56368534415483751, 2.639326808657452039E-16 ) ) ;
#14518 = CARTESIAN_POINT ( 'NONE',  ( 4.559911319644449179, 27.23035201082150536, -9.422509992056141925 ) ) ;
#14519 = CARTESIAN_POINT ( 'NONE',  ( 12.63842701281683034, 62.46726448433410894, 9.846743663894596210 ) ) ;
#14520 = CARTESIAN_POINT ( 'NONE',  ( 21.09922568453594849, 46.20696800326376064, 6.408140936763242479 ) ) ;
#14521 = CARTESIAN_POINT ( 'NONE',  ( -7.750000000000000000, 1.019547802438458550, -4.000000000000000000 ) ) ;
#14522 = ORIENTED_EDGE ( 'NONE', *, *, #90421, .F. ) ;
#14523 = AXIS2_PLACEMENT_3D ( 'NONE', #8588, #9569, #70081 ) ;
#14524 = CARTESIAN_POINT ( 'NONE',  ( 0.5774900079438607392, 13.48035201082150358, 5.440088680355550821 ) ) ;
#14525 = CARTESIAN_POINT ( 'NONE',  ( 21.09922568453595559, 22.04030133659708923, -6.408140936763230044 ) ) ;
#14526 = FACE_OUTER_BOUND ( 'NONE', #14613, .T. ) ;
#14527 = AXIS2_PLACEMENT_3D ( 'NONE', #44706, #75206, #37233 ) ;
#14528 = CARTESIAN_POINT ( 'NONE',  ( 0.1532563361054083140, 51.00893115100078745, 1.131784320476157264E-15 ) ) ;
#14529 = CARTESIAN_POINT ( 'NONE',  ( 0.5774900079438607392, 38.48035201082150536, 5.440088680355550821 ) ) ;
#14530 = CARTESIAN_POINT ( 'NONE',  ( 22.81628187352648496, 26.83196800326374998, -3.434112377981050290 ) ) ;
#14532 = DIRECTION ( 'NONE',  ( -1.049065152435176504E-16, 1.000000000000000000, -0.000000000000000000 ) ) ;
#14531 = CARTESIAN_POINT ( 'NONE',  ( 2.035157376598822676, 47.43868534415484817, -7.964842623401177768 ) ) ;
#14533 = CARTESIAN_POINT ( 'NONE',  ( 13.43411237798106583, 47.66530133659709634, -12.81628187352647252 ) ) ;
#14534 = VERTEX_POINT ( 'NONE', #71240 ) ;
#14535 = CARTESIAN_POINT ( 'NONE',  ( 1.274849032794305170, 17.55509018479936145, -6.499999999999995559 ) ) ;
#14536 = CARTESIAN_POINT ( 'NONE',  ( 20.88017736071110519, 50.56368534415484106, 2.639326808657452039E-16 ) ) ;
#14538 = CARTESIAN_POINT ( 'NONE',  ( -0.3689425029237898834, 6.178748834913968757, -10.36894250292378850 ) ) ;
#14537 = CARTESIAN_POINT ( 'NONE',  ( 0.6178305044545838731, 39.74863466993041072, 9.382169495545420901 ) ) ;
#14539 = CARTESIAN_POINT ( 'NONE',  ( 20.88017736071110164, 45.35535201082149115, 2.915334737309930979 ) ) ;
#14540 = CARTESIAN_POINT ( 'NONE',  ( 1.472469842513823179, 66.42559781766745175, 4.923371831947296329 ) ) ;
#14541 = CARTESIAN_POINT ( 'NONE',  ( 1.472469842513823179, 61.42559781766745175, 4.923371831947296329 ) ) ;
#14542 = CARTESIAN_POINT ( 'NONE',  ( 18.52753015748618282, 13.92559781766745175, -4.923371831947291888 ) ) ;
#14543 = CARTESIAN_POINT ( 'NONE',  ( 17.20831665107776587, 12.88393115100078390, 7.208316651077764980 ) ) ;
#14544 = DIRECTION ( 'NONE',  ( 1.000000000000000000, 2.569960705150826877E-16, -0.000000000000000000 ) ) ;
#14545 = CARTESIAN_POINT ( 'NONE',  ( 22.26659068614895176, 49.72041550158063927, -7.082119434687042414 ) ) ;
#14546 = CARTESIAN_POINT ( 'NONE',  ( 0.000000000000000000, 1.823139558123437975, 0.000000000000000000 ) ) ;
#14547 = CARTESIAN_POINT ( 'NONE',  ( 8.900374253113422895, -1.048990366506262317, -3.750000000000001332 ) ) ;
#14548 = CARTESIAN_POINT ( 'NONE',  ( -7.371446924914479837, -73.25787537890647627, -4.000000000000000888 ) ) ;
#14549 =( BOUNDED_SURFACE ( )  B_SPLINE_SURFACE ( 1, 2, ( 
 ( #67944, #20471, #66448, #75435, #5963, #14956, #22450, #74438, #66952, #50958, #13453, #59439, #12955, #44439, #6949, #74941, #51955, #97470, #37950, #82440, #36953, #14456, #58954, #28934, #89941, #21458, #44928, #67450, #81944, #37456, #52923, #98468, #28460, #13964, #97971, #29427, #59932, #90420, #21960, #75928, #88963, #43939, #82939, #52441, #81454, #58448, #96983, #89454, #20970, #73952, #29921, #60427, #5479, #83436, #90920, #45423, #7453, #96483, #27955, #43451, #51455, #98962, #91423, #93388, #7938, #1434, #53920, #38434, #70408, #91917, #76424, #9401, #46898, #24422, #55397, #24913, #17414, #22951, #53417, #85897, #54886, #85402, #38927, #30418, #16421, #77389, #47880, #69914, #16914, #61897, #68932, #78384, #61408, #76907, #60918, #23927, #9904, #68442, #462, #62889, #83924, #30910, #8902, #15454, #45933, #937, #92404, #47387, #39419, #84429, #77889, #23441, #39902, #15926, #54398, #8420, #31887, #84909, #62385, #92890, #46417, #69414, #31397, #1926, #32384, #93881, #2421, #10391, #71396, #63856, #17892, #72839, #41884, #48376, #65337, #49849, #10880, #11365, #64353, #41404, #50338, #94370, #70901, #63376, #95863, #78880, #72348, #25888, #40895, #42366, #56387, #2910, #80358, #18878, #95357, #27346, #57839, #88348, #25408, #55895, #19846, #26856, #57353, #71870, #32878, #87364, #49360, #80849, #3880, #87846, #33844, #33361, #40407, #86876, #48865, #86391, #94861, #18386, #79375, #3381, #34842, #26364, #56863, #79862, #34344, #64838, #19366, #11858, #4377, #6324, #59809, #6823, #43334, #89334, #67829, #14334, #73826, #82317, #44807, #13837, #51829, #13336, #36834, #44318, #74819, #90303, #12834, #60313, #90805, #82814, #35339, #50845, #21838, #20844, #29804, #37339, #51336, #81818, #65832, #28336, #74316, #27837, #59319, #52321, #89818, #66827, #43820, #52807, #97349, #67325, #29313, #5359, #5842, #35838, #28820, #36332, #97848, #21339, #75313, #98347, #22333, #4863, #58826, #12346, #42853, #96364, #73336, #81337, #66326, #96861, #88841, #58324, #20349, #60798, #9283, #92776, #53805, #54276, #8306, #84316, #93270, #7822, #14838, #7330, #39792, #22822, #16302, #68813, #53301, #85286, #38317, #91298, #24305, #61782, #39306, #70292, #1807, #32264, #37831, #68321, #62769, #69798, #1323, #15816, #45312, #31282, #92292, #24794, #84793, #31774, #76789, #83809, #83314, #76305, #91802, #75808, #38806, #98840, #30295, #15335, #77771, #45817, #346, #23815, #30788, #61293, #23324, #46783, #46302, #77277, #62267, #69302, #824, #8787, #54767, #16794, #47270, #26250, #57230, #56745, #94745, #56270, #79747, #87239, #18764 ),
 ( #4252, #33730, #25291, #42247, #10275, #86762, #55775, #18267, #41280, #49245, #10765, #11738, #11243, #86269, #41763, #72234, #40279, #48746, #3764, #34221, #64230, #34722, #26736, #64718, #72717, #95227, #33250, #79254, #63255, #40773, #55270, #87728, #71754, #19241, #3263, #71275, #49723, #80232, #17781, #93763, #65215, #95740, #85782, #47769, #17293, #2797, #78267, #9781, #70786, #48256, #2303, #63743, #32759, #78766, #94246, #25775, #59199, #81702, #82699, #89703, #96239, #82202, #21217, #12225, #20727, #28708, #51719, #5728, #6705, #97735, #66715, #44698, #36720, #75194, #97239, #36215, #44196, #65713, #29197, #89214, #51216, #13713, #43212, #66207, #74706, #27719, #43708, #14218, #27222, #67210, #37225, #67710, #35718, #13214, #6216, #74195, #96739, #59695, #57720, #90192, #21722, #20226, #28214, #58200, #80730, #88221, #58712, #19731, #50217, #88716, #52205, #42735, #73213, #4744, #35210, #50731, #81219, #12720, #73707, #5240, #46189, #7205, #16677, #60683, #39184, #1202, #53190, #30671, #84195, #54163, #37706, #53678, #83197, #68207, #92177, #61655, #47149, #98729, #84675, #15211, #91182, #9164, #61179, #54650, #77164, #77650, #46666, #39682, #31165, #16183, #60193, #23703, #75693, #91684, #76189, #68691, #22216, #45690, #23203, #14721, #76673, #8672, #8192, #15704, #38204, #98223, #38689, #69188, #69673, #22708, #7709, #711, #31660, #62147, #92655, #83693, #24181, #85168, #29684, #30179, #90688, #222, #52693, #45195, #64111, #18153, #49601, #62643, #17665, #56631, #2679, #24672, #32142, #40158, #2185, #93643, #47658, #3641, #71642, #78152, #95107, #79629, #40655, #41157, #94131, #71153, #80110, #25176, #1688, #93148, #26614, #9663, #3150, #55657, #70664, #72115, #86154, #32644, #11130, #48627, #26138, #57111, #87609, #19120, #55143, #85657, #11617, #87119, #18637, #33130, #17176, #79131, #10643, #70172, #33615, #49127, #63625, #63140, #48138, #78653, #10158, #25658, #56151, #86645, #94627, #41648, #64597, #34106, #12110, #81584, #34598, #95616, #80615, #20607, #72599, #36089, #89589, #36601, #73091, #20102, #97616, #44074, #4629, #13093, #74582, #43589, #74078, #43099, #66594, #5611, #97121, #21098, #42612, #90074, #21600, #13592, #65092, #35092, #51598, #50605, #59581, #67088, #28592, #58591, #81097, #59082, #42133, #82082, #6097, #65591, #12599, #96117, #27103, #52089, #73586, #82582, #4135, #27601, #28093, #5110, #29076, #57603, #88103, #51096, #19612, #58089, #50107, #88593, #89093, #35599, #66087, #96616, #54051, #16064, #68083, #45569, #108, #69068, #52574, #68576, #98101, #83078, #8074, #76556, #31540 ) ),
 .UNSPECIFIED., .F., .F., .F. ) 
 B_SPLINE_SURFACE_WITH_KNOTS ( ( 2, 2 ),
 ( 3, 2, 2, 2, 2, 2, 2, 2, 2, 2, 2, 2, 2, 2, 2, 2, 2, 2, 2, 2, 2, 2, 2, 2, 2, 2, 2, 2, 2, 2, 2, 2, 2, 2, 2, 2, 2, 2, 2, 2, 2, 2, 2, 2, 2, 2, 2, 2, 2, 2, 2, 2, 2, 2, 2, 2, 2, 2, 2, 2, 2, 2, 2, 2, 2, 2, 2, 2, 2, 2, 2, 2, 2, 2, 2, 2, 2, 2, 2, 2, 2, 2, 2, 2, 2, 2, 2, 2, 2, 2, 2, 2, 2, 2, 2, 2, 2, 2, 2, 2, 2, 2, 2, 2, 2, 2, 2, 2, 2, 2, 2, 2, 2, 2, 2, 2, 2, 2, 2, 2, 2, 2, 2, 2, 2, 2, 2, 2, 2, 2, 2, 2, 2, 2, 2, 2, 2, 2, 2, 2, 2, 2, 2, 2, 2, 2, 2, 2, 2, 2, 2, 2, 2, 2, 2, 2, 2, 2, 2, 2, 2, 2, 3 ),
 ( 0.000000000000000000, 1.000000000000000000 ),
 ( 0.000000000000000000, 0.005952380952380952051, 0.01190476190476190410, 0.01785714285714285615, 0.02380952380952380820, 0.02976190476190476025, 0.03571428571428571230, 0.04166666666666666435, 0.04761904761904761640, 0.05357142857142856845, 0.05952380952380952051, 0.06547619047619047949, 0.07142857142857142461, 0.07738095238095238360, 0.08333333333333332871, 0.08928571428571428770, 0.09523809523809523281, 0.1011904761904761918, 0.1071428571428571369, 0.1130952380952380959, 0.1190476190476190410, 0.1250000000000000000, 0.1309523809523809590, 0.1369047619047619180, 0.1428571428571428492, 0.1488095238095238082, 0.1547619047619047672, 0.1607142857142857262, 0.1666666666666666574, 0.1726190476190476164, 0.1785714285714285754, 0.1845238095238095344, 0.1904761904761904656, 0.1964285714285714246, 0.2023809523809523836, 0.2083333333333333426, 0.2142857142857142738, 0.2202380952380952328, 0.2261904761904761918, 0.2321428571428571508, 0.2380952380952380820, 0.2440476190476190410, 0.2500000000000000000, 0.2559523809523809312, 0.2619047619047619180, 0.2678571428571428492, 0.2738095238095238360, 0.2797619047619047672, 0.2857142857142856984, 0.2916666666666666852, 0.2976190476190476164, 0.3035714285714285476, 0.3095238095238095344, 0.3154761904761904656, 0.3214285714285714524, 0.3273809523809523836, 0.3333333333333333148, 0.3392857142857143016, 0.3452380952380952328, 0.3511904761904761640, 0.3571428571428571508, 0.3630952380952380820, 0.3690476190476190688, 0.3750000000000000000, 0.3809523809523809312, 0.3869047619047619180, 0.3928571428571428492, 0.3988095238095238360, 0.4047619047619047672, 0.4107142857142856984, 0.4166666666666666852, 0.4226190476190476164, 0.4285714285714285476, 0.4345238095238095344, 0.4404761904761904656, 0.4464285714285714524, 0.4523809523809523836, 0.4583333333333333148, 0.4642857142857143016, 0.4702380952380952328, 0.4761904761904761640, 0.4821428571428571508, 0.4880952380952380820, 0.4940476190476190688, 0.5000000000000000000, 0.5059523809523809312, 0.5119047619047618625, 0.5178571428571429047, 0.5238095238095238360, 0.5297619047619047672, 0.5357142857142856984, 0.5416666666666666297, 0.5476190476190476719, 0.5535714285714286031, 0.5595238095238095344, 0.5654761904761904656, 0.5714285714285713969, 0.5773809523809523281, 0.5833333333333333703, 0.5892857142857143016, 0.5952380952380952328, 0.6011904761904761640, 0.6071428571428570953, 0.6130952380952381375, 0.6190476190476190688, 0.6250000000000000000, 0.6309523809523809312, 0.6369047619047618625, 0.6428571428571429047, 0.6488095238095238360, 0.6547619047619047672, 0.6607142857142856984, 0.6666666666666666297, 0.6726190476190476719, 0.6785714285714286031, 0.6845238095238095344, 0.6904761904761904656, 0.6964285714285713969, 0.7023809523809523281, 0.7083333333333333703, 0.7142857142857143016, 0.7202380952380952328, 0.7261904761904761640, 0.7321428571428570953, 0.7380952380952381375, 0.7440476190476190688, 0.7500000000000000000, 0.7559523809523809312, 0.7619047619047618625, 0.7678571428571429047, 0.7738095238095238360, 0.7797619047619047672, 0.7857142857142856984, 0.7916666666666666297, 0.7976190476190476719, 0.8035714285714286031, 0.8095238095238095344, 0.8154761904761904656, 0.8214285714285713969, 0.8273809523809523281, 0.8333333333333333703, 0.8392857142857143016, 0.8452380952380952328, 0.8511904761904761640, 0.8571428571428570953, 0.8630952380952381375, 0.8690476190476190688, 0.8750000000000000000, 0.8809523809523809312, 0.8869047619047618625, 0.8928571428571429047, 0.8988095238095238360, 0.9047619047619047672, 0.9107142857142856984, 0.9166666666666666297, 0.9226190476190476719, 0.9285714285714286031, 0.9345238095238095344, 0.9404761904761904656, 0.9464285714285713969, 0.9523809523809523281, 0.9583333333333333703, 0.9642857142857143016 ),
 .UNSPECIFIED. ) 
 GEOMETRIC_REPRESENTATION_ITEM ( )  RATIONAL_B_SPLINE_SURFACE ( (
 ( 1.000000000000000000, 0.9659258262890683122, 1.000000000000000000, 0.9659258262890683122, 1.000000000000000000, 0.9659258262890683122, 1.000000000000000000, 0.9659258262890683122, 1.000000000000000000, 0.9659258262890683122, 1.000000000000000000, 0.9659258262890683122, 1.000000000000000000, 0.9659258262890683122, 1.000000000000000000, 0.9659258262890683122, 1.000000000000000000, 0.9659258262890683122, 1.000000000000000000, 0.9659258262890683122, 1.000000000000000000, 0.9659258262890683122, 1.000000000000000000, 0.9659258262890683122, 1.000000000000000000, 0.9659258262890683122, 1.000000000000000000, 0.9659258262890683122, 1.000000000000000000, 0.9659258262890683122, 1.000000000000000000, 0.9659258262890683122, 1.000000000000000000, 0.9659258262890683122, 1.000000000000000000, 0.9659258262890683122, 1.000000000000000000, 0.9659258262890683122, 1.000000000000000000, 0.9659258262890683122, 1.000000000000000000, 0.9659258262890683122, 1.000000000000000000, 0.9659258262890683122, 1.000000000000000000, 0.9659258262890683122, 1.000000000000000000, 0.9659258262890683122, 1.000000000000000000, 0.9659258262890683122, 1.000000000000000000, 0.9659258262890683122, 1.000000000000000000, 0.9659258262890683122, 1.000000000000000000, 0.9659258262890683122, 1.000000000000000000, 0.9659258262890683122, 1.000000000000000000, 0.9659258262890683122, 1.000000000000000000, 0.9659258262890683122, 1.000000000000000000, 0.9659258262890683122, 1.000000000000000000, 0.9659258262890683122, 1.000000000000000000, 0.9659258262890683122, 1.000000000000000000, 0.9659258262890683122, 1.000000000000000000, 0.9659258262890683122, 1.000000000000000000, 0.9659258262890683122, 1.000000000000000000, 0.9659258262890683122, 1.000000000000000000, 0.9659258262890683122, 1.000000000000000000, 0.9659258262890683122, 1.000000000000000000, 0.9659258262890683122, 1.000000000000000000, 0.9659258262890683122, 1.000000000000000000, 0.9659258262890683122, 1.000000000000000000, 0.9659258262890683122, 1.000000000000000000, 0.9659258262890683122, 1.000000000000000000, 0.9659258262890683122, 1.000000000000000000, 0.9659258262890683122, 1.000000000000000000, 0.9659258262890683122, 1.000000000000000000, 0.9659258262890683122, 1.000000000000000000, 0.9659258262890683122, 1.000000000000000000, 0.9659258262890683122, 1.000000000000000000, 0.9659258262890683122, 1.000000000000000000, 0.9659258262890683122, 1.000000000000000000, 0.9659258262890683122, 1.000000000000000000, 0.9659258262890683122, 1.000000000000000000, 0.9659258262890683122, 1.000000000000000000, 0.9659258262890683122, 1.000000000000000000, 0.9659258262890683122, 1.000000000000000000, 0.9659258262890683122, 1.000000000000000000, 0.9659258262890683122, 1.000000000000000000, 0.9659258262890683122, 1.000000000000000000, 0.9659258262890683122, 1.000000000000000000, 0.9659258262890683122, 1.000000000000000000, 0.9659258262890683122, 1.000000000000000000, 0.9659258262890683122, 1.000000000000000000, 0.9659258262890683122, 1.000000000000000000, 0.9659258262890683122, 1.000000000000000000, 0.9659258262890683122, 1.000000000000000000, 0.9659258262890683122, 1.000000000000000000, 0.9659258262890683122, 1.000000000000000000, 0.9659258262890683122, 1.000000000000000000, 0.9659258262890683122, 1.000000000000000000, 0.9659258262890683122, 1.000000000000000000, 0.9659258262890683122, 1.000000000000000000, 0.9659258262890683122, 1.000000000000000000, 0.9659258262890683122, 1.000000000000000000, 0.9659258262890683122, 1.000000000000000000, 0.9659258262890683122, 1.000000000000000000, 0.9659258262890683122, 1.000000000000000000, 0.9659258262890683122, 1.000000000000000000, 0.9659258262890683122, 1.000000000000000000, 0.9659258262890683122, 1.000000000000000000, 0.9659258262890683122, 1.000000000000000000, 0.9659258262890683122, 1.000000000000000000, 0.9659258262890683122, 1.000000000000000000, 0.9659258262890683122, 1.000000000000000000, 0.9659258262890683122, 1.000000000000000000, 0.9659258262890683122, 1.000000000000000000, 0.9659258262890683122, 1.000000000000000000, 0.9659258262890683122, 1.000000000000000000, 0.9659258262890683122, 1.000000000000000000, 0.9659258262890683122, 1.000000000000000000, 0.9659258262890683122, 1.000000000000000000, 0.9659258262890683122, 1.000000000000000000, 0.9659258262890683122, 1.000000000000000000, 0.9659258262890683122, 1.000000000000000000, 0.9659258262890683122, 1.000000000000000000, 0.9659258262890683122, 1.000000000000000000, 0.9659258262890683122, 1.000000000000000000, 0.9659258262890683122, 1.000000000000000000, 0.9659258262890683122, 1.000000000000000000, 0.9659258262890683122, 1.000000000000000000, 0.9659258262890683122, 1.000000000000000000, 0.9659258262890683122, 1.000000000000000000, 0.9659258262890683122, 1.000000000000000000, 0.9659258262890683122, 1.000000000000000000, 0.9659258262890683122, 1.000000000000000000, 0.9659258262890683122, 1.000000000000000000, 0.9659258262890683122, 1.000000000000000000, 0.9659258262890683122, 1.000000000000000000, 0.9659258262890683122, 1.000000000000000000, 0.9659258262890683122, 1.000000000000000000, 0.9659258262890683122, 1.000000000000000000, 0.9659258262890683122, 1.000000000000000000, 0.9659258262890683122, 1.000000000000000000, 0.9659258262890683122, 1.000000000000000000, 0.9659258262890683122, 1.000000000000000000, 0.9659258262890683122, 1.000000000000000000, 0.9659258262890683122, 1.000000000000000000, 0.9659258262890683122, 1.000000000000000000, 0.9659258262890683122, 1.000000000000000000, 0.9659258262890683122, 1.000000000000000000, 0.9659258262890683122, 1.000000000000000000, 0.9659258262890683122, 1.000000000000000000, 0.9659258262890683122, 1.000000000000000000, 0.9659258262890683122, 1.000000000000000000, 0.9659258262890683122, 1.000000000000000000, 0.9659258262890683122, 1.000000000000000000, 0.9659258262890683122, 1.000000000000000000, 0.9659258262890683122, 1.000000000000000000, 0.9659258262890683122, 1.000000000000000000, 0.9659258262890683122, 1.000000000000000000, 0.9659258262890683122, 1.000000000000000000, 0.9659258262890683122, 1.000000000000000000, 0.9659258262890683122, 1.000000000000000000, 0.9659258262890683122, 1.000000000000000000, 0.9659258262890683122, 1.000000000000000000, 0.9659258262890683122, 1.000000000000000000, 0.9659258262890683122, 1.000000000000000000, 0.9659258262890683122, 1.000000000000000000, 0.9659258262890683122, 1.000000000000000000, 0.9659258262890683122, 1.000000000000000000, 0.9659258262890683122, 1.000000000000000000, 0.9659258262890683122, 1.000000000000000000, 0.9659258262890683122, 1.000000000000000000, 0.9659258262890683122, 1.000000000000000000, 0.9659258262890683122, 1.000000000000000000, 0.9659258262890683122, 1.000000000000000000, 0.9659258262890683122, 1.000000000000000000, 0.9659258262890683122, 1.000000000000000000, 0.9659258262890683122, 1.000000000000000000, 0.9659258262890683122, 1.000000000000000000, 0.9659258262890683122, 1.000000000000000000, 0.9659258262890683122, 1.000000000000000000, 0.9659258262890683122, 1.000000000000000000, 0.9659258262890683122, 1.000000000000000000, 0.9659258262890683122, 1.000000000000000000, 0.9659258262890683122, 1.000000000000000000, 0.9659258262890683122, 1.000000000000000000, 0.9659258262890683122, 1.000000000000000000, 0.9659258262890683122, 1.000000000000000000, 0.9659258262890683122, 1.000000000000000000),
 ( 1.000000000000000000, 0.9659258262890683122, 1.000000000000000000, 0.9659258262890683122, 1.000000000000000000, 0.9659258262890683122, 1.000000000000000000, 0.9659258262890683122, 1.000000000000000000, 0.9659258262890683122, 1.000000000000000000, 0.9659258262890683122, 1.000000000000000000, 0.9659258262890683122, 1.000000000000000000, 0.9659258262890683122, 1.000000000000000000, 0.9659258262890683122, 1.000000000000000000, 0.9659258262890683122, 1.000000000000000000, 0.9659258262890683122, 1.000000000000000000, 0.9659258262890683122, 1.000000000000000000, 0.9659258262890683122, 1.000000000000000000, 0.9659258262890683122, 1.000000000000000000, 0.9659258262890683122, 1.000000000000000000, 0.9659258262890683122, 1.000000000000000000, 0.9659258262890683122, 1.000000000000000000, 0.9659258262890683122, 1.000000000000000000, 0.9659258262890683122, 1.000000000000000000, 0.9659258262890683122, 1.000000000000000000, 0.9659258262890683122, 1.000000000000000000, 0.9659258262890683122, 1.000000000000000000, 0.9659258262890683122, 1.000000000000000000, 0.9659258262890683122, 1.000000000000000000, 0.9659258262890683122, 1.000000000000000000, 0.9659258262890683122, 1.000000000000000000, 0.9659258262890683122, 1.000000000000000000, 0.9659258262890683122, 1.000000000000000000, 0.9659258262890683122, 1.000000000000000000, 0.9659258262890683122, 1.000000000000000000, 0.9659258262890683122, 1.000000000000000000, 0.9659258262890683122, 1.000000000000000000, 0.9659258262890683122, 1.000000000000000000, 0.9659258262890683122, 1.000000000000000000, 0.9659258262890683122, 1.000000000000000000, 0.9659258262890683122, 1.000000000000000000, 0.9659258262890683122, 1.000000000000000000, 0.9659258262890683122, 1.000000000000000000, 0.9659258262890683122, 1.000000000000000000, 0.9659258262890683122, 1.000000000000000000, 0.9659258262890683122, 1.000000000000000000, 0.9659258262890683122, 1.000000000000000000, 0.9659258262890683122, 1.000000000000000000, 0.9659258262890683122, 1.000000000000000000, 0.9659258262890683122, 1.000000000000000000, 0.9659258262890683122, 1.000000000000000000, 0.9659258262890683122, 1.000000000000000000, 0.9659258262890683122, 1.000000000000000000, 0.9659258262890683122, 1.000000000000000000, 0.9659258262890683122, 1.000000000000000000, 0.9659258262890683122, 1.000000000000000000, 0.9659258262890683122, 1.000000000000000000, 0.9659258262890683122, 1.000000000000000000, 0.9659258262890683122, 1.000000000000000000, 0.9659258262890683122, 1.000000000000000000, 0.9659258262890683122, 1.000000000000000000, 0.9659258262890683122, 1.000000000000000000, 0.9659258262890683122, 1.000000000000000000, 0.9659258262890683122, 1.000000000000000000, 0.9659258262890683122, 1.000000000000000000, 0.9659258262890683122, 1.000000000000000000, 0.9659258262890683122, 1.000000000000000000, 0.9659258262890683122, 1.000000000000000000, 0.9659258262890683122, 1.000000000000000000, 0.9659258262890683122, 1.000000000000000000, 0.9659258262890683122, 1.000000000000000000, 0.9659258262890683122, 1.000000000000000000, 0.9659258262890683122, 1.000000000000000000, 0.9659258262890683122, 1.000000000000000000, 0.9659258262890683122, 1.000000000000000000, 0.9659258262890683122, 1.000000000000000000, 0.9659258262890683122, 1.000000000000000000, 0.9659258262890683122, 1.000000000000000000, 0.9659258262890683122, 1.000000000000000000, 0.9659258262890683122, 1.000000000000000000, 0.9659258262890683122, 1.000000000000000000, 0.9659258262890683122, 1.000000000000000000, 0.9659258262890683122, 1.000000000000000000, 0.9659258262890683122, 1.000000000000000000, 0.9659258262890683122, 1.000000000000000000, 0.9659258262890683122, 1.000000000000000000, 0.9659258262890683122, 1.000000000000000000, 0.9659258262890683122, 1.000000000000000000, 0.9659258262890683122, 1.000000000000000000, 0.9659258262890683122, 1.000000000000000000, 0.9659258262890683122, 1.000000000000000000, 0.9659258262890683122, 1.000000000000000000, 0.9659258262890683122, 1.000000000000000000, 0.9659258262890683122, 1.000000000000000000, 0.9659258262890683122, 1.000000000000000000, 0.9659258262890683122, 1.000000000000000000, 0.9659258262890683122, 1.000000000000000000, 0.9659258262890683122, 1.000000000000000000, 0.9659258262890683122, 1.000000000000000000, 0.9659258262890683122, 1.000000000000000000, 0.9659258262890683122, 1.000000000000000000, 0.9659258262890683122, 1.000000000000000000, 0.9659258262890683122, 1.000000000000000000, 0.9659258262890683122, 1.000000000000000000, 0.9659258262890683122, 1.000000000000000000, 0.9659258262890683122, 1.000000000000000000, 0.9659258262890683122, 1.000000000000000000, 0.9659258262890683122, 1.000000000000000000, 0.9659258262890683122, 1.000000000000000000, 0.9659258262890683122, 1.000000000000000000, 0.9659258262890683122, 1.000000000000000000, 0.9659258262890683122, 1.000000000000000000, 0.9659258262890683122, 1.000000000000000000, 0.9659258262890683122, 1.000000000000000000, 0.9659258262890683122, 1.000000000000000000, 0.9659258262890683122, 1.000000000000000000, 0.9659258262890683122, 1.000000000000000000, 0.9659258262890683122, 1.000000000000000000, 0.9659258262890683122, 1.000000000000000000, 0.9659258262890683122, 1.000000000000000000, 0.9659258262890683122, 1.000000000000000000, 0.9659258262890683122, 1.000000000000000000, 0.9659258262890683122, 1.000000000000000000, 0.9659258262890683122, 1.000000000000000000, 0.9659258262890683122, 1.000000000000000000, 0.9659258262890683122, 1.000000000000000000, 0.9659258262890683122, 1.000000000000000000, 0.9659258262890683122, 1.000000000000000000, 0.9659258262890683122, 1.000000000000000000, 0.9659258262890683122, 1.000000000000000000, 0.9659258262890683122, 1.000000000000000000, 0.9659258262890683122, 1.000000000000000000, 0.9659258262890683122, 1.000000000000000000, 0.9659258262890683122, 1.000000000000000000, 0.9659258262890683122, 1.000000000000000000, 0.9659258262890683122, 1.000000000000000000, 0.9659258262890683122, 1.000000000000000000, 0.9659258262890683122, 1.000000000000000000, 0.9659258262890683122, 1.000000000000000000, 0.9659258262890683122, 1.000000000000000000, 0.9659258262890683122, 1.000000000000000000, 0.9659258262890683122, 1.000000000000000000, 0.9659258262890683122, 1.000000000000000000, 0.9659258262890683122, 1.000000000000000000, 0.9659258262890683122, 1.000000000000000000, 0.9659258262890683122, 1.000000000000000000, 0.9659258262890683122, 1.000000000000000000, 0.9659258262890683122, 1.000000000000000000, 0.9659258262890683122, 1.000000000000000000, 0.9659258262890683122, 1.000000000000000000, 0.9659258262890683122, 1.000000000000000000, 0.9659258262890683122, 1.000000000000000000, 0.9659258262890683122, 1.000000000000000000, 0.9659258262890683122, 1.000000000000000000, 0.9659258262890683122, 1.000000000000000000, 0.9659258262890683122, 1.000000000000000000, 0.9659258262890683122, 1.000000000000000000, 0.9659258262890683122, 1.000000000000000000, 0.9659258262890683122, 1.000000000000000000, 0.9659258262890683122, 1.000000000000000000, 0.9659258262890683122, 1.000000000000000000, 0.9659258262890683122, 1.000000000000000000, 0.9659258262890683122, 1.000000000000000000, 0.9659258262890683122, 1.000000000000000000, 0.9659258262890683122, 1.000000000000000000, 0.9659258262890683122, 1.000000000000000000, 0.9659258262890683122, 1.000000000000000000) ) ) 
 REPRESENTATION_ITEM ( '' )  SURFACE ( )  );
#14550 =( GEOMETRIC_REPRESENTATION_CONTEXT ( 3 ) GLOBAL_UNCERTAINTY_ASSIGNED_CONTEXT ( ( #93339 ) ) GLOBAL_UNIT_ASSIGNED_CONTEXT ( ( #54088, #14138, #71079 ) ) REPRESENTATION_CONTEXT ( 'NONE', 'WORKASPACE' ) );
#14551 = ORIENTED_EDGE ( 'NONE', *, *, #79762, .T. ) ;
#14552 = CARTESIAN_POINT ( 'NONE',  ( -4.164238869374099039, 66.80374883491396076, 8.674139862899312516E-16 ) ) ;
#14553 = CARTESIAN_POINT ( 'NONE',  ( -2.266590686148945544, 62.22041550158063927, 7.082119434687048631 ) ) ;
#14554 = CARTESIAN_POINT ( 'NONE',  ( 0.1532563361054082862, 36.21726448433410894, 2.638427012816831674 ) ) ;
#14555 = CARTESIAN_POINT ( 'NONE',  ( 6.565887622018943937, 45.16530133659708923, 12.81628187352647430 ) ) ;
#14556 = CARTESIAN_POINT ( 'NONE',  ( 0.000000000000000000, 12.49999999999999112, 0.000000000000000000 ) ) ;
#14557 = CARTESIAN_POINT ( 'NONE',  ( 17.08211943468705840, 10.13708216824730179, -12.26659068614894466 ) ) ;
#14558 = CARTESIAN_POINT ( 'NONE',  ( 7.084665262690076126, 9.105352010821503583, 10.88017736071109987 ) ) ;
#14559 = CARTESIAN_POINT ( 'NONE',  ( 22.26659068614894466, 53.88708216824731068, 7.082119434687054849 ) ) ;
#14560 = CARTESIAN_POINT ( 'NONE',  ( 2.791683348922240793, 46.63393115100077324, 7.208316651077764092 ) ) ;
#14561 = FACE_OUTER_BOUND ( 'NONE', #11692, .T. ) ;
#14562 = CARTESIAN_POINT ( 'NONE',  ( 17.20831665107776587, 22.88393115100078745, 7.208316651077764980 ) ) ;
#14563 = AXIS2_PLACEMENT_3D ( 'NONE', #23877, #16361, #24366 ) ;
#14564 = AXIS2_PLACEMENT_3D ( 'NONE', #2411, #55884, #2902 ) ;
#14565 = FACE_OUTER_BOUND ( 'NONE', #74792, .T. ) ;
#14566 = CARTESIAN_POINT ( 'NONE',  ( 4.923371831947301658, 17.67559781766744820, 8.527530157486175710 ) ) ;
#14567 = VERTEX_POINT ( 'NONE', #17748 ) ;
#14568 = ORIENTED_EDGE ( 'NONE', *, *, #67459, .F. ) ;
#14569 = CARTESIAN_POINT ( 'NONE',  ( -10.98829462902744858, 46.98606209026556968, 0.000000000000000000 ) ) ;
#14570 = EDGE_LOOP ( 'NONE', ( #73425, #27850, #11071, #70629 ) ) ;
#14571 = CARTESIAN_POINT ( 'NONE',  ( 2.791683348922237240, 50.38393115100078035, -7.208316651077763204 ) ) ;
#14572 = CARTESIAN_POINT ( 'NONE',  ( 20.36894250292379382, 18.67874883491397142, 10.36894250292379205 ) ) ;
#14574 = CARTESIAN_POINT ( 'NONE',  ( 2.035157376598822676, 37.43868534415484106, -7.964842623401177768 ) ) ;
#14573 = CARTESIAN_POINT ( 'NONE',  ( 10.00000000000000178, 39.31368534415484106, 10.88017736071110342 ) ) ;
#14576 = CARTESIAN_POINT ( 'NONE',  ( 3.591859063236763294, 33.29030133659708213, -11.09922568453595026 ) ) ;
#14575 = CARTESIAN_POINT ( 'NONE',  ( 7.361572987183169658, 59.96726448433410894, -9.846743663894592657 ) ) ;
#14577 = CARTESIAN_POINT ( 'NONE',  ( -0.3689425029237881626, 2.428748834913967869, 10.36894250292379027 ) ) ;
#14578 = ADVANCED_FACE ( 'NONE', ( #48226 ), #77739, .T. ) ;
#14579 = CARTESIAN_POINT ( 'NONE',  ( 6.565887622018943937, 28.08196800326375353, -12.81628187352647608 ) ) ;
#14580 = ORIENTED_EDGE ( 'NONE', *, *, #37493, .T. ) ;
#14581 = CARTESIAN_POINT ( 'NONE',  ( 19.84674366389459266, 38.71726448433412315, -2.638427012816827677 ) ) ;
#14582 = CARTESIAN_POINT ( 'NONE',  ( 2.035157376598822676, 12.43868534415483751, -7.964842623401177768 ) ) ;
#14583 = VERTEX_POINT ( 'NONE', #79218 ) ;
#14584 = CARTESIAN_POINT ( 'NONE',  ( 10.00000000000000000, 16.81368534415483751, -10.88017736071110342 ) ) ;
#14585 = VERTEX_POINT ( 'NONE', #10730 ) ;
#14586 = CARTESIAN_POINT ( 'NONE',  ( 20.88017736071110875, 65.77201867748817676, -2.915334737309920765 ) ) ;
#14587 = CARTESIAN_POINT ( 'NONE',  ( 20.88017736071110164, 55.35535201082149825, 2.915334737309930979 ) ) ;
#14588 = CARTESIAN_POINT ( 'NONE',  ( 20.88017736071110519, 65.56368534415483396, 2.639326808657452039E-16 ) ) ;
#14589 = EDGE_CURVE ( 'NONE', #88856, #5496, #77248, .T. ) ;
#14590 = CARTESIAN_POINT ( 'NONE',  ( 4.559911319644449179, 53.89701867748817676, 9.422509992056141925 ) ) ;
#14591 = VECTOR ( 'NONE', #60843, 1000.000000000000114 ) ;
#14592 = AXIS2_PLACEMENT_3D ( 'NONE', #69454, #84462, #6988 ) ;
#14593 = CARTESIAN_POINT ( 'NONE',  ( -0.2418659066527493184, 30.11633188102328162, 6.114288769123083611 ) ) ;
#14594 = LINE ( 'NONE', #83074, #20032 ) ;
#14595 = B_SPLINE_CURVE_WITH_KNOTS ( 'NONE', 3,
 ( #98507, #83961, #45970, #77428, #8940, #4 ),
 .UNSPECIFIED., .F., .F.,
 ( 4, 2, 4 ),
 ( 0.0002800421825936745958, 0.0006862478247299499869, 0.001092453466866225541 ),
 .UNSPECIFIED. ) ;
#14597 = EDGE_LOOP ( 'NONE', ( #56864, #26283, #47747, #47972 ) ) ;
#14596 =( NAMED_UNIT ( * ) SI_UNIT ( $, .STERADIAN. ) SOLID_ANGLE_UNIT ( ) );
#14598 = EDGE_CURVE ( 'NONE', #18488, #66580, #1775, .T. ) ;
#14599 = AXIS2_PLACEMENT_3D ( 'NONE', #51506, #74494, #22503 ) ;
#14600 = CARTESIAN_POINT ( 'NONE',  ( 12.63842701281683922, 44.55059781766745175, -9.846743663894590881 ) ) ;
#14601 = ORIENTED_EDGE ( 'NONE', *, *, #54627, .T. ) ;
#14602 = DIRECTION ( 'NONE',  ( 0.000000000000000000, 0.000000000000000000, 1.000000000000000000 ) ) ;
#14603 = B_SPLINE_CURVE_WITH_KNOTS ( 'NONE', 3,
 ( #30729, #14276, #13269, #90744, #67265, #45753 ),
 .UNSPECIFIED., .F., .F.,
 ( 4, 2, 4 ),
 ( 3.409110551496050731E-05, 0.0004400426677367859753, 0.0008459942299586113755 ),
 .UNSPECIFIED. ) ;
#14605 = EDGE_CURVE ( 'NONE', #2203, #54884, #38776, .T. ) ;
#14604 = LINE ( 'NONE', #38573, #62141 ) ;
#14606 = CARTESIAN_POINT ( 'NONE',  ( -0.3689425029237898834, 6.178748834913968757, -10.36894250292378850 ) ) ;
#14607 = ORIENTED_EDGE ( 'NONE', *, *, #78016, .T. ) ;
#14608 = CARTESIAN_POINT ( 'NONE',  ( -1.926860441876564023, 7.870456701841140656, 3.195792623639529761 ) ) ;
#14609 = CARTESIAN_POINT ( 'NONE',  ( -46.94000000000003325, 103.1207406662227157, -5.953111867825573000 ) ) ;
#14610 = CARTESIAN_POINT ( 'NONE',  ( 2.035157376598822676, 2.438685344154838397, -7.964842623401177768 ) ) ;
#14611 = DIRECTION ( 'NONE',  ( -0.000000000000000000, 0.000000000000000000, -1.000000000000000000 ) ) ;
#14613 = EDGE_LOOP ( 'NONE', ( #38153, #53182, #97519, #57704, #48297, #3714 ) ) ;
#14612 = CARTESIAN_POINT ( 'NONE',  ( -2.816281873526471635, 38.91530133659708213, -3.434112377981056508 ) ) ;
#14614 = CARTESIAN_POINT ( 'NONE',  ( 34.56412365047464874, 11.99999999999999645, -9.500000000000000000 ) ) ;
#14615 = CARTESIAN_POINT ( 'NONE',  ( 1.472469842513823179, 45.59226448433412315, -4.923371831947296329 ) ) ;
#14616 = PRESENTATION_LAYER_ASSIGNMENT (  '', '', ( #95972 ) ) ;
#14617 = CARTESIAN_POINT ( 'NONE',  ( 17.39651004071890128, 29.08210964143323096, -6.499999999999448441 ) ) ;
#14618 = CARTESIAN_POINT ( 'NONE',  ( 6.565887622018943937, 25.16530133659708213, 12.81628187352647430 ) ) ;
#14619 = CARTESIAN_POINT ( 'NONE',  ( 1.472469842513823179, 21.42559781766745175, 4.923371831947296329 ) ) ;
#14620 = DIRECTION ( 'NONE',  ( 0.000000000000000000, 1.000000000000000000, 0.000000000000000000 ) ) ;
#14621 = CARTESIAN_POINT ( 'NONE',  ( 6.565887622018943937, 3.081968003263753531, -12.81628187352647608 ) ) ;
#14622 = DIRECTION ( 'NONE',  ( -0.000000000000000000, -1.000000000000000000, -0.000000000000000000 ) ) ;
#14623 = VECTOR ( 'NONE', #83009, 1000.000000000000227 ) ;
#14624 = ORIENTED_EDGE ( 'NONE', *, *, #29685, .F. ) ;
#14625 = ORIENTED_EDGE ( 'NONE', *, *, #91225, .F. ) ;
#14626 = CARTESIAN_POINT ( 'NONE',  ( -0.8801773607111009756, 23.06368534415484106, 1.068504757029289695E-15 ) ) ;
#14627 = CARTESIAN_POINT ( 'NONE',  ( 24.16423886937410614, 19.51208216824729647, -3.795296366450302550 ) ) ;
#14628 = CARTESIAN_POINT ( 'NONE',  ( 0.1532563361054082862, 26.21726448433411605, 2.638427012816831674 ) ) ;
#14629 = CARTESIAN_POINT ( 'NONE',  ( 7.084665262690076126, 62.02201867748816966, -10.88017736071110164 ) ) ;
#14631 = CARTESIAN_POINT ( 'NONE',  ( -4.247994584727555534, -13.56436116443237516, -3.750000000000000000 ) ) ;
#14630 = CARTESIAN_POINT ( 'NONE',  ( 21.09922568453595559, 37.04030133659708923, -6.408140936763230044 ) ) ;
#14632 = CARTESIAN_POINT ( 'NONE',  ( 15.44008868035555793, 11.39701867748817143, -9.422509992056140149 ) ) ;
#14633 = EDGE_CURVE ( 'NONE', #97319, #89788, #73180, .T. ) ;
#14634 = CARTESIAN_POINT ( 'NONE',  ( 0.2751277870542914172, 43.21833443783938122, 6.499999999999992006 ) ) ;
#14635 = CARTESIAN_POINT ( 'NONE',  ( -1.099225684535947600, 14.54030133659708568, 6.408140936763237150 ) ) ;
#14636 = CARTESIAN_POINT ( 'NONE',  ( 19.38216949554541557, 12.24863466993041961, -9.382169495545420901 ) ) ;
#14637 = CARTESIAN_POINT ( 'NONE',  ( 2.791683348922240793, 21.63393115100078745, 7.208316651077764092 ) ) ;
#14638 = CARTESIAN_POINT ( 'NONE',  ( 9.422509992056141925, -14.01964798917848576, -5.440088680355554374 ) ) ;
#14639 = CARTESIAN_POINT ( 'NONE',  ( 6.565887622018943937, 38.08196800326376064, -12.81628187352647608 ) ) ;
#14640 = CARTESIAN_POINT ( 'NONE',  ( 3.927832320392247389, -0.03417435944610275333, -13.69797916712104602 ) ) ;
#14641 = PRESENTATION_LAYER_ASSIGNMENT (  '', '', ( #51304 ) ) ;
#14643 = CARTESIAN_POINT ( 'NONE',  ( 0.7375392941518293943, 14.49999999999999822, -14.98185688723470932 ) ) ;
#14642 = CARTESIAN_POINT ( 'NONE',  ( 10.00000000000000000, 36.81368534415484106, -10.88017736071110342 ) ) ;
#14644 = LINE ( 'NONE', #37138, #52990 ) ;
#14645 = CARTESIAN_POINT ( 'NONE',  ( -0.1552420861355162940, 14.99999999999805489, 14.62478754979945705 ) ) ;
#14646 = CARTESIAN_POINT ( 'NONE',  ( 15.44008868035555260, 34.73035201082151247, 9.422509992056143702 ) ) ;
#14647 = CARTESIAN_POINT ( 'NONE',  ( 10.00000000000000178, 44.31368534415484106, 10.88017736071110342 ) ) ;
#14648 = CARTESIAN_POINT ( 'NONE',  ( 5.076628168052704559, 65.17559781766745175, -8.527530157486179263 ) ) ;
#14649 = CARTESIAN_POINT ( 'NONE',  ( 12.91533473730993009, 66.60535201082150536, -10.88017736071109987 ) ) ;
#14650 = CARTESIAN_POINT ( 'NONE',  ( 10.00000000000000000, 39.75893115100078745, -9.846743663894594434 ) ) ;
#14651 = CARTESIAN_POINT ( 'NONE',  ( 10.00000000000000178, 4.313685344154837509, 10.88017736071110342 ) ) ;
#14652 = CARTESIAN_POINT ( 'NONE',  ( 3.591859063236763294, 18.29030133659708568, -11.09922568453595026 ) ) ;
#14653 = EDGE_LOOP ( 'NONE', ( #75162, #40145, #96122, #13591 ) ) ;
#14654 = CARTESIAN_POINT ( 'NONE',  ( 12.91533473730993009, 21.60535201082150536, -10.88017736071109987 ) ) ;
#14655 = CARTESIAN_POINT ( 'NONE',  ( 0.000000000000000000, 15.00000000000000000, 0.000000000000000000 ) ) ;
#14656 = CARTESIAN_POINT ( 'NONE',  ( 15.44008868035555793, 21.39701867748817321, -9.422509992056140149 ) ) ;
#14657 = CARTESIAN_POINT ( 'NONE',  ( 0.1532563361054100626, 0.8005978176674514168, -2.638427012816831230 ) ) ;
#14658 = CARTESIAN_POINT ( 'NONE',  ( -4.164238869374099039, 36.80374883491396787, 8.674139862899312516E-16 ) ) ;
#14659 = CARTESIAN_POINT ( 'NONE',  ( 12.63842701281683922, 24.55059781766745175, -9.846743663894590881 ) ) ;
#14660 = CARTESIAN_POINT ( 'NONE',  ( 17.96484262340118221, 41.18868534415484106, -7.964842623401177768 ) ) ;
#14661 = DIRECTION ( 'NONE',  ( 1.000000000000000000, 0.000000000000000000, 0.000000000000000000 ) ) ;
#14662 = CARTESIAN_POINT ( 'NONE',  ( -2.266590686148945544, 6.387082168247300906, -7.082119434687050408 ) ) ;
#14663 = CIRCLE ( 'NONE', #1897, 15.00000000000000000 ) ;
#14664 = ORIENTED_EDGE ( 'NONE', *, *, #79282, .F. ) ;
#14665 = LINE ( 'NONE', #28654, #84859 ) ;
#14666 = CARTESIAN_POINT ( 'NONE',  ( 19.84674366389459266, 53.30059781766744464, 2.638427012816836559 ) ) ;
#14667 = VERTEX_POINT ( 'NONE', #19700 ) ;
#14668 = EDGE_LOOP ( 'NONE', ( #68747, #73289, #52542, #40626 ) ) ;
#14669 = AXIS2_PLACEMENT_3D ( 'NONE', #20292, #81281, #73773 ) ;
#14670 = CARTESIAN_POINT ( 'NONE',  ( 22.26659068614894466, 23.88708216824730357, 7.082119434687054849 ) ) ;
#14671 = CARTESIAN_POINT ( 'NONE',  ( 22.26659068614894466, 18.88708216824730002, 7.082119434687054849 ) ) ;
#14672 = CARTESIAN_POINT ( 'NONE',  ( 2.035157376598822676, 57.43868534415484106, -7.964842623401177768 ) ) ;
#14673 = CARTESIAN_POINT ( 'NONE',  ( 13.79529636645030344, 63.26208216824730357, 14.16423886937410614 ) ) ;
#14674 = CARTESIAN_POINT ( 'NONE',  ( 19.84674366389459266, 48.71726448433413026, -2.638427012816827677 ) ) ;
#14675 = CARTESIAN_POINT ( 'NONE',  ( -11.37541478881037271, -75.76447409171241532, 4.000000000000000000 ) ) ;
#14677 = CARTESIAN_POINT ( 'NONE',  ( 16.40814093676323893, 25.79030133659708923, 11.09922568453595026 ) ) ;
#14676 = CARTESIAN_POINT ( 'NONE',  ( 20.88017736071110164, 45.35535201082149115, 2.915334737309930979 ) ) ;
#14678 = CARTESIAN_POINT ( 'NONE',  ( -4.164238869374099927, 17.01208216824730357, 3.795296366450308767 ) ) ;
#14679 = CARTESIAN_POINT ( 'NONE',  ( 19.42250999205614548, 15.98035201082150714, -5.440088680355545492 ) ) ;
#14680 = CARTESIAN_POINT ( 'NONE',  ( 4.559911319644449179, 17.23035201082150536, -9.422509992056141925 ) ) ;
#14681 = CARTESIAN_POINT ( 'NONE',  ( 10.00000000000000000, 61.81368534415484106, -10.88017736071110342 ) ) ;
#14682 = CARTESIAN_POINT ( 'NONE',  ( -2.816281873526473856, 49.12363466993042493, 9.499525473075851096E-16 ) ) ;
#14683 = CARTESIAN_POINT ( 'NONE',  ( -9.846743663894596210, -19.19940218233254114, -2.638427012816824124 ) ) ;
#14684 = ORIENTED_EDGE ( 'NONE', *, *, #92676, .F. ) ;
#14685 = LINE ( 'NONE', #82165, #41161 ) ;
#14686 = ORIENTED_EDGE ( 'NONE', *, *, #41019, .F. ) ;
#14687 = CARTESIAN_POINT ( 'NONE',  ( -1.926860441876562247, 12.45379003517447458, -3.195792623639530650 ) ) ;
#14688 = DIRECTION ( 'NONE',  ( 0.000000000000000000, 0.000000000000000000, 1.000000000000000000 ) ) ;
#14689 = EDGE_LOOP ( 'NONE', ( #80068, #97209, #57071, #73354 ) ) ;
#14690 = DIRECTION ( 'NONE',  ( 0.000000000000000000, 1.000000000000000000, 0.000000000000000000 ) ) ;
#14692 = CARTESIAN_POINT ( 'NONE',  ( 19.42250999205614193, 5.147018677488171434, 5.440088680355555262 ) ) ;
#14691 = CARTESIAN_POINT ( 'NONE',  ( 20.36894250292379382, 53.67874883491397497, 10.36894250292379205 ) ) ;
#14694 = CARTESIAN_POINT ( 'NONE',  ( 0.1532563361054082862, 51.21726448433412315, 2.638427012816831674 ) ) ;
#14693 = CARTESIAN_POINT ( 'NONE',  ( 12.63842701281683034, 22.46726448433411605, 9.846743663894596210 ) ) ;
#14695 = CARTESIAN_POINT ( 'NONE',  ( 2.035157376598824452, 68.68868534415484817, 7.964842623401179544 ) ) ;
#14696 = EDGE_CURVE ( 'NONE', #7648, #43985, #58914, .T. ) ;
#14697 = MECHANICAL_DESIGN_GEOMETRIC_PRESENTATION_REPRESENTATION (  '', ( #59333 ), #21030 ) ;
#14698 = CARTESIAN_POINT ( 'NONE',  ( 12.91533473730992121, 64.52201867748817676, 10.88017736071110164 ) ) ;
#14699 = CARTESIAN_POINT ( 'NONE',  ( 3.434112377981054287, 17.66530133659708568, -12.81628187352647608 ) ) ;
#14700 = EDGE_LOOP ( 'NONE', ( #54950, #27703, #14201, #20436 ) ) ;
#14701 = CARTESIAN_POINT ( 'NONE',  ( -4.164238869374098151, 31.59541550158063927, -3.795296366450310543 ) ) ;
#14702 = CARTESIAN_POINT ( 'NONE',  ( 24.16423886937410614, 39.51208216824731068, -3.795296366450302550 ) ) ;
#14703 = ORIENTED_EDGE ( 'NONE', *, *, #55004, .F. ) ;
#14704 = CARTESIAN_POINT ( 'NONE',  ( 3.591859063236763294, 53.29030133659708923, -11.09922568453595026 ) ) ;
#14705 = CARTESIAN_POINT ( 'NONE',  ( 1.472469842513823179, 41.42559781766745886, 4.923371831947296329 ) ) ;
#14706 = CARTESIAN_POINT ( 'NONE',  ( 4.559911319644449179, 23.89701867748817321, 9.422509992056141925 ) ) ;
#14707 = CIRCLE ( 'NONE', #89694, 0.2500000000000002220 ) ;
#14708 = CARTESIAN_POINT ( 'NONE',  ( 0.6178305044545838731, 64.74863466993043914, 9.382169495545420901 ) ) ;
#14709 = DIRECTION ( 'NONE',  ( 0.9935718556765863463, 0.000000000000000000, 0.1132032137679171435 ) ) ;
#14710 = CARTESIAN_POINT ( 'NONE',  ( 0.1532563361054082862, 51.21726448433412315, 2.638427012816831674 ) ) ;
#14711 = CARTESIAN_POINT ( 'NONE',  ( 2.791683348922237240, 45.38393115100079456, -7.208316651077763204 ) ) ;
#14713 = ORIENTED_EDGE ( 'NONE', *, *, #31526, .T. ) ;
#14712 = CARTESIAN_POINT ( 'NONE',  ( 3.969999999999999751, 10.25000000000000000, 2.750000000000000000 ) ) ;
#14714 = EDGE_CURVE ( 'NONE', #31231, #43572, #80197, .T. ) ;
#14715 = CARTESIAN_POINT ( 'NONE',  ( -3.115783986955657614, 15.00000000000000000, 14.16128137375395468 ) ) ;
#14716 = LINE ( 'NONE', #45191, #64177 ) ;
#14717 = CARTESIAN_POINT ( 'NONE',  ( 3.640395162852214650, 89.00000000000000000, -5.000000000000000000 ) ) ;
#14718 = EDGE_LOOP ( 'NONE', ( #12, #40130, #88494, #24667 ) ) ;
#14719 = PRODUCT_DEFINITION_SHAPE ( 'NONE', 'NONE',  #32419 ) ;
#14720 = CARTESIAN_POINT ( 'NONE',  ( 0.6076426042653030324, 57.37576471608601025, -6.499999999999985789 ) ) ;
#14721 = CARTESIAN_POINT ( 'NONE',  ( 17.20831665107776587, 32.88393115100078745, 7.208316651077764980 ) ) ;
#14723 = ADVANCED_FACE ( 'NONE', ( #56716 ), #17167, .F. ) ;
#14722 = DIRECTION ( 'NONE',  ( -0.000000000000000000, -0.000000000000000000, -1.000000000000000000 ) ) ;
#14724 = VERTEX_POINT ( 'NONE', #15272 ) ;
#14725 = CARTESIAN_POINT ( 'NONE',  ( 10.00000000000000000, 54.75893115100078745, -9.846743663894594434 ) ) ;
#14726 = DIRECTION ( 'NONE',  ( 4.440892098500626162E-15, 0.000000000000000000, 1.000000000000000000 ) ) ;
#14727 = CARTESIAN_POINT ( 'NONE',  ( 18.52753015748617571, 43.09226448433412315, 4.923371831947298993 ) ) ;
#14728 = CARTESIAN_POINT ( 'NONE',  ( 10.00000000000000000, 30.55374883491397142, -14.16423886937410082 ) ) ;
#14729 = CARTESIAN_POINT ( 'NONE',  ( 19.84674366389459266, 48.30059781766745175, 2.638427012816836559 ) ) ;
#14730 = CARTESIAN_POINT ( 'NONE',  ( 7.313705784284593392, 0.5000000000000004441, -13.09617149020743732 ) ) ;
#14731 = CARTESIAN_POINT ( 'NONE',  ( -6.689969769699040114, -0.03417435944610275333, 12.58200319823965785 ) ) ;
#14732 = CARTESIAN_POINT ( 'NONE',  ( 0.1532563361054100626, 5.800597817667452638, -2.638427012816831230 ) ) ;
#14733 = CARTESIAN_POINT ( 'NONE',  ( 6.204703633549690345, 5.762082168247301794, -14.16423886937410259 ) ) ;
#14734 = CARTESIAN_POINT ( 'NONE',  ( 19.84674366389459266, 43.30059781766744464, 2.638427012816836559 ) ) ;
#14735 = CARTESIAN_POINT ( 'NONE',  ( 7.084665262690076126, 42.02201867748816966, -10.88017736071110164 ) ) ;
#14736 = CARTESIAN_POINT ( 'NONE',  ( 1.472469842513823179, 40.59226448433411605, -4.923371831947296329 ) ) ;
#14737 = CARTESIAN_POINT ( 'NONE',  ( 3.969999999999999751, 36.75000000000000000, -3.750000000000000000 ) ) ;
#14738 = AXIS2_PLACEMENT_3D ( 'NONE', #38052, #1041, #76525 ) ;
#14739 = B_SPLINE_CURVE_WITH_KNOTS ( 'NONE', 3,
 ( #55337, #84381, #23881, #38875, #30862, #1873 ),
 .UNSPECIFIED., .F., .F.,
 ( 4, 2, 4 ),
 ( 0.0002800808511812530191, 0.0006862868719358964590, 0.001092492892690540007 ),
 .UNSPECIFIED. ) ;
#14740 = CARTESIAN_POINT ( 'NONE',  ( 15.44008868035555793, 51.39701867748816966, -9.422509992056140149 ) ) ;
#14741 = EDGE_CURVE ( 'NONE', #29043, #15233, #22928, .T. ) ;
#14742 = ORIENTED_EDGE ( 'NONE', *, *, #42281, .F. ) ;
#14743 = DIRECTION ( 'NONE',  ( -1.000000000000000000, -1.927470528863119542E-16, 0.000000000000000000 ) ) ;
#14744 = CARTESIAN_POINT ( 'NONE',  ( -0.8801773607111008646, 13.27201867748817143, 2.915334737309923430 ) ) ;
#14746 = CARTESIAN_POINT ( 'NONE',  ( 2.035157376598822676, 42.43868534415483396, -7.964842623401177768 ) ) ;
#14745 = CARTESIAN_POINT ( 'NONE',  ( 22.81628187352648496, 1.831968003263753753, -3.434112377981050290 ) ) ;
#14747 = DIRECTION ( 'NONE',  ( -0.000000000000000000, -1.000000000000000000, -0.000000000000000000 ) ) ;
#14748 = CARTESIAN_POINT ( 'NONE',  ( 18.04007052943773104, 13.01528370094808196, 5.767676674365834977 ) ) ;
#14749 = B_SPLINE_CURVE_WITH_KNOTS ( 'NONE', 3,
 ( #18372, #79847, #11842, #64825, #25395, #71858 ),
 .UNSPECIFIED., .F., .F.,
 ( 4, 2, 4 ),
 ( 0.0002800206007755498788, 0.0006862260317144059079, 0.001092431462653262100 ),
 .UNSPECIFIED. ) ;
#14751 = DIRECTION ( 'NONE',  ( -0.000000000000000000, -0.000000000000000000, 1.000000000000000000 ) ) ;
#14750 = CARTESIAN_POINT ( 'NONE',  ( 17.96484262340118221, 44.93868534415483396, 7.964842623401181321 ) ) ;
#14752 = CARTESIAN_POINT ( 'NONE',  ( 2.791683348922240793, 16.63393115100078745, 7.208316651077764092 ) ) ;
#14753 = CARTESIAN_POINT ( 'NONE',  ( 1.472469842513823179, 36.42559781766745175, 4.923371831947296329 ) ) ;
#14754 = CARTESIAN_POINT ( 'NONE',  ( 3.795296366450306547, 15.34541550158064460, -14.16423886937410259 ) ) ;
#14755 = CARTESIAN_POINT ( 'NONE',  ( 0.1532563361054082862, 66.21726448433413736, 2.638427012816831674 ) ) ;
#14756 = B_SPLINE_CURVE_WITH_KNOTS ( 'NONE', 3,
 ( #97760, #29716, #98258, #53705, #75222, #8698 ),
 .UNSPECIFIED., .F., .F.,
 ( 4, 2, 4 ),
 ( 0.0002800912045164338977, 0.0006862973266905296552, 0.001092503448864625250 ),
 .UNSPECIFIED. ) ;
#14757 = CARTESIAN_POINT ( 'NONE',  ( 15.44008868035555260, 4.730352010821505360, 9.422509992056143702 ) ) ;
#14758 = CARTESIAN_POINT ( 'NONE',  ( 3.115783986955557694, 15.00000000000000000, -14.16128137375397955 ) ) ;
#14759 = CARTESIAN_POINT ( 'NONE',  ( 17.08211943468705130, 23.47041550158063572, 12.26659068614894998 ) ) ;
#14760 = CARTESIAN_POINT ( 'NONE',  ( 22.26659068614894466, 53.88708216824731068, 7.082119434687054849 ) ) ;
#14761 = AXIS2_PLACEMENT_3D ( 'NONE', #82199, #12718, #66204 ) ;
#14762 = CARTESIAN_POINT ( 'NONE',  ( 7.084665262690076126, 7.022018677488169658, -10.88017736071110164 ) ) ;
#14763 = VERTEX_POINT ( 'NONE', #97793 ) ;
#14764 = CARTESIAN_POINT ( 'NONE',  ( 12.63842701281683034, 27.46726448433411250, 9.846743663894596210 ) ) ;
#14765 = CARTESIAN_POINT ( 'NONE',  ( 0.5774900079438590739, 32.64701867748816966, -5.440088680355550821 ) ) ;
#14766 = CARTESIAN_POINT ( 'NONE',  ( 5.076628168052703671, 46.84226448433412315, 8.527530157486179263 ) ) ;
#14767 = CARTESIAN_POINT ( 'NONE',  ( -4.164238869374099039, 6.803748834913967869, 8.674139862899312516E-16 ) ) ;
#14768 = DIRECTION ( 'NONE',  ( 0.000000000000000000, 1.000000000000000000, 0.000000000000000000 ) ) ;
#14769 = VECTOR ( 'NONE', #40776, 1000.000000000000000 ) ;
#14770 = FILL_AREA_STYLE_COLOUR ( '', #19541 ) ;
#14771 = CARTESIAN_POINT ( 'NONE',  ( 22.81628187352647785, 36.62363466993041783, 6.195893100308588602E-16 ) ) ;
#14772 = CARTESIAN_POINT ( 'NONE',  ( 18.52753015748617571, 48.09226448433412315, 4.923371831947298993 ) ) ;
#14773 = ORIENTED_EDGE ( 'NONE', *, *, #20104, .F. ) ;
#14774 = CARTESIAN_POINT ( 'NONE',  ( 0.1532563361054082862, 11.21726448433411605, 2.638427012816831674 ) ) ;
#14775 = AXIS2_PLACEMENT_3D ( 'NONE', #12185, #27180, #4210 ) ;
#14776 = CARTESIAN_POINT ( 'NONE',  ( 10.83696084481538868, -98.17058944465519232, -4.000000000000000000 ) ) ;
#14777 = CARTESIAN_POINT ( 'NONE',  ( -14.48718990079892954, 4.238615592650390652E-16, 0.6093675230839495915 ) ) ;
#14778 = CARTESIAN_POINT ( 'NONE',  ( 20.88017736071110519, 15.56368534415483751, 2.639326808657452039E-16 ) ) ;
#14779 = CARTESIAN_POINT ( 'NONE',  ( 10.00000000000000000, 50.55374883491396787, -14.16423886937410082 ) ) ;
#14780 = CARTESIAN_POINT ( 'NONE',  ( 17.96484262340118221, 41.18868534415484106, -7.964842623401177768 ) ) ;
#14781 = CARTESIAN_POINT ( 'NONE',  ( 6.204703633549690345, 0.7620821682473009062, -14.16423886937410259 ) ) ;
#14782 = CARTESIAN_POINT ( 'NONE',  ( 8.564643372776536978, 0.5000000000000004441, 12.31449893000746343 ) ) ;
#14783 = B_SPLINE_CURVE_WITH_KNOTS ( 'NONE', 3,
 ( #69947, #94407, #56423, #77426, #62421, #92925 ),
 .UNSPECIFIED., .F., .F.,
 ( 4, 2, 4 ),
 ( 0.0002800047503720886136, 0.0006862100262544192433, 0.001092415302136749873 ),
 .UNSPECIFIED. ) ;
#14784 = CARTESIAN_POINT ( 'NONE',  ( 19.84674366389459266, 28.30059781766745886, 2.638427012816836559 ) ) ;
#14785 = CARTESIAN_POINT ( 'NONE',  ( -0.8801773607110991993, 2.855352010821504471, -2.915334737309923874 ) ) ;
#14786 = CARTESIAN_POINT ( 'NONE',  ( 17.20831665107776587, 37.88393115100078745, 7.208316651077764980 ) ) ;
#14787 = COLOUR_RGB ( '', 0.66274510, 0.83137255, 0.94901961) ;
#14788 = CARTESIAN_POINT ( 'NONE',  ( 19.84674366389459266, 48.71726448433413026, -2.638427012816827677 ) ) ;
#14789 = CARTESIAN_POINT ( 'NONE',  ( 4.559911319644449179, 42.23035201082151247, -9.422509992056141925 ) ) ;
#14790 = AXIS2_PLACEMENT_3D ( 'NONE', #83391, #14909, #45381 ) ;
#14791 = ORIENTED_EDGE ( 'NONE', *, *, #94068, .F. ) ;
#14792 = CARTESIAN_POINT ( 'NONE',  ( 13.43411237798106583, 52.66530133659708213, -12.81628187352647252 ) ) ;
#14793 = CARTESIAN_POINT ( 'NONE',  ( 3.469446951953614189E-15, 4.171802177851546389, 11.25000000000000355 ) ) ;
#14794 = CARTESIAN_POINT ( 'NONE',  ( 10.00000000000000178, 2.258931151000784787, 9.846743663894594434 ) ) ;
#14795 = CARTESIAN_POINT ( 'NONE',  ( 22.81628187352647785, 51.62363466993042493, 6.195893100308588602E-16 ) ) ;
#14797 = CARTESIAN_POINT ( 'NONE',  ( 7.361572987183170547, 52.05059781766745175, 9.846743663894590881 ) ) ;
#14796 = CARTESIAN_POINT ( 'NONE',  ( 7.084665262690076126, 4.105352010821503583, 10.88017736071109987 ) ) ;
#14798 = CARTESIAN_POINT ( 'NONE',  ( -8.209432707284950226, 0.5000000000000004441, 12.55409154915480485 ) ) ;
#14799 = DIRECTION ( 'NONE',  ( 0.000000000000000000, 0.000000000000000000, 1.000000000000000000 ) ) ;
#14800 = B_SPLINE_CURVE_WITH_KNOTS ( 'NONE', 3,
 ( #11111, #33111, #32119, #3133, #85637, #62616 ),
 .UNSPECIFIED., .F., .F.,
 ( 4, 2, 4 ),
 ( 0.0002800715030460627138, 0.0006862774322447868407, 0.001092483361443510968 ),
 .UNSPECIFIED. ) ;
#14801 = CARTESIAN_POINT ( 'NONE',  ( 24.16423886937410614, 29.51208216824729647, -3.795296366450302550 ) ) ;
#14802 = CARTESIAN_POINT ( 'NONE',  ( 10.00000000000000178, 43.05374883491397497, 14.16423886937410082 ) ) ;
#14803 = CARTESIAN_POINT ( 'NONE',  ( 19.84674366389459621, 53.50893115100078745, 7.409399052514197653E-17 ) ) ;
#14804 = CARTESIAN_POINT ( 'NONE',  ( 4.406177045957827332, -8.255047197809593840, -2.500000000000000000 ) ) ;
#14805 = CARTESIAN_POINT ( 'NONE',  ( 4.559911319644449179, 47.23035201082150536, -9.422509992056141925 ) ) ;
#14806 = CARTESIAN_POINT ( 'NONE',  ( 1.472469842513823179, 1.425597817667451528, 4.923371831947296329 ) ) ;
#14807 = AXIS2_PLACEMENT_3D ( 'NONE', #2435, #10402, #71408 ) ;
#14808 = SURFACE_STYLE_USAGE ( .BOTH. , #23290 ) ;
#14809 = VERTEX_POINT ( 'NONE', #51769 ) ;
#14810 = CARTESIAN_POINT ( 'NONE',  ( 10.00000000000000178, 60.37363466993041783, 12.81628187352647608 ) ) ;
#14811 = ORIENTED_EDGE ( 'NONE', *, *, #68798, .F. ) ;
#14812 = CARTESIAN_POINT ( 'NONE',  ( 20.88017736071110164, 60.35535201082151957, 2.915334737309930979 ) ) ;
#14813 = VERTEX_POINT ( 'NONE', #98785 ) ;
#14814 = CARTESIAN_POINT ( 'NONE',  ( 24.16423886937410614, 4.512082168247300906, -3.795296366450302550 ) ) ;
#14815 = CARTESIAN_POINT ( 'NONE',  ( 1.472469842513823179, 5.592264484334118713, -4.923371831947296329 ) ) ;
#14816 = CARTESIAN_POINT ( 'NONE',  ( 2.035157376598822676, 27.43868534415483396, -7.964842623401177768 ) ) ;
#14817 = ADVANCED_FACE ( 'NONE', ( #81757 ), #29255, .T. ) ;
#14818 = ORIENTED_EDGE ( 'NONE', *, *, #81525, .F. ) ;
#14819 = CARTESIAN_POINT ( 'NONE',  ( 10.00000000000000000, 26.81368534415484106, -10.88017736071110342 ) ) ;
#14820 = AXIS2_PLACEMENT_3D ( 'NONE', #89938, #82437, #88959 ) ;
#14821 = ORIENTED_EDGE ( 'NONE', *, *, #27965, .T. ) ;
#14822 = CARTESIAN_POINT ( 'NONE',  ( 1.046131998950039499, 45.73810908735726599, 6.499999999999985789 ) ) ;
#14823 = ORIENTED_EDGE ( 'NONE', *, *, #6586, .F. ) ;
#14824 = CARTESIAN_POINT ( 'NONE',  ( -2.816281873526473856, 19.33196800326375708, 3.434112377981055619 ) ) ;
#14825 = CARTESIAN_POINT ( 'NONE',  ( 20.88017736071110875, 60.77201867748817676, -2.915334737309920765 ) ) ;
#14826 = DIRECTION ( 'NONE',  ( 0.000000000000000000, 0.000000000000000000, -1.000000000000000000 ) ) ;
#14827 = LINE ( 'NONE', #53292, #1587 ) ;
#14828 = CARTESIAN_POINT ( 'NONE',  ( 12.63842701281683034, 2.467264484334118269, 9.846743663894596210 ) ) ;
#14829 = CARTESIAN_POINT ( 'NONE',  ( 4.559911319644449179, 32.23035201082150536, -9.422509992056141925 ) ) ;
#14830 = CIRCLE ( 'NONE', #62686, 10.65000000000000036 ) ;
#14831 = EDGE_LOOP ( 'NONE', ( #60474, #5384, #19440, #34341 ) ) ;
#14832 = ADVANCED_FACE ( 'NONE', ( #29741 ), #51271, .F. ) ;
#14833 = CARTESIAN_POINT ( 'NONE',  ( 6.565887622018943937, 63.08196800326376064, -12.81628187352647608 ) ) ;
#14834 = CARTESIAN_POINT ( 'NONE',  ( -0.8801773607111008646, 38.27201867748816255, 2.915334737309923430 ) ) ;
#14835 = CARTESIAN_POINT ( 'NONE',  ( -46.77276111675546844, 103.6220771345834919, -6.142410991622097249 ) ) ;
#14836 = EDGE_CURVE ( 'NONE', #6506, #73794, #14603, .T. ) ;
#14837 = CARTESIAN_POINT ( 'NONE',  ( 16.40814093676323893, 55.79030133659708923, 11.09922568453595026 ) ) ;
#14838 = CARTESIAN_POINT ( 'NONE',  ( 15.44008868035555793, 56.39701867748817676, -9.422509992056140149 ) ) ;
#14839 = TOROIDAL_SURFACE ( 'NONE', #515, 3.500000000000000888, 0.5000000000000000000 ) ;
#14840 = CARTESIAN_POINT ( 'NONE',  ( 22.81628187352647785, 1.415301336597087012, 3.434112377981063169 ) ) ;
#14841 = TOROIDAL_SURFACE ( 'NONE', #10047, 18.93999999999999773, 0.5000000000000000000 ) ;
#14842 = CARTESIAN_POINT ( 'NONE',  ( 2.791683348922237240, 20.38393115100078745, -7.208316651077763204 ) ) ;
#14843 = CARTESIAN_POINT ( 'NONE',  ( 19.38216949554541202, 60.99863466993042493, 9.382169495545424454 ) ) ;
#14844 = CARTESIAN_POINT ( 'NONE',  ( 2.603489959281613420, 35.43575266056827644, -6.500000000000031086 ) ) ;
#14845 = CARTESIAN_POINT ( 'NONE',  ( 1.472469842513823179, 6.425597817667451750, 4.923371831947296329 ) ) ;
#14846 = VECTOR ( 'NONE', #85824, 1000.000000000000000 ) ;
#14847 = CARTESIAN_POINT ( 'NONE',  ( 3.591859063236763294, 3.290301336597087012, -11.09922568453595026 ) ) ;
#14849 = CARTESIAN_POINT ( 'NONE',  ( 0.1532563361054083140, 66.00893115100079456, 1.131784320476157264E-15 ) ) ;
#14848 = CARTESIAN_POINT ( 'NONE',  ( 14.94699059465102309, 0.3640475087720504432, -1.259949270174814284 ) ) ;
#14850 = CARTESIAN_POINT ( 'NONE',  ( 0.5774900079438590739, 32.64701867748816966, -5.440088680355550821 ) ) ;
#14851 = CARTESIAN_POINT ( 'NONE',  ( 17.20831665107776587, 52.88393115100078035, 7.208316651077764980 ) ) ;
#14852 = CARTESIAN_POINT ( 'NONE',  ( -1.926860441876564023, 32.87045670184114954, 3.195792623639529761 ) ) ;
#14853 = CARTESIAN_POINT ( 'NONE',  ( 19.84674366389459266, 18.71726448433411960, -2.638427012816827677 ) ) ;
#14854 = CARTESIAN_POINT ( 'NONE',  ( 1.472469842513823179, 5.592264484334118713, -4.923371831947296329 ) ) ;
#14856 = ORIENTED_EDGE ( 'NONE', *, *, #42334, .T. ) ;
#14855 = CARTESIAN_POINT ( 'NONE',  ( 19.38216949554541202, 5.998634669930420493, 9.382169495545424454 ) ) ;
#14857 = FILL_AREA_STYLE ('',( #21857 ) ) ;
#14858 = CARTESIAN_POINT ( 'NONE',  ( 14.92337183194729988, 59.34226448433412315, -8.527530157486177487 ) ) ;
#14859 = CARTESIAN_POINT ( 'NONE',  ( 12.91533473730992121, 4.522018677488170546, 10.88017736071110164 ) ) ;
#14860 = CARTESIAN_POINT ( 'NONE',  ( 0.1532563361054083140, 46.00893115100079456, 1.131784320476157264E-15 ) ) ;
#14861 = ORIENTED_EDGE ( 'NONE', *, *, #76418, .T. ) ;
#14862 = DIRECTION ( 'NONE',  ( -0.1650476058606810958, 0.000000000000000000, 0.9862856015372308827 ) ) ;
#14863 = CARTESIAN_POINT ( 'NONE',  ( 22.26659068614895176, 64.72041550158064638, -7.082119434687042414 ) ) ;
#14864 = CARTESIAN_POINT ( 'NONE',  ( 1.274849032794131976, 13.57228050351029403, 6.499999999999760192 ) ) ;
#14865 = CARTESIAN_POINT ( 'NONE',  ( 20.88017736071110164, 35.35535201082150536, 2.915334737309930979 ) ) ;
#14866 = CARTESIAN_POINT ( 'NONE',  ( 13.79529636645031943, 50.34541550158064638, -14.16423886937409904 ) ) ;
#14868 = DIRECTION ( 'NONE',  ( -1.000000000000000000, 0.000000000000000000, 0.000000000000000000 ) ) ;
#14867 = CARTESIAN_POINT ( 'NONE',  ( 24.16423886937409904, 64.09541550158064638, 3.795296366450317205 ) ) ;
#14869 = CARTESIAN_POINT ( 'NONE',  ( 1.472469842513823179, 6.425597817667451750, 4.923371831947296329 ) ) ;
#14870 = EDGE_CURVE ( 'NONE', #40514, #20839, #7614, .T. ) ;
#14871 = CARTESIAN_POINT ( 'NONE',  ( 0.1532563361054083140, 26.00893115100078745, 1.131784320476157264E-15 ) ) ;
#14872 = CARTESIAN_POINT ( 'NONE',  ( 21.09922568453594849, 16.20696800326375353, 6.408140936763242479 ) ) ;
#14873 = VERTEX_POINT ( 'NONE', #52745 ) ;
#14874 = AXIS2_PLACEMENT_3D ( 'NONE', #85696, #10196, #93679 ) ;
#14875 = ADVANCED_FACE ( 'NONE', ( #74250 ), #20366, .T. ) ;
#14876 = LINE ( 'NONE', #7857, #52291 ) ;
#14877 = FILL_AREA_STYLE_COLOUR ( '', #33928 ) ;
#14878 = CARTESIAN_POINT ( 'NONE',  ( 2.917880565312950480, 5.970415501580634832, -12.26659068614894821 ) ) ;
#14879 = AXIS2_PLACEMENT_3D ( 'NONE', #84671, #84191, #98726 ) ;
#14880 = CARTESIAN_POINT ( 'NONE',  ( 1.472469842513823179, 30.59226448433411960, -4.923371831947296329 ) ) ;
#14881 = DIRECTION ( 'NONE',  ( -0.000000000000000000, -1.000000000000000000, -0.000000000000000000 ) ) ;
#14882 = CARTESIAN_POINT ( 'NONE',  ( 13.79529636645030344, 38.26208216824729647, 14.16423886937410614 ) ) ;
#14883 = CARTESIAN_POINT ( 'NONE',  ( 14.92337183194729988, 9.342264484334119601, -8.527530157486177487 ) ) ;
#14885 = DIRECTION ( 'NONE',  ( -0.000000000000000000, -1.000000000000000000, -0.000000000000000000 ) ) ;
#14884 = CARTESIAN_POINT ( 'NONE',  ( 6.284583270191197002, -88.40194713205143273, -3.750000000000000000 ) ) ;
#14886 = CARTESIAN_POINT ( 'NONE',  ( -0.8801773607110991993, 27.85535201082150181, -2.915334737309923874 ) ) ;
#14887 = CARTESIAN_POINT ( 'NONE',  ( -1.099225684535947600, 54.54030133659708923, 6.408140936763237150 ) ) ;
#14888 = CARTESIAN_POINT ( 'NONE',  ( 20.88017736071110875, 5.772018677488170546, -2.915334737309920765 ) ) ;
#14889 = CARTESIAN_POINT ( 'NONE',  ( 16.40814093676324603, 32.45696800326375353, -11.09922568453594671 ) ) ;
#14890 = CARTESIAN_POINT ( 'NONE',  ( 12.63842701281683034, 2.467264484334118269, 9.846743663894596210 ) ) ;
#14891 = EDGE_LOOP ( 'NONE', ( #11219, #34464, #6947, #45931 ) ) ;
#14892 =( NAMED_UNIT ( * ) SI_UNIT ( $, .STERADIAN. ) SOLID_ANGLE_UNIT ( ) );
#14893 = CARTESIAN_POINT ( 'NONE',  ( -14.99847009497944406, 0.5000000000000004441, -0.2142307401082361173 ) ) ;
#14894 = CARTESIAN_POINT ( 'NONE',  ( 2.917880565312950480, 35.97041550158063217, -12.26659068614894821 ) ) ;
#14895 = CARTESIAN_POINT ( 'NONE',  ( 22.26659068614895176, 19.72041550158063572, -7.082119434687042414 ) ) ;
#14896 = CARTESIAN_POINT ( 'NONE',  ( -0.8801773607111009756, 38.06368534415484106, 1.068504757029289695E-15 ) ) ;
#14897 = DIRECTION ( 'NONE',  ( -0.000000000000000000, -1.000000000000000000, -0.000000000000000000 ) ) ;
#14898 = DIRECTION ( 'NONE',  ( 0.000000000000000000, 1.000000000000000000, 0.000000000000000000 ) ) ;
#14899 = CARTESIAN_POINT ( 'NONE',  ( 2.035157376598822676, 57.43868534415484106, -7.964842623401177768 ) ) ;
#14900 = CARTESIAN_POINT ( 'NONE',  ( 20.88017736071110875, 65.77201867748817676, -2.915334737309920765 ) ) ;
#14901 = CARTESIAN_POINT ( 'NONE',  ( 21.09922568453595559, 27.04030133659708568, -6.408140936763230044 ) ) ;
#14902 = DIRECTION ( 'NONE',  ( 1.257568779154408793E-17, 1.000000000000000000, -0.000000000000000000 ) ) ;
#14903 = CARTESIAN_POINT ( 'NONE',  ( 19.72487221294570858, 26.86607318730131055, 6.500000000000000888 ) ) ;
#14904 = CARTESIAN_POINT ( 'NONE',  ( 5.076628168052703671, 31.84226448433412315, 8.527530157486179263 ) ) ;
#14905 = CARTESIAN_POINT ( 'NONE',  ( 0.6178305044545818747, 13.49863466993041783, -9.382169495545419124 ) ) ;
#14906 = CARTESIAN_POINT ( 'NONE',  ( 1.472469842513823179, 0.5922644843341181575, -4.923371831947296329 ) ) ;
#14907 = CARTESIAN_POINT ( 'NONE',  ( -0.8801773607110991993, 2.855352010821504471, -2.915334737309923874 ) ) ;
#14908 = CARTESIAN_POINT ( 'NONE',  ( 18.52753015748617571, 38.09226448433412315, 4.923371831947298993 ) ) ;
#14909 = DIRECTION ( 'NONE',  ( -0.000000000000000000, -0.000000000000000000, -1.000000000000000000 ) ) ;
#14910 = CIRCLE ( 'NONE', #56434, 3.000000000000000888 ) ;
#14912 = CARTESIAN_POINT ( 'NONE',  ( -4.164238869374099039, 1.803748834913967647, 8.674139862899312516E-16 ) ) ;
#14911 = CARTESIAN_POINT ( 'NONE',  ( 17.20831665107776587, 14.13393115100078568, -7.208316651077762316 ) ) ;
#14913 = CARTESIAN_POINT ( 'NONE',  ( 13.79529636645030344, 3.262082168247301350, 14.16423886937410614 ) ) ;
#14914 = CARTESIAN_POINT ( 'NONE',  ( -6.000000000000000000, 78.07179676972447169, 6.250000000000000000 ) ) ;
#14915 = CARTESIAN_POINT ( 'NONE',  ( 12.91533473730992121, 34.52201867748817676, 10.88017736071110164 ) ) ;
#14917 = CARTESIAN_POINT ( 'NONE',  ( 6.204703633549690345, 27.84541550158063217, 14.16423886937410082 ) ) ;
#14916 = CARTESIAN_POINT ( 'NONE',  ( 10.00000000000000178, 4.313685344154837509, 10.88017736071110342 ) ) ;
#14918 = VECTOR ( 'NONE', #97648, 1000.000000000000000 ) ;
#14919 = CARTESIAN_POINT ( 'NONE',  ( 19.42250999205614193, 35.14701867748816966, 5.440088680355555262 ) ) ;
#14920 = CARTESIAN_POINT ( 'NONE',  ( -0.8801773607111009756, 23.06368534415484106, 1.068504757029289695E-15 ) ) ;
#14921 = VERTEX_POINT ( 'NONE', #14777 ) ;
#14922 = AXIS2_PLACEMENT_3D ( 'NONE', #5557, #66536, #90507 ) ;
#14923 = CARTESIAN_POINT ( 'NONE',  ( 4.559911319644449179, 28.89701867748817321, 9.422509992056141925 ) ) ;
#14924 = CARTESIAN_POINT ( 'NONE',  ( 13.43411237798105340, 45.58196800326374643, 12.81628187352647963 ) ) ;
#14925 = EDGE_CURVE ( 'NONE', #61145, #10785, #38258, .T. ) ;
#14926 = CARTESIAN_POINT ( 'NONE',  ( -0.8801773607111009756, 43.06368534415484106, 1.068504757029289695E-15 ) ) ;
#14928 = CARTESIAN_POINT ( 'NONE',  ( 17.96484262340118221, 51.18868534415483396, -7.964842623401177768 ) ) ;
#14927 = DIRECTION ( 'NONE',  ( 1.000000000000000000, 0.000000000000000000, 0.000000000000000000 ) ) ;
#14929 = VERTEX_POINT ( 'NONE', #52258 ) ;
#14930 = CARTESIAN_POINT ( 'NONE',  ( 15.44008868035555260, 34.73035201082151247, 9.422509992056143702 ) ) ;
#14931 = CARTESIAN_POINT ( 'NONE',  ( 6.757940885639631468, -58.32678904743398363, 3.750000000000000000 ) ) ;
#14932 = CARTESIAN_POINT ( 'NONE',  ( 0.2751277870542906956, 37.28217586085238366, -6.499999999999992006 ) ) ;
#14933 = CARTESIAN_POINT ( 'NONE',  ( 2.917880565312950480, 40.97041550158063217, -12.26659068614894821 ) ) ;
#14934 = CARTESIAN_POINT ( 'NONE',  ( 7.361572987183170547, 2.050597817667451750, 9.846743663894590881 ) ) ;
#14935 = EDGE_CURVE ( 'NONE', #7550, #91796, #76558, .T. ) ;
#14936 = CARTESIAN_POINT ( 'NONE',  ( 19.84674366389459266, 58.30059781766745886, 2.638427012816836559 ) ) ;
#14937 = CARTESIAN_POINT ( 'NONE',  ( 3.115783986955448892, 15.00000000000000000, 14.16128137375397600 ) ) ;
#14938 = CARTESIAN_POINT ( 'NONE',  ( 12.63842701281683034, 37.46726448433411605, 9.846743663894596210 ) ) ;
#14939 = VERTEX_POINT ( 'NONE', #20780 ) ;
#14940 = CARTESIAN_POINT ( 'NONE',  ( 10.00000000000000000, 29.75893115100078745, -9.846743663894594434 ) ) ;
#14941 = CARTESIAN_POINT ( 'NONE',  ( -11.09922568453594316, -15.45969866340291077, 6.408140936763246920 ) ) ;
#14942 = CARTESIAN_POINT ( 'NONE',  ( 10.00000000000000000, 26.81368534415484106, -10.88017736071110342 ) ) ;
#14943 = CARTESIAN_POINT ( 'NONE',  ( 19.84674366389459266, 38.71726448433412315, -2.638427012816827677 ) ) ;
#14944 = CARTESIAN_POINT ( 'NONE',  ( 10.00000000000000000, 22.87363466993042138, -12.81628187352647608 ) ) ;
#14946 = CARTESIAN_POINT ( 'NONE',  ( 15.44008868035555260, 54.73035201082150536, 9.422509992056143702 ) ) ;
#14945 = CARTESIAN_POINT ( 'NONE',  ( 17.75000000000000355, 84.07179676972448590, 4.000000000000000000 ) ) ;
#14948 = CARTESIAN_POINT ( 'NONE',  ( 2.035157376598824452, 3.688685344154837953, 7.964842623401179544 ) ) ;
#14947 = CARTESIAN_POINT ( 'NONE',  ( 10.00000000000000000, 31.81368534415483751, -10.88017736071110342 ) ) ;
#14949 = CARTESIAN_POINT ( 'NONE',  ( -0.3689425029237898834, 61.17874883491396076, -10.36894250292378850 ) ) ;
#14950 = STYLED_ITEM ( 'NONE', ( #21762 ), #40082 ) ;
#14951 = VECTOR ( 'NONE', #89463, 1000.000000000000114 ) ;
#14952 = EDGE_CURVE ( 'NONE', #67464, #40303, #76250, .T. ) ;
#14953 = CARTESIAN_POINT ( 'NONE',  ( -9.876730923139175999, 0.3639310091266617642, -11.28938378619078264 ) ) ;
#14954 = VERTEX_POINT ( 'NONE', #68265 ) ;
#14955 = CARTESIAN_POINT ( 'NONE',  ( -2.816281873526473856, 19.33196800326375708, 3.434112377981055619 ) ) ;
#14956 = CARTESIAN_POINT ( 'NONE',  ( -0.8801773607110991993, 2.855352010821504471, -2.915334737309923874 ) ) ;
#14957 = CARTESIAN_POINT ( 'NONE',  ( 0.5774900079438607392, 43.48035201082151247, 5.440088680355550821 ) ) ;
#14958 = ADVANCED_FACE ( 'NONE', ( #91239 ), #89026, .T. ) ;
#14959 = ORIENTED_EDGE ( 'NONE', *, *, #71380, .F. ) ;
#14960 = B_SPLINE_CURVE_WITH_KNOTS ( 'NONE', 3,
 ( #44005, #12037, #65520, #49532 ),
 .UNSPECIFIED., .F., .F.,
 ( 4, 4 ),
 ( 5.444379262168902198E-17, 0.002562518741975295181 ),
 .UNSPECIFIED. ) ;
#14961 = CARTESIAN_POINT ( 'NONE',  ( 2.035157376598824452, 53.68868534415484817, 7.964842623401179544 ) ) ;
#14962 = CARTESIAN_POINT ( 'NONE',  ( 2.791683348922240793, 41.63393115100078745, 7.208316651077764092 ) ) ;
#14963 = CARTESIAN_POINT ( 'NONE',  ( 18.52753015748618282, 18.92559781766745175, -4.923371831947291888 ) ) ;
#14964 = CARTESIAN_POINT ( 'NONE',  ( 5.076628168052703671, 16.84226448433411960, 8.527530157486179263 ) ) ;
#14965 = CARTESIAN_POINT ( 'NONE',  ( 13.61464873478162829, 14.49999999999999822, 6.296136897217933459 ) ) ;
#14967 = CARTESIAN_POINT ( 'NONE',  ( 13.43411237798105340, 35.58196800326375353, 12.81628187352647963 ) ) ;
#14966 = DIRECTION ( 'NONE',  ( 0.000000000000000000, -0.000000000000000000, 1.000000000000000000 ) ) ;
#14969 = CARTESIAN_POINT ( 'NONE',  ( 11.96291822454875842, 4.834832779786913688E-16, 8.193813980849165901 ) ) ;
#14968 = CARTESIAN_POINT ( 'NONE',  ( 5.076628168052703671, 11.84226448433411960, 8.527530157486179263 ) ) ;
#14970 = DIRECTION ( 'NONE',  ( 1.000000000000000000, -0.000000000000000000, -0.000000000000000000 ) ) ;
#14972 = VERTEX_POINT ( 'NONE', #53244 ) ;
#14971 = CARTESIAN_POINT ( 'NONE',  ( 17.20831665107776587, 29.13393115100078390, -7.208316651077762316 ) ) ;
#14973 = LINE ( 'NONE', #40913, #91681 ) ;
#14974 = CARTESIAN_POINT ( 'NONE',  ( 22.81628187352648496, 11.83196800326375531, -3.434112377981050290 ) ) ;
#14975 = CIRCLE ( 'NONE', #75619, 0.2500000000000002220 ) ;
#14976 = CARTESIAN_POINT ( 'NONE',  ( 4.559911319644449179, 57.23035201082150536, -9.422509992056141925 ) ) ;
#14977 = CARTESIAN_POINT ( 'NONE',  ( 6.204703633549690345, 30.76208216824730357, -14.16423886937410259 ) ) ;
#14978 = CARTESIAN_POINT ( 'NONE',  ( -11.22722615950653413, 89.90850287678183861, 6.380836486320208500 ) ) ;
#14979 = AXIS2_PLACEMENT_3D ( 'NONE', #53949, #9432, #30941 ) ;
#14980 = CARTESIAN_POINT ( 'NONE',  ( 20.36894250292379738, 34.92874883491396076, -10.36894250292379027 ) ) ;
#14981 = CARTESIAN_POINT ( 'NONE',  ( -4.164238869374099039, 56.80374883491397497, 8.674139862899312516E-16 ) ) ;
#14982 = CARTESIAN_POINT ( 'NONE',  ( 17.08211943468705130, 8.470415501580635720, 12.26659068614894998 ) ) ;
#14984 = CARTESIAN_POINT ( 'NONE',  ( -2.888814634336603238, 15.00000000000000178, -14.33747749179072883 ) ) ;
#14983 = CARTESIAN_POINT ( 'NONE',  ( -2.266590686148945544, 27.22041550158063572, 7.082119434687048631 ) ) ;
#14985 = CARTESIAN_POINT ( 'NONE',  ( 2.035157376598822676, 52.43868534415483396, -7.964842623401177768 ) ) ;
#14986 = CARTESIAN_POINT ( 'NONE',  ( 4.526800700887880780, -5.190657137169758073, -2.750000000000000000 ) ) ;
#14987 = CARTESIAN_POINT ( 'NONE',  ( 1.472469842513823179, 26.42559781766745175, 4.923371831947296329 ) ) ;
#14989 = CARTESIAN_POINT ( 'NONE',  ( 12.63842701281683034, 42.46726448433412315, 9.846743663894596210 ) ) ;
#14988 = CARTESIAN_POINT ( 'NONE',  ( 20.88017736071110875, 65.77201867748817676, -2.915334737309920765 ) ) ;
#14990 = CARTESIAN_POINT ( 'NONE',  ( 17.96484262340118221, 29.93868534415484106, 7.964842623401181321 ) ) ;
#14991 = CARTESIAN_POINT ( 'NONE',  ( 22.81628187352647785, 56.62363466993042493, 6.195893100308588602E-16 ) ) ;
#14992 = CARTESIAN_POINT ( 'NONE',  ( 18.52753015748617571, 58.09226448433411605, 4.923371831947298993 ) ) ;
#14993 = CARTESIAN_POINT ( 'NONE',  ( -9.876730923139204421, 14.49999999999999112, -11.28938378619079863 ) ) ;
#14994 = EDGE_CURVE ( 'NONE', #55728, #45005, #83749, .T. ) ;
#14995 = CARTESIAN_POINT ( 'NONE',  ( 5.076628168052703671, 26.84226448433411960, 8.527530157486179263 ) ) ;
#14996 = CARTESIAN_POINT ( 'NONE',  ( 22.81628187352648496, 51.83196800326376064, -3.434112377981050290 ) ) ;
#14997 = CARTESIAN_POINT ( 'NONE',  ( 3.795296366450306547, -24.65458449841936428, -14.16423886937410259 ) ) ;
#14998 = CARTESIAN_POINT ( 'NONE',  ( 20.88017736071110875, 45.77201867748816966, -2.915334737309920765 ) ) ;
#14999 = CARTESIAN_POINT ( 'NONE',  ( 0.1532563361054082862, 56.21726448433411605, 2.638427012816831674 ) ) ;
#15000 = CARTESIAN_POINT ( 'NONE',  ( 6.204703633549690345, 37.84541550158063927, 14.16423886937410082 ) ) ;
#15001 = ORIENTED_EDGE ( 'NONE', *, *, #87170, .T. ) ;
#15002 = CARTESIAN_POINT ( 'NONE',  ( 24.16423886937410614, 4.303748834913967869, 8.672049930838204340E-16 ) ) ;
#15003 = CARTESIAN_POINT ( 'NONE',  ( 7.084665262690076126, 57.02201867748817676, -10.88017736071110164 ) ) ;
#15004 = DIRECTION ( 'NONE',  ( 0.000000000000000000, 1.000000000000000000, 0.000000000000000000 ) ) ;
#15005 = CARTESIAN_POINT ( 'NONE',  ( 6.204703633549690345, 55.76208216824730357, -14.16423886937410259 ) ) ;
#15006 = CARTESIAN_POINT ( 'NONE',  ( 21.09922568453594849, 11.20696800326375531, 6.408140936763242479 ) ) ;
#15007 = CARTESIAN_POINT ( 'NONE',  ( -3.836325488035982278, 14.49999999999999112, -14.50112432709434351 ) ) ;
#15008 = CARTESIAN_POINT ( 'NONE',  ( 15.44008868035555793, 51.39701867748816966, -9.422509992056140149 ) ) ;
#15009 = LINE ( 'NONE', #45479, #82110 ) ;
#15010 = CARTESIAN_POINT ( 'NONE',  ( -46.94000000000001194, 100.8028158894829289, -8.422108456579607605 ) ) ;
#15011 = CARTESIAN_POINT ( 'NONE',  ( 22.81628187352647785, 31.41530133659709279, 3.434112377981063169 ) ) ;
#15012 = CARTESIAN_POINT ( 'NONE',  ( 10.00000000000000178, 48.05374883491396787, 14.16423886937410082 ) ) ;
#15013 = CARTESIAN_POINT ( 'NONE',  ( 9.422509992056141925, 30.14701867748817321, 5.440088680355547268 ) ) ;
#15014 = CARTESIAN_POINT ( 'NONE',  ( 15.44008868035555260, 14.73035201082150536, 9.422509992056143702 ) ) ;
#15015 = CARTESIAN_POINT ( 'NONE',  ( 10.00000000000000178, 29.31368534415483751, 10.88017736071110342 ) ) ;
#15016 = CARTESIAN_POINT ( 'NONE',  ( 17.20831665107776587, 54.13393115100079456, -7.208316651077762316 ) ) ;
#15017 = CARTESIAN_POINT ( 'NONE',  ( 22.81628187352648496, 46.83196800326376064, -3.434112377981050290 ) ) ;
#15018 = PRESENTATION_STYLE_ASSIGNMENT (( #29484 ) ) ;
#15019 = ORIENTED_EDGE ( 'NONE', *, *, #24095, .T. ) ;
#15020 = CARTESIAN_POINT ( 'NONE',  ( -0.8801773607110991993, 17.85535201082150536, -2.915334737309923874 ) ) ;
#15021 = CARTESIAN_POINT ( 'NONE',  ( 19.38216949554541202, 20.99863466993042138, 9.382169495545424454 ) ) ;
#15022 = CYLINDRICAL_SURFACE ( 'NONE', #62479, 19.99999999999999645 ) ;
#15023 = CARTESIAN_POINT ( 'NONE',  ( 0.1532563361054082862, 46.21726448433411605, 2.638427012816831674 ) ) ;
#15024 = CARTESIAN_POINT ( 'NONE',  ( 12.91533473730993009, 36.60535201082151247, -10.88017736071109987 ) ) ;
#15025 = CARTESIAN_POINT ( 'NONE',  ( 3.591859063236763294, 23.29030133659708568, -11.09922568453595026 ) ) ;
#15027 = CARTESIAN_POINT ( 'NONE',  ( 20.88017736071110875, 15.77201867748817143, -2.915334737309920321 ) ) ;
#15026 = CARTESIAN_POINT ( 'NONE',  ( 7.084665262690076126, 47.02201867748818387, -10.88017736071110164 ) ) ;
#15028 = EDGE_CURVE ( 'NONE', #57285, #58602, #26432, .T. ) ;
#15029 =( LENGTH_UNIT ( ) NAMED_UNIT ( * ) SI_UNIT ( .MILLI., .METRE. ) );
#15030 = CARTESIAN_POINT ( 'NONE',  ( 16.40814093676323893, 55.79030133659708923, 11.09922568453595026 ) ) ;
#15031 = ORIENTED_EDGE ( 'NONE', *, *, #7055, .T. ) ;
#15032 = CARTESIAN_POINT ( 'NONE',  ( 17.96484262340118221, 54.93868534415484106, 7.964842623401181321 ) ) ;
#15034 = CARTESIAN_POINT ( 'NONE',  ( 20.36894250292379738, 4.928748834913967869, -10.36894250292379027 ) ) ;
#15033 = CARTESIAN_POINT ( 'NONE',  ( -1.099225684535947600, 28.70696800326375353, -6.408140936763238038 ) ) ;
#15035 = CARTESIAN_POINT ( 'NONE',  ( 5.076628168052704559, 5.175597817667451750, -8.527530157486179263 ) ) ;
#15036 = CARTESIAN_POINT ( 'NONE',  ( 7.084665262690076126, 57.02201867748817676, -10.88017736071110164 ) ) ;
#15037 = CARTESIAN_POINT ( 'NONE',  ( 10.00000000000000000, 45.55374883491397497, -14.16423886937410082 ) ) ;
#15038 = DIRECTION ( 'NONE',  ( 1.000000000000000000, -0.000000000000000000, -0.000000000000000000 ) ) ;
#15039 = CARTESIAN_POINT ( 'NONE',  ( 12.63842701281683034, 12.46726448433411782, 9.846743663894596210 ) ) ;
#15040 = CARTESIAN_POINT ( 'NONE',  ( 2.791683348922240793, 1.633931151000784565, 7.208316651077764092 ) ) ;
#15041 = DIRECTION ( 'NONE',  ( 0.000000000000000000, 0.000000000000000000, -1.000000000000000000 ) ) ;
#15042 = CARTESIAN_POINT ( 'NONE',  ( -4.164238869374099927, 47.01208216824729647, 3.795296366450308767 ) ) ;
#15043 = CARTESIAN_POINT ( 'NONE',  ( 20.24186590665277663, 24.73410085661204150, 6.114288769123037426 ) ) ;
#15044 = EDGE_CURVE ( 'NONE', #92547, #14921, #53844, .T. ) ;
#15045 = CARTESIAN_POINT ( 'NONE',  ( -0.8801773607111008646, 13.27201867748817143, 2.915334737309923430 ) ) ;
#15046 = CARTESIAN_POINT ( 'NONE',  ( -7.124934413272103306, -78.83349193436582425, -4.000000000000001776 ) ) ;
#15047 = VERTEX_POINT ( 'NONE', #62209 ) ;
#15048 = CARTESIAN_POINT ( 'NONE',  ( 4.559911319644449179, 13.89701867748817321, 9.422509992056141925 ) ) ;
#15049 = CARTESIAN_POINT ( 'NONE',  ( 24.16423886937410614, 64.51208216824728936, -3.795296366450302550 ) ) ;
#15050 = CARTESIAN_POINT ( 'NONE',  ( 17.20831665107776587, 49.13393115100078745, -7.208316651077762316 ) ) ;
#15051 = CARTESIAN_POINT ( 'NONE',  ( 19.38216949554541557, 42.24863466993041783, -9.382169495545420901 ) ) ;
#15052 = CARTESIAN_POINT ( 'NONE',  ( -1.499999999999998668, 1.840000000000001412, 0.000000000000000000 ) ) ;
#15055 = CARTESIAN_POINT ( 'NONE',  ( 24.16423886937409904, 9.095415501580633943, 3.795296366450317205 ) ) ;
#15054 = CARTESIAN_POINT ( 'NONE',  ( 3.836325488036075981, 14.49999999999999112, 14.50112432709431687 ) ) ;
#15053 = COLOUR_RGB ( '', 0.72549020, 0.75294118, 0.79215686) ;
#15056 = CARTESIAN_POINT ( 'NONE',  ( 4.559911319644449179, 18.89701867748817321, 9.422509992056141925 ) ) ;
#15057 = CARTESIAN_POINT ( 'NONE',  ( 19.42250999205614193, 10.14701867748816966, 5.440088680355555262 ) ) ;
#15058 = EDGE_CURVE ( 'NONE', #72922, #62857, #32201, .T. ) ;
#15059 = ADVANCED_FACE ( 'NONE', ( #77221 ), #44267, .T. ) ;
#15060 = CARTESIAN_POINT ( 'NONE',  ( 0.1532563361054100626, 40.80059781766745886, -2.638427012816831230 ) ) ;
#15061 = CARTESIAN_POINT ( 'NONE',  ( -4.020549461440751315, 0.000000000000000000, 3.684154808197060316 ) ) ;
#15062 = CARTESIAN_POINT ( 'NONE',  ( 10.00000000000000178, 27.25893115100078390, 9.846743663894594434 ) ) ;
#15063 = AXIS2_PLACEMENT_3D ( 'NONE', #63652, #55684, #86184 ) ;
#15064 = B_SPLINE_CURVE_WITH_KNOTS ( 'NONE', 3,
 ( #84651, #40633, #10138, #93620, #54623, #55118 ),
 .UNSPECIFIED., .F., .F.,
 ( 4, 2, 4 ),
 ( 3.409110551494654820E-05, 0.0004400426677367934021, 0.0008459942299586403237 ),
 .UNSPECIFIED. ) ;
#15065 = LINE ( 'NONE', #92999, #86529 ) ;
#15066 = CARTESIAN_POINT ( 'NONE',  ( -2.638427012816840111, 14.96726448433411605, -9.846743663894590881 ) ) ;
#15067 = ORIENTED_EDGE ( 'NONE', *, *, #64680, .T. ) ;
#15068 = VERTEX_POINT ( 'NONE', #24241 ) ;
#15069 = FILL_AREA_STYLE ('',( #22562 ) ) ;
#15070 = VERTEX_POINT ( 'NONE', #77710 ) ;
#15071 = CARTESIAN_POINT ( 'NONE',  ( 0.1532563361054083140, 56.00893115100078745, 1.131784320476157264E-15 ) ) ;
#15072 = CARTESIAN_POINT ( 'NONE',  ( -4.164238869374099039, 16.80374883491396787, 8.674139862899312516E-16 ) ) ;
#15074 = CARTESIAN_POINT ( 'NONE',  ( -0.8801773607111009756, 38.06368534415484106, 1.068504757029289695E-15 ) ) ;
#15073 = CARTESIAN_POINT ( 'NONE',  ( 15.44008868035555260, 39.73035201082150536, 9.422509992056143702 ) ) ;
#15076 = CARTESIAN_POINT ( 'NONE',  ( 19.38216949554541557, 37.24863466993041783, -9.382169495545420901 ) ) ;
#15075 = FACE_OUTER_BOUND ( 'NONE', #78243, .T. ) ;
#15077 = CARTESIAN_POINT ( 'NONE',  ( 24.16423886937410614, 4.512082168247300906, -3.795296366450302550 ) ) ;
#15078 = EDGE_CURVE ( 'NONE', #14052, #73541, #65087, .T. ) ;
#15079 = CARTESIAN_POINT ( 'NONE',  ( 0.6178305044545838731, 39.74863466993041072, 9.382169495545420901 ) ) ;
#15080 = VERTEX_POINT ( 'NONE', #71212 ) ;
#15081 = CARTESIAN_POINT ( 'NONE',  ( 7.361572987183169658, 39.96726448433411605, -9.846743663894592657 ) ) ;
#15082 = CARTESIAN_POINT ( 'NONE',  ( 17.96484262340118221, 6.188685344154837509, -7.964842623401177768 ) ) ;
#15083 = ORIENTED_EDGE ( 'NONE', *, *, #64565, .T. ) ;
#15084 = EDGE_CURVE ( 'NONE', #97132, #16779, #1507, .T. ) ;
#15085 = CARTESIAN_POINT ( 'NONE',  ( 20.88017736071110875, 10.77201867748817143, -2.915334737309920765 ) ) ;
#15086 = ORIENTED_EDGE ( 'NONE', *, *, #52894, .F. ) ;
#15087 = CARTESIAN_POINT ( 'NONE',  ( -0.8801773607111008646, 63.27201867748817676, 2.915334737309923430 ) ) ;
#15088 = CARTESIAN_POINT ( 'NONE',  ( 10.00000000000000178, 59.31368534415484106, 10.88017736071110342 ) ) ;
#15089 = CARTESIAN_POINT ( 'NONE',  ( 15.44008868035555793, 66.39701867748817676, -9.422509992056140149 ) ) ;
#15090 = CARTESIAN_POINT ( 'NONE',  ( 4.559911319644449179, 57.23035201082150536, -9.422509992056141925 ) ) ;
#15091 = CYLINDRICAL_SURFACE ( 'NONE', #69855, 0.5000000000000004441 ) ;
#15093 = VERTEX_POINT ( 'NONE', #78204 ) ;
#15092 = CARTESIAN_POINT ( 'NONE',  ( 8.742110228208591849, -4.148858702914717256, 4.000000000000000000 ) ) ;
#15094 = CARTESIAN_POINT ( 'NONE',  ( 1.472469842513823179, 35.59226448433412315, -4.923371831947296329 ) ) ;
#15095 = EDGE_LOOP ( 'NONE', ( #90786, #69838, #57977, #30280 ) ) ;
#15096 = PLANE ( 'NONE',  #55435 ) ;
#15097 = CARTESIAN_POINT ( 'NONE',  ( -0.3689425029237881626, 7.428748834913967869, 10.36894250292379027 ) ) ;
#15098 = PLANE ( 'NONE',  #88958 ) ;
#15099 = DIRECTION ( 'NONE',  ( 1.000000000000000000, 0.000000000000000000, 0.000000000000000000 ) ) ;
#15100 = CARTESIAN_POINT ( 'NONE',  ( -0.8801773607110991993, 2.855352010821504471, -2.915334737309923874 ) ) ;
#15101 = DIRECTION ( 'NONE',  ( 1.000000000000000000, 2.107602052970794797E-16, -0.000000000000000000 ) ) ;
#15103 = ORIENTED_EDGE ( 'NONE', *, *, #19629, .F. ) ;
#15102 = CARTESIAN_POINT ( 'NONE',  ( 19.38216949554541557, 47.24863466993041783, -9.382169495545420901 ) ) ;
#15104 = PLANE ( 'NONE',  #1759 ) ;
#15105 = CARTESIAN_POINT ( 'NONE',  ( 17.20831665107776587, 49.13393115100078745, -7.208316651077762316 ) ) ;
#15106 = CARTESIAN_POINT ( 'NONE',  ( -2.816281873526473856, 24.33196800326375353, 3.434112377981055619 ) ) ;
#15107 = CARTESIAN_POINT ( 'NONE',  ( 17.20831665107776587, 24.13393115100078035, -7.208316651077762316 ) ) ;
#15108 = CARTESIAN_POINT ( 'NONE',  ( 18.72515096720568195, 26.07228050351032778, -6.500000000000018652 ) ) ;
#15109 = CARTESIAN_POINT ( 'NONE',  ( 5.076628168052703671, 66.84226448433412315, 8.527530157486179263 ) ) ;
#15110 = DIRECTION ( 'NONE',  ( -1.000000000000000000, -0.000000000000000000, -0.000000000000000000 ) ) ;
#15111 = CARTESIAN_POINT ( 'NONE',  ( 2.791683348922237240, 10.38393115100078390, -7.208316651077763204 ) ) ;
#15112 = VECTOR ( 'NONE', #87984, 1000.000000000000114 ) ;
#15113 = ORIENTED_EDGE ( 'NONE', *, *, #29705, .T. ) ;
#15114 =( GEOMETRIC_REPRESENTATION_CONTEXT ( 3 ) GLOBAL_UNCERTAINTY_ASSIGNED_CONTEXT ( ( #6467 ) ) GLOBAL_UNIT_ASSIGNED_CONTEXT ( ( #63702, #93717, #3721 ) ) REPRESENTATION_CONTEXT ( 'NONE', 'WORKASPACE' ) );
#15115 = CARTESIAN_POINT ( 'NONE',  ( 0.5774900079438590739, 17.64701867748817321, -5.440088680355550821 ) ) ;
#15116 = CARTESIAN_POINT ( 'NONE',  ( -0.3689425029237898834, 21.17874883491396432, -10.36894250292378850 ) ) ;
#15117 = CARTESIAN_POINT ( 'NONE',  ( 17.20831665107776587, 27.88393115100078390, 7.208316651077764980 ) ) ;
#15118 = CARTESIAN_POINT ( 'NONE',  ( 10.00000000000000178, 69.31368534415484817, 10.88017736071110342 ) ) ;
#15120 = LINE ( 'NONE', #45596, #87932 ) ;
#15119 = CARTESIAN_POINT ( 'NONE',  ( 6.565887622018943937, 35.16530133659708923, 12.81628187352647430 ) ) ;
#15121 = CARTESIAN_POINT ( 'NONE',  ( 7.084665262690076126, 17.02201867748817676, -10.88017736071110164 ) ) ;
#15122 = AXIS2_PLACEMENT_3D ( 'NONE', #49523, #43505, #72520 ) ;
#15123 = PLANE ( 'NONE',  #98130 ) ;
#15124 = CARTESIAN_POINT ( 'NONE',  ( 13.43411237798106583, 12.66530133659708746, -12.81628187352647252 ) ) ;
#15125 = CARTESIAN_POINT ( 'NONE',  ( 13.43411237798105340, 10.58196800326375353, 12.81628187352647963 ) ) ;
#15126 = CARTESIAN_POINT ( 'NONE',  ( 7.361572987183169658, 29.96726448433411960, -9.846743663894592657 ) ) ;
#15127 = CARTESIAN_POINT ( 'NONE',  ( -9.422509992056145478, -7.352981322511817019, -5.440088680355541939 ) ) ;
#15128 = CARTESIAN_POINT ( 'NONE',  ( 13.43411237798105340, 30.58196800326374998, 12.81628187352647963 ) ) ;
#15129 = DIRECTION ( 'NONE',  ( 0.000000000000000000, -0.000000000000000000, -1.000000000000000000 ) ) ;
#15131 = CARTESIAN_POINT ( 'NONE',  ( 14.48718990079892066, 4.852832169489322230E-16, 0.6093675230841453239 ) ) ;
#15130 = CARTESIAN_POINT ( 'NONE',  ( 2.035157376598824452, 43.68868534415484106, 7.964842623401179544 ) ) ;
#15132 = DIRECTION ( 'NONE',  ( -1.049065152435176504E-16, 1.000000000000000000, -0.000000000000000000 ) ) ;
#15133 = FILL_AREA_STYLE ('',( #23626 ) ) ;
#15134 =( BOUNDED_SURFACE ( )  B_SPLINE_SURFACE ( 1, 2, ( 
 ( #29081, #14097, #60069, #82584, #83579, #90570, #97124, #83080, #22097, #13098, #21604, #29565, #52576, #6587, #38091, #98615, #28095, #91064, #58596, #5614, #98103, #67595, #45074, #66597, #30062, #90078, #44581, #14606, #74585, #97618, #75578, #28595, #75081, #15097, #89096, #68086, #45573, #68579, #36604, #7090, #37592, #60574, #59583, #22592, #53067, #51601, #76067, #20610, #51098, #59084, #81587, #43593, #74080, #36091, #89592, #21102, #82085, #13595, #6099, #92060, #17062, #77536, #69563, #61062, #47040, #9054, #55546, #1578, #85550, #92541, #8075, #86045, #23587, #8566, #91573, #54538, #17558, #110, #31052, #93530, #30556, #69072, #39566, #23090, #53558, #38574, #70055, #84073, #93038, #47544, #25061, #61552, #77054, #48023, #2075, #54053, #32027, #32535, #62531, #24571, #1084, #55031, #78042, #9545, #40047, #608, #78536, #10048, #70547, #15590, #84566, #63033, #39070, #40547, #46073, #31545, #62040, #76560, #16066, #24070, #46555, #85054, #16566, #49499, #26509, #11022, #12493, #57005, #11507, #87993, #33504, #79522, #3536, #95001, #19505, #80002, #56526, #86536, #33996, #63523, #2570, #87508, #41540, #4027, #19020, #64983, #42031, #50494, #94028, #18525, #57498, #64494, #25550, #33026, #41042, #3049, #94514, #48518, #4519, #72495, #79021, #96007, #80508, #72007, #34490, #95508, #27000, #50002, #27490, #56042, #18041, #57983, #10532, #12004, #87015, #71542, #72989, #42507, #64002, #26033, #34983, #65486, #88490, #19992, #80991, #49015, #71047, #51478, #14484, #97995, #81972, #83460, #28962, #82468, #59957, #5503, #13484, #74464, #66977, #90449, #21483, #28484, #58478, #5990, #35486, #73475, #97498, #43962, #74966, #59465, #36975, #89967, #22474, #65982, #89481, #29450, #36485, #96507, #5004, #12979, #73977, #66478, #20494, #75459, #44464, #50982, #67969, #52462, #51981, #13988, #6471, #67475, #21987, #98494, #27980, #88990, #29949, #81477, #82965, #58978, #43476, #44956, #6975, #35976, #97006, #37480, #60454, #90943, #52949, #42992, #20992, #16937, #23471, #85428, #69939, #84451, #75953, #61926, #92427, #70434, #16445, #1459, #8443, #22976, #1951, #7964, #53944, #7480, #69442, #32415, #14981, #45959, #9427, #45452, #83950, #54425, #37977, #68467, #53441, #23952, #98987, #8931, #62412, #39931, #76448, #91940, #62917, #47419, #38462, #84934, #77921, #46923, #77415, #15950, #39448, #31910, #92917, #24447, #15476, #93417, #24940, #55422, #30441, #68954, #54914, #46443, #60940, #91451, #76934, #38950, #486, #30935, #962, #61434, #31422, #95384, #64380, #41430, #25439, #79886, #49385, #4403, #55922, #41915, #2939 ),
 ( #11393, #34374, #80387, #17922, #63885, #42390, #87873, #48406, #56888, #19389, #87391, #26388, #86900, #72378, #18909, #3907, #64863, #86421, #34871, #65365, #57379, #9930, #78909, #26886, #94397, #95895, #11890, #25912, #56414, #40434, #33387, #48893, #2451, #33875, #49874, #94890, #71891, #18410, #27374, #3414, #72869, #85930, #10418, #79406, #10908, #17440, #47907, #78412, #71423, #32907, #70933, #63406, #93911, #40926, #96890, #89847, #13362, #51859, #5869, #37363, #50368, #5388, #44344, #89360, #12374, #19875, #27864, #88871, #81363, #35371, #90329, #59345, #65861, #82843, #67352, #28366, #28842, #58854, #20871, #81848, #14363, #88378, #80876, #44832, #96390, #21364, #43360, #58349, #59839, #82344, #4891, #42880, #66856, #13865, #75337, #6851, #67856, #20377, #21868, #66352, #29338, #74850, #51362, #73363, #36360, #97374, #98375, #6351, #36860, #43847, #50871, #73859, #74341, #97878, #12862, #52346, #57866, #35863, #69825, #16819, #70320, #38346, #84342, #31308, #46329, #68841, #851, #15845, #53326, #92315, #91831, #374, #30324, #83343, #47295, #30821, #29831, #60339, #68351, #23349, #90833, #22853, #83835, #46811, #8332, #62297, #15360, #45845, #61810, #76331, #38835, #77797, #91327, #1347, #31799, #7848, #61320, #76815, #84821, #98869, #69329, #14865, #60826, #23841, #54308, #9307, #53831, #16328, #77303, #8817, #39815, #39331, #85311, #92805, #22360, #24334, #52834, #54794, #45337, #75837, #7357, #37859, #94275, #78796, #63767, #9809, #55805, #1835, #3792, #2823, #56773, #25798, #86299, #79283, #49272, #63284, #40311, #87268, #41791, #56298, #93297, #3291, #48285, #57258, #49752, #10792, #70816, #87754, #17805, #33274, #2332, #86792, #18293, #33755, #48776, #19268, #64259, #32787, #18790, #94772, #85808, #41309, #26271, #79771, #71782, #80263, #72264, #32292, #64747, #62797, #78293, #11271, #34247, #95259, #93790, #26765, #11766, #42275, #24821, #55297, #10304, #17320, #47794, #25319, #40803, #71303, #57748, #12254, #66740, #36244, #90219, #42761, #28734, #88747, #35244, #82724, #5268, #29224, #51745, #21751, #21246, #52232, #5755, #59225, #34752, #97264, #50243, #66233, #50758, #35745, #80759, #27744, #72745, #74729, #73738, #89729, #96768, #58227, #51241, #82228, #65741, #73243, #13742, #44225, #28243, #65241, #74222, #20257, #59724, #14242, #81728, #4770, #4278, #81244, #58738, #96271, #89243, #20751, #6242, #13243, #95767, #36745, #12743, #67236, #97759, #88251, #43735, #27250, #19759, #43242, #24210, #16209, #44724, #8697, #75221, #22240, #15733, #53704, #61687, #83224, #46693, #7736, #68719, #8220, #60709 ) ),
 .UNSPECIFIED., .F., .F., .T. ) 
 B_SPLINE_SURFACE_WITH_KNOTS ( ( 2, 2 ),
 ( 3, 2, 2, 2, 2, 2, 2, 2, 2, 2, 2, 2, 2, 2, 2, 2, 2, 2, 2, 2, 2, 2, 2, 2, 2, 2, 2, 2, 2, 2, 2, 2, 2, 2, 2, 2, 2, 2, 2, 2, 2, 2, 2, 2, 2, 2, 2, 2, 2, 2, 2, 2, 2, 2, 2, 2, 2, 2, 2, 2, 2, 2, 2, 2, 2, 2, 2, 2, 2, 2, 2, 2, 2, 2, 2, 2, 2, 2, 2, 2, 2, 2, 2, 2, 2, 2, 2, 2, 2, 2, 2, 2, 2, 2, 2, 2, 2, 2, 2, 2, 2, 2, 2, 2, 2, 2, 2, 2, 2, 2, 2, 2, 2, 2, 2, 2, 2, 2, 2, 2, 2, 2, 2, 2, 2, 2, 2, 2, 2, 2, 2, 2, 2, 2, 2, 2, 2, 2, 2, 2, 2, 2, 2, 2, 2, 2, 2, 2, 2, 2, 2, 2, 2, 2, 2, 2, 2, 2, 2, 2, 2, 2, 3 ),
 ( 0.000000000000000000, 1.000000000000000000 ),
 ( 0.000000000000000000, 0.005952380952380952051, 0.01190476190476190410, 0.01785714285714285615, 0.02380952380952380820, 0.02976190476190476025, 0.03571428571428571230, 0.04166666666666666435, 0.04761904761904761640, 0.05357142857142856845, 0.05952380952380952051, 0.06547619047619047949, 0.07142857142857142461, 0.07738095238095238360, 0.08333333333333332871, 0.08928571428571428770, 0.09523809523809523281, 0.1011904761904761918, 0.1071428571428571369, 0.1130952380952380959, 0.1190476190476190410, 0.1250000000000000000, 0.1309523809523809590, 0.1369047619047619180, 0.1428571428571428492, 0.1488095238095238082, 0.1547619047619047672, 0.1607142857142857262, 0.1666666666666666574, 0.1726190476190476164, 0.1785714285714285754, 0.1845238095238095344, 0.1904761904761904656, 0.1964285714285714246, 0.2023809523809523836, 0.2083333333333333426, 0.2142857142857142738, 0.2202380952380952328, 0.2261904761904761918, 0.2321428571428571508, 0.2380952380952380820, 0.2440476190476190410, 0.2500000000000000000, 0.2559523809523809312, 0.2619047619047619180, 0.2678571428571428492, 0.2738095238095238360, 0.2797619047619047672, 0.2857142857142856984, 0.2916666666666666852, 0.2976190476190476164, 0.3035714285714285476, 0.3095238095238095344, 0.3154761904761904656, 0.3214285714285714524, 0.3273809523809523836, 0.3333333333333333148, 0.3392857142857143016, 0.3452380952380952328, 0.3511904761904761640, 0.3571428571428571508, 0.3630952380952380820, 0.3690476190476190688, 0.3750000000000000000, 0.3809523809523809312, 0.3869047619047619180, 0.3928571428571428492, 0.3988095238095238360, 0.4047619047619047672, 0.4107142857142856984, 0.4166666666666666852, 0.4226190476190476164, 0.4285714285714285476, 0.4345238095238095344, 0.4404761904761904656, 0.4464285714285714524, 0.4523809523809523836, 0.4583333333333333148, 0.4642857142857143016, 0.4702380952380952328, 0.4761904761904761640, 0.4821428571428571508, 0.4880952380952380820, 0.4940476190476190688, 0.5000000000000000000, 0.5059523809523809312, 0.5119047619047618625, 0.5178571428571429047, 0.5238095238095238360, 0.5297619047619047672, 0.5357142857142856984, 0.5416666666666666297, 0.5476190476190476719, 0.5535714285714286031, 0.5595238095238095344, 0.5654761904761904656, 0.5714285714285713969, 0.5773809523809523281, 0.5833333333333333703, 0.5892857142857143016, 0.5952380952380952328, 0.6011904761904761640, 0.6071428571428570953, 0.6130952380952381375, 0.6190476190476190688, 0.6250000000000000000, 0.6309523809523809312, 0.6369047619047618625, 0.6428571428571429047, 0.6488095238095238360, 0.6547619047619047672, 0.6607142857142856984, 0.6666666666666666297, 0.6726190476190476719, 0.6785714285714286031, 0.6845238095238095344, 0.6904761904761904656, 0.6964285714285713969, 0.7023809523809523281, 0.7083333333333333703, 0.7142857142857143016, 0.7202380952380952328, 0.7261904761904761640, 0.7321428571428570953, 0.7380952380952381375, 0.7440476190476190688, 0.7500000000000000000, 0.7559523809523809312, 0.7619047619047618625, 0.7678571428571429047, 0.7738095238095238360, 0.7797619047619047672, 0.7857142857142856984, 0.7916666666666666297, 0.7976190476190476719, 0.8035714285714286031, 0.8095238095238095344, 0.8154761904761904656, 0.8214285714285713969, 0.8273809523809523281, 0.8333333333333333703, 0.8392857142857143016, 0.8452380952380952328, 0.8511904761904761640, 0.8571428571428570953, 0.8630952380952381375, 0.8690476190476190688, 0.8750000000000000000, 0.8809523809523809312, 0.8869047619047618625, 0.8928571428571429047, 0.8988095238095238360, 0.9047619047619047672, 0.9107142857142856984, 0.9166666666666666297, 0.9226190476190476719, 0.9285714285714286031, 0.9345238095238095344, 0.9404761904761904656, 0.9464285714285713969, 0.9523809523809523281, 0.9583333333333333703, 0.9642857142857143016 ),
 .UNSPECIFIED. ) 
 GEOMETRIC_REPRESENTATION_ITEM ( )  RATIONAL_B_SPLINE_SURFACE ( (
 ( 1.000000000000000000, 0.9659258262890683122, 1.000000000000000000, 0.9659258262890683122, 1.000000000000000000, 0.9659258262890683122, 1.000000000000000000, 0.9659258262890683122, 1.000000000000000000, 0.9659258262890683122, 1.000000000000000000, 0.9659258262890683122, 1.000000000000000000, 0.9659258262890683122, 1.000000000000000000, 0.9659258262890683122, 1.000000000000000000, 0.9659258262890683122, 1.000000000000000000, 0.9659258262890683122, 1.000000000000000000, 0.9659258262890683122, 1.000000000000000000, 0.9659258262890683122, 1.000000000000000000, 0.9659258262890683122, 1.000000000000000000, 0.9659258262890683122, 1.000000000000000000, 0.9659258262890683122, 1.000000000000000000, 0.9659258262890683122, 1.000000000000000000, 0.9659258262890683122, 1.000000000000000000, 0.9659258262890683122, 1.000000000000000000, 0.9659258262890683122, 1.000000000000000000, 0.9659258262890683122, 1.000000000000000000, 0.9659258262890683122, 1.000000000000000000, 0.9659258262890683122, 1.000000000000000000, 0.9659258262890683122, 1.000000000000000000, 0.9659258262890683122, 1.000000000000000000, 0.9659258262890683122, 1.000000000000000000, 0.9659258262890683122, 1.000000000000000000, 0.9659258262890683122, 1.000000000000000000, 0.9659258262890683122, 1.000000000000000000, 0.9659258262890683122, 1.000000000000000000, 0.9659258262890683122, 1.000000000000000000, 0.9659258262890683122, 1.000000000000000000, 0.9659258262890683122, 1.000000000000000000, 0.9659258262890683122, 1.000000000000000000, 0.9659258262890683122, 1.000000000000000000, 0.9659258262890683122, 1.000000000000000000, 0.9659258262890683122, 1.000000000000000000, 0.9659258262890683122, 1.000000000000000000, 0.9659258262890683122, 1.000000000000000000, 0.9659258262890683122, 1.000000000000000000, 0.9659258262890683122, 1.000000000000000000, 0.9659258262890683122, 1.000000000000000000, 0.9659258262890683122, 1.000000000000000000, 0.9659258262890683122, 1.000000000000000000, 0.9659258262890683122, 1.000000000000000000, 0.9659258262890683122, 1.000000000000000000, 0.9659258262890683122, 1.000000000000000000, 0.9659258262890683122, 1.000000000000000000, 0.9659258262890683122, 1.000000000000000000, 0.9659258262890683122, 1.000000000000000000, 0.9659258262890683122, 1.000000000000000000, 0.9659258262890683122, 1.000000000000000000, 0.9659258262890683122, 1.000000000000000000, 0.9659258262890683122, 1.000000000000000000, 0.9659258262890683122, 1.000000000000000000, 0.9659258262890683122, 1.000000000000000000, 0.9659258262890683122, 1.000000000000000000, 0.9659258262890683122, 1.000000000000000000, 0.9659258262890683122, 1.000000000000000000, 0.9659258262890683122, 1.000000000000000000, 0.9659258262890683122, 1.000000000000000000, 0.9659258262890683122, 1.000000000000000000, 0.9659258262890683122, 1.000000000000000000, 0.9659258262890683122, 1.000000000000000000, 0.9659258262890683122, 1.000000000000000000, 0.9659258262890683122, 1.000000000000000000, 0.9659258262890683122, 1.000000000000000000, 0.9659258262890683122, 1.000000000000000000, 0.9659258262890683122, 1.000000000000000000, 0.9659258262890683122, 1.000000000000000000, 0.9659258262890683122, 1.000000000000000000, 0.9659258262890683122, 1.000000000000000000, 0.9659258262890683122, 1.000000000000000000, 0.9659258262890683122, 1.000000000000000000, 0.9659258262890683122, 1.000000000000000000, 0.9659258262890683122, 1.000000000000000000, 0.9659258262890683122, 1.000000000000000000, 0.9659258262890683122, 1.000000000000000000, 0.9659258262890683122, 1.000000000000000000, 0.9659258262890683122, 1.000000000000000000, 0.9659258262890683122, 1.000000000000000000, 0.9659258262890683122, 1.000000000000000000, 0.9659258262890683122, 1.000000000000000000, 0.9659258262890683122, 1.000000000000000000, 0.9659258262890683122, 1.000000000000000000, 0.9659258262890683122, 1.000000000000000000, 0.9659258262890683122, 1.000000000000000000, 0.9659258262890683122, 1.000000000000000000, 0.9659258262890683122, 1.000000000000000000, 0.9659258262890683122, 1.000000000000000000, 0.9659258262890683122, 1.000000000000000000, 0.9659258262890683122, 1.000000000000000000, 0.9659258262890683122, 1.000000000000000000, 0.9659258262890683122, 1.000000000000000000, 0.9659258262890683122, 1.000000000000000000, 0.9659258262890683122, 1.000000000000000000, 0.9659258262890683122, 1.000000000000000000, 0.9659258262890683122, 1.000000000000000000, 0.9659258262890683122, 1.000000000000000000, 0.9659258262890683122, 1.000000000000000000, 0.9659258262890683122, 1.000000000000000000, 0.9659258262890683122, 1.000000000000000000, 0.9659258262890683122, 1.000000000000000000, 0.9659258262890683122, 1.000000000000000000, 0.9659258262890683122, 1.000000000000000000, 0.9659258262890683122, 1.000000000000000000, 0.9659258262890683122, 1.000000000000000000, 0.9659258262890683122, 1.000000000000000000, 0.9659258262890683122, 1.000000000000000000, 0.9659258262890683122, 1.000000000000000000, 0.9659258262890683122, 1.000000000000000000, 0.9659258262890683122, 1.000000000000000000, 0.9659258262890683122, 1.000000000000000000, 0.9659258262890683122, 1.000000000000000000, 0.9659258262890683122, 1.000000000000000000, 0.9659258262890683122, 1.000000000000000000, 0.9659258262890683122, 1.000000000000000000, 0.9659258262890683122, 1.000000000000000000, 0.9659258262890683122, 1.000000000000000000, 0.9659258262890683122, 1.000000000000000000, 0.9659258262890683122, 1.000000000000000000, 0.9659258262890683122, 1.000000000000000000, 0.9659258262890683122, 1.000000000000000000, 0.9659258262890683122, 1.000000000000000000, 0.9659258262890683122, 1.000000000000000000, 0.9659258262890683122, 1.000000000000000000, 0.9659258262890683122, 1.000000000000000000, 0.9659258262890683122, 1.000000000000000000, 0.9659258262890683122, 1.000000000000000000, 0.9659258262890683122, 1.000000000000000000, 0.9659258262890683122, 1.000000000000000000, 0.9659258262890683122, 1.000000000000000000, 0.9659258262890683122, 1.000000000000000000, 0.9659258262890683122, 1.000000000000000000, 0.9659258262890683122, 1.000000000000000000, 0.9659258262890683122, 1.000000000000000000, 0.9659258262890683122, 1.000000000000000000, 0.9659258262890683122, 1.000000000000000000, 0.9659258262890683122, 1.000000000000000000, 0.9659258262890683122, 1.000000000000000000, 0.9659258262890683122, 1.000000000000000000, 0.9659258262890683122, 1.000000000000000000, 0.9659258262890683122, 1.000000000000000000, 0.9659258262890683122, 1.000000000000000000, 0.9659258262890683122, 1.000000000000000000, 0.9659258262890683122, 1.000000000000000000, 0.9659258262890683122, 1.000000000000000000, 0.9659258262890683122, 1.000000000000000000, 0.9659258262890683122, 1.000000000000000000, 0.9659258262890683122, 1.000000000000000000, 0.9659258262890683122, 1.000000000000000000, 0.9659258262890683122, 1.000000000000000000, 0.9659258262890683122, 1.000000000000000000, 0.9659258262890683122, 1.000000000000000000, 0.9659258262890683122, 1.000000000000000000, 0.9659258262890683122, 1.000000000000000000, 0.9659258262890683122, 1.000000000000000000, 0.9659258262890683122, 1.000000000000000000, 0.9659258262890683122, 1.000000000000000000, 0.9659258262890683122, 1.000000000000000000, 0.9659258262890683122, 1.000000000000000000, 0.9659258262890683122, 1.000000000000000000, 0.9659258262890683122, 1.000000000000000000),
 ( 1.000000000000000000, 0.9659258262890683122, 1.000000000000000000, 0.9659258262890683122, 1.000000000000000000, 0.9659258262890683122, 1.000000000000000000, 0.9659258262890683122, 1.000000000000000000, 0.9659258262890683122, 1.000000000000000000, 0.9659258262890683122, 1.000000000000000000, 0.9659258262890683122, 1.000000000000000000, 0.9659258262890683122, 1.000000000000000000, 0.9659258262890683122, 1.000000000000000000, 0.9659258262890683122, 1.000000000000000000, 0.9659258262890683122, 1.000000000000000000, 0.9659258262890683122, 1.000000000000000000, 0.9659258262890683122, 1.000000000000000000, 0.9659258262890683122, 1.000000000000000000, 0.9659258262890683122, 1.000000000000000000, 0.9659258262890683122, 1.000000000000000000, 0.9659258262890683122, 1.000000000000000000, 0.9659258262890683122, 1.000000000000000000, 0.9659258262890683122, 1.000000000000000000, 0.9659258262890683122, 1.000000000000000000, 0.9659258262890683122, 1.000000000000000000, 0.9659258262890683122, 1.000000000000000000, 0.9659258262890683122, 1.000000000000000000, 0.9659258262890683122, 1.000000000000000000, 0.9659258262890683122, 1.000000000000000000, 0.9659258262890683122, 1.000000000000000000, 0.9659258262890683122, 1.000000000000000000, 0.9659258262890683122, 1.000000000000000000, 0.9659258262890683122, 1.000000000000000000, 0.9659258262890683122, 1.000000000000000000, 0.9659258262890683122, 1.000000000000000000, 0.9659258262890683122, 1.000000000000000000, 0.9659258262890683122, 1.000000000000000000, 0.9659258262890683122, 1.000000000000000000, 0.9659258262890683122, 1.000000000000000000, 0.9659258262890683122, 1.000000000000000000, 0.9659258262890683122, 1.000000000000000000, 0.9659258262890683122, 1.000000000000000000, 0.9659258262890683122, 1.000000000000000000, 0.9659258262890683122, 1.000000000000000000, 0.9659258262890683122, 1.000000000000000000, 0.9659258262890683122, 1.000000000000000000, 0.9659258262890683122, 1.000000000000000000, 0.9659258262890683122, 1.000000000000000000, 0.9659258262890683122, 1.000000000000000000, 0.9659258262890683122, 1.000000000000000000, 0.9659258262890683122, 1.000000000000000000, 0.9659258262890683122, 1.000000000000000000, 0.9659258262890683122, 1.000000000000000000, 0.9659258262890683122, 1.000000000000000000, 0.9659258262890683122, 1.000000000000000000, 0.9659258262890683122, 1.000000000000000000, 0.9659258262890683122, 1.000000000000000000, 0.9659258262890683122, 1.000000000000000000, 0.9659258262890683122, 1.000000000000000000, 0.9659258262890683122, 1.000000000000000000, 0.9659258262890683122, 1.000000000000000000, 0.9659258262890683122, 1.000000000000000000, 0.9659258262890683122, 1.000000000000000000, 0.9659258262890683122, 1.000000000000000000, 0.9659258262890683122, 1.000000000000000000, 0.9659258262890683122, 1.000000000000000000, 0.9659258262890683122, 1.000000000000000000, 0.9659258262890683122, 1.000000000000000000, 0.9659258262890683122, 1.000000000000000000, 0.9659258262890683122, 1.000000000000000000, 0.9659258262890683122, 1.000000000000000000, 0.9659258262890683122, 1.000000000000000000, 0.9659258262890683122, 1.000000000000000000, 0.9659258262890683122, 1.000000000000000000, 0.9659258262890683122, 1.000000000000000000, 0.9659258262890683122, 1.000000000000000000, 0.9659258262890683122, 1.000000000000000000, 0.9659258262890683122, 1.000000000000000000, 0.9659258262890683122, 1.000000000000000000, 0.9659258262890683122, 1.000000000000000000, 0.9659258262890683122, 1.000000000000000000, 0.9659258262890683122, 1.000000000000000000, 0.9659258262890683122, 1.000000000000000000, 0.9659258262890683122, 1.000000000000000000, 0.9659258262890683122, 1.000000000000000000, 0.9659258262890683122, 1.000000000000000000, 0.9659258262890683122, 1.000000000000000000, 0.9659258262890683122, 1.000000000000000000, 0.9659258262890683122, 1.000000000000000000, 0.9659258262890683122, 1.000000000000000000, 0.9659258262890683122, 1.000000000000000000, 0.9659258262890683122, 1.000000000000000000, 0.9659258262890683122, 1.000000000000000000, 0.9659258262890683122, 1.000000000000000000, 0.9659258262890683122, 1.000000000000000000, 0.9659258262890683122, 1.000000000000000000, 0.9659258262890683122, 1.000000000000000000, 0.9659258262890683122, 1.000000000000000000, 0.9659258262890683122, 1.000000000000000000, 0.9659258262890683122, 1.000000000000000000, 0.9659258262890683122, 1.000000000000000000, 0.9659258262890683122, 1.000000000000000000, 0.9659258262890683122, 1.000000000000000000, 0.9659258262890683122, 1.000000000000000000, 0.9659258262890683122, 1.000000000000000000, 0.9659258262890683122, 1.000000000000000000, 0.9659258262890683122, 1.000000000000000000, 0.9659258262890683122, 1.000000000000000000, 0.9659258262890683122, 1.000000000000000000, 0.9659258262890683122, 1.000000000000000000, 0.9659258262890683122, 1.000000000000000000, 0.9659258262890683122, 1.000000000000000000, 0.9659258262890683122, 1.000000000000000000, 0.9659258262890683122, 1.000000000000000000, 0.9659258262890683122, 1.000000000000000000, 0.9659258262890683122, 1.000000000000000000, 0.9659258262890683122, 1.000000000000000000, 0.9659258262890683122, 1.000000000000000000, 0.9659258262890683122, 1.000000000000000000, 0.9659258262890683122, 1.000000000000000000, 0.9659258262890683122, 1.000000000000000000, 0.9659258262890683122, 1.000000000000000000, 0.9659258262890683122, 1.000000000000000000, 0.9659258262890683122, 1.000000000000000000, 0.9659258262890683122, 1.000000000000000000, 0.9659258262890683122, 1.000000000000000000, 0.9659258262890683122, 1.000000000000000000, 0.9659258262890683122, 1.000000000000000000, 0.9659258262890683122, 1.000000000000000000, 0.9659258262890683122, 1.000000000000000000, 0.9659258262890683122, 1.000000000000000000, 0.9659258262890683122, 1.000000000000000000, 0.9659258262890683122, 1.000000000000000000, 0.9659258262890683122, 1.000000000000000000, 0.9659258262890683122, 1.000000000000000000, 0.9659258262890683122, 1.000000000000000000, 0.9659258262890683122, 1.000000000000000000, 0.9659258262890683122, 1.000000000000000000, 0.9659258262890683122, 1.000000000000000000, 0.9659258262890683122, 1.000000000000000000, 0.9659258262890683122, 1.000000000000000000, 0.9659258262890683122, 1.000000000000000000, 0.9659258262890683122, 1.000000000000000000, 0.9659258262890683122, 1.000000000000000000, 0.9659258262890683122, 1.000000000000000000, 0.9659258262890683122, 1.000000000000000000, 0.9659258262890683122, 1.000000000000000000, 0.9659258262890683122, 1.000000000000000000, 0.9659258262890683122, 1.000000000000000000, 0.9659258262890683122, 1.000000000000000000, 0.9659258262890683122, 1.000000000000000000, 0.9659258262890683122, 1.000000000000000000, 0.9659258262890683122, 1.000000000000000000, 0.9659258262890683122, 1.000000000000000000, 0.9659258262890683122, 1.000000000000000000, 0.9659258262890683122, 1.000000000000000000, 0.9659258262890683122, 1.000000000000000000, 0.9659258262890683122, 1.000000000000000000, 0.9659258262890683122, 1.000000000000000000, 0.9659258262890683122, 1.000000000000000000, 0.9659258262890683122, 1.000000000000000000, 0.9659258262890683122, 1.000000000000000000, 0.9659258262890683122, 1.000000000000000000, 0.9659258262890683122, 1.000000000000000000, 0.9659258262890683122, 1.000000000000000000, 0.9659258262890683122, 1.000000000000000000) ) ) 
 REPRESENTATION_ITEM ( '' )  SURFACE ( )  );
#15135 = CARTESIAN_POINT ( 'NONE',  ( 19.42250999205614193, 35.14701867748816966, 5.440088680355555262 ) ) ;
#15136 = CARTESIAN_POINT ( 'NONE',  ( 17.96484262340118221, 44.93868534415483396, 7.964842623401181321 ) ) ;
#15137 = CARTESIAN_POINT ( 'NONE',  ( -0.1491070598754174470, 61.94583914210339515, -5.000000000000000000 ) ) ;
#15138 = DIRECTION ( 'NONE',  ( -0.000000000000000000, 1.000000000000000000, -0.000000000000000000 ) ) ;
#15139 = UNCERTAINTY_MEASURE_WITH_UNIT (LENGTH_MEASURE( 1.000000000000000082E-05 ), #11881, 'distance_accuracy_value', 'NONE');
#15140 = CARTESIAN_POINT ( 'NONE',  ( 0.1532563361054082862, 51.21726448433412315, 2.638427012816831674 ) ) ;
#15142 = DIRECTION ( 'NONE',  ( -1.000000000000000000, 0.000000000000000000, 0.000000000000000000 ) ) ;
#15141 = CARTESIAN_POINT ( 'NONE',  ( 19.42250999205614548, 5.980352010821504471, -5.440088680355545492 ) ) ;
#15143 = CARTESIAN_POINT ( 'NONE',  ( 3.591859063236761518, 14.95696800326375531, 11.09922568453594849 ) ) ;
#15144 = ORIENTED_EDGE ( 'NONE', *, *, #77356, .F. ) ;
#15145 = CARTESIAN_POINT ( 'NONE',  ( 20.88017736071110519, 40.56368534415484106, 2.639326808657452039E-16 ) ) ;
#15147 = PRESENTATION_STYLE_ASSIGNMENT (( #44634 ) ) ;
#15146 = CARTESIAN_POINT ( 'NONE',  ( 0.1532563361054082862, 66.21726448433413736, 2.638427012816831674 ) ) ;
#15148 = CARTESIAN_POINT ( 'NONE',  ( 4.559911319644449179, 22.23035201082150536, -9.422509992056141925 ) ) ;
#15149 = CARTESIAN_POINT ( 'NONE',  ( -2.266590686148945544, 37.22041550158063217, 7.082119434687048631 ) ) ;
#15150 = CARTESIAN_POINT ( 'NONE',  ( 12.63842701281683034, 32.46726448433412315, 9.846743663894596210 ) ) ;
#15151 = CARTESIAN_POINT ( 'NONE',  ( 15.44008868035555793, 51.39701867748816966, -9.422509992056140149 ) ) ;
#15152 = CARTESIAN_POINT ( 'NONE',  ( 38.04706783004212411, 44.99999999999999289, 7.000000000000000000 ) ) ;
#15153 = ADVANCED_FACE ( 'NONE', ( #2239 ), #9716, .T. ) ;
#15154 = VECTOR ( 'NONE', #92253, 999.9999999999998863 ) ;
#15155 = CARTESIAN_POINT ( 'NONE',  ( 19.84674366389459621, 58.50893115100078745, 7.409399052514197653E-17 ) ) ;
#15157 = ORIENTED_EDGE ( 'NONE', *, *, #2782, .T. ) ;
#15156 = ADVANCED_FACE ( 'NONE', ( #55713 ), #38687, .F. ) ;
#15158 = ORIENTED_EDGE ( 'NONE', *, *, #9970, .T. ) ;
#15159 = CARTESIAN_POINT ( 'NONE',  ( 24.16423886937409904, 29.09541550158063572, 3.795296366450317205 ) ) ;
#15160 = CARTESIAN_POINT ( 'NONE',  ( 6.204703633549690345, 27.84541550158063217, 14.16423886937410082 ) ) ;
#15161 = CARTESIAN_POINT ( 'NONE',  ( 2.791683348922237240, 0.3839311510007847872, -7.208316651077763204 ) ) ;
#15162 = CARTESIAN_POINT ( 'NONE',  ( 2.917880565312950480, 65.97041550158063217, -12.26659068614894821 ) ) ;
#15163 = CARTESIAN_POINT ( 'NONE',  ( 18.52753015748617571, 53.09226448433412315, 4.923371831947298993 ) ) ;
#15164 = CARTESIAN_POINT ( 'NONE',  ( -10.32520421616337813, -40.46224970679962496, 4.000000000000000000 ) ) ;
#15166 = CARTESIAN_POINT ( 'NONE',  ( 22.81628187352647785, 21.62363466993041783, 6.195893100308588602E-16 ) ) ;
#15165 = CARTESIAN_POINT ( 'NONE',  ( 20.88017736071110519, 40.56368534415484106, 2.639326808657452039E-16 ) ) ;
#15167 = CARTESIAN_POINT ( 'NONE',  ( 22.26659068614895176, 14.72041550158063572, -7.082119434687042414 ) ) ;
#15168 = CARTESIAN_POINT ( 'NONE',  ( -0.8801773607110991993, 7.855352010821506248, -2.915334737309923874 ) ) ;
#15169 = EDGE_CURVE ( 'NONE', #6847, #85540, #17242, .T. ) ;
#15170 = CARTESIAN_POINT ( 'NONE',  ( 7.084665262690076126, 34.10535201082151247, 10.88017736071109987 ) ) ;
#15171 = FACE_OUTER_BOUND ( 'NONE', #47847, .T. ) ;
#15172 = CARTESIAN_POINT ( 'NONE',  ( 19.42250999205614193, 55.14701867748817676, 5.440088680355555262 ) ) ;
#15173 = CARTESIAN_POINT ( 'NONE',  ( 21.09922568453594849, 51.20696800326375353, 6.408140936763242479 ) ) ;
#15174 = CARTESIAN_POINT ( 'NONE',  ( 9.846743663894590881, -21.28273551566588395, -2.638427012816833894 ) ) ;
#15175 = ORIENTED_EDGE ( 'NONE', *, *, #81721, .T. ) ;
#15176 = CARTESIAN_POINT ( 'NONE',  ( -8.000000000000000000, 41.24999999999999289, 6.500000000000000888 ) ) ;
#15177 = VECTOR ( 'NONE', #10841, 1000.000000000000000 ) ;
#15178 = VERTEX_POINT ( 'NONE', #80669 ) ;
#15179 = DIRECTION ( 'NONE',  ( 0.000000000000000000, 0.000000000000000000, -1.000000000000000000 ) ) ;
#15180 = EDGE_LOOP ( 'NONE', ( #78896, #4154, #35824, #1052 ) ) ;
#15181 = DIRECTION ( 'NONE',  ( -0.9762960071199346945, 0.000000000000000000, 0.2164396139380971307 ) ) ;
#15183 = CARTESIAN_POINT ( 'NONE',  ( 24.16423886937409904, 59.09541550158063217, 3.795296366450317205 ) ) ;
#15182 = CARTESIAN_POINT ( 'NONE',  ( -2.266590686148945544, 56.38708216824731068, -7.082119434687050408 ) ) ;
#15185 = CARTESIAN_POINT ( 'NONE',  ( 10.00000000000000178, 57.25893115100078745, 9.846743663894594434 ) ) ;
#15184 = CARTESIAN_POINT ( 'NONE',  ( 7.361572987183170547, 27.05059781766745175, 9.846743663894590881 ) ) ;
#15186 = CARTESIAN_POINT ( 'NONE',  ( -0.8801773607111008646, 68.27201867748817676, 2.915334737309923430 ) ) ;
#15187 = CARTESIAN_POINT ( 'NONE',  ( -12.81628187352647608, 24.12363466993042138, 3.903127820947815962E-15 ) ) ;
#15188 = ORIENTED_EDGE ( 'NONE', *, *, #25103, .T. ) ;
#15189 = CARTESIAN_POINT ( 'NONE',  ( 10.00000000000000178, 33.05374883491396787, 14.16423886937410082 ) ) ;
#15190 = EDGE_CURVE ( 'NONE', #49358, #10984, #49658, .T. ) ;
#15191 = CARTESIAN_POINT ( 'NONE',  ( 22.26659068614894466, 43.88708216824729647, 7.082119434687054849 ) ) ;
#15192 = ORIENTED_EDGE ( 'NONE', *, *, #80003, .T. ) ;
#15193 = CARTESIAN_POINT ( 'NONE',  ( 19.38216949554541557, 57.24863466993042493, -9.382169495545420901 ) ) ;
#15194 = CARTESIAN_POINT ( 'NONE',  ( 4.559911319644449179, 22.23035201082150536, -9.422509992056141925 ) ) ;
#15195 = CARTESIAN_POINT ( 'NONE',  ( 14.92337183194729988, 54.34226448433412315, -8.527530157486177487 ) ) ;
#15196 = CARTESIAN_POINT ( 'NONE',  ( 20.88017736071110519, 25.56368534415483751, 2.639326808657452039E-16 ) ) ;
#15197 = CARTESIAN_POINT ( 'NONE',  ( 19.38216949554541202, 60.99863466993042493, 9.382169495545424454 ) ) ;
#15198 = DIRECTION ( 'NONE',  ( 0.000000000000000000, -0.000000000000000000, 1.000000000000000000 ) ) ;
#15199 = CARTESIAN_POINT ( 'NONE',  ( 12.63842701281683922, 59.55059781766744464, -9.846743663894590881 ) ) ;
#15200 = CARTESIAN_POINT ( 'NONE',  ( 0.1532563361054100626, 45.80059781766745886, -2.638427012816831230 ) ) ;
#15201 = ADVANCED_FACE ( 'NONE', ( #12655 ), #35221, .T. ) ;
#15202 =( BOUNDED_CURVE ( )  B_SPLINE_CURVE ( 2, ( #40185, #4161, #43127, #51124, #65622, #96148, #82111, #42642, #12627 ),
 .UNSPECIFIED., .F., .F. ) 
 B_SPLINE_CURVE_WITH_KNOTS ( ( 3, 2, 2, 2, 3 ),
 ( 0.1544266512259456492, 0.1547619047619047672, 0.1607142857142856984, 0.1666666666666666297, 0.1670019202026257477 ),
 .UNSPECIFIED. ) 
 CURVE ( )  GEOMETRIC_REPRESENTATION_ITEM ( )  RATIONAL_B_SPLINE_CURVE ( ( 0.9963778908391762723, 0.9980808541467921513, 1.000000000000000000, 0.9659258262890682012, 1.000000000000000000, 0.9659258262890682012, 1.000000000000000000, 0.9980808541467922623, 0.9963778908391763833 ) ) 
 REPRESENTATION_ITEM ( '' )  );
#15204 = ORIENTED_EDGE ( 'NONE', *, *, #55912, .F. ) ;
#15203 = CARTESIAN_POINT ( 'NONE',  ( 12.98685442714775640, 15.00000000000000000, 6.449155920607609893 ) ) ;
#15205 = VECTOR ( 'NONE', #20483, 1000.000000000000000 ) ;
#15206 = DIRECTION ( 'NONE',  ( 0.000000000000000000, -0.000000000000000000, -1.000000000000000000 ) ) ;
#15207 = CARTESIAN_POINT ( 'NONE',  ( 19.84674366389459621, 8.508931151000785675, 7.409399052514197653E-17 ) ) ;
#15208 = CARTESIAN_POINT ( 'NONE',  ( -8.721827932831688557, -2.980708941387882104E-15, -11.74045266257187592 ) ) ;
#15209 = ORIENTED_EDGE ( 'NONE', *, *, #66706, .T. ) ;
#15210 = FILL_AREA_STYLE_COLOUR ( '', #97275 ) ;
#15211 = CARTESIAN_POINT ( 'NONE',  ( 19.84674366389459266, 28.71726448433411960, -2.638427012816827677 ) ) ;
#15212 = CARTESIAN_POINT ( 'NONE',  ( -18.00000000000000355, 75.73428692542562146, 3.000000000000000000 ) ) ;
#15213 = CARTESIAN_POINT ( 'NONE',  ( 0.6178305044545818747, 33.49863466993042493, -9.382169495545419124 ) ) ;
#15214 = DIRECTION ( 'NONE',  ( 0.000000000000000000, -1.000000000000000000, 0.000000000000000000 ) ) ;
#15215 = CARTESIAN_POINT ( 'NONE',  ( 0.000000000000000000, 0.5000000000000004441, 0.000000000000000000 ) ) ;
#15216 = ORIENTED_EDGE ( 'NONE', *, *, #53671, .T. ) ;
#15217 = CARTESIAN_POINT ( 'NONE',  ( 0.000000000000000000, 15.00000000000000000, 0.000000000000000000 ) ) ;
#15218 = CARTESIAN_POINT ( 'NONE',  ( -33.19000000000001194, 92.00000000000000000, 9.500000000000000000 ) ) ;
#15219 = CARTESIAN_POINT ( 'NONE',  ( 17.20831665107776587, 42.88393115100077324, 7.208316651077764980 ) ) ;
#15220 = CARTESIAN_POINT ( 'NONE',  ( 13.79529636645031943, 35.34541550158063927, -14.16423886937409904 ) ) ;
#15221 = CARTESIAN_POINT ( 'NONE',  ( 19.84674366389459266, 58.71726448433411605, -2.638427012816827677 ) ) ;
#15222 = DIRECTION ( 'NONE',  ( -0.7604059656000257128, 0.000000000000000000, -0.6494480483301898754 ) ) ;
#15223 = CARTESIAN_POINT ( 'NONE',  ( 5.076628168052703671, 6.842264484334118713, 8.527530157486179263 ) ) ;
#15224 =( NAMED_UNIT ( * ) SI_UNIT ( $, .STERADIAN. ) SOLID_ANGLE_UNIT ( ) );
#15225 = TOROIDAL_SURFACE ( 'NONE', #82287, 14.49999999999999822, 0.5000000000000000000 ) ;
#15226 = CARTESIAN_POINT ( 'NONE',  ( 7.361572987183170547, 47.05059781766745175, 9.846743663894590881 ) ) ;
#15227 = CARTESIAN_POINT ( 'NONE',  ( 10.00000000000000000, 51.81368534415484106, -10.88017736071110342 ) ) ;
#15228 = CARTESIAN_POINT ( 'NONE',  ( 5.076628168052704559, 45.17559781766745175, -8.527530157486179263 ) ) ;
#15229 = ITEM_DEFINED_TRANSFORMATION ( 'NONE', 'NONE', #39160,  #27931 ) ;
#15230 = FACE_OUTER_BOUND ( 'NONE', #15484, .T. ) ;
#15231 = AXIS2_PLACEMENT_3D ( 'NONE', #13761, #20277, #90240 ) ;
#15232 = CARTESIAN_POINT ( 'NONE',  ( 20.88017736071110875, 45.77201867748816966, -2.915334737309920765 ) ) ;
#15233 = VERTEX_POINT ( 'NONE', #63586 ) ;
#15234 = CARTESIAN_POINT ( 'NONE',  ( 0.000000000000000000, 14.49999999999999822, 0.000000000000000000 ) ) ;
#15235 = CARTESIAN_POINT ( 'NONE',  ( 2.035157376598824452, 33.68868534415484106, 7.964842623401179544 ) ) ;
#15237 = CARTESIAN_POINT ( 'NONE',  ( -0.8801773607111008646, 53.27201867748816966, 2.915334737309923430 ) ) ;
#15236 = CARTESIAN_POINT ( 'NONE',  ( 10.00000000000000178, 67.25893115100079456, 9.846743663894594434 ) ) ;
#15238 = DIRECTION ( 'NONE',  ( 0.3826834323650877834, -0.000000000000000000, 0.9238795325112876267 ) ) ;
#15239 = B_SPLINE_CURVE_WITH_KNOTS ( 'NONE', 3,
 ( #1854, #47811, #78311, #57280, #72279, #11292 ),
 .UNSPECIFIED., .F., .F.,
 ( 4, 2, 4 ),
 ( 3.409110551496119171E-05, 0.0004400426677367866800, 0.0008459942299586122429 ),
 .UNSPECIFIED. ) ;
#15240 = LINE ( 'NONE', #23728, #23624 ) ;
#15241 = CARTESIAN_POINT ( 'NONE',  ( -46.43608953664445949, 103.5215118185570589, -6.243227838361740112 ) ) ;
#15242 = B_SPLINE_CURVE_WITH_KNOTS ( 'NONE', 3,
 ( #79081, #29025, #97073, #43059, #82034, #52524, #59532, #66545, #28546, #21054, #6052, #67541, #59038, #14048, #50555, #51545, #98055, #27549, #36550, #13545, #20558, #67040, #44530, #35551, #14547, #45018, #37043 ),
 .UNSPECIFIED., .F., .F.,
 ( 4, 2, 2, 2, 1, 2, 2, 2, 2, 2, 2, 2, 2, 4 ),
 ( -6.000000001272176776E-08, 0.0007750911056877003409, 0.001550242211375413553, 0.003100544422750839760, 0.006201148845501692174, 0.01240235769100339613, 0.02480477538200680579, 0.03720719307301021544, 0.04960961076401360775, 0.07441444614602037155, 0.08681686383702374998, 0.09301807268252543226, 0.09611867710527627340, 0.09921928152802711454 ),
 .UNSPECIFIED. ) ;
#15244 = CARTESIAN_POINT ( 'NONE',  ( -7.750000000000000000, 79.82179676972448590, -4.250000000000000000 ) ) ;
#15243 = CARTESIAN_POINT ( 'NONE',  ( 19.42250999205614548, 40.98035201082150536, -5.440088680355545492 ) ) ;
#15245 = CARTESIAN_POINT ( 'NONE',  ( 14.92337183194729988, 9.342264484334119601, -8.527530157486177487 ) ) ;
#15246 = EDGE_CURVE ( 'NONE', #50110, #51389, #17623, .T. ) ;
#15247 = VECTOR ( 'NONE', #57980, 1000.000000000000114 ) ;
#15248 = CARTESIAN_POINT ( 'NONE',  ( 19.84674366389459266, 33.71726448433410894, -2.638427012816827677 ) ) ;
#15249 = CARTESIAN_POINT ( 'NONE',  ( -1.780824192092602010, 14.63595249122789177, 14.89391369643512952 ) ) ;
#15250 = CARTESIAN_POINT ( 'NONE',  ( -12.26659068614894110, 17.22041550158065348, 7.082119434687058401 ) ) ;
#15251 = CARTESIAN_POINT ( 'NONE',  ( 6.565887622018943937, -1.918031996736246692, -12.81628187352647608 ) ) ;
#15252 = CARTESIAN_POINT ( 'NONE',  ( 19.42250999205614193, 5.147018677488171434, 5.440088680355555262 ) ) ;
#15253 = DIRECTION ( 'NONE',  ( -0.9099612708765455471, 0.000000000000000000, 0.4146932426562339180 ) ) ;
#15254 = EDGE_CURVE ( 'NONE', #4847, #54861, #34763, .T. ) ;
#15255 = CARTESIAN_POINT ( 'NONE',  ( 22.26659068614894466, 18.88708216824730002, 7.082119434687054849 ) ) ;
#15256 = CARTESIAN_POINT ( 'NONE',  ( 20.36894250292379738, 44.92874883491396787, -10.36894250292379027 ) ) ;
#15257 = CARTESIAN_POINT ( 'NONE',  ( 2.791683348922237240, 15.38393115100078212, -7.208316651077763204 ) ) ;
#15258 = ORIENTED_EDGE ( 'NONE', *, *, #95193, .T. ) ;
#15259 = CARTESIAN_POINT ( 'NONE',  ( 17.20831665107776587, 22.88393115100078745, 7.208316651077764980 ) ) ;
#15260 = CARTESIAN_POINT ( 'NONE',  ( 20.88017736071110519, 25.56368534415483751, 2.639326808657452039E-16 ) ) ;
#15261 = CARTESIAN_POINT ( 'NONE',  ( 12.63842701281683922, 49.55059781766744464, -9.846743663894590881 ) ) ;
#15263 = DIRECTION ( 'NONE',  ( -0.000000000000000000, -1.000000000000000000, -0.000000000000000000 ) ) ;
#15262 = CARTESIAN_POINT ( 'NONE',  ( 13.79529636645030344, 13.26208216824729824, 14.16423886937410614 ) ) ;
#15264 = CARTESIAN_POINT ( 'NONE',  ( -8.924603092375777535, 75.06466731010172566, 3.000000000000000000 ) ) ;
#15265 = VECTOR ( 'NONE', #45487, 1000.000000000000000 ) ;
#15266 = CARTESIAN_POINT ( 'NONE',  ( 18.52753015748617571, 13.09226448433411960, 4.923371831947298993 ) ) ;
#15267 = CARTESIAN_POINT ( 'NONE',  ( -1.099225684535947600, 33.70696800326375353, -6.408140936763238038 ) ) ;
#15268 = CARTESIAN_POINT ( 'NONE',  ( 18.52753015748617571, 43.09226448433412315, 4.923371831947298993 ) ) ;
#15269 = ORIENTED_EDGE ( 'NONE', *, *, #84673, .F. ) ;
#15270 = CARTESIAN_POINT ( 'NONE',  ( 10.00000000000000178, 27.25893115100078390, 9.846743663894594434 ) ) ;
#15271 = CARTESIAN_POINT ( 'NONE',  ( 10.47193227291256790, -40.28585825689869893, -4.000000000000000000 ) ) ;
#15272 = CARTESIAN_POINT ( 'NONE',  ( 0.8801356535991349261, 124.4373638429518962, 4.500000000000000888 ) ) ;
#15273 = CARTESIAN_POINT ( 'NONE',  ( 22.26659068614895176, 49.72041550158063927, -7.082119434687042414 ) ) ;
#15274 = CARTESIAN_POINT ( 'NONE',  ( 17.96484262340118221, 56.18868534415484817, -7.964842623401177768 ) ) ;
#15275 = CARTESIAN_POINT ( 'NONE',  ( -11.96291822454887033, 4.341775326899288507E-16, 8.193813980848993594 ) ) ;
#15276 = SURFACE_SIDE_STYLE ('',( #98790 ) ) ;
#15277 = CARTESIAN_POINT ( 'NONE',  ( 12.63842701281683034, 32.46726448433412315, 9.846743663894596210 ) ) ;
#15278 = CARTESIAN_POINT ( 'NONE',  ( 17.96484262340118221, 4.938685344154837509, 7.964842623401181321 ) ) ;
#15279 = CARTESIAN_POINT ( 'NONE',  ( 17.20831665107776587, 42.88393115100077324, 7.208316651077764980 ) ) ;
#15280 = FILL_AREA_STYLE_COLOUR ( '', #11240 ) ;
#15281 = CARTESIAN_POINT ( 'NONE',  ( 10.00000000000000000, 44.75893115100078745, -9.846743663894594434 ) ) ;
#15282 = CARTESIAN_POINT ( 'NONE',  ( 17.96484262340118221, 54.93868534415484106, 7.964842623401181321 ) ) ;
#15284 = VERTEX_POINT ( 'NONE', #19085 ) ;
#15283 = EDGE_CURVE ( 'NONE', #56877, #59079, #90662, .T. ) ;
#15285 = VERTEX_POINT ( 'NONE', #64069 ) ;
#15286 = CARTESIAN_POINT ( 'NONE',  ( 6.565887622018943937, 53.08196800326374643, -12.81628187352647608 ) ) ;
#15287 = AXIS2_PLACEMENT_3D ( 'NONE', #55685, #92688, #71668 ) ;
#15288 = CARTESIAN_POINT ( 'NONE',  ( 19.84674366389459266, 3.300597817667451750, 2.638427012816836559 ) ) ;
#15289 = CARTESIAN_POINT ( 'NONE',  ( 22.81628187352647785, 51.41530133659708923, 3.434112377981063169 ) ) ;
#15291 = CARTESIAN_POINT ( 'NONE',  ( 10.00000000000000000, 49.75893115100078745, -9.846743663894594434 ) ) ;
#15290 = CARTESIAN_POINT ( 'NONE',  ( -0.8801773607110991993, 7.855352010821506248, -2.915334737309923874 ) ) ;
#15292 = CARTESIAN_POINT ( 'NONE',  ( -18.89999999999999147, 99.99999999999998579, -7.750000000000000000 ) ) ;
#15293 = CARTESIAN_POINT ( 'NONE',  ( 17.08211943468705840, 30.13708216824730357, -12.26659068614894466 ) ) ;
#15294 = EDGE_CURVE ( 'NONE', #32092, #96723, #89089, .T. ) ;
#15295 = CARTESIAN_POINT ( 'NONE',  ( 10.00000000000000178, 63.05374883491396076, 14.16423886937410082 ) ) ;
#15296 = CARTESIAN_POINT ( 'NONE',  ( 0.1532563361054100626, 60.80059781766744464, -2.638427012816831230 ) ) ;
#15297 = CARTESIAN_POINT ( 'NONE',  ( 19.42250999205614193, 55.14701867748817676, 5.440088680355555262 ) ) ;
#15298 = CARTESIAN_POINT ( 'NONE',  ( 18.52753015748618282, 8.925597817667451750, -4.923371831947291888 ) ) ;
#15299 = CARTESIAN_POINT ( 'NONE',  ( -3.750000000000000888, 1.019547802438453887, 4.000000000000000000 ) ) ;
#15300 = ORIENTED_EDGE ( 'NONE', *, *, #61757, .T. ) ;
#15301 = CARTESIAN_POINT ( 'NONE',  ( 3.591859063236763294, 53.29030133659708923, -11.09922568453595026 ) ) ;
#15302 = ORIENTED_EDGE ( 'NONE', *, *, #33284, .T. ) ;
#15303 = CARTESIAN_POINT ( 'NONE',  ( 10.00000000000000000, 9.758931151000785675, -9.846743663894594434 ) ) ;
#15304 = ORIENTED_EDGE ( 'NONE', *, *, #76212, .F. ) ;
#15305 = CARTESIAN_POINT ( 'NONE',  ( -2.266590686148945544, 21.38708216824730357, -7.082119434687050408 ) ) ;
#15306 = CARTESIAN_POINT ( 'NONE',  ( 18.52753015748618282, 18.92559781766745175, -4.923371831947291888 ) ) ;
#15307 = CARTESIAN_POINT ( 'NONE',  ( 17.96484262340118221, 24.93868534415484461, 7.964842623401181321 ) ) ;
#15308 = CARTESIAN_POINT ( 'NONE',  ( 7.109031286574768238, 0.04962885628204084798, 12.92745085449643128 ) ) ;
#15309 = ORIENTED_EDGE ( 'NONE', *, *, #73045, .T. ) ;
#15310 = CARTESIAN_POINT ( 'NONE',  ( 20.88017736071110875, 30.77201867748816966, -2.915334737309920765 ) ) ;
#15311 = CIRCLE ( 'NONE', #56613, 0.2500000000000002220 ) ;
#15312 = EDGE_CURVE ( 'NONE', #63974, #58305, #61892, .T. ) ;
#15313 = ORIENTED_EDGE ( 'NONE', *, *, #88300, .F. ) ;
#15314 = CARTESIAN_POINT ( 'NONE',  ( 4.559911319644449179, 33.89701867748817676, 9.422509992056141925 ) ) ;
#15315 = CARTESIAN_POINT ( 'NONE',  ( 1.472469842513823179, 66.42559781766745175, 4.923371831947296329 ) ) ;
#15316 = ORIENTED_EDGE ( 'NONE', *, *, #94125, .F. ) ;
#15317 = EDGE_CURVE ( 'NONE', #27101, #32140, #29991, .T. ) ;
#15318 = VERTEX_POINT ( 'NONE', #73546 ) ;
#15319 = CARTESIAN_POINT ( 'NONE',  ( 3.591859063236761518, 14.95696800326375531, 11.09922568453594849 ) ) ;
#15320 = CARTESIAN_POINT ( 'NONE',  ( -4.250000000000000000, 0.000000000000000000, -3.750000000000000000 ) ) ;
#15321 = CARTESIAN_POINT ( 'NONE',  ( 0.1532563361054083140, 6.008931151000784787, 1.131784320476157264E-15 ) ) ;
#15322 = DIRECTION ( 'NONE',  ( 1.000000000000000000, -0.000000000000000000, -0.000000000000000000 ) ) ;
#15323 = CARTESIAN_POINT ( 'NONE',  ( 20.03743638938530225, 6.751975280310174021, 6.399506433553884932 ) ) ;
#15324 = CARTESIAN_POINT ( 'NONE',  ( 14.92337183194729633, 12.67559781766745353, 8.527530157486181039 ) ) ;
#15325 = CARTESIAN_POINT ( 'NONE',  ( -0.8801773607110991993, 27.85535201082150181, -2.915334737309923874 ) ) ;
#15326 = VECTOR ( 'NONE', #93095, 999.9999999999998863 ) ;
#15328 = VERTEX_POINT ( 'NONE', #56595 ) ;
#15327 = VECTOR ( 'NONE', #43308, 999.9999999999998863 ) ;
#15329 = ORIENTED_EDGE ( 'NONE', *, *, #15680, .T. ) ;
#15330 = CARTESIAN_POINT ( 'NONE',  ( -2.816281873526473856, 64.12363466993042493, 9.499525473075851096E-16 ) ) ;
#15331 = CARTESIAN_POINT ( 'NONE',  ( 2.035157376598822676, 57.43868534415484106, -7.964842623401177768 ) ) ;
#15332 = FACE_OUTER_BOUND ( 'NONE', #79308, .T. ) ;
#15333 = CIRCLE ( 'NONE', #4181, 0.2500000000000002220 ) ;
#15334 = CARTESIAN_POINT ( 'NONE',  ( 0.6178305044545818747, 58.49863466993042493, -9.382169495545419124 ) ) ;
#15335 = CARTESIAN_POINT ( 'NONE',  ( 7.084665262690076126, 64.10535201082150536, 10.88017736071109987 ) ) ;
#15336 = CARTESIAN_POINT ( 'NONE',  ( 2.791683348922237240, 65.38393115100078035, -7.208316651077763204 ) ) ;
#15337 = LINE ( 'NONE', #38320, #47943 ) ;
#15338 = CARTESIAN_POINT ( 'NONE',  ( 19.84674366389459266, 28.71726448433411960, -2.638427012816827677 ) ) ;
#15339 = CARTESIAN_POINT ( 'NONE',  ( 19.38216949554541202, 55.99863466993041072, 9.382169495545424454 ) ) ;
#15340 = LINE ( 'NONE', #68327, #96044 ) ;
#15341 = CARTESIAN_POINT ( 'NONE',  ( 2.791683348922240793, 6.633931151000785675, 7.208316651077764092 ) ) ;
#15342 = CARTESIAN_POINT ( 'NONE',  ( 6.565887622018943937, 25.16530133659708213, 12.81628187352647430 ) ) ;
#15344 = CARTESIAN_POINT ( 'NONE',  ( -42.16485527613927076, 107.5383484153110061, 4.500000000000000888 ) ) ;
#15343 = CARTESIAN_POINT ( 'NONE',  ( -46.56032276184168950, 103.8061269828102837, 5.692785089662784515 ) ) ;
#15345 = CARTESIAN_POINT ( 'NONE',  ( 0.5774900079438607392, 33.48035201082150536, 5.440088680355550821 ) ) ;
#15346 = CARTESIAN_POINT ( 'NONE',  ( -2.816281873526473856, -0.6680319967362464695, 3.434112377981055619 ) ) ;
#15347 = CARTESIAN_POINT ( 'NONE',  ( 1.472469842513823179, 20.59226448433411960, -4.923371831947296329 ) ) ;
#15348 = CARTESIAN_POINT ( 'NONE',  ( 1.472469842513823179, 6.425597817667451750, 4.923371831947296329 ) ) ;
#15349 = CARTESIAN_POINT ( 'NONE',  ( 19.42250999205614193, 15.14701867748817143, 5.440088680355555262 ) ) ;
#15351 = ORIENTED_EDGE ( 'NONE', *, *, #54980, .F. ) ;
#15350 = CARTESIAN_POINT ( 'NONE',  ( 16.40814093676324603, 12.45696800326375353, -11.09922568453594671 ) ) ;
#15352 = DIRECTION ( 'NONE',  ( 0.9990482215818582423, 0.000000000000000000, -0.04361938736532634114 ) ) ;
#15353 = VECTOR ( 'NONE', #28623, 999.9999999999998863 ) ;
#15354 = CARTESIAN_POINT ( 'NONE',  ( 5.783743716939243384, -36.05632648146325181, -2.499999999999999112 ) ) ;
#15355 = CARTESIAN_POINT ( 'NONE',  ( 19.42250999205614193, 10.14701867748816966, 5.440088680355555262 ) ) ;
#15356 = CARTESIAN_POINT ( 'NONE',  ( 19.84674366389459266, 43.30059781766744464, 2.638427012816836559 ) ) ;
#15357 = ORIENTED_EDGE ( 'NONE', *, *, #20916, .T. ) ;
#15358 = CARTESIAN_POINT ( 'NONE',  ( 0.000000000000000000, 80.32179676972448590, -4.250000000000000000 ) ) ;
#15359 = CARTESIAN_POINT ( 'NONE',  ( -4.164238869374099039, 66.80374883491396076, 8.674139862899312516E-16 ) ) ;
#15360 = CARTESIAN_POINT ( 'NONE',  ( 4.559911319644449179, 32.23035201082150536, -9.422509992056141925 ) ) ;
#15362 = CARTESIAN_POINT ( 'NONE',  ( 11.22915323889574601, 0.000000000000000000, 8.773176023390684364 ) ) ;
#15361 = CARTESIAN_POINT ( 'NONE',  ( 20.36894250292379738, 59.92874883491397497, -10.36894250292379027 ) ) ;
#15363 = CARTESIAN_POINT ( 'NONE',  ( 12.63842701281683034, 7.467264484334118713, 9.846743663894596210 ) ) ;
#15364 = CARTESIAN_POINT ( 'NONE',  ( 10.00000000000000178, 22.25893115100078745, 9.846743663894594434 ) ) ;
#15365 = CARTESIAN_POINT ( 'NONE',  ( 13.43411237798106583, 7.665301336597086568, -12.81628187352647252 ) ) ;
#15366 = CARTESIAN_POINT ( 'NONE',  ( -46.48622585131851537, 103.4028339409962172, 6.319095158313501770 ) ) ;
#15367 = VECTOR ( 'NONE', #1619, 1000.000000000000000 ) ;
#15368 = CARTESIAN_POINT ( 'NONE',  ( 6.761335002693093621, 0.2301500669213601691, -13.32315948060037059 ) ) ;
#15369 = ADVANCED_FACE ( 'NONE', ( #35559 ), #86603, .F. ) ;
#15370 = DIRECTION ( 'NONE',  ( 0.06975647374412535795, 0.9975640502598243087, -0.000000000000000000 ) ) ;
#15371 =( NAMED_UNIT ( * ) SI_UNIT ( $, .STERADIAN. ) SOLID_ANGLE_UNIT ( ) );
#15372 = CARTESIAN_POINT ( 'NONE',  ( -0.3689425029237898834, 16.17874883491396076, -10.36894250292378850 ) ) ;
#15373 = CARTESIAN_POINT ( 'NONE',  ( 10.00000000000000178, 27.25893115100078390, 9.846743663894594434 ) ) ;
#15374 = FILL_AREA_STYLE ('',( #23362 ) ) ;
#15375 = VERTEX_POINT ( 'NONE', #73056 ) ;
#15376 = CARTESIAN_POINT ( 'NONE',  ( 13.79529636645030344, 53.26208216824730357, 14.16423886937410614 ) ) ;
#15377 = CARTESIAN_POINT ( 'NONE',  ( 10.00000000000000000, 4.758931151000784787, -9.846743663894594434 ) ) ;
#15378 = CARTESIAN_POINT ( 'NONE',  ( 2.035157376598824452, 38.68868534415483396, 7.964842623401179544 ) ) ;
#15379 = CARTESIAN_POINT ( 'NONE',  ( 3.591859063236763294, 48.29030133659708923, -11.09922568453595026 ) ) ;
#15380 = CARTESIAN_POINT ( 'NONE',  ( -0.8801773607110991993, 12.85535201082150358, -2.915334737309923874 ) ) ;
#15381 = CARTESIAN_POINT ( 'NONE',  ( 19.38216949554541202, 50.99863466993042493, 9.382169495545424454 ) ) ;
#15382 = CARTESIAN_POINT ( 'NONE',  ( 5.076628168052703671, 61.84226448433412315, 8.527530157486179263 ) ) ;
#15383 = SURFACE_STYLE_USAGE ( .BOTH. , #22385 ) ;
#15384 = ORIENTED_EDGE ( 'NONE', *, *, #72713, .F. ) ;
#15385 = CARTESIAN_POINT ( 'NONE',  ( 1.383448333479229797, 12.37718327197428536, -6.499999999999972466 ) ) ;
#15386 = CARTESIAN_POINT ( 'NONE',  ( 11.62112565934141095, 15.00000000000000711, 8.881879596174812264 ) ) ;
#15387 = CARTESIAN_POINT ( 'NONE',  ( 17.08211943468705840, 45.13708216824730357, -12.26659068614894466 ) ) ;
#15388 = CARTESIAN_POINT ( 'NONE',  ( 10.00000000000000000, 20.55374883491396787, -14.16423886937410082 ) ) ;
#15389 = CARTESIAN_POINT ( 'NONE',  ( 10.00000000000000000, 11.81368534415483751, -10.88017736071110342 ) ) ;
#15390 = CARTESIAN_POINT ( 'NONE',  ( 20.88017736071110164, 35.35535201082150536, 2.915334737309930979 ) ) ;
#15391 = DIRECTION ( 'NONE',  ( -0.8526401643540953978, 0.000000000000000000, 0.5224985647159435809 ) ) ;
#15392 = DIRECTION ( 'NONE',  ( -0.000000000000000000, -1.000000000000000000, -0.000000000000000000 ) ) ;
#15393 = CARTESIAN_POINT ( 'NONE',  ( 14.92337183194729633, 2.675597817667451750, 8.527530157486181039 ) ) ;
#15394 = CARTESIAN_POINT ( 'NONE',  ( -0.8801773607111008646, 68.27201867748817676, 2.915334737309923430 ) ) ;
#15395 = CARTESIAN_POINT ( 'NONE',  ( 19.38216949554541557, 32.24863466993041783, -9.382169495545420901 ) ) ;
#15396 = DIRECTION ( 'NONE',  ( -0.000000000000000000, 1.000000000000000000, 0.000000000000000000 ) ) ;
#15397 = CARTESIAN_POINT ( 'NONE',  ( 0.1143410931637246636, 30.21691075486303291, 6.480892540919863443 ) ) ;
#15398 = CARTESIAN_POINT ( 'NONE',  ( 12.63842701281683922, 39.55059781766744464, -9.846743663894590881 ) ) ;
#15399 = CARTESIAN_POINT ( 'NONE',  ( 0.5774900079438607392, 8.480352010821505360, 5.440088680355550821 ) ) ;
#15400 = B_SPLINE_CURVE_WITH_KNOTS ( 'NONE', 3,
 ( #3926, #95411, #11911, #27395, #56911, #18929 ),
 .UNSPECIFIED., .F., .F.,
 ( 4, 2, 4 ),
 ( 3.409110551494637202E-05, 0.0004400426677367945405, 0.0008459942299586427090 ),
 .UNSPECIFIED. ) ;
#15401 = MECHANICAL_DESIGN_GEOMETRIC_PRESENTATION_REPRESENTATION (  '', ( #85610 ), #71265 ) ;
#15402 = VECTOR ( 'NONE', #44828, 1000.000000000000000 ) ;
#15403 = AXIS2_PLACEMENT_3D ( 'NONE', #9756, #57206, #40746 ) ;
#15404 = EDGE_CURVE ( 'NONE', #57215, #87334, #18798, .T. ) ;
#15405 = CARTESIAN_POINT ( 'NONE',  ( 10.00000000000000178, 15.37363466993042138, 12.81628187352647608 ) ) ;
#15406 = CARTESIAN_POINT ( 'NONE',  ( 7.361572987183169658, 14.96726448433411960, -9.846743663894592657 ) ) ;
#15407 = CARTESIAN_POINT ( 'NONE',  ( 2.035157376598824452, 3.688685344154837953, 7.964842623401179544 ) ) ;
#15408 = VECTOR ( 'NONE', #88590, 1000.000000000000000 ) ;
#15409 = CARTESIAN_POINT ( 'NONE',  ( 2.791683348922237240, 40.38393115100078035, -7.208316651077763204 ) ) ;
#15410 = CARTESIAN_POINT ( 'NONE',  ( 3.591859063236761518, 59.95696800326375353, 11.09922568453594849 ) ) ;
#15412 = CARTESIAN_POINT ( 'NONE',  ( -0.3689425029237898834, 1.178748834913967869, -10.36894250292378850 ) ) ;
#15411 = CARTESIAN_POINT ( 'NONE',  ( 18.52753015748617571, 18.09226448433411960, 4.923371831947298993 ) ) ;
#15413 = EDGE_CURVE ( 'NONE', #17506, #21360, #79467, .T. ) ;
#15414 = CARTESIAN_POINT ( 'NONE',  ( 20.36894250292379382, 8.678748834913967869, 10.36894250292379205 ) ) ;
#15415 = DIRECTION ( 'NONE',  ( 0.1650476058606878405, 0.000000000000000000, -0.9862856015372296614 ) ) ;
#15416 = CARTESIAN_POINT ( 'NONE',  ( 17.96484262340118221, 29.93868534415484106, 7.964842623401181321 ) ) ;
#15418 = CARTESIAN_POINT ( 'NONE',  ( 24.16423886937410614, 44.30374883491397497, 8.672049930838204340E-16 ) ) ;
#15417 = CARTESIAN_POINT ( 'NONE',  ( -0.8801773607110991993, 17.85535201082150536, -2.915334737309923874 ) ) ;
#15419 = CARTESIAN_POINT ( 'NONE',  ( 0.5774900079438590739, 27.64701867748817676, -5.440088680355550821 ) ) ;
#15420 = CARTESIAN_POINT ( 'NONE',  ( 20.88017736071110164, 20.35535201082150891, 2.915334737309930979 ) ) ;
#15421 = ORIENTED_EDGE ( 'NONE', *, *, #46150, .T. ) ;
#15422 =( BOUNDED_CURVE ( )  B_SPLINE_CURVE ( 2, ( #40503, #3972, #87945, #4472, #40995, #86964, #65436, #42460, #71492 ),
 .UNSPECIFIED., .F., .F. ) 
 B_SPLINE_CURVE_WITH_KNOTS ( ( 3, 2, 2, 2, 3 ),
 ( 0.9391432315068940495, 0.9404761904761904656, 0.9464285714285713969, 0.9523809523809523281, 0.9537139113502488552 ),
 .UNSPECIFIED. ) 
 CURVE ( )  GEOMETRIC_REPRESENTATION_ITEM ( )  RATIONAL_B_SPLINE_CURVE ( ( 0.9881565478350733400, 0.9923695281211490915, 1.000000000000000000, 0.9659258262890683122, 1.000000000000000000, 0.9659258262890683122, 1.000000000000000000, 0.9923695281211485364, 0.9881565478350726739 ) ) 
 REPRESENTATION_ITEM ( '' )  );
#15423 = CARTESIAN_POINT ( 'NONE',  ( -0.8801773607110991993, 42.85535201082150536, -2.915334737309923874 ) ) ;
#15424 = CARTESIAN_POINT ( 'NONE',  ( 22.81628187352648496, 56.83196800326374643, -3.434112377981050290 ) ) ;
#15426 = AXIS2_PLACEMENT_3D ( 'NONE', #7730, #61202, #31678 ) ;
#15425 = CARTESIAN_POINT ( 'NONE',  ( 20.88017736071110519, 45.56368534415484106, 2.639326808657452039E-16 ) ) ;
#15428 = CARTESIAN_POINT ( 'NONE',  ( 0.5774900079438590739, 52.64701867748817676, -5.440088680355550821 ) ) ;
#15427 = PLANE ( 'NONE',  #76045 ) ;
#15429 = ORIENTED_EDGE ( 'NONE', *, *, #48758, .T. ) ;
#15430 = AXIS2_PLACEMENT_3D ( 'NONE', #84923, #37965, #76437 ) ;
#15431 = CARTESIAN_POINT ( 'NONE',  ( 12.91533473730993009, 56.60535201082151247, -10.88017736071109987 ) ) ;
#15432 = CARTESIAN_POINT ( 'NONE',  ( -1.926860441876562025, 24.47997603579417358, -3.195792623639529761 ) ) ;
#15433 = CARTESIAN_POINT ( 'NONE',  ( 22.26659068614895176, 44.72041550158063927, -7.082119434687042414 ) ) ;
#15434 = CARTESIAN_POINT ( 'NONE',  ( 2.035157376598824452, 68.68868534415484817, 7.964842623401179544 ) ) ;
#15435 = CARTESIAN_POINT ( 'NONE',  ( -5.320211218918606377, -24.96484130673365343, -3.999999999999999112 ) ) ;
#15436 = CARTESIAN_POINT ( 'NONE',  ( 12.63842701281683034, 57.46726448433411605, 9.846743663894596210 ) ) ;
#15437 = FILL_AREA_STYLE_COLOUR ( '', #98788 ) ;
#15438 = CARTESIAN_POINT ( 'NONE',  ( 5.076628168052703671, 36.84226448433412315, 8.527530157486179263 ) ) ;
#15439 = CARTESIAN_POINT ( 'NONE',  ( 12.63842701281683922, 39.55059781766744464, -9.846743663894590881 ) ) ;
#15440 = CARTESIAN_POINT ( 'NONE',  ( -9.382169495545413795, -0.2513653300695748993, 9.382169495545428006 ) ) ;
#15441 = CARTESIAN_POINT ( 'NONE',  ( 17.96484262340118221, 34.93868534415482685, 7.964842623401181321 ) ) ;
#15442 = CARTESIAN_POINT ( 'NONE',  ( 19.84674366389459621, 43.50893115100078745, 7.409399052514197653E-17 ) ) ;
#15443 = CARTESIAN_POINT ( 'NONE',  ( 21.09922568453595559, 22.04030133659708923, -6.408140936763230044 ) ) ;
#15444 = CARTESIAN_POINT ( 'NONE',  ( -14.88232117145534517, 14.49999999999999112, -1.875237731503371030 ) ) ;
#15446 = CARTESIAN_POINT ( 'NONE',  ( 20.88017736071110875, 5.772018677488170546, -2.915334737309920765 ) ) ;
#15445 = CARTESIAN_POINT ( 'NONE',  ( 19.42250999205614548, 40.98035201082150536, -5.440088680355545492 ) ) ;
#15447 = CARTESIAN_POINT ( 'NONE',  ( 6.204703633549690345, 55.76208216824730357, -14.16423886937410259 ) ) ;
#15448 = STYLED_ITEM ( 'NONE', ( #79981 ), #55723 ) ;
#15449 = ADVANCED_FACE ( 'NONE', ( #18596, #72078, #88559 ), #94095, .F. ) ;
#15450 = CARTESIAN_POINT ( 'NONE',  ( -2.816281873526471635, 28.91530133659708213, -3.434112377981056508 ) ) ;
#15451 = DIRECTION ( 'NONE',  ( -1.000000000000000000, 0.000000000000000000, 0.000000000000000000 ) ) ;
#15452 = VERTEX_POINT ( 'NONE', #4093 ) ;
#15453 = CARTESIAN_POINT ( 'NONE',  ( -2.816281873526471635, 13.91530133659708746, -3.434112377981056508 ) ) ;
#15454 = CARTESIAN_POINT ( 'NONE',  ( -0.8801773607111008646, 23.27201867748817676, 2.915334737309923430 ) ) ;
#15455 = CARTESIAN_POINT ( 'NONE',  ( 20.88017736071110875, 65.77201867748817676, -2.915334737309920765 ) ) ;
#15456 = ORIENTED_EDGE ( 'NONE', *, *, #60444, .T. ) ;
#15457 = CARTESIAN_POINT ( 'NONE',  ( 10.00000000000000178, 54.31368534415484106, 10.88017736071110342 ) ) ;
#15458 = CARTESIAN_POINT ( 'NONE',  ( 1.472469842513823179, 45.59226448433412315, -4.923371831947296329 ) ) ;
#15459 = CARTESIAN_POINT ( 'NONE',  ( 5.076628168052703671, 21.84226448433411960, 8.527530157486179263 ) ) ;
#15460 = CARTESIAN_POINT ( 'NONE',  ( 12.63842701281683034, 22.46726448433411605, 9.846743663894596210 ) ) ;
#15461 = CARTESIAN_POINT ( 'NONE',  ( 6.000000000000000000, 11.50000000000000000, 5.000000000000000000 ) ) ;
#15463 = CARTESIAN_POINT ( 'NONE',  ( 16.40814093676324603, 42.45696800326375353, -11.09922568453594671 ) ) ;
#15462 = CARTESIAN_POINT ( 'NONE',  ( 3.969999999999999751, 36.75000000000000000, -2.750000000000000000 ) ) ;
#15465 = CARTESIAN_POINT ( 'NONE',  ( -7.882504294823764468, 15.00000000000000888, -12.32089577884801379 ) ) ;
#15464 = CARTESIAN_POINT ( 'NONE',  ( 17.20831665107776587, 19.13393115100078035, -7.208316651077762316 ) ) ;
#15466 = CARTESIAN_POINT ( 'NONE',  ( 4.721516313243696139, -3.620689210586685913, -3.999999999999998224 ) ) ;
#15467 = PRESENTATION_LAYER_ASSIGNMENT (  '', '', ( #1050 ) ) ;
#15469 = VERTEX_POINT ( 'NONE', #3604 ) ;
#15468 = CARTESIAN_POINT ( 'NONE',  ( 19.84674366389459621, 33.50893115100078745, 7.409399052514197653E-17 ) ) ;
#15470 = LINE ( 'NONE', #479, #94882 ) ;
#15471 = CARTESIAN_POINT ( 'NONE',  ( 22.81628187352647785, 6.415301336597088344, 3.434112377981063169 ) ) ;
#15472 = CARTESIAN_POINT ( 'NONE',  ( 19.42250999205614193, 50.14701867748817676, 5.440088680355555262 ) ) ;
#15473 = CARTESIAN_POINT ( 'NONE',  ( 13.79529636645030344, 33.26208216824730357, 14.16423886937410614 ) ) ;
#15474 = CARTESIAN_POINT ( 'NONE',  ( -13.59072821818278065, 90.85999462608739918, 7.686992381056737322 ) ) ;
#15475 = CARTESIAN_POINT ( 'NONE',  ( 6.204703633549690345, 25.76208216824730712, -14.16423886937410259 ) ) ;
#15476 = CARTESIAN_POINT ( 'NONE',  ( 2.917880565312948704, 62.63708216824730357, 12.26659068614894643 ) ) ;
#15477 = CARTESIAN_POINT ( 'NONE',  ( 2.917880565312950480, 10.97041550158063572, -12.26659068614894821 ) ) ;
#15479 = CARTESIAN_POINT ( 'NONE',  ( -0.2418659066527643342, 37.23410085661203794, -6.114288769123057854 ) ) ;
#15478 = CARTESIAN_POINT ( 'NONE',  ( 17.08211943468705840, 30.13708216824730357, -12.26659068614894466 ) ) ;
#15480 = CARTESIAN_POINT ( 'NONE',  ( 10.00000000000000000, 51.81368534415484106, -10.88017736071110342 ) ) ;
#15481 = CARTESIAN_POINT ( 'NONE',  ( 3.469446951953614189E-15, 11.36803362898265135, 11.25000000000000178 ) ) ;
#15483 = CARTESIAN_POINT ( 'NONE',  ( 19.84674366389459266, 43.71726448433410894, -2.638427012816827677 ) ) ;
#15482 = CARTESIAN_POINT ( 'NONE',  ( 5.429204171145670443, -28.64228857780832982, 2.500000000000000000 ) ) ;
#15484 = EDGE_LOOP ( 'NONE', ( #32942, #50065, #14119, #30605 ) ) ;
#15485 = DIRECTION ( 'NONE',  ( -0.8433914458128884961, 0.000000000000000000, 0.5372996083468194461 ) ) ;
#15486 = CARTESIAN_POINT ( 'NONE',  ( 19.84674366389459266, 58.71726448433411605, -2.638427012816827677 ) ) ;
#15487 = CARTESIAN_POINT ( 'NONE',  ( -0.07285406091746288171, 0.4131759111665360140, -9.500000000000000000 ) ) ;
#15488 = EDGE_CURVE ( 'NONE', #66734, #11231, #20062, .T. ) ;
#15489 = CARTESIAN_POINT ( 'NONE',  ( -1.099225684535947600, 58.70696800326375353, -6.408140936763238038 ) ) ;
#15490 = CARTESIAN_POINT ( 'NONE',  ( 12.26659068614894821, -1.112917831752692432, 7.082119434687044190 ) ) ;
#15491 = CIRCLE ( 'NONE', #12323, 14.49999999999999822 ) ;
#15492 = CARTESIAN_POINT ( 'NONE',  ( 0.1532563361054082862, 41.21726448433411605, 2.638427012816831674 ) ) ;
#15493 = CARTESIAN_POINT ( 'NONE',  ( 7.361572987183169658, 54.96726448433413026, -9.846743663894592657 ) ) ;
#15494 = CARTESIAN_POINT ( 'NONE',  ( -0.3689425029237898834, 36.17874883491396787, -10.36894250292378850 ) ) ;
#15495 = CIRCLE ( 'NONE', #28234, 0.4999999999999998890 ) ;
#15496 = ORIENTED_EDGE ( 'NONE', *, *, #26882, .F. ) ;
#15497 = CARTESIAN_POINT ( 'NONE',  ( 20.36894250292379382, 18.67874883491397142, 10.36894250292379205 ) ) ;
#15498 = CARTESIAN_POINT ( 'NONE',  ( 10.00000000000000178, 59.31368534415484106, 10.88017736071110342 ) ) ;
#15499 = CARTESIAN_POINT ( 'NONE',  ( 8.629999999999995453, 40.99999999999999289, 6.250000000000000000 ) ) ;
#15500 = CARTESIAN_POINT ( 'NONE',  ( 13.79529636645030344, 58.26208216824728936, 14.16423886937410614 ) ) ;
#15501 = CARTESIAN_POINT ( 'NONE',  ( 16.40814093676323893, 15.79030133659708746, 11.09922568453595026 ) ) ;
#15502 = CARTESIAN_POINT ( 'NONE',  ( 2.815433093577012880, 14.49999999999999112, 14.73340885523758281 ) ) ;
#15503 = CARTESIAN_POINT ( 'NONE',  ( 5.076628168052703671, 1.842264484334118047, 8.527530157486179263 ) ) ;
#15504 = CARTESIAN_POINT ( 'NONE',  ( -0.1503990784575287842, 28.10158574516642815, 6.262539305110075283 ) ) ;
#15505 = CARTESIAN_POINT ( 'NONE',  ( 1.959929470562269183, 30.51528370094808196, -5.767676674365832312 ) ) ;
#15506 = CARTESIAN_POINT ( 'NONE',  ( 21.09922568453594849, 31.20696800326375353, 6.408140936763242479 ) ) ;
#15507 = CARTESIAN_POINT ( 'NONE',  ( 24.16423886937410614, 59.51208216824728936, -3.795296366450302550 ) ) ;
#15508 = CARTESIAN_POINT ( 'NONE',  ( 3.469446951953614189E-15, 29.31368534415484817, 10.88017736071110342 ) ) ;
#15509 = CARTESIAN_POINT ( 'NONE',  ( 17.96484262340118221, 16.18868534415483396, -7.964842623401177768 ) ) ;
#15510 = CARTESIAN_POINT ( 'NONE',  ( -0.8801773607111009756, 28.06368534415484106, 1.068504757029289695E-15 ) ) ;
#15511 = CARTESIAN_POINT ( 'NONE',  ( 5.076628168052703671, 51.84226448433412315, 8.527530157486179263 ) ) ;
#15512 = CARTESIAN_POINT ( 'NONE',  ( 18.52753015748617571, 58.09226448433411605, 4.923371831947298993 ) ) ;
#15513 = CARTESIAN_POINT ( 'NONE',  ( 16.40814093676324603, 52.45696800326375353, -11.09922568453594671 ) ) ;
#15514 = DIRECTION ( 'NONE',  ( 0.000000000000000000, 0.000000000000000000, 1.000000000000000000 ) ) ;
#15515 = VERTEX_POINT ( 'NONE', #50564 ) ;
#15516 = CARTESIAN_POINT ( 'NONE',  ( 12.91533473730992121, 14.52201867748817143, 10.88017736071110164 ) ) ;
#15517 = CARTESIAN_POINT ( 'NONE',  ( 3.591859063236761518, 14.95696800326375531, 11.09922568453594849 ) ) ;
#15518 = CARTESIAN_POINT ( 'NONE',  ( -13.78891971893213331, 14.63595249122791842, 5.904717858191443014 ) ) ;
#15519 = ADVANCED_FACE ( 'NONE', ( #87573 ), #64560, .F. ) ;
#15520 = CARTESIAN_POINT ( 'NONE',  ( 17.20831665107776587, 47.88393115100078745, 7.208316651077764980 ) ) ;
#15521 = CARTESIAN_POINT ( 'NONE',  ( 19.42250999205614193, 55.14701867748817676, 5.440088680355555262 ) ) ;
#15522 = AXIS2_PLACEMENT_3D ( 'NONE', #83688, #15206, #45686 ) ;
#15523 = CARTESIAN_POINT ( 'NONE',  ( -1.099225684535947600, 18.70696800326375353, -6.408140936763238038 ) ) ;
#15525 = CARTESIAN_POINT ( 'NONE',  ( 0.000000000000000000, 15.00000000000000000, -14.25000000000000000 ) ) ;
#15524 = CARTESIAN_POINT ( 'NONE',  ( 2.035157376598824452, 53.68868534415484817, 7.964842623401179544 ) ) ;
#15526 =( BOUNDED_SURFACE ( )  B_SPLINE_SURFACE ( 1, 2, ( 
 ( #89456, #36459, #66954, #39798, #70298, #78272, #10771, #25295, #55782, #41768, #18770, #25781, #32268, #18273, #56275, #47275, #86277, #63748, #86770, #40780, #72239, #33734, #62274, #26254, #92780, #1813, #33257, #71280, #79260, #62777, #24799, #55276, #17786, #64235, #9786, #2310, #48752, #93276, #78774, #49252, #24311, #3270, #79752, #3772, #70793, #48261, #94253, #10280, #32765, #41286, #2802, #85786, #71760, #94752, #63260, #17299, #16799, #11250, #93769, #54776, #85292, #47774, #56751, #77776, #40285, #87244, #9289, #12725, #66722, #27230, #50222, #35725, #57725, #43220, #51727, #95746, #74201, #36221, #88228, #65719, #20233, #89223, #72723, #88722, #19246, #4257, #28220, #96744, #82209, #34728, #20732, #80736, #19737, #44203, #96245, #89709, #13221, #13719, #81707, #74713, #66213, #51223, #95233, #58718, #11745, #27725, #12231, #58205, #42253, #42740, #34226, #97246, #35219, #43717, #50737, #73221, #73714, #5735, #4749, #65219, #28715, #59206, #81226, #26741, #21223, #5247, #64723, #57236, #87734, #49730, #80237, #98231, #60690, #8202, #22225, #45204, #30680, #6713, #22715, #61666, #6223, #46198, #92185, #46675, #14728, #91190, #7718, #53199, #75703, #76199, #83703, #29692, #68700, #68217, #7214, #37230, #59703, #23711, #37715, #36727, #67218, #44703, #98738, #97741, #60201, #90696, #23213, #15220, #38697, #52701, #83206, #38215, #30189, #45699, #54172, #67718, #76682, #69196, #232, #61188, #91694, #53686, #75203, #84204, #90200, #15712, #721, #31175, #84683, #16193, #29204, #21730, #52212, #82706, #14224, #33620, #56160, #26146, #25667, #56640, #10165, #33137, #39193, #40663, #54660, #70672, #55152, #40167, #85176, #32151, #77173, #79140, #78160, #63632, #2192, #62653, #55664, #86653, #39691, #16686, #94139, #18158, #32654, #69681, #78660, #24681, #64119, #87125, #86163, #47156, #71161, #77659, #9173, #93157, #48636, #63148, #93650, #18646, #94636, #2686, #70179, #10651, #41166, #62157, #25184, #71650, #3158, #17673, #8681, #1212, #31667, #92663, #24191, #1695, #48146, #85666, #17186, #47666, #9670, #58095, #5121, #36095, #5619, #97130, #11627, #51104, #57612, #20615, #35609, #19620, #11136, #96127, #27608, #66602, #50614, #66095, #42620, #57120, #28600, #42143, #88111, #41655, #4637, #59089, #49135, #80119, #43598, #79637, #19131, #88600, #72122, #3650, #87618, #20110, #34115, #43107, #96624, #74086, #72607, #27113, #89598, #81591, #4142, #81105, #13102, #12606, #73594, #50114, #28099, #58600, #89102, #64607, #49609, #95115, #26623, #34607, #65103, #95624, #80624, #12118, #73099, #35101, #65599, #90574, #51606 ),
 ( #76070, #83583, #6105, #14610, #22594, #15100, #98619, #612, #91576, #21107, #84077, #82090, #97622, #91068, #30067, #38096, #59587, #82589, #14103, #75582, #23093, #37103, #60073, #45576, #21610, #37596, #76565, #13601, #61066, #8081, #61556, #29569, #7094, #53071, #68090, #22100, #7600, #60577, #44586, #68583, #83083, #52580, #52095, #74591, #38577, #45077, #44081, #36610, #90083, #114, #67097, #75085, #6591, #29085, #67600, #30560, #53563, #15592, #98107, #46076, #69075, #31056, #94032, #9058, #32031, #17560, #92545, #9548, #48521, #92064, #33029, #79023, #33507, #1582, #47548, #93534, #40050, #62535, #63036, #78046, #16570, #55549, #55035, #93041, #24074, #46558, #10535, #24575, #23592, #54056, #31549, #85553, #84570, #85057, #47043, #10050, #70550, #25553, #77540, #39571, #25064, #70060, #2078, #41045, #54541, #63525, #56045, #17066, #32538, #86049, #48027, #62045, #78539, #77057, #40549, #71049, #2572, #71544, #86538, #18043, #3053, #16071, #8569, #39074, #69567, #1087, #12983, #12497, #43479, #96009, #19995, #26036, #27494, #41544, #57501, #42033, #27004, #72008, #19023, #64005, #65985, #64985, #50497, #87996, #49500, #42508, #42996, #26512, #3539, #80994, #5007, #19509, #56528, #65489, #11510, #20498, #73981, #72992, #33999, #57987, #64497, #95004, #80005, #73478, #50004, #80510, #5506, #50986, #88492, #57007, #35490, #96512, #49018, #12007, #27983, #58480, #4522, #94517, #88993, #87017, #81480, #87509, #72497, #4030, #34985, #18528, #34493, #95510, #79525, #11026, #52466, #91454, #35980, #75956, #22980, #76452, #44468, #90453, #37484, #82969, #74970, #6979, #21990, #59469, #98498, #97999, #6475, #36489, #89484, #53445, #36979, #66482, #97010, #74470, #29453, #28488, #28966, #89971, #52953, #14488, #68471, #21487, #51984, #67973, #82472, #44960, #83954, #97502, #7484, #37981, #13993, #67478, #75463, #90948, #5994, #29953, #20995, #66980, #60458, #22478, #15480, #59961, #83464, #14985, #45456, #45963, #34337, #58981, #30444, #51482, #60944, #81976, #13488, #43966, #68958, #41304, #85804, #2819, #86294, #71299, #17314, #63279, #7968, #11266, #10299, #64253, #33269, #93785, #86787, #56768, #70811, #47790, #94768, #49268, #63763, #490, #10786, #55800, #64742, #57252, #18289, #78288, #71777, #9804, #40305, #25314, #87264, #94270, #25794, #87749, #95254, #3286, #2326, #26267, #33751, #93292, #56293, #18785, #79768, #48772, #19263, #41786, #38466, #72258, #30939, #32782, #79277, #3787, #34242, #62792, #26760, #17801, #49747, #48279, #24816, #78791, #40798, #55292, #82223, #81239, #36239, #43237, #65736, #58733, #28729 ) ),
 .UNSPECIFIED., .F., .F., .F. ) 
 B_SPLINE_SURFACE_WITH_KNOTS ( ( 2, 2 ),
 ( 3, 2, 2, 2, 2, 2, 2, 2, 2, 2, 2, 2, 2, 2, 2, 2, 2, 2, 2, 2, 2, 2, 2, 2, 2, 2, 2, 2, 2, 2, 2, 2, 2, 2, 2, 2, 2, 2, 2, 2, 2, 2, 2, 2, 2, 2, 2, 2, 2, 2, 2, 2, 2, 2, 2, 2, 2, 2, 2, 2, 2, 2, 2, 2, 2, 2, 2, 2, 2, 2, 2, 2, 2, 2, 2, 2, 2, 2, 2, 2, 2, 2, 2, 2, 2, 2, 2, 2, 2, 2, 2, 2, 2, 2, 2, 2, 2, 2, 2, 2, 2, 2, 2, 2, 2, 2, 2, 2, 2, 2, 2, 2, 2, 2, 2, 2, 2, 2, 2, 2, 2, 2, 2, 2, 2, 2, 2, 2, 2, 2, 2, 2, 2, 2, 2, 2, 2, 2, 2, 2, 2, 2, 2, 2, 2, 2, 2, 2, 2, 2, 2, 2, 2, 2, 2, 2, 2, 2, 2, 2, 2, 2, 3 ),
 ( 0.000000000000000000, 1.000000000000000000 ),
 ( 0.000000000000000000, 0.005952380952380952051, 0.01190476190476190410, 0.01785714285714285615, 0.02380952380952380820, 0.02976190476190476025, 0.03571428571428571230, 0.04166666666666666435, 0.04761904761904761640, 0.05357142857142856845, 0.05952380952380952051, 0.06547619047619047949, 0.07142857142857142461, 0.07738095238095238360, 0.08333333333333332871, 0.08928571428571428770, 0.09523809523809523281, 0.1011904761904761918, 0.1071428571428571369, 0.1130952380952380959, 0.1190476190476190410, 0.1250000000000000000, 0.1309523809523809590, 0.1369047619047619180, 0.1428571428571428492, 0.1488095238095238082, 0.1547619047619047672, 0.1607142857142857262, 0.1666666666666666574, 0.1726190476190476164, 0.1785714285714285754, 0.1845238095238095344, 0.1904761904761904656, 0.1964285714285714246, 0.2023809523809523836, 0.2083333333333333426, 0.2142857142857142738, 0.2202380952380952328, 0.2261904761904761918, 0.2321428571428571508, 0.2380952380952380820, 0.2440476190476190410, 0.2500000000000000000, 0.2559523809523809312, 0.2619047619047619180, 0.2678571428571428492, 0.2738095238095238360, 0.2797619047619047672, 0.2857142857142856984, 0.2916666666666666852, 0.2976190476190476164, 0.3035714285714285476, 0.3095238095238095344, 0.3154761904761904656, 0.3214285714285714524, 0.3273809523809523836, 0.3333333333333333148, 0.3392857142857143016, 0.3452380952380952328, 0.3511904761904761640, 0.3571428571428571508, 0.3630952380952380820, 0.3690476190476190688, 0.3750000000000000000, 0.3809523809523809312, 0.3869047619047619180, 0.3928571428571428492, 0.3988095238095238360, 0.4047619047619047672, 0.4107142857142856984, 0.4166666666666666852, 0.4226190476190476164, 0.4285714285714285476, 0.4345238095238095344, 0.4404761904761904656, 0.4464285714285714524, 0.4523809523809523836, 0.4583333333333333148, 0.4642857142857143016, 0.4702380952380952328, 0.4761904761904761640, 0.4821428571428571508, 0.4880952380952380820, 0.4940476190476190688, 0.5000000000000000000, 0.5059523809523809312, 0.5119047619047618625, 0.5178571428571429047, 0.5238095238095238360, 0.5297619047619047672, 0.5357142857142856984, 0.5416666666666666297, 0.5476190476190476719, 0.5535714285714286031, 0.5595238095238095344, 0.5654761904761904656, 0.5714285714285713969, 0.5773809523809523281, 0.5833333333333333703, 0.5892857142857143016, 0.5952380952380952328, 0.6011904761904761640, 0.6071428571428570953, 0.6130952380952381375, 0.6190476190476190688, 0.6250000000000000000, 0.6309523809523809312, 0.6369047619047618625, 0.6428571428571429047, 0.6488095238095238360, 0.6547619047619047672, 0.6607142857142856984, 0.6666666666666666297, 0.6726190476190476719, 0.6785714285714286031, 0.6845238095238095344, 0.6904761904761904656, 0.6964285714285713969, 0.7023809523809523281, 0.7083333333333333703, 0.7142857142857143016, 0.7202380952380952328, 0.7261904761904761640, 0.7321428571428570953, 0.7380952380952381375, 0.7440476190476190688, 0.7500000000000000000, 0.7559523809523809312, 0.7619047619047618625, 0.7678571428571429047, 0.7738095238095238360, 0.7797619047619047672, 0.7857142857142856984, 0.7916666666666666297, 0.7976190476190476719, 0.8035714285714286031, 0.8095238095238095344, 0.8154761904761904656, 0.8214285714285713969, 0.8273809523809523281, 0.8333333333333333703, 0.8392857142857143016, 0.8452380952380952328, 0.8511904761904761640, 0.8571428571428570953, 0.8630952380952381375, 0.8690476190476190688, 0.8750000000000000000, 0.8809523809523809312, 0.8869047619047618625, 0.8928571428571429047, 0.8988095238095238360, 0.9047619047619047672, 0.9107142857142856984, 0.9166666666666666297, 0.9226190476190476719, 0.9285714285714286031, 0.9345238095238095344, 0.9404761904761904656, 0.9464285714285713969, 0.9523809523809523281, 0.9583333333333333703, 0.9642857142857143016 ),
 .UNSPECIFIED. ) 
 GEOMETRIC_REPRESENTATION_ITEM ( )  RATIONAL_B_SPLINE_SURFACE ( (
 ( 1.000000000000000000, 0.9659258262890683122, 1.000000000000000000, 0.9659258262890683122, 1.000000000000000000, 0.9659258262890683122, 1.000000000000000000, 0.9659258262890683122, 1.000000000000000000, 0.9659258262890683122, 1.000000000000000000, 0.9659258262890683122, 1.000000000000000000, 0.9659258262890683122, 1.000000000000000000, 0.9659258262890683122, 1.000000000000000000, 0.9659258262890683122, 1.000000000000000000, 0.9659258262890683122, 1.000000000000000000, 0.9659258262890683122, 1.000000000000000000, 0.9659258262890683122, 1.000000000000000000, 0.9659258262890683122, 1.000000000000000000, 0.9659258262890683122, 1.000000000000000000, 0.9659258262890683122, 1.000000000000000000, 0.9659258262890683122, 1.000000000000000000, 0.9659258262890683122, 1.000000000000000000, 0.9659258262890683122, 1.000000000000000000, 0.9659258262890683122, 1.000000000000000000, 0.9659258262890683122, 1.000000000000000000, 0.9659258262890683122, 1.000000000000000000, 0.9659258262890683122, 1.000000000000000000, 0.9659258262890683122, 1.000000000000000000, 0.9659258262890683122, 1.000000000000000000, 0.9659258262890683122, 1.000000000000000000, 0.9659258262890683122, 1.000000000000000000, 0.9659258262890683122, 1.000000000000000000, 0.9659258262890683122, 1.000000000000000000, 0.9659258262890683122, 1.000000000000000000, 0.9659258262890683122, 1.000000000000000000, 0.9659258262890683122, 1.000000000000000000, 0.9659258262890683122, 1.000000000000000000, 0.9659258262890683122, 1.000000000000000000, 0.9659258262890683122, 1.000000000000000000, 0.9659258262890683122, 1.000000000000000000, 0.9659258262890683122, 1.000000000000000000, 0.9659258262890683122, 1.000000000000000000, 0.9659258262890683122, 1.000000000000000000, 0.9659258262890683122, 1.000000000000000000, 0.9659258262890683122, 1.000000000000000000, 0.9659258262890683122, 1.000000000000000000, 0.9659258262890683122, 1.000000000000000000, 0.9659258262890683122, 1.000000000000000000, 0.9659258262890683122, 1.000000000000000000, 0.9659258262890683122, 1.000000000000000000, 0.9659258262890683122, 1.000000000000000000, 0.9659258262890683122, 1.000000000000000000, 0.9659258262890683122, 1.000000000000000000, 0.9659258262890683122, 1.000000000000000000, 0.9659258262890683122, 1.000000000000000000, 0.9659258262890683122, 1.000000000000000000, 0.9659258262890683122, 1.000000000000000000, 0.9659258262890683122, 1.000000000000000000, 0.9659258262890683122, 1.000000000000000000, 0.9659258262890683122, 1.000000000000000000, 0.9659258262890683122, 1.000000000000000000, 0.9659258262890683122, 1.000000000000000000, 0.9659258262890683122, 1.000000000000000000, 0.9659258262890683122, 1.000000000000000000, 0.9659258262890683122, 1.000000000000000000, 0.9659258262890683122, 1.000000000000000000, 0.9659258262890683122, 1.000000000000000000, 0.9659258262890683122, 1.000000000000000000, 0.9659258262890683122, 1.000000000000000000, 0.9659258262890683122, 1.000000000000000000, 0.9659258262890683122, 1.000000000000000000, 0.9659258262890683122, 1.000000000000000000, 0.9659258262890683122, 1.000000000000000000, 0.9659258262890683122, 1.000000000000000000, 0.9659258262890683122, 1.000000000000000000, 0.9659258262890683122, 1.000000000000000000, 0.9659258262890683122, 1.000000000000000000, 0.9659258262890683122, 1.000000000000000000, 0.9659258262890683122, 1.000000000000000000, 0.9659258262890683122, 1.000000000000000000, 0.9659258262890683122, 1.000000000000000000, 0.9659258262890683122, 1.000000000000000000, 0.9659258262890683122, 1.000000000000000000, 0.9659258262890683122, 1.000000000000000000, 0.9659258262890683122, 1.000000000000000000, 0.9659258262890683122, 1.000000000000000000, 0.9659258262890683122, 1.000000000000000000, 0.9659258262890683122, 1.000000000000000000, 0.9659258262890683122, 1.000000000000000000, 0.9659258262890683122, 1.000000000000000000, 0.9659258262890683122, 1.000000000000000000, 0.9659258262890683122, 1.000000000000000000, 0.9659258262890683122, 1.000000000000000000, 0.9659258262890683122, 1.000000000000000000, 0.9659258262890683122, 1.000000000000000000, 0.9659258262890683122, 1.000000000000000000, 0.9659258262890683122, 1.000000000000000000, 0.9659258262890683122, 1.000000000000000000, 0.9659258262890683122, 1.000000000000000000, 0.9659258262890683122, 1.000000000000000000, 0.9659258262890683122, 1.000000000000000000, 0.9659258262890683122, 1.000000000000000000, 0.9659258262890683122, 1.000000000000000000, 0.9659258262890683122, 1.000000000000000000, 0.9659258262890683122, 1.000000000000000000, 0.9659258262890683122, 1.000000000000000000, 0.9659258262890683122, 1.000000000000000000, 0.9659258262890683122, 1.000000000000000000, 0.9659258262890683122, 1.000000000000000000, 0.9659258262890683122, 1.000000000000000000, 0.9659258262890683122, 1.000000000000000000, 0.9659258262890683122, 1.000000000000000000, 0.9659258262890683122, 1.000000000000000000, 0.9659258262890683122, 1.000000000000000000, 0.9659258262890683122, 1.000000000000000000, 0.9659258262890683122, 1.000000000000000000, 0.9659258262890683122, 1.000000000000000000, 0.9659258262890683122, 1.000000000000000000, 0.9659258262890683122, 1.000000000000000000, 0.9659258262890683122, 1.000000000000000000, 0.9659258262890683122, 1.000000000000000000, 0.9659258262890683122, 1.000000000000000000, 0.9659258262890683122, 1.000000000000000000, 0.9659258262890683122, 1.000000000000000000, 0.9659258262890683122, 1.000000000000000000, 0.9659258262890683122, 1.000000000000000000, 0.9659258262890683122, 1.000000000000000000, 0.9659258262890683122, 1.000000000000000000, 0.9659258262890683122, 1.000000000000000000, 0.9659258262890683122, 1.000000000000000000, 0.9659258262890683122, 1.000000000000000000, 0.9659258262890683122, 1.000000000000000000, 0.9659258262890683122, 1.000000000000000000, 0.9659258262890683122, 1.000000000000000000, 0.9659258262890683122, 1.000000000000000000, 0.9659258262890683122, 1.000000000000000000, 0.9659258262890683122, 1.000000000000000000, 0.9659258262890683122, 1.000000000000000000, 0.9659258262890683122, 1.000000000000000000, 0.9659258262890683122, 1.000000000000000000, 0.9659258262890683122, 1.000000000000000000, 0.9659258262890683122, 1.000000000000000000, 0.9659258262890683122, 1.000000000000000000, 0.9659258262890683122, 1.000000000000000000, 0.9659258262890683122, 1.000000000000000000, 0.9659258262890683122, 1.000000000000000000, 0.9659258262890683122, 1.000000000000000000, 0.9659258262890683122, 1.000000000000000000, 0.9659258262890683122, 1.000000000000000000, 0.9659258262890683122, 1.000000000000000000, 0.9659258262890683122, 1.000000000000000000, 0.9659258262890683122, 1.000000000000000000, 0.9659258262890683122, 1.000000000000000000, 0.9659258262890683122, 1.000000000000000000, 0.9659258262890683122, 1.000000000000000000, 0.9659258262890683122, 1.000000000000000000, 0.9659258262890683122, 1.000000000000000000, 0.9659258262890683122, 1.000000000000000000, 0.9659258262890683122, 1.000000000000000000, 0.9659258262890683122, 1.000000000000000000, 0.9659258262890683122, 1.000000000000000000, 0.9659258262890683122, 1.000000000000000000, 0.9659258262890683122, 1.000000000000000000, 0.9659258262890683122, 1.000000000000000000, 0.9659258262890683122, 1.000000000000000000, 0.9659258262890683122, 1.000000000000000000, 0.9659258262890683122, 1.000000000000000000),
 ( 1.000000000000000000, 0.9659258262890683122, 1.000000000000000000, 0.9659258262890683122, 1.000000000000000000, 0.9659258262890683122, 1.000000000000000000, 0.9659258262890683122, 1.000000000000000000, 0.9659258262890683122, 1.000000000000000000, 0.9659258262890683122, 1.000000000000000000, 0.9659258262890683122, 1.000000000000000000, 0.9659258262890683122, 1.000000000000000000, 0.9659258262890683122, 1.000000000000000000, 0.9659258262890683122, 1.000000000000000000, 0.9659258262890683122, 1.000000000000000000, 0.9659258262890683122, 1.000000000000000000, 0.9659258262890683122, 1.000000000000000000, 0.9659258262890683122, 1.000000000000000000, 0.9659258262890683122, 1.000000000000000000, 0.9659258262890683122, 1.000000000000000000, 0.9659258262890683122, 1.000000000000000000, 0.9659258262890683122, 1.000000000000000000, 0.9659258262890683122, 1.000000000000000000, 0.9659258262890683122, 1.000000000000000000, 0.9659258262890683122, 1.000000000000000000, 0.9659258262890683122, 1.000000000000000000, 0.9659258262890683122, 1.000000000000000000, 0.9659258262890683122, 1.000000000000000000, 0.9659258262890683122, 1.000000000000000000, 0.9659258262890683122, 1.000000000000000000, 0.9659258262890683122, 1.000000000000000000, 0.9659258262890683122, 1.000000000000000000, 0.9659258262890683122, 1.000000000000000000, 0.9659258262890683122, 1.000000000000000000, 0.9659258262890683122, 1.000000000000000000, 0.9659258262890683122, 1.000000000000000000, 0.9659258262890683122, 1.000000000000000000, 0.9659258262890683122, 1.000000000000000000, 0.9659258262890683122, 1.000000000000000000, 0.9659258262890683122, 1.000000000000000000, 0.9659258262890683122, 1.000000000000000000, 0.9659258262890683122, 1.000000000000000000, 0.9659258262890683122, 1.000000000000000000, 0.9659258262890683122, 1.000000000000000000, 0.9659258262890683122, 1.000000000000000000, 0.9659258262890683122, 1.000000000000000000, 0.9659258262890683122, 1.000000000000000000, 0.9659258262890683122, 1.000000000000000000, 0.9659258262890683122, 1.000000000000000000, 0.9659258262890683122, 1.000000000000000000, 0.9659258262890683122, 1.000000000000000000, 0.9659258262890683122, 1.000000000000000000, 0.9659258262890683122, 1.000000000000000000, 0.9659258262890683122, 1.000000000000000000, 0.9659258262890683122, 1.000000000000000000, 0.9659258262890683122, 1.000000000000000000, 0.9659258262890683122, 1.000000000000000000, 0.9659258262890683122, 1.000000000000000000, 0.9659258262890683122, 1.000000000000000000, 0.9659258262890683122, 1.000000000000000000, 0.9659258262890683122, 1.000000000000000000, 0.9659258262890683122, 1.000000000000000000, 0.9659258262890683122, 1.000000000000000000, 0.9659258262890683122, 1.000000000000000000, 0.9659258262890683122, 1.000000000000000000, 0.9659258262890683122, 1.000000000000000000, 0.9659258262890683122, 1.000000000000000000, 0.9659258262890683122, 1.000000000000000000, 0.9659258262890683122, 1.000000000000000000, 0.9659258262890683122, 1.000000000000000000, 0.9659258262890683122, 1.000000000000000000, 0.9659258262890683122, 1.000000000000000000, 0.9659258262890683122, 1.000000000000000000, 0.9659258262890683122, 1.000000000000000000, 0.9659258262890683122, 1.000000000000000000, 0.9659258262890683122, 1.000000000000000000, 0.9659258262890683122, 1.000000000000000000, 0.9659258262890683122, 1.000000000000000000, 0.9659258262890683122, 1.000000000000000000, 0.9659258262890683122, 1.000000000000000000, 0.9659258262890683122, 1.000000000000000000, 0.9659258262890683122, 1.000000000000000000, 0.9659258262890683122, 1.000000000000000000, 0.9659258262890683122, 1.000000000000000000, 0.9659258262890683122, 1.000000000000000000, 0.9659258262890683122, 1.000000000000000000, 0.9659258262890683122, 1.000000000000000000, 0.9659258262890683122, 1.000000000000000000, 0.9659258262890683122, 1.000000000000000000, 0.9659258262890683122, 1.000000000000000000, 0.9659258262890683122, 1.000000000000000000, 0.9659258262890683122, 1.000000000000000000, 0.9659258262890683122, 1.000000000000000000, 0.9659258262890683122, 1.000000000000000000, 0.9659258262890683122, 1.000000000000000000, 0.9659258262890683122, 1.000000000000000000, 0.9659258262890683122, 1.000000000000000000, 0.9659258262890683122, 1.000000000000000000, 0.9659258262890683122, 1.000000000000000000, 0.9659258262890683122, 1.000000000000000000, 0.9659258262890683122, 1.000000000000000000, 0.9659258262890683122, 1.000000000000000000, 0.9659258262890683122, 1.000000000000000000, 0.9659258262890683122, 1.000000000000000000, 0.9659258262890683122, 1.000000000000000000, 0.9659258262890683122, 1.000000000000000000, 0.9659258262890683122, 1.000000000000000000, 0.9659258262890683122, 1.000000000000000000, 0.9659258262890683122, 1.000000000000000000, 0.9659258262890683122, 1.000000000000000000, 0.9659258262890683122, 1.000000000000000000, 0.9659258262890683122, 1.000000000000000000, 0.9659258262890683122, 1.000000000000000000, 0.9659258262890683122, 1.000000000000000000, 0.9659258262890683122, 1.000000000000000000, 0.9659258262890683122, 1.000000000000000000, 0.9659258262890683122, 1.000000000000000000, 0.9659258262890683122, 1.000000000000000000, 0.9659258262890683122, 1.000000000000000000, 0.9659258262890683122, 1.000000000000000000, 0.9659258262890683122, 1.000000000000000000, 0.9659258262890683122, 1.000000000000000000, 0.9659258262890683122, 1.000000000000000000, 0.9659258262890683122, 1.000000000000000000, 0.9659258262890683122, 1.000000000000000000, 0.9659258262890683122, 1.000000000000000000, 0.9659258262890683122, 1.000000000000000000, 0.9659258262890683122, 1.000000000000000000, 0.9659258262890683122, 1.000000000000000000, 0.9659258262890683122, 1.000000000000000000, 0.9659258262890683122, 1.000000000000000000, 0.9659258262890683122, 1.000000000000000000, 0.9659258262890683122, 1.000000000000000000, 0.9659258262890683122, 1.000000000000000000, 0.9659258262890683122, 1.000000000000000000, 0.9659258262890683122, 1.000000000000000000, 0.9659258262890683122, 1.000000000000000000, 0.9659258262890683122, 1.000000000000000000, 0.9659258262890683122, 1.000000000000000000, 0.9659258262890683122, 1.000000000000000000, 0.9659258262890683122, 1.000000000000000000, 0.9659258262890683122, 1.000000000000000000, 0.9659258262890683122, 1.000000000000000000, 0.9659258262890683122, 1.000000000000000000, 0.9659258262890683122, 1.000000000000000000, 0.9659258262890683122, 1.000000000000000000, 0.9659258262890683122, 1.000000000000000000, 0.9659258262890683122, 1.000000000000000000, 0.9659258262890683122, 1.000000000000000000, 0.9659258262890683122, 1.000000000000000000, 0.9659258262890683122, 1.000000000000000000, 0.9659258262890683122, 1.000000000000000000, 0.9659258262890683122, 1.000000000000000000, 0.9659258262890683122, 1.000000000000000000, 0.9659258262890683122, 1.000000000000000000, 0.9659258262890683122, 1.000000000000000000, 0.9659258262890683122, 1.000000000000000000, 0.9659258262890683122, 1.000000000000000000, 0.9659258262890683122, 1.000000000000000000, 0.9659258262890683122, 1.000000000000000000, 0.9659258262890683122, 1.000000000000000000, 0.9659258262890683122, 1.000000000000000000, 0.9659258262890683122, 1.000000000000000000, 0.9659258262890683122, 1.000000000000000000, 0.9659258262890683122, 1.000000000000000000, 0.9659258262890683122, 1.000000000000000000) ) ) 
 REPRESENTATION_ITEM ( '' )  SURFACE ( )  );
#15527 = CARTESIAN_POINT ( 'NONE',  ( 22.81628187352647785, 56.62363466993042493, 6.195893100308588602E-16 ) ) ;
#15528 = ORIENTED_EDGE ( 'NONE', *, *, #52791, .F. ) ;
#15529 = CARTESIAN_POINT ( 'NONE',  ( 5.076628168052703671, 61.84226448433412315, 8.527530157486179263 ) ) ;
#15530 = ADVANCED_FACE ( 'NONE', ( #4589 ), #79592, .T. ) ;
#15531 = CARTESIAN_POINT ( 'NONE',  ( -0.8801773607111009756, 48.06368534415484817, 1.068504757029289695E-15 ) ) ;
#15533 = CARTESIAN_POINT ( 'NONE',  ( -2.266590686148945544, 12.22041550158063394, 7.082119434687048631 ) ) ;
#15532 = CARTESIAN_POINT ( 'NONE',  ( 16.40814093676324603, 42.45696800326375353, -11.09922568453594671 ) ) ;
#15534 = DIRECTION ( 'NONE',  ( -1.776356839400250465E-15, 0.000000000000000000, 1.000000000000000000 ) ) ;
#15535 = CARTESIAN_POINT ( 'NONE',  ( 17.20831665107776587, 34.13393115100078745, -7.208316651077762316 ) ) ;
#15536 = CARTESIAN_POINT ( 'NONE',  ( 5.076628168052704559, 5.175597817667451750, -8.527530157486179263 ) ) ;
#15537 = FACE_OUTER_BOUND ( 'NONE', #72454, .T. ) ;
#15538 = CARTESIAN_POINT ( 'NONE',  ( -2.266590686148945544, 37.22041550158063217, 7.082119434687048631 ) ) ;
#15539 = LINE ( 'NONE', #82530, #34600 ) ;
#15540 = CARTESIAN_POINT ( 'NONE',  ( 7.084665262690076126, 14.10535201082150358, 10.88017736071109987 ) ) ;
#15541 = CARTESIAN_POINT ( 'NONE',  ( -6.868018881897137717, -58.39307134327864901, -3.749999999999999556 ) ) ;
#15542 = ORIENTED_EDGE ( 'NONE', *, *, #15869, .T. ) ;
#15543 = ORIENTED_EDGE ( 'NONE', *, *, #27469, .T. ) ;
#15544 = CARTESIAN_POINT ( 'NONE',  ( 15.44008868035555260, 14.73035201082150536, 9.422509992056143702 ) ) ;
#15545 = CARTESIAN_POINT ( 'NONE',  ( 0.5774900079438590739, 7.647018677488171434, -5.440088680355550821 ) ) ;
#15546 = CARTESIAN_POINT ( 'NONE',  ( 10.00000000000000000, 39.75893115100078745, -9.846743663894594434 ) ) ;
#15547 = CARTESIAN_POINT ( 'NONE',  ( 22.81628187352647785, 36.41530133659707502, 3.434112377981063169 ) ) ;
#15549 = CARTESIAN_POINT ( 'NONE',  ( 2.917880565312950480, 5.970415501580634832, -12.26659068614894821 ) ) ;
#15548 = CARTESIAN_POINT ( 'NONE',  ( -9.286179496275984491, 88.06418697516615168, -4.851265792414058531 ) ) ;
#15550 = CARTESIAN_POINT ( 'NONE',  ( -0.8801773607110991993, 22.85535201082150181, -2.915334737309923874 ) ) ;
#15551 = CARTESIAN_POINT ( 'NONE',  ( 20.36894250292379738, 64.92874883491397497, -10.36894250292379027 ) ) ;
#15552 = VECTOR ( 'NONE', #87123, 1000.000000000000000 ) ;
#15553 = CARTESIAN_POINT ( 'NONE',  ( 0.1532563361054083140, 36.00893115100078745, 1.131784320476157264E-15 ) ) ;
#15554 = LINE ( 'NONE', #84528, #25329 ) ;
#15555 = CARTESIAN_POINT ( 'NONE',  ( 19.84674366389459266, 18.30059781766745175, 2.638427012816836559 ) ) ;
#15556 = CARTESIAN_POINT ( 'NONE',  ( -8.527530157486173934, 26.42559781766745530, 4.923371831947302546 ) ) ;
#15557 = CIRCLE ( 'NONE', #71425, 2.500000000000002220 ) ;
#15558 = ORIENTED_EDGE ( 'NONE', *, *, #1003, .T. ) ;
#15559 = FACE_OUTER_BOUND ( 'NONE', #14570, .T. ) ;
#15560 = EDGE_LOOP ( 'NONE', ( #96733, #76359, #664, #88824 ) ) ;
#15561 = CARTESIAN_POINT ( 'NONE',  ( 1.472469842513823179, 56.42559781766745886, 4.923371831947296329 ) ) ;
#15563 = CARTESIAN_POINT ( 'NONE',  ( 20.88017736071110875, 35.77201867748816966, -2.915334737309920765 ) ) ;
#15562 = CARTESIAN_POINT ( 'NONE',  ( 10.00000000000000178, 29.31368534415483751, 10.88017736071110342 ) ) ;
#15565 = CARTESIAN_POINT ( 'NONE',  ( 22.81628187352647785, 31.62363466993042138, 6.195893100308588602E-16 ) ) ;
#15564 = CARTESIAN_POINT ( 'NONE',  ( -0.8801773607110991993, 2.855352010821504471, -2.915334737309923874 ) ) ;
#15566 = CARTESIAN_POINT ( 'NONE',  ( 2.917880565312950480, 20.97041550158063217, -12.26659068614894821 ) ) ;
#15567 = EDGE_CURVE ( 'NONE', #82021, #73831, #70657, .T. ) ;
#15568 = AXIS2_PLACEMENT_3D ( 'NONE', #96871, #13346, #30183 ) ;
#15569 = COLOUR_RGB ( '', 0.72549020, 0.75294118, 0.79215686) ;
#15570 = CARTESIAN_POINT ( 'NONE',  ( 10.00000000000000178, 50.37363466993042493, 12.81628187352647608 ) ) ;
#15571 = ORIENTED_EDGE ( 'NONE', *, *, #4880, .F. ) ;
#15572 = CARTESIAN_POINT ( 'NONE',  ( 7.361572987183170547, 47.05059781766745175, 9.846743663894590881 ) ) ;
#15573 = CARTESIAN_POINT ( 'NONE',  ( 19.42250999205614193, 25.14701867748817321, 5.440088680355555262 ) ) ;
#15574 = EDGE_LOOP ( 'NONE', ( #58874, #93353, #72209, #86364 ) ) ;
#15575 = CARTESIAN_POINT ( 'NONE',  ( 15.44008868035555260, 19.73035201082150536, 9.422509992056143702 ) ) ;
#15576 = EDGE_CURVE ( 'NONE', #97363, #37672, #85892, .T. ) ;
#15577 = ORIENTED_EDGE ( 'NONE', *, *, #20131, .T. ) ;
#15578 = CARTESIAN_POINT ( 'NONE',  ( 0.5774900079438590739, 57.64701867748817676, -5.440088680355550821 ) ) ;
#15579 = CARTESIAN_POINT ( 'NONE',  ( 12.91533473730993009, 61.60535201082150536, -10.88017736071109987 ) ) ;
#15580 = CARTESIAN_POINT ( 'NONE',  ( -0.8801773607111009756, 58.06368534415484106, 1.068504757029289695E-15 ) ) ;
#15581 = CARTESIAN_POINT ( 'NONE',  ( -1.926860441876564023, 29.68830936912750573, 1.004413902775740781E-15 ) ) ;
#15582 = CARTESIAN_POINT ( 'NONE',  ( -46.94000000000126960, 101.3832071409885884, 8.175121524388728744 ) ) ;
#15584 = ORIENTED_EDGE ( 'NONE', *, *, #78572, .T. ) ;
#15583 = CARTESIAN_POINT ( 'NONE',  ( 20.15039907845753220, 54.72266099184918886, 6.262539305110078836 ) ) ;
#15585 = CARTESIAN_POINT ( 'NONE',  ( 0.1532563361054083140, 41.00893115100078745, 1.131784320476157264E-15 ) ) ;
#15586 = VERTEX_POINT ( 'NONE', #20567 ) ;
#15587 = CARTESIAN_POINT ( 'NONE',  ( 0.2751277870542967463, 70.00000000000000000, 6.000000000000000000 ) ) ;
#15588 =( LENGTH_UNIT ( ) NAMED_UNIT ( * ) SI_UNIT ( .MILLI., .METRE. ) );
#15589 = VECTOR ( 'NONE', #15396, 1000.000000000000000 ) ;
#15590 = CARTESIAN_POINT ( 'NONE',  ( 13.79529636645030344, 23.26208216824730002, 14.16423886937410614 ) ) ;
#15591 = DIRECTION ( 'NONE',  ( 0.000000000000000000, 0.000000000000000000, 1.000000000000000000 ) ) ;
#15592 = CARTESIAN_POINT ( 'NONE',  ( 2.035157376598824452, 13.68868534415483751, 7.964842623401179544 ) ) ;
#15593 = CARTESIAN_POINT ( 'NONE',  ( 0.2751277870542871984, 68.21833443783938833, 6.499999999999984901 ) ) ;
#15595 = ORIENTED_EDGE ( 'NONE', *, *, #13820, .T. ) ;
#15594 = CARTESIAN_POINT ( 'NONE',  ( 22.81628187352648496, 36.83196800326376064, -3.434112377981050290 ) ) ;
#15596 = CARTESIAN_POINT ( 'NONE',  ( 19.80427997160309417, 62.75733960839542647, -6.499999999999983125 ) ) ;
#15597 = CARTESIAN_POINT ( 'NONE',  ( 14.92337183194729633, 2.675597817667451750, 8.527530157486181039 ) ) ;
#15598 = CARTESIAN_POINT ( 'NONE',  ( 13.43411237798106583, 32.66530133659708213, -12.81628187352647252 ) ) ;
#15599 = CARTESIAN_POINT ( 'NONE',  ( 17.20831665107776587, 19.13393115100078035, -7.208316651077762316 ) ) ;
#15600 = EDGE_CURVE ( 'NONE', #16779, #18519, #39581, .T. ) ;
#15601 = CARTESIAN_POINT ( 'NONE',  ( -1.099225684535947600, 13.70696800326375353, -6.408140936763238038 ) ) ;
#15602 = CARTESIAN_POINT ( 'NONE',  ( 6.880000000000007887, 41.24999999999999289, -6.250000000000000000 ) ) ;
#15603 = MECHANICAL_DESIGN_GEOMETRIC_PRESENTATION_REPRESENTATION (  '', ( #9234 ), #63534 ) ;
#15604 = CARTESIAN_POINT ( 'NONE',  ( 10.00000000000000000, -0.2410688489992152128, -9.846743663894594434 ) ) ;
#15605 = ORIENTED_EDGE ( 'NONE', *, *, #39446, .T. ) ;
#15606 = EDGE_CURVE ( 'NONE', #5928, #70551, #83760, .T. ) ;
#15607 = B_SPLINE_CURVE_WITH_KNOTS ( 'NONE', 3,
 ( #43219, #66720, #12724, #27229, #96743, #67217 ),
 .UNSPECIFIED., .F., .F.,
 ( 4, 2, 4 ),
 ( 3.409110551496041244E-05, 0.0004400426677367855958, 0.0008459942299586108334 ),
 .UNSPECIFIED. ) ;
#15608 = EDGE_LOOP ( 'NONE', ( #8355, #9526, #16776, #67796 ) ) ;
#15609 = CARTESIAN_POINT ( 'NONE',  ( 0.5774900079438590739, 22.64701867748817321, -5.440088680355550821 ) ) ;
#15610 = CARTESIAN_POINT ( 'NONE',  ( 17.08211943468705130, 23.47041550158063572, 12.26659068614894998 ) ) ;
#15611 = CARTESIAN_POINT ( 'NONE',  ( 12.63842701281683034, 47.46726448433412315, 9.846743663894596210 ) ) ;
#15612 = CARTESIAN_POINT ( 'NONE',  ( 17.96484262340118221, 66.18868534415483396, -7.964842623401177768 ) ) ;
#15614 = DIRECTION ( 'NONE',  ( -0.000000000000000000, 0.000000000000000000, 1.000000000000000000 ) ) ;
#15613 = CARTESIAN_POINT ( 'NONE',  ( 13.43411237798106583, 42.66530133659707502, -12.81628187352647252 ) ) ;
#15615 = CARTESIAN_POINT ( 'NONE',  ( -0.8801773607111008646, 8.272018677488171434, 2.915334737309923430 ) ) ;
#15616 = DIRECTION ( 'NONE',  ( -0.000000000000000000, 1.000000000000000000, -0.000000000000000000 ) ) ;
#15617 = AXIS2_PLACEMENT_3D ( 'NONE', #77617, #62116, #2156 ) ;
#15618 = CARTESIAN_POINT ( 'NONE',  ( -1.099225684535947600, 8.706968003263753531, -6.408140936763238038 ) ) ;
#15619 = CARTESIAN_POINT ( 'NONE',  ( -1.099225684535947600, 13.70696800326375353, -6.408140936763238038 ) ) ;
#15620 = CARTESIAN_POINT ( 'NONE',  ( 19.84674366389459266, 33.71726448433410894, -2.638427012816827677 ) ) ;
#15621 = CARTESIAN_POINT ( 'NONE',  ( 7.964842623401181321, -10.06131465584515716, 7.964842623401174215 ) ) ;
#15622 = CARTESIAN_POINT ( 'NONE',  ( -2.816281873526473856, 34.12363466993042493, 9.499525473075851096E-16 ) ) ;
#15623 = CYLINDRICAL_SURFACE ( 'NONE', #53217, 0.2500000000000002220 ) ;
#15625 = CARTESIAN_POINT ( 'NONE',  ( 20.15039907845753930, 9.722660991849181755, 6.262539305110064625 ) ) ;
#15624 = CARTESIAN_POINT ( 'NONE',  ( 4.559911319644449179, 57.23035201082150536, -9.422509992056141925 ) ) ;
#15626 = AXIS2_PLACEMENT_3D ( 'NONE', #97889, #88389, #19888 ) ;
#15627 = FACE_OUTER_BOUND ( 'NONE', #48697, .T. ) ;
#15628 = DIRECTION ( 'NONE',  ( 0.000000000000000000, -0.000000000000000000, -1.000000000000000000 ) ) ;
#15629 = VECTOR ( 'NONE', #49207, 1000.000000000000000 ) ;
#15630 = CARTESIAN_POINT ( 'NONE',  ( 7.084665262690076126, 34.10535201082151247, 10.88017736071109987 ) ) ;
#15631 = CARTESIAN_POINT ( 'NONE',  ( 12.91533473730993009, 46.60535201082150536, -10.88017736071109987 ) ) ;
#15632 = CARTESIAN_POINT ( 'NONE',  ( 10.00000000000000178, 67.25893115100079456, 9.846743663894594434 ) ) ;
#15633 = CARTESIAN_POINT ( 'NONE',  ( -7.313705784284419309, 0.5000000000000004441, -13.09617149020753502 ) ) ;
#15634 = CARTESIAN_POINT ( 'NONE',  ( 12.63842701281683034, 52.46726448433413026, 9.846743663894596210 ) ) ;
#15636 = DIRECTION ( 'NONE',  ( -1.000000000000000000, 0.000000000000000000, 0.000000000000000000 ) ) ;
#15635 = CARTESIAN_POINT ( 'NONE',  ( -0.8801773607111009756, 3.063685344154837509, 1.068504757029289695E-15 ) ) ;
#15637 = CARTESIAN_POINT ( 'NONE',  ( 22.81628187352647785, 6.415301336597088344, 3.434112377981063169 ) ) ;
#15638 = VERTEX_POINT ( 'NONE', #66049 ) ;
#15639 = CARTESIAN_POINT ( 'NONE',  ( 19.42250999205614548, 40.98035201082150536, -5.440088680355545492 ) ) ;
#15640 = ADVANCED_FACE ( 'NONE', ( #36557 ), #83534, .F. ) ;
#15642 = FACE_OUTER_BOUND ( 'NONE', #91752, .T. ) ;
#15641 = CARTESIAN_POINT ( 'NONE',  ( 0.1532563361054083140, 61.00893115100078745, 1.131784320476157264E-15 ) ) ;
#15643 = CARTESIAN_POINT ( 'NONE',  ( 15.44008868035555260, 9.730352010821505360, 9.422509992056143702 ) ) ;
#15644 = CARTESIAN_POINT ( 'NONE',  ( 0.5774900079438590739, 32.64701867748816966, -5.440088680355550821 ) ) ;
#15645 = CARTESIAN_POINT ( 'NONE',  ( -0.3689425029237881626, 42.42874883491396787, 10.36894250292379027 ) ) ;
#15646 = CARTESIAN_POINT ( 'NONE',  ( 5.076628168052703671, 31.84226448433412315, 8.527530157486179263 ) ) ;
#15647 = CARTESIAN_POINT ( 'NONE',  ( 0.5774900079438590739, 52.64701867748817676, -5.440088680355550821 ) ) ;
#15648 =( NAMED_UNIT ( * ) SI_UNIT ( $, .STERADIAN. ) SOLID_ANGLE_UNIT ( ) );
#15649 = CARTESIAN_POINT ( 'NONE',  ( 10.00000000000000178, 3.053748834913967425, 14.16423886937410082 ) ) ;
#15650 = CARTESIAN_POINT ( 'NONE',  ( 5.810213597521796558, 0.04962897357397456216, -13.56092647078870606 ) ) ;
#15651 = CARTESIAN_POINT ( 'NONE',  ( 1.472469842513823179, 60.59226448433412315, -4.923371831947296329 ) ) ;
#15652 = EDGE_LOOP ( 'NONE', ( #34778, #33299, #29678, #6761 ) ) ;
#15653 = VERTEX_POINT ( 'NONE', #15052 ) ;
#15654 = CARTESIAN_POINT ( 'NONE',  ( -0.3689425029237881626, 37.42874883491396787, 10.36894250292379027 ) ) ;
#15655 = CARTESIAN_POINT ( 'NONE',  ( 24.16423886937410614, 24.51208216824730002, -3.795296366450302550 ) ) ;
#15656 = CARTESIAN_POINT ( 'NONE',  ( 2.035157376598824452, 68.68868534415484817, 7.964842623401179544 ) ) ;
#15657 = CARTESIAN_POINT ( 'NONE',  ( 10.00000000000000178, 10.37363466993041961, 12.81628187352647608 ) ) ;
#15658 = DIRECTION ( 'NONE',  ( -0.000000000000000000, -1.000000000000000000, -0.000000000000000000 ) ) ;
#15659 = CARTESIAN_POINT ( 'NONE',  ( -11.33435148538996096, -69.53340079812301155, 4.000000000000000000 ) ) ;
#15661 = CARTESIAN_POINT ( 'NONE',  ( 6.565887622018943937, 23.08196800326375708, -12.81628187352647608 ) ) ;
#15660 = CARTESIAN_POINT ( 'NONE',  ( -0.8801773607110991993, 62.85535201082150536, -2.915334737309923874 ) ) ;
#15662 = CARTESIAN_POINT ( 'NONE',  ( -0.3689425029237898834, 31.17874883491396787, -10.36894250292378850 ) ) ;
#15663 = CARTESIAN_POINT ( 'NONE',  ( 15.44008868035555260, 14.73035201082150536, 9.422509992056143702 ) ) ;
#15664 = CARTESIAN_POINT ( 'NONE',  ( 0.5774900079438590739, 27.64701867748817676, -5.440088680355550821 ) ) ;
#15665 = CARTESIAN_POINT ( 'NONE',  ( -31.17076923076924544, 90.15384615384616041, -9.500000000000000000 ) ) ;
#15666 = CARTESIAN_POINT ( 'NONE',  ( 12.91533473730993009, 51.60535201082149825, -10.88017736071109987 ) ) ;
#15667 = CARTESIAN_POINT ( 'NONE',  ( 21.09922568453595559, 52.04030133659708923, -6.408140936763230044 ) ) ;
#15668 = CARTESIAN_POINT ( 'NONE',  ( -9.846743663894594434, -28.99106884899921255, 3.469446951953614189E-15 ) ) ;
#15669 = ORIENTED_EDGE ( 'NONE', *, *, #93405, .T. ) ;
#15670 = DIRECTION ( 'NONE',  ( 0.000000000000000000, 0.000000000000000000, -1.000000000000000000 ) ) ;
#15671 = EDGE_LOOP ( 'NONE', ( #75714, #70152, #61547, #22318 ) ) ;
#15672 = CARTESIAN_POINT ( 'NONE',  ( -7.313705784284471711, 14.49999999999999112, -13.09617149020757942 ) ) ;
#15673 = ORIENTED_EDGE ( 'NONE', *, *, #51915, .F. ) ;
#15674 = CARTESIAN_POINT ( 'NONE',  ( -12.25993886608615568, 14.49999999999999112, 8.642563219313586842 ) ) ;
#15676 = CARTESIAN_POINT ( 'NONE',  ( -4.164238869374099927, 62.01208216824728936, 3.795296366450308767 ) ) ;
#15675 = CARTESIAN_POINT ( 'NONE',  ( -4.164238869374099927, 57.01208216824731068, 3.795296366450308767 ) ) ;
#15678 = CARTESIAN_POINT ( 'NONE',  ( 1.472469842513823179, 61.42559781766745175, 4.923371831947296329 ) ) ;
#15677 = CARTESIAN_POINT ( 'NONE',  ( 18.52753015748618282, 28.92559781766745175, -4.923371831947291888 ) ) ;
#15679 = CARTESIAN_POINT ( 'NONE',  ( 19.80832241502127644, 49.75868815902069997, 6.499999999999990230 ) ) ;
#15680 = EDGE_CURVE ( 'NONE', #52137, #43409, #84267, .T. ) ;
#15681 = AXIS2_PLACEMENT_3D ( 'NONE', #49182, #64167, #20159 ) ;
#15682 = CARTESIAN_POINT ( 'NONE',  ( 13.43411237798105340, 10.58196800326375353, 12.81628187352647963 ) ) ;
#15683 = CARTESIAN_POINT ( 'NONE',  ( -3.434112377981047626, 20.16530133659709634, 12.81628187352647963 ) ) ;
#15684 = ORIENTED_EDGE ( 'NONE', *, *, #72107, .T. ) ;
#15685 = CARTESIAN_POINT ( 'NONE',  ( -4.164238869374099039, 36.80374883491396787, 8.674139862899312516E-16 ) ) ;
#15686 = CARTESIAN_POINT ( 'NONE',  ( 22.26659068614894466, 48.88708216824730357, 7.082119434687054849 ) ) ;
#15687 = ORIENTED_EDGE ( 'NONE', *, *, #66846, .T. ) ;
#15688 = CARTESIAN_POINT ( 'NONE',  ( 16.40814093676323893, 55.79030133659708923, 11.09922568453595026 ) ) ;
#15689 = AXIS2_PLACEMENT_3D ( 'NONE', #19127, #2189, #48143 ) ;
#15690 = CARTESIAN_POINT ( 'NONE',  ( 17.96484262340118221, 24.93868534415484461, 7.964842623401181321 ) ) ;
#15691 = CARTESIAN_POINT ( 'NONE',  ( 10.00000000000000178, 47.25893115100078745, 9.846743663894594434 ) ) ;
#15692 = CARTESIAN_POINT ( 'NONE',  ( 10.00000000000000000, 26.81368534415484106, -10.88017736071110342 ) ) ;
#15693 = DIRECTION ( 'NONE',  ( 0.6186827199538796895, 0.6777609120374844531, -0.3973308925122567281 ) ) ;
#15694 = CARTESIAN_POINT ( 'NONE',  ( 10.00000000000000000, 59.75893115100078745, -9.846743663894594434 ) ) ;
#15695 = CARTESIAN_POINT ( 'NONE',  ( 17.20831665107776587, 52.88393115100078035, 7.208316651077764980 ) ) ;
#15696 = STYLED_ITEM ( 'NONE', ( #55732 ), #59598 ) ;
#15697 =( GEOMETRIC_REPRESENTATION_CONTEXT ( 3 ) GLOBAL_UNCERTAINTY_ASSIGNED_CONTEXT ( ( #9233 ) ) GLOBAL_UNIT_ASSIGNED_CONTEXT ( ( #25621, #94590, #57082 ) ) REPRESENTATION_CONTEXT ( 'NONE', 'WORKASPACE' ) );
#15698 = CARTESIAN_POINT ( 'NONE',  ( 20.00000000000000355, 70.00000000000000000, 4.500000000000000888 ) ) ;
#15699 = CARTESIAN_POINT ( 'NONE',  ( -5.204170427930421283E-15, 3.438309369127513726, -11.92686044187656513 ) ) ;
#15700 = CARTESIAN_POINT ( 'NONE',  ( 7.361572987183169658, -0.03273551566588185635, -9.846743663894592657 ) ) ;
#15701 = DIRECTION ( 'NONE',  ( 0.000000000000000000, -0.000000000000000000, -1.000000000000000000 ) ) ;
#15702 = ORIENTED_EDGE ( 'NONE', *, *, #79044, .T. ) ;
#15703 = CARTESIAN_POINT ( 'NONE',  ( 8.630000001799311704, -0.01509713870841188424, 4.000000000000000000 ) ) ;
#15704 = CARTESIAN_POINT ( 'NONE',  ( 19.84674366389459266, 33.71726448433410894, -2.638427012816827677 ) ) ;
#15705 = DIRECTION ( 'NONE',  ( 0.000000000000000000, 1.000000000000000000, 0.000000000000000000 ) ) ;
#15706 = CARTESIAN_POINT ( 'NONE',  ( 22.81628187352647785, 41.41530133659708923, 3.434112377981063169 ) ) ;
#15707 = DIRECTION ( 'NONE',  ( -0.000000000000000000, -0.000000000000000000, -1.000000000000000000 ) ) ;
#15708 = EDGE_LOOP ( 'NONE', ( #28578, #8997, #20589, #12760, #46420, #17894 ) ) ;
#15709 = CARTESIAN_POINT ( 'NONE',  ( 14.04391541078765471, 3.833537969851530006E-16, -3.608107528142839637 ) ) ;
#15710 = CARTESIAN_POINT ( 'NONE',  ( -8.606322355891181886, 15.00000000000000000, -11.66967075398817322 ) ) ;
#15711 = CARTESIAN_POINT ( 'NONE',  ( 12.63842701281683034, 52.46726448433413026, 9.846743663894596210 ) ) ;
#15712 = CARTESIAN_POINT ( 'NONE',  ( 24.16423886937409904, 39.09541550158062506, 3.795296366450317205 ) ) ;
#15713 = CARTESIAN_POINT ( 'NONE',  ( 0.1532563361054100626, 55.80059781766745175, -2.638427012816831230 ) ) ;
#15714 = DIRECTION ( 'NONE',  ( 0.000000000000000000, 0.000000000000000000, 1.000000000000000000 ) ) ;
#15715 = CARTESIAN_POINT ( 'NONE',  ( 2.791683348922240793, 6.633931151000785675, 7.208316651077764092 ) ) ;
#15716 = B_SPLINE_CURVE_WITH_KNOTS ( 'NONE', 3,
 ( #8906, #63380, #23932, #54401, #39422, #25412 ),
 .UNSPECIFIED., .F., .F.,
 ( 4, 2, 4 ),
 ( 0.0002800484630364014570, 0.0006862541666483245543, 0.001092459870260247814 ),
 .UNSPECIFIED. ) ;
#15717 = CARTESIAN_POINT ( 'NONE',  ( 22.81628187352647785, 51.62363466993042493, 6.195893100308588602E-16 ) ) ;
#15718 = CARTESIAN_POINT ( 'NONE',  ( 2.917880565312948704, 2.637082168247300906, 12.26659068614894643 ) ) ;
#15719 = CARTESIAN_POINT ( 'NONE',  ( 17.20831665107776587, 49.13393115100078745, -7.208316651077762316 ) ) ;
#15720 = CARTESIAN_POINT ( 'NONE',  ( 2.035157376598824452, 53.68868534415484817, 7.964842623401179544 ) ) ;
#15721 = CARTESIAN_POINT ( 'NONE',  ( 12.63842701281683922, 39.55059781766744464, -9.846743663894590881 ) ) ;
#15722 = ITEM_DEFINED_TRANSFORMATION ( 'NONE', 'NONE', #7253,  #27931 ) ;
#15723 = CARTESIAN_POINT ( 'NONE',  ( 19.72487221294570858, 31.86607318730074567, 6.500000000000000888 ) ) ;
#15724 = EDGE_CURVE ( 'NONE', #11101, #6373, #96576, .T. ) ;
#15725 = CARTESIAN_POINT ( 'NONE',  ( 4.559911319644449179, 62.23035201082150536, -9.422509992056141925 ) ) ;
#15726 = EDGE_CURVE ( 'NONE', #44602, #51203, #58751, .T. ) ;
#15727 = ADVANCED_FACE ( 'NONE', ( #58548 ), #98703, .F. ) ;
#15728 = ORIENTED_EDGE ( 'NONE', *, *, #4857, .F. ) ;
#15729 = CARTESIAN_POINT ( 'NONE',  ( 6.767445849361155119, 0.3640475087720991820, 13.38662304974502071 ) ) ;
#15730 = CARTESIAN_POINT ( 'NONE',  ( 12.91533473730993009, 31.60535201082150891, -10.88017736071109987 ) ) ;
#15732 = CARTESIAN_POINT ( 'NONE',  ( 4.559911319644449179, 52.23035201082151247, -9.422509992056141925 ) ) ;
#15731 = CARTESIAN_POINT ( 'NONE',  ( 6.565887622018943937, 5.165301336597086568, 12.81628187352647430 ) ) ;
#15733 = CARTESIAN_POINT ( 'NONE',  ( 0.5774900079438590739, 67.64701867748817676, -5.440088680355550821 ) ) ;
#15735 = CARTESIAN_POINT ( 'NONE',  ( 20.00000000000000711, 92.98956734509515343, -4.826711383682784628 ) ) ;
#15734 = CARTESIAN_POINT ( 'NONE',  ( 15.44008868035555793, 36.39701867748816966, -9.422509992056140149 ) ) ;
#15736 = CARTESIAN_POINT ( 'NONE',  ( 0.1532563361054083140, 11.00893115100078568, 1.131784320476157264E-15 ) ) ;
#15737 = CARTESIAN_POINT ( 'NONE',  ( 17.20831665107776587, 32.88393115100078745, 7.208316651077764980 ) ) ;
#15738 = FACE_OUTER_BOUND ( 'NONE', #75596, .T. ) ;
#15739 = CARTESIAN_POINT ( 'NONE',  ( 12.26659068614894821, 13.88708216824730712, 7.082119434687044190 ) ) ;
#15740 = CARTESIAN_POINT ( 'NONE',  ( 12.63842701281683922, 64.55059781766745175, -9.846743663894590881 ) ) ;
#15741 = CARTESIAN_POINT ( 'NONE',  ( 17.08211943468705840, 60.13708216824729647, -12.26659068614894466 ) ) ;
#15742 = CARTESIAN_POINT ( 'NONE',  ( -6.000000000000009770, 40.99999999999999289, 6.250000000000000000 ) ) ;
#15743 = CARTESIAN_POINT ( 'NONE',  ( 13.79529636645030344, 28.26208216824729647, 14.16423886937410614 ) ) ;
#15744 = CARTESIAN_POINT ( 'NONE',  ( 24.16423886937410614, 54.30374883491396787, 8.672049930838204340E-16 ) ) ;
#15745 = CARTESIAN_POINT ( 'NONE',  ( 19.84674366389459266, 13.30059781766745353, 2.638427012816836559 ) ) ;
#15746 = VERTEX_POINT ( 'NONE', #89054 ) ;
#15747 = CARTESIAN_POINT ( 'NONE',  ( 5.076628168052703671, 26.84226448433411960, 8.527530157486179263 ) ) ;
#15748 = CARTESIAN_POINT ( 'NONE',  ( 12.91533473730993009, 21.60535201082150536, -10.88017736071109987 ) ) ;
#15749 = CARTESIAN_POINT ( 'NONE',  ( 5.076628168052704559, 60.17559781766745175, -8.527530157486179263 ) ) ;
#15751 = CARTESIAN_POINT ( 'NONE',  ( 0.2751277870542980231, 5.302231764288316107, 6.500000000000002665 ) ) ;
#15750 = CARTESIAN_POINT ( 'NONE',  ( 2.917880565312950480, 10.97041550158063572, -12.26659068614894821 ) ) ;
#15752 = DIRECTION ( 'NONE',  ( 0.000000000000000000, -1.000000000000000000, 0.000000000000000000 ) ) ;
#15753 = CARTESIAN_POINT ( 'NONE',  ( 19.84674366389459621, 13.50893115100078568, 7.409399052514197653E-17 ) ) ;
#15754 = CARTESIAN_POINT ( 'NONE',  ( 19.38216949554541557, 42.24863466993041783, -9.382169495545420901 ) ) ;
#15755 = CARTESIAN_POINT ( 'NONE',  ( 5.076628168052704559, 45.17559781766745175, -8.527530157486179263 ) ) ;
#15756 = ORIENTED_EDGE ( 'NONE', *, *, #98332, .T. ) ;
#15757 = CARTESIAN_POINT ( 'NONE',  ( 10.00000000000000178, 22.25893115100078745, 9.846743663894594434 ) ) ;
#15758 = EDGE_CURVE ( 'NONE', #96487, #45519, #90035, .T. ) ;
#15759 = CARTESIAN_POINT ( 'NONE',  ( 11.04400142293669518, -89.88311504651142059, -4.000000000000000000 ) ) ;
#15760 = CARTESIAN_POINT ( 'NONE',  ( 10.00000000000000178, 48.05374883491396787, 14.16423886937410082 ) ) ;
#15761 = CARTESIAN_POINT ( 'NONE',  ( 19.42250999205614193, 50.14701867748817676, 5.440088680355555262 ) ) ;
#15762 = CARTESIAN_POINT ( 'NONE',  ( -9.000000000000001776, 83.89999999999994884, 0.000000000000000000 ) ) ;
#15763 = CARTESIAN_POINT ( 'NONE',  ( 17.20831665107776587, 42.88393115100077324, 7.208316651077764980 ) ) ;
#15764 = CARTESIAN_POINT ( 'NONE',  ( 7.084665262690076126, 12.02201867748817143, -10.88017736071110164 ) ) ;
#15765 = CARTESIAN_POINT ( 'NONE',  ( 18.52753015748618282, 48.92559781766745886, -4.923371831947291888 ) ) ;
#15766 = CARTESIAN_POINT ( 'NONE',  ( 19.42250999205614193, 50.14701867748817676, 5.440088680355555262 ) ) ;
#15767 = B_SPLINE_CURVE_WITH_KNOTS ( 'NONE', 3,
 ( #4956, #12442, #75406, #37432, #67922, #66427 ),
 .UNSPECIFIED., .F., .F.,
 ( 4, 2, 4 ),
 ( 5.553824967135427403E-18, 0.0002605067024380902543, 0.0005210134048761749792 ),
 .UNSPECIFIED. ) ;
#15768 = EDGE_LOOP ( 'NONE', ( #39043, #58107, #45153, #40912 ) ) ;
#15769 = ORIENTED_EDGE ( 'NONE', *, *, #17550, .F. ) ;
#15770 = CARTESIAN_POINT ( 'NONE',  ( -0.1503990784575328643, 70.00000000000000000, -6.262539305110068177 ) ) ;
#15771 = CARTESIAN_POINT ( 'NONE',  ( 5.624999999999998224, 6.255135511184880315, -9.742785792574936821 ) ) ;
#15772 = CARTESIAN_POINT ( 'NONE',  ( 2.791683348922237240, 10.38393115100078390, -7.208316651077763204 ) ) ;
#15773 = CARTESIAN_POINT ( 'NONE',  ( 13.43411237798106583, 62.66530133659708923, -12.81628187352647252 ) ) ;
#15775 = CARTESIAN_POINT ( 'NONE',  ( 19.84674366389459266, 48.30059781766745175, 2.638427012816836559 ) ) ;
#15774 = CARTESIAN_POINT ( 'NONE',  ( 10.00000000000000178, 4.313685344154837509, 10.88017736071110342 ) ) ;
#15776 = CARTESIAN_POINT ( 'NONE',  ( 4.469999999999999751, 10.25000000000000000, -4.000000000000000000 ) ) ;
#15777 = CARTESIAN_POINT ( 'NONE',  ( -4.164238869374098151, 26.59541550158063217, -3.795296366450310543 ) ) ;
#15778 = CARTESIAN_POINT ( 'NONE',  ( -2.266590686148945544, 61.38708216824730357, -7.082119434687050408 ) ) ;
#15779 = CARTESIAN_POINT ( 'NONE',  ( 5.076628168052703671, 61.84226448433412315, 8.527530157486179263 ) ) ;
#15780 = DIRECTION ( 'NONE',  ( 0.000000000000000000, 0.000000000000000000, 1.000000000000000000 ) ) ;
#15781 = CARTESIAN_POINT ( 'NONE',  ( 20.88017736071110164, 45.35535201082149115, 2.915334737309930979 ) ) ;
#15782 = CARTESIAN_POINT ( 'NONE',  ( 7.361572987183169658, -0.03273551566588185635, -9.846743663894592657 ) ) ;
#15783 = SURFACE_SIDE_STYLE ('',( #68293 ) ) ;
#15784 = AXIS2_PLACEMENT_3D ( 'NONE', #47986, #86503, #18001 ) ;
#15785 = ORIENTED_EDGE ( 'NONE', *, *, #36578, .F. ) ;
#15786 = CARTESIAN_POINT ( 'NONE',  ( 3.591859063236761518, 54.95696800326376064, 11.09922568453594849 ) ) ;
#15787 = ORIENTED_EDGE ( 'NONE', *, *, #97123, .T. ) ;
#15788 = CARTESIAN_POINT ( 'NONE',  ( 2.791683348922240793, 6.633931151000785675, 7.208316651077764092 ) ) ;
#15789 = VERTEX_POINT ( 'NONE', #51052 ) ;
#15790 = CARTESIAN_POINT ( 'NONE',  ( 13.79529636645031943, 15.34541550158063750, -14.16423886937409904 ) ) ;
#15791 = CARTESIAN_POINT ( 'NONE',  ( 12.63842701281683922, 14.55059781766744997, -9.846743663894590881 ) ) ;
#15792 = CARTESIAN_POINT ( 'NONE',  ( 2.035157376598824452, 33.68868534415484106, 7.964842623401179544 ) ) ;
#15793 = FILL_AREA_STYLE_COLOUR ( '', #32924 ) ;
#15794 = ORIENTED_EDGE ( 'NONE', *, *, #17316, .F. ) ;
#15795 = CARTESIAN_POINT ( 'NONE',  ( 19.42250999205614193, 25.14701867748817321, 5.440088680355555262 ) ) ;
#15796 = B_SPLINE_CURVE_WITH_KNOTS ( 'NONE', 3,
 ( #32671, #16705, #55173, #85200 ),
 .UNSPECIFIED., .F., .F.,
 ( 4, 4 ),
 ( 0.000000000000000000, 0.002657014572711318551 ),
 .UNSPECIFIED. ) ;
#15797 =( BOUNDED_SURFACE ( )  B_SPLINE_SURFACE ( 3, 2, ( 
 ( #22331, #46300, #67827 ),
 ( #37829, #14835, #91296 ),
 ( #45815, #52319, #45310 ),
 ( #69300, #30786, #84791 ) ),
 .UNSPECIFIED., .F., .F., .F. ) 
 B_SPLINE_SURFACE_WITH_KNOTS ( ( 4, 4 ),
 ( 3, 3 ),
 ( 0.000000000000000000, 0.0004264778881141670364 ),
 ( 0.000000000000000000, 1.000000000000000000 ),
 .UNSPECIFIED. ) 
 GEOMETRIC_REPRESENTATION_ITEM ( )  RATIONAL_B_SPLINE_SURFACE ( (
 ( 1.000000000000000000, 0.8414823709351039183, 1.000000000000000000),
 ( 1.000000000000000000, 0.8184116177158143879, 1.000000000000000000),
 ( 1.000000000000000000, 0.7848884419355106612, 1.000000000000000000),
 ( 1.000000000000000000, 0.7411386215560255009, 1.000000000000000000) ) ) 
 REPRESENTATION_ITEM ( '' )  SURFACE ( )  );
#15798 = ORIENTED_EDGE ( 'NONE', *, *, #84556, .T. ) ;
#15799 = CARTESIAN_POINT ( 'NONE',  ( 19.42250999205614193, 35.14701867748816966, 5.440088680355555262 ) ) ;
#15800 = CARTESIAN_POINT ( 'NONE',  ( -39.69000000000001194, 92.00000000000000000, 9.500000000000000000 ) ) ;
#15801 = CARTESIAN_POINT ( 'NONE',  ( 17.62281668512000365, 48.28593319516822646, 6.500000000000063061 ) ) ;
#15802 = ORIENTED_EDGE ( 'NONE', *, *, #86156, .F. ) ;
#15803 = CARTESIAN_POINT ( 'NONE',  ( -1.099225684535947600, 13.70696800326375353, -6.408140936763238038 ) ) ;
#15804 = CARTESIAN_POINT ( 'NONE',  ( 12.63842701281683034, 12.46726448433411782, 9.846743663894596210 ) ) ;
#15806 = CYLINDRICAL_SURFACE ( 'NONE', #76909, 1.249999999999987121 ) ;
#15805 = B_SPLINE_CURVE_WITH_KNOTS ( 'NONE', 3,
 ( #7002, #53469, #82498, #59985, #37006, #90478 ),
 .UNSPECIFIED., .F., .F.,
 ( 4, 2, 4 ),
 ( 3.409110551494641268E-05, 0.0004400426677367923721, 0.0008459942299586382638 ),
 .UNSPECIFIED. ) ;
#15807 = DIRECTION ( 'NONE',  ( 0.000000000000000000, 0.000000000000000000, 1.000000000000000000 ) ) ;
#15808 = CARTESIAN_POINT ( 'NONE',  ( 18.52753015748617571, 18.09226448433411960, 4.923371831947298993 ) ) ;
#15809 = CARTESIAN_POINT ( 'NONE',  ( 19.42250999205614548, 25.98035201082150891, -5.440088680355545492 ) ) ;
#15810 = EDGE_CURVE ( 'NONE', #48181, #92979, #10963, .T. ) ;
#15811 = ORIENTED_EDGE ( 'NONE', *, *, #81515, .T. ) ;
#15812 = DIRECTION ( 'NONE',  ( -0.000000000000000000, 0.000000000000000000, 1.000000000000000000 ) ) ;
#15813 = CARTESIAN_POINT ( 'NONE',  ( 19.42250999205614193, 60.14701867748817676, 5.440088680355555262 ) ) ;
#15814 = CARTESIAN_POINT ( 'NONE',  ( 0.000000000000000000, 0.5000000000000004441, 0.000000000000000000 ) ) ;
#15815 = CARTESIAN_POINT ( 'NONE',  ( 13.43411237798106583, 57.66530133659708923, -12.81628187352647252 ) ) ;
#15816 = CARTESIAN_POINT ( 'NONE',  ( 20.88017736071110875, 60.77201867748817676, -2.915334737309920765 ) ) ;
#15817 = CARTESIAN_POINT ( 'NONE',  ( 0.6178305044545838731, 4.748634669930420493, 9.382169495545420901 ) ) ;
#15818 = VECTOR ( 'NONE', #20191, 1000.000000000000000 ) ;
#15819 = CARTESIAN_POINT ( 'NONE',  ( 2.791683348922237240, 35.38393115100079456, -7.208316651077763204 ) ) ;
#15820 = CARTESIAN_POINT ( 'NONE',  ( 22.81628187352648496, 51.83196800326376064, -3.434112377981050290 ) ) ;
#15821 = CARTESIAN_POINT ( 'NONE',  ( 2.602085213965210642E-15, 78.91966277462714174, 9.500000000000000000 ) ) ;
#15822 = CARTESIAN_POINT ( 'NONE',  ( 7.361572987183169658, 24.96726448433412315, -9.846743663894592657 ) ) ;
#15823 = CARTESIAN_POINT ( 'NONE',  ( 0.6178305044545818747, 13.49863466993041783, -9.382169495545419124 ) ) ;
#15824 = CARTESIAN_POINT ( 'NONE',  ( 19.50000000000000711, 105.0000000000000000, -5.000000000000000000 ) ) ;
#15825 = CARTESIAN_POINT ( 'NONE',  ( 17.96484262340118221, 39.93868534415484106, 7.964842623401181321 ) ) ;
#15826 = CARTESIAN_POINT ( 'NONE',  ( -1.099225684535947600, -0.4596986634029132657, 6.408140936763237150 ) ) ;
#15827 = SURFACE_STYLE_USAGE ( .BOTH. , #30806 ) ;
#15829 = CARTESIAN_POINT ( 'NONE',  ( 5.076628168052704559, 25.17559781766745175, -8.527530157486179263 ) ) ;
#15828 = AXIS2_PLACEMENT_3D ( 'NONE', #16031, #62499, #92023 ) ;
#15830 = CARTESIAN_POINT ( 'NONE',  ( 18.52753015748618282, 8.925597817667451750, -4.923371831947291888 ) ) ;
#15831 = CARTESIAN_POINT ( 'NONE',  ( 15.44008868035555260, 9.730352010821505360, 9.422509992056143702 ) ) ;
#15832 = CARTESIAN_POINT ( 'NONE',  ( 16.40814093676324603, 17.45696800326375353, -11.09922568453594671 ) ) ;
#15833 = AXIS2_PLACEMENT_3D ( 'NONE', #77163, #61654, #93642 ) ;
#15834 = B_SPLINE_CURVE_WITH_KNOTS ( 'NONE', 3,
 ( #79030, #3063, #87518, #86544, #79533, #50015 ),
 .UNSPECIFIED., .F., .F.,
 ( 4, 2, 4 ),
 ( 0.000000000000000000, 0.0002701661927229300235, 0.0005403323854458600469 ),
 .UNSPECIFIED. ) ;
#15835 = SHAPE_REPRESENTATION_RELATIONSHIP ( 'NONE' , 'NONE' ,  #51695, #95471 ) ;
#15836 = CARTESIAN_POINT ( 'NONE',  ( 5.076628168052704559, 65.17559781766745175, -8.527530157486179263 ) ) ;
#15837 = ADVANCED_FACE ( 'NONE', ( #81542 ), #97081, .T. ) ;
#15838 = CARTESIAN_POINT ( 'NONE',  ( 6.033511671488541950, -36.04540650267416879, -2.750000000001608935 ) ) ;
#15839 = CARTESIAN_POINT ( 'NONE',  ( 4.559911319644449179, 23.89701867748817321, 9.422509992056141925 ) ) ;
#15840 = CARTESIAN_POINT ( 'NONE',  ( 18.52753015748617571, 48.09226448433412315, 4.923371831947298993 ) ) ;
#15841 = ADVANCED_FACE ( 'NONE', ( #68536 ), #84522, .T. ) ;
#15842 = CARTESIAN_POINT ( 'NONE',  ( -1.926860441876563801, 49.89664270246083078, 3.195792623639529761 ) ) ;
#15843 = CARTESIAN_POINT ( 'NONE',  ( 4.559911319644449179, 23.89701867748817321, 9.422509992056141925 ) ) ;
#15844 = CARTESIAN_POINT ( 'NONE',  ( 1.472469842513823179, 6.425597817667451750, 4.923371831947296329 ) ) ;
#15845 = CARTESIAN_POINT ( 'NONE',  ( -0.8801773607111008646, 28.27201867748817321, 2.915334737309923430 ) ) ;
#15847 = SPHERICAL_SURFACE ( 'NONE', #17523, 0.2500000000000000000 ) ;
#15846 = CARTESIAN_POINT ( 'NONE',  ( -2.266590686148945544, 67.22041550158063217, 7.082119434687048631 ) ) ;
#15848 = CARTESIAN_POINT ( 'NONE',  ( 14.92337183194729633, 27.67559781766745530, 8.527530157486181039 ) ) ;
#15849 = CARTESIAN_POINT ( 'NONE',  ( -2.816281873526473856, 9.123634669930421381, 9.499525473075851096E-16 ) ) ;
#15850 = DIRECTION ( 'NONE',  ( 1.000000000000000000, 6.938893903907222067E-15, 0.000000000000000000 ) ) ;
#15851 = MECHANICAL_DESIGN_GEOMETRIC_PRESENTATION_REPRESENTATION (  '', ( #3083 ), #30171 ) ;
#15852 = CARTESIAN_POINT ( 'NONE',  ( 0.2751277870542893633, 25.30223176428832232, 6.499999999999988454 ) ) ;
#15853 = CARTESIAN_POINT ( 'NONE',  ( -7.909660991811269248, -4.175919252832432704, -4.000000000000000000 ) ) ;
#15854 = CARTESIAN_POINT ( 'NONE',  ( 22.26659068614894466, 13.88708216824730179, 7.082119434687054849 ) ) ;
#15855 = CARTESIAN_POINT ( 'NONE',  ( 7.361572987183170547, 42.05059781766745886, 9.846743663894590881 ) ) ;
#15856 = LINE ( 'NONE', #38850, #46477 ) ;
#15857 = EDGE_LOOP ( 'NONE', ( #24737, #9115, #31855, #7982, #13692, #46537 ) ) ;
#15858 = CARTESIAN_POINT ( 'NONE',  ( 24.16423886937410614, 54.51208216824730357, -3.795296366450302550 ) ) ;
#15859 = CARTESIAN_POINT ( 'NONE',  ( 10.00000000000000178, 17.25893115100078745, 9.846743663894594434 ) ) ;
#15861 = CARTESIAN_POINT ( 'NONE',  ( 12.60874940350940321, 15.00000000000000000, 7.160268045227115685 ) ) ;
#15860 = PLANE ( 'NONE',  #46655 ) ;
#15862 = CARTESIAN_POINT ( 'NONE',  ( 7.084665262690076126, 49.10535201082149825, 10.88017736071109987 ) ) ;
#15863 = CARTESIAN_POINT ( 'NONE',  ( 10.00000000000000178, 45.37363466993041783, 12.81628187352647608 ) ) ;
#15864 = CARTESIAN_POINT ( 'NONE',  ( -0.8801773607111008646, 23.27201867748817676, 2.915334737309923430 ) ) ;
#15865 = CARTESIAN_POINT ( 'NONE',  ( 22.81628187352647785, 46.41530133659708213, 3.434112377981063169 ) ) ;
#15866 = CARTESIAN_POINT ( 'NONE',  ( -2.816281873526473856, -0.8763653300695799508, 9.499525473075851096E-16 ) ) ;
#15867 = ORIENTED_EDGE ( 'NONE', *, *, #75684, .F. ) ;
#15868 = CARTESIAN_POINT ( 'NONE',  ( -0.1503990784575321704, 8.101585745166424601, 6.262539305110068177 ) ) ;
#15869 = EDGE_CURVE ( 'NONE', #1559, #82102, #76321, .T. ) ;
#15870 = CARTESIAN_POINT ( 'NONE',  ( 2.342957944459074682, 0.8396798841124157864, -6.500000000000004441 ) ) ;
#15871 = CARTESIAN_POINT ( 'NONE',  ( -2.266590686148945544, 46.38708216824730357, -7.082119434687050408 ) ) ;
#15872 = CARTESIAN_POINT ( 'NONE',  ( 6.204703633549690345, 15.76208216824730179, -14.16423886937410259 ) ) ;
#15873 = CARTESIAN_POINT ( 'NONE',  ( 19.42250999205614548, 25.98035201082150891, -5.440088680355545492 ) ) ;
#15874 = CARTESIAN_POINT ( 'NONE',  ( 7.084665262690076126, 37.02201867748817676, -10.88017736071110164 ) ) ;
#15875 = CARTESIAN_POINT ( 'NONE',  ( -14.99847009497945116, 14.63595249122789177, -0.2142307401082309548 ) ) ;
#15876 = AXIS2_PLACEMENT_3D ( 'NONE', #50545, #11074, #19556 ) ;
#15877 = CARTESIAN_POINT ( 'NONE',  ( 64.56412365047462742, 26.99999999999999645, 10.00000000000000000 ) ) ;
#15878 = CARTESIAN_POINT ( 'NONE',  ( 12.91533473730992121, 64.52201867748817676, 10.88017736071110164 ) ) ;
#15879 = CARTESIAN_POINT ( 'NONE',  ( 0.5774900079438590739, 67.64701867748817676, -5.440088680355550821 ) ) ;
#15880 = CARTESIAN_POINT ( 'NONE',  ( 13.43411237798105340, 30.58196800326374998, 12.81628187352647963 ) ) ;
#15881 = CARTESIAN_POINT ( 'NONE',  ( 5.056330833737696651, 15.00000000000000000, -13.58983143751348521 ) ) ;
#15882 = DIRECTION ( 'NONE',  ( 0.000000000000000000, 0.000000000000000000, -1.000000000000000000 ) ) ;
#15883 = CARTESIAN_POINT ( 'NONE',  ( 1.472469842513823179, 11.42559781766745175, 4.923371831947296329 ) ) ;
#15884 = CARTESIAN_POINT ( 'NONE',  ( 7.361572987183170547, 42.05059781766745886, 9.846743663894590881 ) ) ;
#15885 = CARTESIAN_POINT ( 'NONE',  ( 0.5774900079438590739, 12.64701867748817143, -5.440088680355550821 ) ) ;
#15886 = CARTESIAN_POINT ( 'NONE',  ( 21.09922568453595559, 27.04030133659708568, -6.408140936763230044 ) ) ;
#15887 = CARTESIAN_POINT ( 'NONE',  ( 12.63842701281683922, 9.550597817667449974, -9.846743663894590881 ) ) ;
#15888 = CARTESIAN_POINT ( 'NONE',  ( 20.88017736071110164, 5.355352010821502695, 2.915334737309930979 ) ) ;
#15889 = CARTESIAN_POINT ( 'NONE',  ( 0.1532563361054083140, 36.00893115100078745, 1.131784320476157264E-15 ) ) ;
#15890 = CARTESIAN_POINT ( 'NONE',  ( 19.84674366389459266, 38.71726448433412315, -2.638427012816827677 ) ) ;
#15891 = CARTESIAN_POINT ( 'NONE',  ( -0.3689425029237881626, 22.42874883491397142, 10.36894250292379027 ) ) ;
#15892 = CARTESIAN_POINT ( 'NONE',  ( 20.88017736071110164, 30.35535201082151247, 2.915334737309930979 ) ) ;
#15893 = CARTESIAN_POINT ( 'NONE',  ( 10.00000000000000000, 6.813685344154838397, -10.88017736071110342 ) ) ;
#15894 = CARTESIAN_POINT ( 'NONE',  ( -0.8801773607110991993, 37.85535201082151247, -2.915334737309923874 ) ) ;
#15895 = CARTESIAN_POINT ( 'NONE',  ( 19.42250999205614548, 30.98035201082150536, -5.440088680355545492 ) ) ;
#15896 = EDGE_LOOP ( 'NONE', ( #93097, #92273, #15316, #45080 ) ) ;
#15897 = CARTESIAN_POINT ( 'NONE',  ( 15.44008868035555260, 44.73035201082151247, 9.422509992056143702 ) ) ;
#15898 = CARTESIAN_POINT ( 'NONE',  ( 19.38216949554541202, 55.99863466993041072, 9.382169495545424454 ) ) ;
#15899 = CARTESIAN_POINT ( 'NONE',  ( 10.00000000000000000, 41.81368534415484106, -10.88017736071110342 ) ) ;
#15900 = CARTESIAN_POINT ( 'NONE',  ( 20.88017736071110519, 45.56368534415484106, 2.639326808657452039E-16 ) ) ;
#15901 = ORIENTED_EDGE ( 'NONE', *, *, #77882, .F. ) ;
#15902 = CARTESIAN_POINT ( 'NONE',  ( 20.88017736071110519, 55.56368534415484817, 2.639326808657452039E-16 ) ) ;
#15903 = CARTESIAN_POINT ( 'NONE',  ( -15.96747533562963994, -0.03417435944610275333, 0.9576679184939570488 ) ) ;
#15904 = CARTESIAN_POINT ( 'NONE',  ( 14.82269085861169167, 0.3640475087720976832, -2.299529454046960630 ) ) ;
#15905 = DIRECTION ( 'NONE',  ( -0.000000000000000000, 0.000000000000000000, 1.000000000000000000 ) ) ;
#15906 = CARTESIAN_POINT ( 'NONE',  ( -2.266590686148945544, 57.22041550158063217, 7.082119434687048631 ) ) ;
#15907 = CARTESIAN_POINT ( 'NONE',  ( -0.8801773607111009756, 63.06368534415484106, 1.068504757029289695E-15 ) ) ;
#15908 = CARTESIAN_POINT ( 'NONE',  ( -14.29484424893248473, 14.76984993772165744, 4.345072767107034828 ) ) ;
#15909 = CARTESIAN_POINT ( 'NONE',  ( -7.287667432647799259, -86.26780665046146623, -4.000000000000000000 ) ) ;
#15910 = CARTESIAN_POINT ( 'NONE',  ( 19.84674366389459621, 28.50893115100078745, 7.409399052514197653E-17 ) ) ;
#15911 = ORIENTED_EDGE ( 'NONE', *, *, #44603, .F. ) ;
#15912 = CARTESIAN_POINT ( 'NONE',  ( 1.472469842513823179, 36.42559781766745175, 4.923371831947296329 ) ) ;
#15913 = CARTESIAN_POINT ( 'NONE',  ( 4.559911319644449179, 33.89701867748817676, 9.422509992056141925 ) ) ;
#15914 = CARTESIAN_POINT ( 'NONE',  ( 14.92337183194729633, 37.67559781766745175, 8.527530157486181039 ) ) ;
#15915 = CARTESIAN_POINT ( 'NONE',  ( 16.40814093676323893, 25.79030133659708923, 11.09922568453595026 ) ) ;
#15917 = CARTESIAN_POINT ( 'NONE',  ( 17.96484262340118221, 54.93868534415484106, 7.964842623401181321 ) ) ;
#15916 = CARTESIAN_POINT ( 'NONE',  ( 66.56412365047464164, 26.99999999999998224, -9.500000000000000000 ) ) ;
#15919 = CARTESIAN_POINT ( 'NONE',  ( 10.00000000000000000, 6.813685344154838397, -10.88017736071110342 ) ) ;
#15918 = CARTESIAN_POINT ( 'NONE',  ( 17.96484262340118221, 39.93868534415484106, 7.964842623401181321 ) ) ;
#15920 = CARTESIAN_POINT ( 'NONE',  ( 2.917880565312950480, 55.97041550158063217, -12.26659068614894821 ) ) ;
#15921 = EDGE_CURVE ( 'NONE', #19669, #37030, #34745, .T. ) ;
#15922 = CARTESIAN_POINT ( 'NONE',  ( 21.09922568453595559, 22.04030133659708923, -6.408140936763230044 ) ) ;
#15923 = CYLINDRICAL_SURFACE ( 'NONE', #78670, 15.00000000000000000 ) ;
#15924 = VERTEX_POINT ( 'NONE', #77490 ) ;
#15925 = CARTESIAN_POINT ( 'NONE',  ( 21.09922568453595559, 17.04030133659708923, -6.408140936763230044 ) ) ;
#15926 = CARTESIAN_POINT ( 'NONE',  ( 20.88017736071110164, 25.35535201082150891, 2.915334737309930979 ) ) ;
#15927 = CARTESIAN_POINT ( 'NONE',  ( 10.00000000000000178, 54.31368534415484106, 10.88017736071110342 ) ) ;
#15928 = ORIENTED_EDGE ( 'NONE', *, *, #348, .T. ) ;
#15929 = STYLED_ITEM ( 'NONE', ( #47796 ), #4915 ) ;
#15930 = CARTESIAN_POINT ( 'NONE',  ( 5.076628168052704559, 0.1755978176674514724, -8.527530157486179263 ) ) ;
#15931 = CARTESIAN_POINT ( 'NONE',  ( 19.84674366389459266, 48.71726448433413026, -2.638427012816827677 ) ) ;
#15932 = CARTESIAN_POINT ( 'NONE',  ( 19.84674366389459266, 33.30059781766744464, 2.638427012816836559 ) ) ;
#15933 = CARTESIAN_POINT ( 'NONE',  ( -14.02068044289371684, 0.5000000000000004441, -5.331089937175857330 ) ) ;
#15934 = CARTESIAN_POINT ( 'NONE',  ( 2.791683348922240793, 21.63393115100078745, 7.208316651077764092 ) ) ;
#15935 = CARTESIAN_POINT ( 'NONE',  ( 19.89220837332778302, 54.74062864464239908, 6.478736007405906605 ) ) ;
#15936 = FACE_OUTER_BOUND ( 'NONE', #43012, .T. ) ;
#15938 = CARTESIAN_POINT ( 'NONE',  ( -7.993154516100878126, 14.95077488074853456, -12.39982181464625022 ) ) ;
#15937 = CARTESIAN_POINT ( 'NONE',  ( 7.361572987183170547, 12.05059781766744997, 9.846743663894590881 ) ) ;
#15939 = CARTESIAN_POINT ( 'NONE',  ( 4.823525747195460234, -6.402798798525329182, -3.999999999999998224 ) ) ;
#15941 = ORIENTED_EDGE ( 'NONE', *, *, #57670, .F. ) ;
#15940 = CARTESIAN_POINT ( 'NONE',  ( 7.361572987183170547, 52.05059781766745175, 9.846743663894590881 ) ) ;
#15942 = EDGE_CURVE ( 'NONE', #53047, #30064, #78966, .T. ) ;
#15943 = CARTESIAN_POINT ( 'NONE',  ( 22.81628187352648496, 6.831968003263753531, -3.434112377981050290 ) ) ;
#15944 = CARTESIAN_POINT ( 'NONE',  ( 20.88017736071110519, 55.56368534415484817, 2.639326808657452039E-16 ) ) ;
#15945 = CARTESIAN_POINT ( 'NONE',  ( 17.08211943468705130, 38.47041550158063217, 12.26659068614894998 ) ) ;
#15946 = EDGE_CURVE ( 'NONE', #16892, #95455, #67, .T. ) ;
#15947 = FACE_OUTER_BOUND ( 'NONE', #88835, .T. ) ;
#15948 = CARTESIAN_POINT ( 'NONE',  ( 19.67853978997394293, 89.81963405576850334, 5.461515559775651063 ) ) ;
#15949 = CARTESIAN_POINT ( 'NONE',  ( 17.08211943468705840, 40.13708216824731068, -12.26659068614894466 ) ) ;
#15950 = CARTESIAN_POINT ( 'NONE',  ( -4.164238869374098151, 61.59541550158063217, -3.795296366450310543 ) ) ;
#15951 = CARTESIAN_POINT ( 'NONE',  ( 22.26659068614895176, 29.72041550158063572, -7.082119434687042414 ) ) ;
#15953 = LINE ( 'NONE', #1462, #81304 ) ;
#15952 = CARTESIAN_POINT ( 'NONE',  ( -0.3689425029237898834, 21.17874883491396432, -10.36894250292378850 ) ) ;
#15954 = CARTESIAN_POINT ( 'NONE',  ( 0.1129803114748920007, 29.29427333184091609, -6.480634945678687586 ) ) ;
#15956 = CARTESIAN_POINT ( 'NONE',  ( 2.791683348922237240, 40.38393115100078035, -7.208316651077763204 ) ) ;
#15955 = CARTESIAN_POINT ( 'NONE',  ( -3.270119481323782828, 0.04922511925147937673, 14.38584091150419653 ) ) ;
#15957 = EDGE_LOOP ( 'NONE', ( #31871, #39002, #7905, #72984, #44582, #86746 ) ) ;
#15958 = FACE_OUTER_BOUND ( 'NONE', #30140, .T. ) ;
#15959 = CARTESIAN_POINT ( 'NONE',  ( 0.1532563361054100626, 65.80059781766745175, -2.638427012816831230 ) ) ;
#15960 = CARTESIAN_POINT ( 'NONE',  ( -0.1503990784575328643, 45.12777174578613426, 6.262539305110068177 ) ) ;
#15961 = CARTESIAN_POINT ( 'NONE',  ( 1.472469842513823179, 45.59226448433412315, -4.923371831947296329 ) ) ;
#15962 = CARTESIAN_POINT ( 'NONE',  ( -2.816281873526473856, 49.12363466993042493, 9.499525473075851096E-16 ) ) ;
#15963 = CARTESIAN_POINT ( 'NONE',  ( 12.26659068614894466, -0.2795844984193537885, -7.082119434687053960 ) ) ;
#15964 = CARTESIAN_POINT ( 'NONE',  ( 1.472469842513823179, 45.59226448433412315, -4.923371831947296329 ) ) ;
#15965 = CARTESIAN_POINT ( 'NONE',  ( 10.00000000000000178, 57.25893115100078745, 9.846743663894594434 ) ) ;
#15966 = CARTESIAN_POINT ( 'NONE',  ( 22.26659068614894466, 38.88708216824731068, 7.082119434687054849 ) ) ;
#15967 = VERTEX_POINT ( 'NONE', #47977 ) ;
#15968 = B_SPLINE_CURVE_WITH_KNOTS ( 'NONE', 3,
 ( #1383, #93334, #76372, #47332 ),
 .UNSPECIFIED., .F., .F.,
 ( 4, 4 ),
 ( 3.418109631315660599E-17, 0.002392975128318410027 ),
 .UNSPECIFIED. ) ;
#15969 = CARTESIAN_POINT ( 'NONE',  ( 20.36894250292379738, 14.92874883491396432, -10.36894250292379027 ) ) ;
#15970 = ADVANCED_FACE ( 'NONE', ( #16019 ), #39657, .T. ) ;
#15971 = CARTESIAN_POINT ( 'NONE',  ( -0.8801773607111008646, 63.27201867748817676, 2.915334737309923430 ) ) ;
#15973 = DIRECTION ( 'NONE',  ( 0.6883545756937550220, 0.000000000000000000, 0.7253743710122867450 ) ) ;
#15972 =( LENGTH_UNIT ( ) NAMED_UNIT ( * ) SI_UNIT ( .MILLI., .METRE. ) );
#15974 = CARTESIAN_POINT ( 'NONE',  ( 0.5774900079438607392, 3.480352010821504916, 5.440088680355550821 ) ) ;
#15975 = CARTESIAN_POINT ( 'NONE',  ( 22.81628187352648496, 16.83196800326374998, -3.434112377981050290 ) ) ;
#15976 = CARTESIAN_POINT ( 'NONE',  ( 6.579634127946654587, -87.99828267815715321, 4.000000000000000000 ) ) ;
#15977 = CARTESIAN_POINT ( 'NONE',  ( 19.84674366389459266, 3.300597817667451750, 2.638427012816836559 ) ) ;
#15978 = VECTOR ( 'NONE', #5299, 1000.000000000000000 ) ;
#15979 = CARTESIAN_POINT ( 'NONE',  ( -46.94000000000001194, 100.9546402834806713, -8.718409068399685324 ) ) ;
#15980 = CYLINDRICAL_SURFACE ( 'NONE', #47047, 15.00000000000000000 ) ;
#15981 = CARTESIAN_POINT ( 'NONE',  ( 24.16423886937410614, 59.30374883491397497, 8.672049930838204340E-16 ) ) ;
#15982 = CARTESIAN_POINT ( 'NONE',  ( 6.382347221874473675, 14.49999999999999112, -13.57444820018232079 ) ) ;
#15983 = CARTESIAN_POINT ( 'NONE',  ( 20.88017736071110164, 20.35535201082150891, 2.915334737309930979 ) ) ;
#15984 = CARTESIAN_POINT ( 'NONE',  ( 19.42250999205614193, 25.14701867748817321, 5.440088680355555262 ) ) ;
#15985 = CARTESIAN_POINT ( 'NONE',  ( 12.63842701281683922, 59.55059781766744464, -9.846743663894590881 ) ) ;
#15986 = CARTESIAN_POINT ( 'NONE',  ( 18.52753015748618282, 58.92559781766745886, -4.923371831947291888 ) ) ;
#15987 = CARTESIAN_POINT ( 'NONE',  ( -1.099225684535947600, 48.70696800326375353, -6.408140936763238038 ) ) ;
#15989 = VERTEX_POINT ( 'NONE', #39022 ) ;
#15988 = AXIS2_PLACEMENT_3D ( 'NONE', #54388, #16413, #16905 ) ;
#15990 = VECTOR ( 'NONE', #80953, 1000.000000000000000 ) ;
#15991 = CARTESIAN_POINT ( 'NONE',  ( 2.035157376598822676, 22.43868534415483396, -7.964842623401177768 ) ) ;
#15992 = CARTESIAN_POINT ( 'NONE',  ( 10.00000000000000178, 15.37363466993042138, 12.81628187352647608 ) ) ;
#15993 = CARTESIAN_POINT ( 'NONE',  ( 69.60148758828984228, -4.049828892140921146E-15, 9.500000000000000000 ) ) ;
#15994 = CARTESIAN_POINT ( 'NONE',  ( 2.791683348922240793, 51.63393115100078745, 7.208316651077764092 ) ) ;
#15995 = CARTESIAN_POINT ( 'NONE',  ( 0.5774900079438590739, 47.64701867748817676, -5.440088680355550821 ) ) ;
#15996 = CARTESIAN_POINT ( 'NONE',  ( 21.09922568453595559, 17.04030133659708923, -6.408140936763230044 ) ) ;
#15998 = CARTESIAN_POINT ( 'NONE',  ( -0.1503990784575328643, 70.00000000000000000, 6.262539305110068177 ) ) ;
#15997 = CARTESIAN_POINT ( 'NONE',  ( 2.035157376598822676, 62.43868534415483396, -7.964842623401177768 ) ) ;
#15999 = CARTESIAN_POINT ( 'NONE',  ( -0.03447792253739274948, 50.15514106990690379, 6.401564815979743805 ) ) ;
#16000 = ORIENTED_EDGE ( 'NONE', *, *, #87262, .T. ) ;
#16001 = CARTESIAN_POINT ( 'NONE',  ( 64.56412365047461321, -3.756725070333740926E-15, -7.000000000000000000 ) ) ;
#16002 = CARTESIAN_POINT ( 'NONE',  ( -0.8801773607111008646, 43.27201867748817676, 2.915334737309923430 ) ) ;
#16004 = CARTESIAN_POINT ( 'NONE',  ( 24.16423886937410614, 14.30374883491396787, 8.672049930838204340E-16 ) ) ;
#16003 = CARTESIAN_POINT ( 'NONE',  ( 19.38216949554541557, 42.24863466993041783, -9.382169495545420901 ) ) ;
#16005 = CARTESIAN_POINT ( 'NONE',  ( -7.750000000000000000, 41.24999999999999289, 4.250000000000000000 ) ) ;
#16006 = CARTESIAN_POINT ( 'NONE',  ( 0.1532563361054083140, 21.00893115100078745, 1.131784320476157264E-15 ) ) ;
#16007 = DIRECTION ( 'NONE',  ( 1.000000000000000000, -0.000000000000000000, 0.000000000000000000 ) ) ;
#16008 = CARTESIAN_POINT ( 'NONE',  ( 6.204703633549690345, 45.76208216824729647, -14.16423886937410259 ) ) ;
#16009 = FACE_OUTER_BOUND ( 'NONE', #60979, .T. ) ;
#16010 = CARTESIAN_POINT ( 'NONE',  ( 4.559911319644449179, 7.230352010821504471, -9.422509992056141925 ) ) ;
#16011 = CARTESIAN_POINT ( 'NONE',  ( -6.031993939708431895, -39.82530731230059473, -3.749999999998387512 ) ) ;
#16012 = ORIENTED_EDGE ( 'NONE', *, *, #58593, .T. ) ;
#16013 = ORIENTED_EDGE ( 'NONE', *, *, #46442, .F. ) ;
#16014 = CARTESIAN_POINT ( 'NONE',  ( -0.8801773607111008646, 3.272018677488171434, 2.915334737309923430 ) ) ;
#16015 = CARTESIAN_POINT ( 'NONE',  ( 4.559911319644449179, 12.23035201082150714, -9.422509992056141925 ) ) ;
#16016 = CARTESIAN_POINT ( 'NONE',  ( 2.791683348922237240, 40.38393115100078035, -7.208316651077763204 ) ) ;
#16017 = VECTOR ( 'NONE', #1096, 1000.000000000000000 ) ;
#16018 = CARTESIAN_POINT ( 'NONE',  ( 16.40814093676324603, 37.45696800326376064, -11.09922568453594671 ) ) ;
#16019 = FACE_OUTER_BOUND ( 'NONE', #3523, .T. ) ;
#16021 = CARTESIAN_POINT ( 'NONE',  ( 2.917880565312948704, 7.637082168247301794, 12.26659068614894643 ) ) ;
#16020 = CARTESIAN_POINT ( 'NONE',  ( 0.9408516040111536416, 2.466938638839759168, -6.499999999999972466 ) ) ;
#16022 = CARTESIAN_POINT ( 'NONE',  ( 15.44008868035555793, 31.39701867748817676, -9.422509992056140149 ) ) ;
#16023 = CARTESIAN_POINT ( 'NONE',  ( 19.42250999205614548, 5.980352010821504471, -5.440088680355545492 ) ) ;
#16025 = B_SPLINE_CURVE_WITH_KNOTS ( 'NONE', 3,
 ( #90160, #190, #68177, #98696, #45661, #21690 ),
 .UNSPECIFIED., .F., .F.,
 ( 4, 2, 4 ),
 ( 0.0002800124554034236863, 0.0006862178066545029931, 0.001092423157905582191 ),
 .UNSPECIFIED. ) ;
#16024 = CARTESIAN_POINT ( 'NONE',  ( 10.00000000000000178, 37.25893115100078745, 9.846743663894594434 ) ) ;
#16026 = DIRECTION ( 'NONE',  ( -0.000000000000000000, -0.000000000000000000, 1.000000000000000000 ) ) ;
#16027 = CARTESIAN_POINT ( 'NONE',  ( 1.472469842513823179, 16.42559781766745175, 4.923371831947296329 ) ) ;
#16028 = CARTESIAN_POINT ( 'NONE',  ( 8.722765153436254693, 15.00000000000000888, 11.74102699209690392 ) ) ;
#16029 = CARTESIAN_POINT ( 'NONE',  ( -6.408140936763246032, -41.70969866340291077, -11.09922568453594316 ) ) ;
#16030 = VERTEX_POINT ( 'NONE', #61998 ) ;
#16031 = CARTESIAN_POINT ( 'NONE',  ( 0.000000000000000000, 0.000000000000000000, 2.500000000000000000 ) ) ;
#16032 = ORIENTED_EDGE ( 'NONE', *, *, #3014, .F. ) ;
#16033 = CARTESIAN_POINT ( 'NONE',  ( 10.00000000000000000, 59.75893115100078745, -9.846743663894594434 ) ) ;
#16035 = CARTESIAN_POINT ( 'NONE',  ( 0.5774900079438590739, 42.64701867748816966, -5.440088680355550821 ) ) ;
#16034 = CARTESIAN_POINT ( 'NONE',  ( -0.8801773607111009756, 28.06368534415484106, 1.068504757029289695E-15 ) ) ;
#16037 = CARTESIAN_POINT ( 'NONE',  ( 0.6178305044545838731, 29.74863466993042138, 9.382169495545420901 ) ) ;
#16036 = CARTESIAN_POINT ( 'NONE',  ( 15.44008868035555260, 9.730352010821505360, 9.422509992056143702 ) ) ;
#16038 = CARTESIAN_POINT ( 'NONE',  ( 24.16423886937410614, 19.30374883491397142, 8.672049930838204340E-16 ) ) ;
#16039 = EDGE_CURVE ( 'NONE', #8246, #4144, #72904, .T. ) ;
#16040 = VECTOR ( 'NONE', #41709, 1000.000000000000000 ) ;
#16041 = CARTESIAN_POINT ( 'NONE',  ( 6.565887622018943937, 43.08196800326374643, -12.81628187352647608 ) ) ;
#16042 = ORIENTED_EDGE ( 'NONE', *, *, #5771, .F. ) ;
#16043 = CARTESIAN_POINT ( 'NONE',  ( 0.1532563361054082862, 41.21726448433411605, 2.638427012816831674 ) ) ;
#16044 = CARTESIAN_POINT ( 'NONE',  ( 15.44008868035555793, 21.39701867748817321, -9.422509992056140149 ) ) ;
#16045 = ORIENTED_EDGE ( 'NONE', *, *, #82737, .F. ) ;
#16046 = AXIS2_PLACEMENT_3D ( 'NONE', #97913, #89882, #36896 ) ;
#16047 = CARTESIAN_POINT ( 'NONE',  ( -0.8801773607111009756, 23.06368534415484106, 1.068504757029289695E-15 ) ) ;
#16048 = VERTEX_POINT ( 'NONE', #70011 ) ;
#16049 = CARTESIAN_POINT ( 'NONE',  ( -0.8801773607111008646, 58.27201867748816966, 2.915334737309923430 ) ) ;
#16050 = CIRCLE ( 'NONE', #73554, 1.000000000000000888 ) ;
#16051 = CARTESIAN_POINT ( 'NONE',  ( 0.5774900079438590739, 67.64701867748817676, -5.440088680355550821 ) ) ;
#16052 = CARTESIAN_POINT ( 'NONE',  ( 20.88017736071110875, 60.77201867748817676, -2.915334737309920765 ) ) ;
#16053 = CARTESIAN_POINT ( 'NONE',  ( 0.1532563361054083140, 16.00893115100078390, 1.131784320476157264E-15 ) ) ;
#16054 = CARTESIAN_POINT ( 'NONE',  ( 5.076628168052703671, 1.842264484334118047, 8.527530157486179263 ) ) ;
#16055 = AXIS2_PLACEMENT_3D ( 'NONE', #8905, #43823, #72842 ) ;
#16056 = DIRECTION ( 'NONE',  ( 0.6246950475544238435, 0.7808688094430307203, 0.000000000000000000 ) ) ;
#16057 = DIRECTION ( 'NONE',  ( 0.000000000000000000, 0.000000000000000000, 1.000000000000000000 ) ) ;
#16059 = VERTEX_POINT ( 'NONE', #1536 ) ;
#16058 = CARTESIAN_POINT ( 'NONE',  ( 19.84674366389459621, 3.508931151000785231, 7.409399052514197653E-17 ) ) ;
#16060 = ADVANCED_FACE ( 'NONE', ( #31980 ), #32488, .F. ) ;
#16061 = CARTESIAN_POINT ( 'NONE',  ( 0.1532563361054100626, 45.80059781766745886, -2.638427012816831230 ) ) ;
#16062 = VERTEX_POINT ( 'NONE', #64933 ) ;
#16063 = ORIENTED_EDGE ( 'NONE', *, *, #18847, .T. ) ;
#16064 = CARTESIAN_POINT ( 'NONE',  ( 7.361572987183169658, 64.96726448433412315, -9.846743663894592657 ) ) ;
#16065 = DIRECTION ( 'NONE',  ( 0.000000000000000000, 0.000000000000000000, 1.000000000000000000 ) ) ;
#16066 = CARTESIAN_POINT ( 'NONE',  ( 17.08211943468705840, 25.13708216824730357, -12.26659068614894466 ) ) ;
#16067 = VECTOR ( 'NONE', #63064, 999.9999999999998863 ) ;
#16068 = CARTESIAN_POINT ( 'NONE',  ( -0.2418659066527787949, 7.234100856612040609, -6.114288769123032985 ) ) ;
#16070 = CARTESIAN_POINT ( 'NONE',  ( 20.88017736071110519, 60.56368534415484106, 2.639326808657452039E-16 ) ) ;
#16069 = DIRECTION ( 'NONE',  ( 0.000000000000000000, 0.000000000000000000, 1.000000000000000000 ) ) ;
#16071 = CARTESIAN_POINT ( 'NONE',  ( 7.084665262690076126, 27.02201867748817676, -10.88017736071110164 ) ) ;
#16072 = CARTESIAN_POINT ( 'NONE',  ( 13.99999999999999822, 11.50000000000000000, -6.500000000000000888 ) ) ;
#16073 = VERTEX_POINT ( 'NONE', #27442 ) ;
#16074 = CARTESIAN_POINT ( 'NONE',  ( 10.00000000000000178, 2.258931151000784787, 9.846743663894594434 ) ) ;
#16075 = VECTOR ( 'NONE', #16091, 1000.000000000000114 ) ;
#16076 = CARTESIAN_POINT ( 'NONE',  ( 22.81628187352648496, 26.83196800326374998, -3.434112377981050290 ) ) ;
#16077 = CARTESIAN_POINT ( 'NONE',  ( 10.00000000000000000, 24.75893115100078745, -9.846743663894594434 ) ) ;
#16078 = DIRECTION ( 'NONE',  ( -0.000000000000000000, -1.000000000000000000, 0.000000000000000000 ) ) ;
#16079 = CARTESIAN_POINT ( 'NONE',  ( 3.591859063236763294, 13.29030133659708746, -11.09922568453595026 ) ) ;
#16080 = CARTESIAN_POINT ( 'NONE',  ( 20.15039907845753220, 40.60158574516643171, -6.262539305110077947 ) ) ;
#16081 = AXIS2_PLACEMENT_3D ( 'NONE', #83210, #90203, #68221 ) ;
#16082 = CARTESIAN_POINT ( 'NONE',  ( 1.472469842513823179, 10.59226448433411782, -4.923371831947296329 ) ) ;
#16083 = VERTEX_POINT ( 'NONE', #33943 ) ;
#16084 = ORIENTED_EDGE ( 'NONE', *, *, #69416, .T. ) ;
#16085 = CARTESIAN_POINT ( 'NONE',  ( -0.8801773607110991993, 17.85535201082150536, -2.915334737309923874 ) ) ;
#16086 = CARTESIAN_POINT ( 'NONE',  ( 20.36894250292379738, 19.92874883491396787, -10.36894250292379027 ) ) ;
#16087 = CARTESIAN_POINT ( 'NONE',  ( 12.63842701281683922, 39.55059781766744464, -9.846743663894590881 ) ) ;
#16088 =( BOUNDED_CURVE ( )  B_SPLINE_CURVE ( 2, ( #73314, #68659, #91653, #38652, #73803, #14687, #61626, #23669, #35814 ),
 .UNSPECIFIED., .F., .F. ) 
 B_SPLINE_CURVE_WITH_KNOTS ( ( 3, 2, 2, 2, 3 ),
 ( 0.7972837940830885817, 0.7976190476190476719, 0.8035714285714286031, 0.8095238095238095344, 0.8098590630597686246 ),
 .UNSPECIFIED. ) 
 CURVE ( )  GEOMETRIC_REPRESENTATION_ITEM ( )  RATIONAL_B_SPLINE_CURVE ( ( 0.9963778908391764944, 0.9980808541467923733, 1.000000000000000000, 0.9659258262890682012, 1.000000000000000000, 0.9659258262890682012, 1.000000000000000000, 0.9980808541467922623, 0.9963778908391764944 ) ) 
 REPRESENTATION_ITEM ( '' )  );
#16089 = CARTESIAN_POINT ( 'NONE',  ( 17.20831665107776587, 2.883931151000785231, 7.208316651077764980 ) ) ;
#16091 = DIRECTION ( 'NONE',  ( 0.8038568606172243891, 0.000000000000000000, -0.5948227867513316003 ) ) ;
#16090 = CARTESIAN_POINT ( 'NONE',  ( 21.09922568453594849, 51.20696800326375353, 6.408140936763242479 ) ) ;
#16092 = CARTESIAN_POINT ( 'NONE',  ( 12.91533473730993009, 31.60535201082150891, -10.88017736071109987 ) ) ;
#16093 = CARTESIAN_POINT ( 'NONE',  ( -0.9940297508535884674, -0.03417435944610275333, -14.21528771620250886 ) ) ;
#16094 = EDGE_CURVE ( 'NONE', #96185, #85865, #45458, .T. ) ;
#16095 = CARTESIAN_POINT ( 'NONE',  ( -1.099225684535947600, 14.54030133659708568, 6.408140936763237150 ) ) ;
#16096 = CARTESIAN_POINT ( 'NONE',  ( 18.52753015748617571, 38.09226448433412315, 4.923371831947298993 ) ) ;
#16097 = CARTESIAN_POINT ( 'NONE',  ( 2.915334737309921209, -3.394647989178489311, -10.88017736071110164 ) ) ;
#16098 = CARTESIAN_POINT ( 'NONE',  ( 10.00000000000000000, 42.87363466993042493, -12.81628187352647608 ) ) ;
#16099 = DIRECTION ( 'NONE',  ( -0.000000000000000000, 1.000000000000000000, -0.000000000000000000 ) ) ;
#16101 = DIRECTION ( 'NONE',  ( 1.000000000000000000, -5.818595309480553908E-17, 5.329070518200750605E-15 ) ) ;
#16100 = CARTESIAN_POINT ( 'NONE',  ( -0.8801773607111009756, 58.06368534415484106, 1.068504757029289695E-15 ) ) ;
#16102 = EDGE_CURVE ( 'NONE', #80852, #6068, #15422, .T. ) ;
#16103 = CARTESIAN_POINT ( 'NONE',  ( -14.22792531055116783, -3.140798168418944474E-15, -3.387425595041295256 ) ) ;
#16104 = CARTESIAN_POINT ( 'NONE',  ( 17.39651004071842166, 27.93575266056828355, 6.499999999999998224 ) ) ;
#16105 = CARTESIAN_POINT ( 'NONE',  ( 12.91533473730993009, 56.60535201082151247, -10.88017736071109987 ) ) ;
#16106 = CARTESIAN_POINT ( 'NONE',  ( 19.42250999205614548, 40.98035201082150536, -5.440088680355545492 ) ) ;
#16107 = DIRECTION ( 'NONE',  ( 1.000000000000000000, 0.000000000000000000, 0.000000000000000000 ) ) ;
#16108 = CARTESIAN_POINT ( 'NONE',  ( 0.5774900079438590739, 67.64701867748817676, -5.440088680355550821 ) ) ;
#16109 = CARTESIAN_POINT ( 'NONE',  ( 5.076628168052704559, 45.17559781766745175, -8.527530157486179263 ) ) ;
#16111 = CARTESIAN_POINT ( 'NONE',  ( -10.64017930668212664, 0.5000000000000004441, 10.57291749337208309 ) ) ;
#16110 = CARTESIAN_POINT ( 'NONE',  ( 2.035157376598824452, 3.688685344154837953, 7.964842623401179544 ) ) ;
#16112 = PRESENTATION_LAYER_ASSIGNMENT (  '', '', ( #225 ) ) ;
#16113 = CARTESIAN_POINT ( 'NONE',  ( 16.40814093676323893, 25.79030133659708923, 11.09922568453595026 ) ) ;
#16114 = ORIENTED_EDGE ( 'NONE', *, *, #4231, .T. ) ;
#16115 = CARTESIAN_POINT ( 'NONE',  ( 7.084665262690076126, 34.10535201082151247, 10.88017736071109987 ) ) ;
#16116 = EDGE_CURVE ( 'NONE', #46764, #9418, #18479, .T. ) ;
#16118 = CARTESIAN_POINT ( 'NONE',  ( 9.879999999999990123, 20.99999999999999645, 0.000000000000000000 ) ) ;
#16117 = CARTESIAN_POINT ( 'NONE',  ( 6.565887622018943937, 3.081968003263753531, -12.81628187352647608 ) ) ;
#16119 = CARTESIAN_POINT ( 'NONE',  ( 20.88017736071110519, 15.56368534415483751, 2.639326808657452039E-16 ) ) ;
#16120 = CARTESIAN_POINT ( 'NONE',  ( 17.96484262340118221, 26.18868534415483396, -7.964842623401177768 ) ) ;
#16121 = CARTESIAN_POINT ( 'NONE',  ( 13.79529636645030344, 38.26208216824729647, 14.16423886937410614 ) ) ;
#16122 = CARTESIAN_POINT ( 'NONE',  ( 5.076628168052704559, 25.17559781766745175, -8.527530157486179263 ) ) ;
#16123 = CARTESIAN_POINT ( 'NONE',  ( 2.035157376598824452, 53.68868534415484817, 7.964842623401179544 ) ) ;
#16124 = CARTESIAN_POINT ( 'NONE',  ( 0.9408516040111475354, 32.46693863883975695, -6.499999999999953815 ) ) ;
#16125 = CARTESIAN_POINT ( 'NONE',  ( -0.3689425029237898834, 1.178748834913967869, -10.36894250292378850 ) ) ;
#16126 = UNCERTAINTY_MEASURE_WITH_UNIT (LENGTH_MEASURE( 1.000000000000000082E-05 ), #21549, 'distance_accuracy_value', 'NONE');
#16127 = CARTESIAN_POINT ( 'NONE',  ( 14.92337183194729633, 62.67559781766745886, 8.527530157486181039 ) ) ;
#16128 = ORIENTED_EDGE ( 'NONE', *, *, #87707, .T. ) ;
#16129 = VERTEX_POINT ( 'NONE', #49952 ) ;
#16130 = CARTESIAN_POINT ( 'NONE',  ( -4.164238869374098151, 36.59541550158063217, -3.795296366450310543 ) ) ;
#16131 = CARTESIAN_POINT ( 'NONE',  ( 2.917880565312950480, 40.97041550158063217, -12.26659068614894821 ) ) ;
#16132 = CARTESIAN_POINT ( 'NONE',  ( -0.8801773607111009756, 68.06368534415484817, 1.068504757029289695E-15 ) ) ;
#16133 = CARTESIAN_POINT ( 'NONE',  ( 1.472469842513823179, 55.59226448433412315, -4.923371831947296329 ) ) ;
#16134 = CARTESIAN_POINT ( 'NONE',  ( -11.51383254012985802, -65.37322064360738239, 3.750000000000000000 ) ) ;
#16136 = CARTESIAN_POINT ( 'NONE',  ( 3.591859063236761518, 14.95696800326375531, 11.09922568453594849 ) ) ;
#16135 = CARTESIAN_POINT ( 'NONE',  ( 2.035157376598824452, 58.68868534415482685, 7.964842623401179544 ) ) ;
#16137 = CARTESIAN_POINT ( 'NONE',  ( -0.3689425029237898834, 26.17874883491396432, -10.36894250292378850 ) ) ;
#16138 = CARTESIAN_POINT ( 'NONE',  ( 10.00000000000000178, 29.31368534415483751, 10.88017736071110342 ) ) ;
#16139 = CARTESIAN_POINT ( 'NONE',  ( 17.96484262340118221, 36.18868534415484106, -7.964842623401177768 ) ) ;
#16140 = CARTESIAN_POINT ( 'NONE',  ( 20.30776406404399737, 70.00000000000000000, 6.000000000000270894 ) ) ;
#16141 = CARTESIAN_POINT ( 'NONE',  ( 19.42250999205614548, 50.98035201082151247, -5.440088680355545492 ) ) ;
#16142 = CARTESIAN_POINT ( 'NONE',  ( -4.923371831947302546, -4.824402182332542921, -8.527530157486173934 ) ) ;
#16143 = ORIENTED_EDGE ( 'NONE', *, *, #91022, .F. ) ;
#16144 = CARTESIAN_POINT ( 'NONE',  ( -5.999999999999994671, 43.00000000000000000, 4.250000000000000000 ) ) ;
#16145 = VERTEX_POINT ( 'NONE', #25982 ) ;
#16146 =( LENGTH_UNIT ( ) NAMED_UNIT ( * ) SI_UNIT ( .MILLI., .METRE. ) );
#16147 = ORIENTED_EDGE ( 'NONE', *, *, #59478, .F. ) ;
#16148 = CIRCLE ( 'NONE', #54463, 0.2500000000000004441 ) ;
#16149 = CARTESIAN_POINT ( 'NONE',  ( 22.26659068614894466, 8.887082168247300018, 7.082119434687054849 ) ) ;
#16151 = CARTESIAN_POINT ( 'NONE',  ( 2.917880565312948704, 62.63708216824730357, 12.26659068614894643 ) ) ;
#16150 = CARTESIAN_POINT ( 'NONE',  ( -4.164238869374098151, 56.59541550158063927, -3.795296366450310543 ) ) ;
#16153 = CARTESIAN_POINT ( 'NONE',  ( 12.63842701281683922, 64.55059781766745175, -9.846743663894590881 ) ) ;
#16152 = CARTESIAN_POINT ( 'NONE',  ( 7.361572987183169658, 34.96726448433411605, -9.846743663894592657 ) ) ;
#16154 = SURFACE_SIDE_STYLE ('',( #9139 ) ) ;
#16155 = VECTOR ( 'NONE', #67863, 999.9999999999998863 ) ;
#16156 = CARTESIAN_POINT ( 'NONE',  ( 20.04068437667227087, 44.71974360917720759, 6.396802510829643573 ) ) ;
#16157 = EDGE_CURVE ( 'NONE', #44682, #71137, #48964, .T. ) ;
#16158 = COLOUR_RGB ( '', 0.72549020, 0.75294118, 0.79215686) ;
#16159 = EDGE_CURVE ( 'NONE', #88013, #89546, #49192, .T. ) ;
#16160 = CARTESIAN_POINT ( 'NONE',  ( 3.591859063236761518, 4.956968003263753531, 11.09922568453594849 ) ) ;
#16161 = CARTESIAN_POINT ( 'NONE',  ( -6.408140936763246032, 28.29030133659709989, -11.09922568453594316 ) ) ;
#16162 = ORIENTED_EDGE ( 'NONE', *, *, #71749, .T. ) ;
#16163 = CARTESIAN_POINT ( 'NONE',  ( 2.917880565312950480, 40.97041550158063217, -12.26659068614894821 ) ) ;
#16164 = CARTESIAN_POINT ( 'NONE',  ( 6.204703633549690345, 42.84541550158063217, 14.16423886937410082 ) ) ;
#16165 = ORIENTED_EDGE ( 'NONE', *, *, #4287, .F. ) ;
#16166 = CARTESIAN_POINT ( 'NONE',  ( 19.42250999205614193, 25.14701867748817321, 5.440088680355555262 ) ) ;
#16167 = CARTESIAN_POINT ( 'NONE',  ( 16.40814093676323893, 60.79030133659709634, 11.09922568453595026 ) ) ;
#16168 = CARTESIAN_POINT ( 'NONE',  ( 0.5774900079438607392, 28.48035201082150891, 5.440088680355550821 ) ) ;
#16169 = CARTESIAN_POINT ( 'NONE',  ( 12.63842701281683034, 47.46726448433412315, 9.846743663894596210 ) ) ;
#16170 = CARTESIAN_POINT ( 'NONE',  ( 17.96484262340118221, 21.18868534415483396, -7.964842623401177768 ) ) ;
#16171 = CARTESIAN_POINT ( 'NONE',  ( -3.250000000000000444, 1.019547802438465656, 2.500000000000000000 ) ) ;
#16172 = CARTESIAN_POINT ( 'NONE',  ( 14.92337183194729988, 54.34226448433412315, -8.527530157486177487 ) ) ;
#16173 = CARTESIAN_POINT ( 'NONE',  ( 12.91533473730993009, 66.60535201082150536, -10.88017736071109987 ) ) ;
#16176 = ORIENTED_EDGE ( 'NONE', *, *, #19935, .T. ) ;
#16175 = VECTOR ( 'NONE', #54954, 1000.000000000000114 ) ;
#16174 = LINE ( 'NONE', #8185, #82390 ) ;
#16177 = EDGE_CURVE ( 'NONE', #97822, #43200, #90730, .T. ) ;
#16178 = DIRECTION ( 'NONE',  ( -0.000000000000000000, -1.000000000000000000, -0.000000000000000000 ) ) ;
#16179 = SURFACE_SIDE_STYLE ('',( #62638 ) ) ;
#16180 = DIRECTION ( 'NONE',  ( -1.000000000000000000, 0.000000000000000000, 0.000000000000000000 ) ) ;
#16181 = ORIENTED_EDGE ( 'NONE', *, *, #5217, .F. ) ;
#16182 = CARTESIAN_POINT ( 'NONE',  ( 8.900267494866982432, -1.043573704937230007, 4.000000000000000000 ) ) ;
#16183 = CARTESIAN_POINT ( 'NONE',  ( 0.1532563361054100626, 30.80059781766744820, -2.638427012816831230 ) ) ;
#16184 = DIRECTION ( 'NONE',  ( 0.000000000000000000, -1.000000000000000000, 0.000000000000000000 ) ) ;
#16185 = CARTESIAN_POINT ( 'NONE',  ( 16.40814093676323893, 45.79030133659708923, 11.09922568453595026 ) ) ;
#16186 = AXIS2_PLACEMENT_3D ( 'NONE', #52508, #91501, #76001 ) ;
#16187 = ADVANCED_FACE ( 'NONE', ( #34938 ), #80457, .T. ) ;
#16188 = DIRECTION ( 'NONE',  ( 0.9996573249755570378, 0.000000000000000000, 0.02617694830788287394 ) ) ;
#16189 = ORIENTED_EDGE ( 'NONE', *, *, #16876, .T. ) ;
#16190 = LINE ( 'NONE', #84201, #79550 ) ;
#16191 = CARTESIAN_POINT ( 'NONE',  ( -11.62719953690053742, 14.63606895804558583, -9.476720473301991632 ) ) ;
#16192 = CARTESIAN_POINT ( 'NONE',  ( 7.361572987183169658, 59.96726448433410894, -9.846743663894592657 ) ) ;
#16193 = CARTESIAN_POINT ( 'NONE',  ( 20.36894250292379738, 39.92874883491396787, -10.36894250292379027 ) ) ;
#16194 = CARTESIAN_POINT ( 'NONE',  ( 7.361572987183169658, 54.96726448433413026, -9.846743663894592657 ) ) ;
#16196 = CIRCLE ( 'NONE', #41754, 14.49999999999999822 ) ;
#16195 = CARTESIAN_POINT ( 'NONE',  ( -11.42945456197606724, 2.337810934421868936E-16, -9.127207413380881817 ) ) ;
#16197 = CARTESIAN_POINT ( 'NONE',  ( 12.63842701281683922, 14.55059781766744997, -9.846743663894590881 ) ) ;
#16198 = CARTESIAN_POINT ( 'NONE',  ( 19.38216949554541202, 50.99863466993042493, 9.382169495545424454 ) ) ;
#16199 = CARTESIAN_POINT ( 'NONE',  ( 0.6178305044545818747, -1.501365330069579951, -9.382169495545419124 ) ) ;
#16200 = CARTESIAN_POINT ( 'NONE',  ( 4.559911319644449179, 53.89701867748817676, 9.422509992056141925 ) ) ;
#16201 = CARTESIAN_POINT ( 'NONE',  ( 5.076628168052704559, 40.17559781766745175, -8.527530157486179263 ) ) ;
#16202 = CARTESIAN_POINT ( 'NONE',  ( 20.32896413005680714, 15.57879003517447281, -5.963430220938276349 ) ) ;
#16203 = VERTEX_POINT ( 'NONE', #88444 ) ;
#16204 = CARTESIAN_POINT ( 'NONE',  ( -12.80781515976318907, 15.00000000000000000, 6.246788841744232990 ) ) ;
#16205 = CARTESIAN_POINT ( 'NONE',  ( 2.035157376598822676, 22.43868534415483396, -7.964842623401177768 ) ) ;
#16207 = CARTESIAN_POINT ( 'NONE',  ( 19.42250999205614548, 50.98035201082151247, -5.440088680355545492 ) ) ;
#16206 = CARTESIAN_POINT ( 'NONE',  ( 19.38216949554541202, 5.998634669930420493, 9.382169495545424454 ) ) ;
#16208 = DIRECTION ( 'NONE',  ( 0.000000000000000000, 0.000000000000000000, -1.000000000000000000 ) ) ;
#16209 = CARTESIAN_POINT ( 'NONE',  ( 12.91533473730993009, 66.60535201082150536, -10.88017736071109987 ) ) ;
#16210 = CARTESIAN_POINT ( 'NONE',  ( 11.92686044187656869, 5.370456701841152203, -3.195792623639533758 ) ) ;
#16212 = DIRECTION ( 'NONE',  ( 0.000000000000000000, 0.000000000000000000, -1.000000000000000000 ) ) ;
#16211 = CARTESIAN_POINT ( 'NONE',  ( 10.00000000000000000, 36.81368534415484106, -10.88017736071110342 ) ) ;
#16213 = CARTESIAN_POINT ( 'NONE',  ( 12.63842701281683034, 37.46726448433411605, 9.846743663894596210 ) ) ;
#16214 = CARTESIAN_POINT ( 'NONE',  ( -10.36894250292378317, 27.42874883491397853, 10.36894250292379560 ) ) ;
#16215 = CARTESIAN_POINT ( 'NONE',  ( -2.816281873526473856, 4.331968003263754419, 3.434112377981055619 ) ) ;
#16217 = PRESENTATION_STYLE_ASSIGNMENT (( #46225 ) ) ;
#16216 = CARTESIAN_POINT ( 'NONE',  ( 15.44008868035555260, 14.73035201082150536, 9.422509992056143702 ) ) ;
#16219 = AXIS2_PLACEMENT_3D ( 'NONE', #5278, #88260, #50251 ) ;
#16218 = CARTESIAN_POINT ( 'NONE',  ( -10.04755927614759869, -3.159856409732166232E-15, 10.62803196998849486 ) ) ;
#16220 = CARTESIAN_POINT ( 'NONE',  ( 10.00000000000000000, 25.55374883491396787, -14.16423886937410082 ) ) ;
#16221 = EDGE_CURVE ( 'NONE', #40747, #83143, #53983, .T. ) ;
#16222 = CARTESIAN_POINT ( 'NONE',  ( 20.36894250292379738, 64.92874883491397497, -10.36894250292379027 ) ) ;
#16223 = CARTESIAN_POINT ( 'NONE',  ( 10.00000000000000000, 34.75893115100078745, -9.846743663894594434 ) ) ;
#16224 = CARTESIAN_POINT ( 'NONE',  ( 5.076628168052703671, 21.84226448433411960, 8.527530157486179263 ) ) ;
#16225 = DIRECTION ( 'NONE',  ( 1.000000000000000000, 0.000000000000000000, 0.000000000000000000 ) ) ;
#16226 = PRESENTATION_LAYER_ASSIGNMENT (  '', '', ( #64092 ) ) ;
#16227 = ORIENTED_EDGE ( 'NONE', *, *, #65518, .T. ) ;
#16228 = CARTESIAN_POINT ( 'NONE',  ( 7.361572987183169658, 24.96726448433412315, -9.846743663894592657 ) ) ;
#16229 = CARTESIAN_POINT ( 'NONE',  ( 2.035157376598822676, 22.43868534415483396, -7.964842623401177768 ) ) ;
#16230 = CARTESIAN_POINT ( 'NONE',  ( 7.361572987183170547, 62.05059781766745886, 9.846743663894590881 ) ) ;
#16232 = CARTESIAN_POINT ( 'NONE',  ( 17.75000000000000000, 77.07179676972445748, 6.250000000000000000 ) ) ;
#16231 = CARTESIAN_POINT ( 'NONE',  ( 24.16423886937410614, 14.30374883491396787, 8.672049930838204340E-16 ) ) ;
#16233 = CARTESIAN_POINT ( 'NONE',  ( 0.000000000000000000, 14.49999999999999822, 0.000000000000000000 ) ) ;
#16234 = UNCERTAINTY_MEASURE_WITH_UNIT (LENGTH_MEASURE( 1.000000000000000082E-05 ), #80918, 'distance_accuracy_value', 'NONE');
#16235 = CARTESIAN_POINT ( 'NONE',  ( 14.92337183194729988, 9.342264484334119601, -8.527530157486177487 ) ) ;
#16236 = CARTESIAN_POINT ( 'NONE',  ( 19.38216949554541557, 32.24863466993041783, -9.382169495545420901 ) ) ;
#16237 = CARTESIAN_POINT ( 'NONE',  ( 17.20831665107776587, 39.13393115100079456, -7.208316651077762316 ) ) ;
#16238 = ORIENTED_EDGE ( 'NONE', *, *, #30268, .T. ) ;
#16239 = CARTESIAN_POINT ( 'NONE',  ( 0.1532563361054082862, 16.21726448433411960, 2.638427012816831674 ) ) ;
#16240 = CARTESIAN_POINT ( 'NONE',  ( 1.042145700049403434, 34.74216108172000617, -6.499999999999937828 ) ) ;
#16241 = CARTESIAN_POINT ( 'NONE',  ( 20.36894250292379738, 54.92874883491396076, -10.36894250292379027 ) ) ;
#16242 = CARTESIAN_POINT ( 'NONE',  ( 6.204703633549690345, 2.845415501580634388, 14.16423886937410082 ) ) ;
#16243 = CARTESIAN_POINT ( 'NONE',  ( 17.96484262340118221, 51.18868534415483396, -7.964842623401177768 ) ) ;
#16244 = CARTESIAN_POINT ( 'NONE',  ( 18.52753015748618282, 33.92559781766745886, -4.923371831947291888 ) ) ;
#16245 = CARTESIAN_POINT ( 'NONE',  ( 17.96484262340118221, 19.93868534415484106, 7.964842623401181321 ) ) ;
#16246 = CARTESIAN_POINT ( 'NONE',  ( -6.732636091893168029, -88.11213685669366669, 3.750000000000000000 ) ) ;
#16247 = CARTESIAN_POINT ( 'NONE',  ( 10.00000000000000000, 54.75893115100078745, -9.846743663894594434 ) ) ;
#16248 = CARTESIAN_POINT ( 'NONE',  ( 0.5774900079438607392, 53.48035201082151247, 5.440088680355550821 ) ) ;
#16249 = FACE_OUTER_BOUND ( 'NONE', #5405, .T. ) ;
#16250 = COLOUR_RGB ( '', 0.09019608, 0.27058824, 0.51372549) ;
#16251 = EDGE_LOOP ( 'NONE', ( #27169, #70544, #76718, #85544 ) ) ;
#16252 = AXIS2_PLACEMENT_3D ( 'NONE', #15344, #70797, #85789 ) ;
#16253 = ORIENTED_EDGE ( 'NONE', *, *, #25653, .T. ) ;
#16254 = CARTESIAN_POINT ( 'NONE',  ( -10.88853822400146676, 46.97908644289115188, 3.000000000000000000 ) ) ;
#16255 = CARTESIAN_POINT ( 'NONE',  ( 2.917880565312948704, 2.637082168247300906, 12.26659068614894643 ) ) ;
#16256 = CARTESIAN_POINT ( 'NONE',  ( 10.00000000000000000, 44.75893115100078745, -9.846743663894594434 ) ) ;
#16257 = CARTESIAN_POINT ( 'NONE',  ( 7.361572987183170547, 17.05059781766745530, 9.846743663894590881 ) ) ;
#16258 = CARTESIAN_POINT ( 'NONE',  ( 3.591859063236763294, 53.29030133659708923, -11.09922568453595026 ) ) ;
#16260 = CARTESIAN_POINT ( 'NONE',  ( 5.076628168052703671, 51.84226448433412315, 8.527530157486179263 ) ) ;
#16259 = CARTESIAN_POINT ( 'NONE',  ( 20.88017736071110164, 15.35535201082150358, 2.915334737309930979 ) ) ;
#16261 = FILL_AREA_STYLE_COLOUR ( '', #71032 ) ;
#16262 = CARTESIAN_POINT ( 'NONE',  ( -4.164238869374099039, 26.80374883491397142, 8.674139862899312516E-16 ) ) ;
#16263 = CARTESIAN_POINT ( 'NONE',  ( 20.36894250292379382, 63.67874883491396787, 10.36894250292379205 ) ) ;
#16264 = CARTESIAN_POINT ( 'NONE',  ( 12.63842701281683922, 59.55059781766744464, -9.846743663894590881 ) ) ;
#16265 = ADVANCED_FACE ( 'NONE', ( #11461 ), #7749, .T. ) ;
#16266 = AXIS2_PLACEMENT_3D ( 'NONE', #97946, #4469, #4952 ) ;
#16267 = CARTESIAN_POINT ( 'NONE',  ( 0.000000000000000000, 14.49999999999999822, 0.000000000000000000 ) ) ;
#16268 = CARTESIAN_POINT ( 'NONE',  ( 2.035157376598824452, 53.68868534415484817, 7.964842623401179544 ) ) ;
#16269 = CARTESIAN_POINT ( 'NONE',  ( 0.1532563361054100626, 15.80059781766745353, -2.638427012816831230 ) ) ;
#16270 = CARTESIAN_POINT ( 'NONE',  ( -4.787219229848344249, -17.54708441702821631, 3.999999999999999112 ) ) ;
#16271 = VERTEX_POINT ( 'NONE', #95461 ) ;
#16272 = CARTESIAN_POINT ( 'NONE',  ( -14.42571047809463636, 14.76930270348881002, 3.890621016587766601 ) ) ;
#16273 = AXIS2_PLACEMENT_3D ( 'NONE', #14102, #13600, #5618 ) ;
#16274 = ORIENTED_EDGE ( 'NONE', *, *, #93009, .F. ) ;
#16275 = CARTESIAN_POINT ( 'NONE',  ( 0.1532563361054083140, 6.008931151000784787, 1.131784320476157264E-15 ) ) ;
#16276 = ORIENTED_EDGE ( 'NONE', *, *, #89073, .F. ) ;
#16277 = CARTESIAN_POINT ( 'NONE',  ( -0.3689425029237898834, 26.17874883491396432, -10.36894250292378850 ) ) ;
#16278 = CARTESIAN_POINT ( 'NONE',  ( 0.1532563361054082862, 16.21726448433411960, 2.638427012816831674 ) ) ;
#16279 = CARTESIAN_POINT ( 'NONE',  ( 15.44008868035555260, 44.73035201082151247, 9.422509992056143702 ) ) ;
#16280 = DIRECTION ( 'NONE',  ( 0.000000000000000000, 0.000000000000000000, 1.000000000000000000 ) ) ;
#16281 = VERTEX_POINT ( 'NONE', #32975 ) ;
#16282 = CARTESIAN_POINT ( 'NONE',  ( 15.44008868035555793, 21.39701867748817321, -9.422509992056140149 ) ) ;
#16283 = EDGE_CURVE ( 'NONE', #96556, #97330, #34859, .T. ) ;
#16284 = EDGE_CURVE ( 'NONE', #98330, #49831, #48475, .T. ) ;
#16285 = ORIENTED_EDGE ( 'NONE', *, *, #43351, .F. ) ;
#16286 = CARTESIAN_POINT ( 'NONE',  ( -2.266590686148945544, 2.220415501580634388, 7.082119434687048631 ) ) ;
#16287 = ORIENTED_EDGE ( 'NONE', *, *, #5973, .F. ) ;
#16288 = B_SPLINE_CURVE_WITH_KNOTS ( 'NONE', 3,
 ( #50294, #58787, #71828, #26813 ),
 .UNSPECIFIED., .F., .F.,
 ( 4, 4 ),
 ( 5.421010862427522170E-20, 0.002657014572711347174 ),
 .UNSPECIFIED. ) ;
#16289 = VERTEX_POINT ( 'NONE', #56479 ) ;
#16290 = CARTESIAN_POINT ( 'NONE',  ( -2.816281873526473856, 24.12363466993042138, 9.499525473075851096E-16 ) ) ;
#16291 = CARTESIAN_POINT ( 'NONE',  ( 18.52753015748618282, 13.92559781766745175, -4.923371831947291888 ) ) ;
#16292 = CARTESIAN_POINT ( 'NONE',  ( -0.3077640640439943676, 70.00000000000000000, -6.000000000000270894 ) ) ;
#16293 = DIRECTION ( 'NONE',  ( -2.107602052970794797E-16, 1.000000000000000000, -0.000000000000000000 ) ) ;
#16294 = CARTESIAN_POINT ( 'NONE',  ( 7.361572987183170547, 17.05059781766745530, 9.846743663894590881 ) ) ;
#16295 = CARTESIAN_POINT ( 'NONE',  ( 20.88017736071110875, 30.77201867748816966, -2.915334737309920765 ) ) ;
#16296 = VERTEX_POINT ( 'NONE', #5942 ) ;
#16297 = EDGE_CURVE ( 'NONE', #10816, #68783, #50937, .T. ) ;
#16298 = CARTESIAN_POINT ( 'NONE',  ( 16.40814093676324603, 62.45696800326376064, -11.09922568453594671 ) ) ;
#16299 = CARTESIAN_POINT ( 'NONE',  ( -0.8801773607111009756, 53.06368534415484106, 1.068504757029289695E-15 ) ) ;
#16300 = CARTESIAN_POINT ( 'NONE',  ( 0.000000000000000000, 0.5000000000000004441, 0.000000000000000000 ) ) ;
#16301 = DIRECTION ( 'NONE',  ( -5.818595309480553908E-17, -1.000000000000000000, -0.000000000000000000 ) ) ;
#16302 = CARTESIAN_POINT ( 'NONE',  ( 4.559911319644449179, 57.23035201082150536, -9.422509992056141925 ) ) ;
#16303 = CARTESIAN_POINT ( 'NONE',  ( 19.84674366389459266, 63.30059781766745886, 2.638427012816836559 ) ) ;
#16304 = EDGE_CURVE ( 'NONE', #11556, #57334, #73930, .T. ) ;
#16305 = CARTESIAN_POINT ( 'NONE',  ( 10.80773140175846159, 12.34856811493710715, 3.780460097596739288 ) ) ;
#16306 = CARTESIAN_POINT ( 'NONE',  ( 2.791683348922237240, 30.38393115100078390, -7.208316651077763204 ) ) ;
#16307 = CARTESIAN_POINT ( 'NONE',  ( -1.099225684535947600, 54.54030133659708923, 6.408140936763237150 ) ) ;
#16308 = LINE ( 'NONE', #68818, #64039 ) ;
#16309 = CARTESIAN_POINT ( 'NONE',  ( 0.1532563361054082862, 26.21726448433411605, 2.638427012816831674 ) ) ;
#16310 = CARTESIAN_POINT ( 'NONE',  ( 10.00000000000000000, 22.87363466993042138, -12.81628187352647608 ) ) ;
#16311 = FACE_OUTER_BOUND ( 'NONE', #22068, .T. ) ;
#16312 = CARTESIAN_POINT ( 'NONE',  ( 2.035157376598822676, 47.43868534415484817, -7.964842623401177768 ) ) ;
#16313 = CARTESIAN_POINT ( 'NONE',  ( 12.63842701281683034, 57.46726448433411605, 9.846743663894596210 ) ) ;
#16314 = CARTESIAN_POINT ( 'NONE',  ( 12.07856007377822394, 4.551077920620485022E-16, 8.022367888854921247 ) ) ;
#16315 = CARTESIAN_POINT ( 'NONE',  ( 18.52753015748617571, 33.09226448433411605, 4.923371831947298993 ) ) ;
#16316 = CARTESIAN_POINT ( 'NONE',  ( 12.63842701281683034, 22.46726448433411605, 9.846743663894596210 ) ) ;
#16317 = CARTESIAN_POINT ( 'NONE',  ( -0.8801773607110991993, 7.855352010821504471, -2.915334737309923874 ) ) ;
#16318 = CARTESIAN_POINT ( 'NONE',  ( 3.591859063236763294, 18.29030133659708568, -11.09922568453595026 ) ) ;
#16319 = SURFACE_STYLE_FILL_AREA ( #14857 ) ;
#16320 = CARTESIAN_POINT ( 'NONE',  ( -10.17588876012433197, 89.26462023800682744, 5.905476706514949825 ) ) ;
#16321 = CARTESIAN_POINT ( 'NONE',  ( 4.380000000000000782, 1.019547802438464768, -2.500000000000000000 ) ) ;
#16322 = CARTESIAN_POINT ( 'NONE',  ( 15.44008868035555260, 24.73035201082150891, 9.422509992056143702 ) ) ;
#16323 = AXIS2_PLACEMENT_3D ( 'NONE', #54773, #64232, #79749 ) ;
#16324 = VECTOR ( 'NONE', #59090, 1000.000000000000000 ) ;
#16325 =( NAMED_UNIT ( * ) PLANE_ANGLE_UNIT ( ) SI_UNIT ( $, .RADIAN. ) );
#16326 = CARTESIAN_POINT ( 'NONE',  ( 7.084665262690076126, 17.02201867748817676, -10.88017736071110164 ) ) ;
#16327 = CARTESIAN_POINT ( 'NONE',  ( 1.959929470562270959, 5.515283700948081957, -5.767676674365834977 ) ) ;
#16328 = CARTESIAN_POINT ( 'NONE',  ( 12.91533473730993009, 36.60535201082151247, -10.88017736071109987 ) ) ;
#16330 = CARTESIAN_POINT ( 'NONE',  ( 9.520529577030400148, 15.00000000000000888, 11.10395710204425868 ) ) ;
#16329 = CARTESIAN_POINT ( 'NONE',  ( -2.266590686148945544, 61.38708216824730357, -7.082119434687050408 ) ) ;
#16331 = AXIS2_PLACEMENT_3D ( 'NONE', #985, #92448, #23972 ) ;
#16332 = CARTESIAN_POINT ( 'NONE',  ( 5.076628168052704559, 20.17559781766745175, -8.527530157486179263 ) ) ;
#16333 = LINE ( 'NONE', #46816, #74445 ) ;
#16334 = LINE ( 'NONE', #45344, #49669 ) ;
#16335 = CARTESIAN_POINT ( 'NONE',  ( 0.1532563361054082862, 66.21726448433413736, 2.638427012816831674 ) ) ;
#16336 = CARTESIAN_POINT ( 'NONE',  ( 19.72487221294571569, 54.78217586085238366, 6.499999999999995559 ) ) ;
#16337 = CARTESIAN_POINT ( 'NONE',  ( -10.57486859793700873, -40.44919682093607349, -4.000000000000000000 ) ) ;
#16339 = VECTOR ( 'NONE', #94279, 1000.000000000000000 ) ;
#16338 = CARTESIAN_POINT ( 'NONE',  ( 6.204703633549690345, 17.84541550158063217, 14.16423886937410082 ) ) ;
#16340 = CARTESIAN_POINT ( 'NONE',  ( 14.92337183194729988, 34.34226448433411605, -8.527530157486177487 ) ) ;
#16341 = PLANE ( 'NONE',  #92788 ) ;
#16342 = ORIENTED_EDGE ( 'NONE', *, *, #16597, .F. ) ;
#16343 = CARTESIAN_POINT ( 'NONE',  ( 6.204703633549690345, 52.84541550158062506, 14.16423886937410082 ) ) ;
#16344 = CARTESIAN_POINT ( 'NONE',  ( 5.076628168052703671, 21.84226448433411960, 8.527530157486179263 ) ) ;
#16346 = CARTESIAN_POINT ( 'NONE',  ( 64.56412365047461321, 29.50000000000000000, -9.500000000000000000 ) ) ;
#16345 = FACE_OUTER_BOUND ( 'NONE', #68791, .T. ) ;
#16347 = CARTESIAN_POINT ( 'NONE',  ( 17.96484262340118221, 51.18868534415483396, -7.964842623401177768 ) ) ;
#16348 = CARTESIAN_POINT ( 'NONE',  ( 16.40814093676324603, 52.45696800326375353, -11.09922568453594671 ) ) ;
#16349 = CARTESIAN_POINT ( 'NONE',  ( 12.91533473730993009, 16.60535201082150891, -10.88017736071109987 ) ) ;
#16350 = CARTESIAN_POINT ( 'NONE',  ( 0.6178305044545838731, 44.74863466993042493, 9.382169495545420901 ) ) ;
#16351 = CARTESIAN_POINT ( 'NONE',  ( 19.84674366389459621, 63.50893115100078745, 7.409399052514197653E-17 ) ) ;
#16352 = CARTESIAN_POINT ( 'NONE',  ( 18.52753015748618282, 3.925597817667451306, -4.923371831947291888 ) ) ;
#16353 = ORIENTED_EDGE ( 'NONE', *, *, #80768, .T. ) ;
#16354 = DIRECTION ( 'NONE',  ( 2.569960705150826877E-16, -1.000000000000000000, 0.000000000000000000 ) ) ;
#16355 = FACE_OUTER_BOUND ( 'NONE', #96836, .T. ) ;
#16356 = CARTESIAN_POINT ( 'NONE',  ( 24.16423886937410614, 49.51208216824730357, -3.795296366450302550 ) ) ;
#16357 = CARTESIAN_POINT ( 'NONE',  ( 24.16423886937410614, 19.30374883491397142, 8.672049930838204340E-16 ) ) ;
#16358 = CARTESIAN_POINT ( 'NONE',  ( 10.00000000000000000, 21.81368534415484106, -10.88017736071110342 ) ) ;
#16359 = CARTESIAN_POINT ( 'NONE',  ( -0.8801773607111009756, 33.06368534415484106, 1.068504757029289695E-15 ) ) ;
#16360 = DIRECTION ( 'NONE',  ( 1.000000000000000000, 0.000000000000000000, 0.000000000000000000 ) ) ;
#16361 = DIRECTION ( 'NONE',  ( -0.000000000000000000, -0.000000000000000000, -1.000000000000000000 ) ) ;
#16362 = CARTESIAN_POINT ( 'NONE',  ( 15.44008868035555793, 61.39701867748817676, -9.422509992056140149 ) ) ;
#16363 = CARTESIAN_POINT ( 'NONE',  ( 20.15039907845753930, 70.00000000000000000, 6.262539305110068177 ) ) ;
#16364 = CARTESIAN_POINT ( 'NONE',  ( 12.63842701281683034, 17.46726448433411250, 9.846743663894596210 ) ) ;
#16365 = FACE_OUTER_BOUND ( 'NONE', #35722, .T. ) ;
#16366 = DIRECTION ( 'NONE',  ( 0.000000000000000000, 0.000000000000000000, -1.000000000000000000 ) ) ;
#16367 = CARTESIAN_POINT ( 'NONE',  ( 7.361572987183170547, 7.050597817667451750, 9.846743663894590881 ) ) ;
#16368 = CARTESIAN_POINT ( 'NONE',  ( 7.361572987183170547, 32.05059781766745175, 9.846743663894590881 ) ) ;
#16369 = EDGE_CURVE ( 'NONE', #44561, #15653, #23678, .T. ) ;
#16370 = CARTESIAN_POINT ( 'NONE',  ( 20.88017736071110519, 10.56368534415483751, 2.639326808657452039E-16 ) ) ;
#16371 =( BOUNDED_SURFACE ( )  B_SPLINE_SURFACE ( 1, 2, ( 
 ( #20322, #36306, #90782, #20816, #29288, #27810, #5329, #66297, #35810, #75780, #35309, #52294, #83289, #59295, #66802, #89792, #90278, #22308, #52780, #14814, #65801, #97323, #50818, #21810, #21310, #51803, #43792, #67801, #58800, #74286, #81311, #6303, #13807, #96335, #51307, #96831, #28308, #89308, #58294, #81789, #45285, #59785, #12806, #37312, #44291, #98321, #74795, #13306, #82790, #36805, #14312, #67299, #97826, #44782, #75288, #6798, #29775, #60285, #88810, #43306, #91275, #84291, #62246, #47244, #31751, #77254, #8763, #85262, #22797, #61267, #60773, #15790, #53275, #30271, #92752, #1298, #7796, #91775, #24277, #24764, #77745, #32239, #38780, #39765, #38292, #83782, #9258, #54741, #46278, #47742, #92268, #46759, #16769, #68787, #76763, #69279, #23297, #70265, #62738, #76281, #15305, #801, #98818, #37802, #61750, #8283, #39280, #23792, #319, #1781, #85756, #54257, #69768, #93238, #55242, #17267, #68299, #30761, #53775, #31254, #45790, #7303, #84768, #16277, #79225, #78742, #18736, #26707, #41255, #71730, #57696, #34696, #41739, #48233, #34198, #72210, #63232, #3240, #79720, #40255, #65189, #86243, #70762, #78239, #42223, #9753, #55752, #49216, #87213, #95202, #17756, #40743, #71247, #33706, #80205, #10736, #63719, #27194, #10250, #94721, #95711, #2276, #19215, #88196, #19705, #86739, #64206, #49696, #2770, #72689, #57202, #64691, #11220, #32732, #33224, #94222, #3738, #93735, #25269, #25752, #11711, #56246, #87699, #18241, #26228, #56721, #48722, #4226, #28679, #82671, #43189, #42707, #52177, #29168, #13187, #59173, #37195, #20196, #90657, #58684, #73185, #50192, #20698, #67686, #97211, #36691, #5700, #35693, #36186, #5209, #66686, #88688, #21191, #73677, #44168, #89678, #43679, #74676, #74166, #51690, #58176, #82169, #13682, #81672, #6187, #67179, #97702, #59669, #50698, #90161, #96711, #21691, #14187, #44671, #51190, #75165, #66177, #6675, #98195, #81192, #29652, #60161, #28189, #89185, #80703, #12198, #4721, #35184, #65686, #96210, #12693, #27692, #91154, #62611, #30638, #14691, #22183, #91656, #9135, #69160, #8645, #76643, #7681, #8164, #76159, #38655, #60655, #92147, #15182, #16150, #684, #15675, #46634, #84170, #46160, #30146, #31135, #23672, #53651, #61628, #54134, #84647, #77136, #22678, #39155, #68664, #69645, #1169, #31629, #23174, #62120, #38174, #92628, #24151, #53159, #54619, #85140, #191, #61147, #16648, #47120, #77620, #1664, #45662, #39651, #83664, #70143, #32113, #52664, #83166, #45161, #75665, #7176, #37679, #68178, #98697, #63114, #49100, #56608, #78125, #86619, #94599, #55114, #49577, #2161 ),
 ( #93616, #87097, #72573, #79106, #26116, #34083, #42111, #18611, #85632, #25151, #55628, #17641, #70633, #26588, #79603, #32616, #10618, #4106, #41625, #34570, #9635, #63601, #80087, #78623, #11106, #17150, #86128, #48109, #10134, #93118, #24645, #72090, #47629, #18130, #94106, #48602, #3614, #11592, #40133, #40629, #71127, #25634, #2654, #64574, #56124, #95083, #33106, #41130, #57090, #87584, #71618, #3129, #33589, #64084, #19096, #35065, #51067, #35572, #81074, #43075, #5589, #12577, #67062, #44554, #88570, #73561, #4604, #89565, #66063, #65564, #36066, #13565, #28066, #58563, #75050, #21575, #28567, #96090, #21073, #59060, #50084, #89068, #66567, #27077, #52063, #73068, #57578, #65066, #29048, #95592, #42588, #97096, #74056, #82057, #27572, #58067, #20074, #20582, #97588, #96591, #50579, #14074, #5085, #81559, #82558, #88074, #6073, #6559, #19586, #13066, #43558, #36574, #51571, #59556, #44052, #74557, #90052, #80588, #12083, #75549, #31021, #52548, #85023, #68056, #8537, #98079, #16034, #76039, #84041, #30529, #7572, #54026, #15562, #69532, #30035, #29538, #39038, #46523, #82, #46047, #24039, #7065, #77503, #45542, #60043, #37069, #38058, #54510, #76532, #23557, #91542, #22565, #23059, #91036, #53528, #37565, #8047, #60543, #61517, #38547, #61030, #92027, #69042, #576, #45040, #84537, #77023, #68551, #1046, #31513, #62012, #92512, #98586, #16536, #53034, #47013, #67567, #90541, #22073, #83053, #14573, #83550, #15073, #79489, #2041, #71976, #25998, #63967, #48488, #1550, #78008, #47507, #3022, #24539, #56970, #40015, #10989, #70026, #86982, #47993, #56008, #2537, #78504, #56493, #86511, #41509, #32502, #31995, #3501, #18492, #71015, #18007, #94969, #9515, #49465, #17527, #62502, #9016, #10017, #26471, #78990, #94480, #63495, #93504, #93997, #63000, #25520, #70518, #10496, #25028, #33471, #41008, #32991, #48980, #71509, #33958, #17028, #64463, #87473, #40518, #18987, #39534, #93005, #54999, #55515, #85517, #86014, #65947, #5472, #81446, #80959, #42964, #65449, #58438, #28448, #49964, #96474, #50452, #95974, #57950, #20461, #27457, #81934, #59429, #4484, #88457, #19474, #35944, #12458, #80469, #50951, #58945, #73445, #4971, #89932, #36448, #43442, #11968, #66440, #73943, #64947, #35451, #12947, #41994, #66940, #87958, #72458, #79971, #43930, #11477, #57465, #96974, #88953, #89446, #42471, #72955, #34951, #27946, #13443, #20960, #19957, #5955, #51447, #95476, #74428, #3991, #34456, #97460, #28925, #21448, #26964, #21952, #45924, #31388, #37940, #53407, #91906, #926, #83915, #13955, #52431, #82929, #75425, #29417, #84419 ) ),
 .UNSPECIFIED., .F., .F., .F. ) 
 B_SPLINE_SURFACE_WITH_KNOTS ( ( 2, 2 ),
 ( 3, 2, 2, 2, 2, 2, 2, 2, 2, 2, 2, 2, 2, 2, 2, 2, 2, 2, 2, 2, 2, 2, 2, 2, 2, 2, 2, 2, 2, 2, 2, 2, 2, 2, 2, 2, 2, 2, 2, 2, 2, 2, 2, 2, 2, 2, 2, 2, 2, 2, 2, 2, 2, 2, 2, 2, 2, 2, 2, 2, 2, 2, 2, 2, 2, 2, 2, 2, 2, 2, 2, 2, 2, 2, 2, 2, 2, 2, 2, 2, 2, 2, 2, 2, 2, 2, 2, 2, 2, 2, 2, 2, 2, 2, 2, 2, 2, 2, 2, 2, 2, 2, 2, 2, 2, 2, 2, 2, 2, 2, 2, 2, 2, 2, 2, 2, 2, 2, 2, 2, 2, 2, 2, 2, 2, 2, 2, 2, 2, 2, 2, 2, 2, 2, 2, 2, 2, 2, 2, 2, 2, 2, 2, 2, 2, 2, 2, 2, 2, 2, 2, 2, 2, 2, 2, 2, 2, 2, 2, 2, 2, 2, 3 ),
 ( 0.000000000000000000, 1.000000000000000000 ),
 ( 0.000000000000000000, 0.005952380952380952051, 0.01190476190476190410, 0.01785714285714285615, 0.02380952380952380820, 0.02976190476190476025, 0.03571428571428571230, 0.04166666666666666435, 0.04761904761904761640, 0.05357142857142856845, 0.05952380952380952051, 0.06547619047619047949, 0.07142857142857142461, 0.07738095238095238360, 0.08333333333333332871, 0.08928571428571428770, 0.09523809523809523281, 0.1011904761904761918, 0.1071428571428571369, 0.1130952380952380959, 0.1190476190476190410, 0.1250000000000000000, 0.1309523809523809590, 0.1369047619047619180, 0.1428571428571428492, 0.1488095238095238082, 0.1547619047619047672, 0.1607142857142857262, 0.1666666666666666574, 0.1726190476190476164, 0.1785714285714285754, 0.1845238095238095344, 0.1904761904761904656, 0.1964285714285714246, 0.2023809523809523836, 0.2083333333333333426, 0.2142857142857142738, 0.2202380952380952328, 0.2261904761904761918, 0.2321428571428571508, 0.2380952380952380820, 0.2440476190476190410, 0.2500000000000000000, 0.2559523809523809312, 0.2619047619047619180, 0.2678571428571428492, 0.2738095238095238360, 0.2797619047619047672, 0.2857142857142856984, 0.2916666666666666852, 0.2976190476190476164, 0.3035714285714285476, 0.3095238095238095344, 0.3154761904761904656, 0.3214285714285714524, 0.3273809523809523836, 0.3333333333333333148, 0.3392857142857143016, 0.3452380952380952328, 0.3511904761904761640, 0.3571428571428571508, 0.3630952380952380820, 0.3690476190476190688, 0.3750000000000000000, 0.3809523809523809312, 0.3869047619047619180, 0.3928571428571428492, 0.3988095238095238360, 0.4047619047619047672, 0.4107142857142856984, 0.4166666666666666852, 0.4226190476190476164, 0.4285714285714285476, 0.4345238095238095344, 0.4404761904761904656, 0.4464285714285714524, 0.4523809523809523836, 0.4583333333333333148, 0.4642857142857143016, 0.4702380952380952328, 0.4761904761904761640, 0.4821428571428571508, 0.4880952380952380820, 0.4940476190476190688, 0.5000000000000000000, 0.5059523809523809312, 0.5119047619047618625, 0.5178571428571429047, 0.5238095238095238360, 0.5297619047619047672, 0.5357142857142856984, 0.5416666666666666297, 0.5476190476190476719, 0.5535714285714286031, 0.5595238095238095344, 0.5654761904761904656, 0.5714285714285713969, 0.5773809523809523281, 0.5833333333333333703, 0.5892857142857143016, 0.5952380952380952328, 0.6011904761904761640, 0.6071428571428570953, 0.6130952380952381375, 0.6190476190476190688, 0.6250000000000000000, 0.6309523809523809312, 0.6369047619047618625, 0.6428571428571429047, 0.6488095238095238360, 0.6547619047619047672, 0.6607142857142856984, 0.6666666666666666297, 0.6726190476190476719, 0.6785714285714286031, 0.6845238095238095344, 0.6904761904761904656, 0.6964285714285713969, 0.7023809523809523281, 0.7083333333333333703, 0.7142857142857143016, 0.7202380952380952328, 0.7261904761904761640, 0.7321428571428570953, 0.7380952380952381375, 0.7440476190476190688, 0.7500000000000000000, 0.7559523809523809312, 0.7619047619047618625, 0.7678571428571429047, 0.7738095238095238360, 0.7797619047619047672, 0.7857142857142856984, 0.7916666666666666297, 0.7976190476190476719, 0.8035714285714286031, 0.8095238095238095344, 0.8154761904761904656, 0.8214285714285713969, 0.8273809523809523281, 0.8333333333333333703, 0.8392857142857143016, 0.8452380952380952328, 0.8511904761904761640, 0.8571428571428570953, 0.8630952380952381375, 0.8690476190476190688, 0.8750000000000000000, 0.8809523809523809312, 0.8869047619047618625, 0.8928571428571429047, 0.8988095238095238360, 0.9047619047619047672, 0.9107142857142856984, 0.9166666666666666297, 0.9226190476190476719, 0.9285714285714286031, 0.9345238095238095344, 0.9404761904761904656, 0.9464285714285713969, 0.9523809523809523281, 0.9583333333333333703, 0.9642857142857143016 ),
 .UNSPECIFIED. ) 
 GEOMETRIC_REPRESENTATION_ITEM ( )  RATIONAL_B_SPLINE_SURFACE ( (
 ( 1.000000000000000000, 0.9659258262890683122, 1.000000000000000000, 0.9659258262890683122, 1.000000000000000000, 0.9659258262890683122, 1.000000000000000000, 0.9659258262890683122, 1.000000000000000000, 0.9659258262890683122, 1.000000000000000000, 0.9659258262890683122, 1.000000000000000000, 0.9659258262890683122, 1.000000000000000000, 0.9659258262890683122, 1.000000000000000000, 0.9659258262890683122, 1.000000000000000000, 0.9659258262890683122, 1.000000000000000000, 0.9659258262890683122, 1.000000000000000000, 0.9659258262890683122, 1.000000000000000000, 0.9659258262890683122, 1.000000000000000000, 0.9659258262890683122, 1.000000000000000000, 0.9659258262890683122, 1.000000000000000000, 0.9659258262890683122, 1.000000000000000000, 0.9659258262890683122, 1.000000000000000000, 0.9659258262890683122, 1.000000000000000000, 0.9659258262890683122, 1.000000000000000000, 0.9659258262890683122, 1.000000000000000000, 0.9659258262890683122, 1.000000000000000000, 0.9659258262890683122, 1.000000000000000000, 0.9659258262890683122, 1.000000000000000000, 0.9659258262890683122, 1.000000000000000000, 0.9659258262890683122, 1.000000000000000000, 0.9659258262890683122, 1.000000000000000000, 0.9659258262890683122, 1.000000000000000000, 0.9659258262890683122, 1.000000000000000000, 0.9659258262890683122, 1.000000000000000000, 0.9659258262890683122, 1.000000000000000000, 0.9659258262890683122, 1.000000000000000000, 0.9659258262890683122, 1.000000000000000000, 0.9659258262890683122, 1.000000000000000000, 0.9659258262890683122, 1.000000000000000000, 0.9659258262890683122, 1.000000000000000000, 0.9659258262890683122, 1.000000000000000000, 0.9659258262890683122, 1.000000000000000000, 0.9659258262890683122, 1.000000000000000000, 0.9659258262890683122, 1.000000000000000000, 0.9659258262890683122, 1.000000000000000000, 0.9659258262890683122, 1.000000000000000000, 0.9659258262890683122, 1.000000000000000000, 0.9659258262890683122, 1.000000000000000000, 0.9659258262890683122, 1.000000000000000000, 0.9659258262890683122, 1.000000000000000000, 0.9659258262890683122, 1.000000000000000000, 0.9659258262890683122, 1.000000000000000000, 0.9659258262890683122, 1.000000000000000000, 0.9659258262890683122, 1.000000000000000000, 0.9659258262890683122, 1.000000000000000000, 0.9659258262890683122, 1.000000000000000000, 0.9659258262890683122, 1.000000000000000000, 0.9659258262890683122, 1.000000000000000000, 0.9659258262890683122, 1.000000000000000000, 0.9659258262890683122, 1.000000000000000000, 0.9659258262890683122, 1.000000000000000000, 0.9659258262890683122, 1.000000000000000000, 0.9659258262890683122, 1.000000000000000000, 0.9659258262890683122, 1.000000000000000000, 0.9659258262890683122, 1.000000000000000000, 0.9659258262890683122, 1.000000000000000000, 0.9659258262890683122, 1.000000000000000000, 0.9659258262890683122, 1.000000000000000000, 0.9659258262890683122, 1.000000000000000000, 0.9659258262890683122, 1.000000000000000000, 0.9659258262890683122, 1.000000000000000000, 0.9659258262890683122, 1.000000000000000000, 0.9659258262890683122, 1.000000000000000000, 0.9659258262890683122, 1.000000000000000000, 0.9659258262890683122, 1.000000000000000000, 0.9659258262890683122, 1.000000000000000000, 0.9659258262890683122, 1.000000000000000000, 0.9659258262890683122, 1.000000000000000000, 0.9659258262890683122, 1.000000000000000000, 0.9659258262890683122, 1.000000000000000000, 0.9659258262890683122, 1.000000000000000000, 0.9659258262890683122, 1.000000000000000000, 0.9659258262890683122, 1.000000000000000000, 0.9659258262890683122, 1.000000000000000000, 0.9659258262890683122, 1.000000000000000000, 0.9659258262890683122, 1.000000000000000000, 0.9659258262890683122, 1.000000000000000000, 0.9659258262890683122, 1.000000000000000000, 0.9659258262890683122, 1.000000000000000000, 0.9659258262890683122, 1.000000000000000000, 0.9659258262890683122, 1.000000000000000000, 0.9659258262890683122, 1.000000000000000000, 0.9659258262890683122, 1.000000000000000000, 0.9659258262890683122, 1.000000000000000000, 0.9659258262890683122, 1.000000000000000000, 0.9659258262890683122, 1.000000000000000000, 0.9659258262890683122, 1.000000000000000000, 0.9659258262890683122, 1.000000000000000000, 0.9659258262890683122, 1.000000000000000000, 0.9659258262890683122, 1.000000000000000000, 0.9659258262890683122, 1.000000000000000000, 0.9659258262890683122, 1.000000000000000000, 0.9659258262890683122, 1.000000000000000000, 0.9659258262890683122, 1.000000000000000000, 0.9659258262890683122, 1.000000000000000000, 0.9659258262890683122, 1.000000000000000000, 0.9659258262890683122, 1.000000000000000000, 0.9659258262890683122, 1.000000000000000000, 0.9659258262890683122, 1.000000000000000000, 0.9659258262890683122, 1.000000000000000000, 0.9659258262890683122, 1.000000000000000000, 0.9659258262890683122, 1.000000000000000000, 0.9659258262890683122, 1.000000000000000000, 0.9659258262890683122, 1.000000000000000000, 0.9659258262890683122, 1.000000000000000000, 0.9659258262890683122, 1.000000000000000000, 0.9659258262890683122, 1.000000000000000000, 0.9659258262890683122, 1.000000000000000000, 0.9659258262890683122, 1.000000000000000000, 0.9659258262890683122, 1.000000000000000000, 0.9659258262890683122, 1.000000000000000000, 0.9659258262890683122, 1.000000000000000000, 0.9659258262890683122, 1.000000000000000000, 0.9659258262890683122, 1.000000000000000000, 0.9659258262890683122, 1.000000000000000000, 0.9659258262890683122, 1.000000000000000000, 0.9659258262890683122, 1.000000000000000000, 0.9659258262890683122, 1.000000000000000000, 0.9659258262890683122, 1.000000000000000000, 0.9659258262890683122, 1.000000000000000000, 0.9659258262890683122, 1.000000000000000000, 0.9659258262890683122, 1.000000000000000000, 0.9659258262890683122, 1.000000000000000000, 0.9659258262890683122, 1.000000000000000000, 0.9659258262890683122, 1.000000000000000000, 0.9659258262890683122, 1.000000000000000000, 0.9659258262890683122, 1.000000000000000000, 0.9659258262890683122, 1.000000000000000000, 0.9659258262890683122, 1.000000000000000000, 0.9659258262890683122, 1.000000000000000000, 0.9659258262890683122, 1.000000000000000000, 0.9659258262890683122, 1.000000000000000000, 0.9659258262890683122, 1.000000000000000000, 0.9659258262890683122, 1.000000000000000000, 0.9659258262890683122, 1.000000000000000000, 0.9659258262890683122, 1.000000000000000000, 0.9659258262890683122, 1.000000000000000000, 0.9659258262890683122, 1.000000000000000000, 0.9659258262890683122, 1.000000000000000000, 0.9659258262890683122, 1.000000000000000000, 0.9659258262890683122, 1.000000000000000000, 0.9659258262890683122, 1.000000000000000000, 0.9659258262890683122, 1.000000000000000000, 0.9659258262890683122, 1.000000000000000000, 0.9659258262890683122, 1.000000000000000000, 0.9659258262890683122, 1.000000000000000000, 0.9659258262890683122, 1.000000000000000000, 0.9659258262890683122, 1.000000000000000000, 0.9659258262890683122, 1.000000000000000000, 0.9659258262890683122, 1.000000000000000000, 0.9659258262890683122, 1.000000000000000000, 0.9659258262890683122, 1.000000000000000000, 0.9659258262890683122, 1.000000000000000000, 0.9659258262890683122, 1.000000000000000000, 0.9659258262890683122, 1.000000000000000000, 0.9659258262890683122, 1.000000000000000000, 0.9659258262890683122, 1.000000000000000000),
 ( 1.000000000000000000, 0.9659258262890683122, 1.000000000000000000, 0.9659258262890683122, 1.000000000000000000, 0.9659258262890683122, 1.000000000000000000, 0.9659258262890683122, 1.000000000000000000, 0.9659258262890683122, 1.000000000000000000, 0.9659258262890683122, 1.000000000000000000, 0.9659258262890683122, 1.000000000000000000, 0.9659258262890683122, 1.000000000000000000, 0.9659258262890683122, 1.000000000000000000, 0.9659258262890683122, 1.000000000000000000, 0.9659258262890683122, 1.000000000000000000, 0.9659258262890683122, 1.000000000000000000, 0.9659258262890683122, 1.000000000000000000, 0.9659258262890683122, 1.000000000000000000, 0.9659258262890683122, 1.000000000000000000, 0.9659258262890683122, 1.000000000000000000, 0.9659258262890683122, 1.000000000000000000, 0.9659258262890683122, 1.000000000000000000, 0.9659258262890683122, 1.000000000000000000, 0.9659258262890683122, 1.000000000000000000, 0.9659258262890683122, 1.000000000000000000, 0.9659258262890683122, 1.000000000000000000, 0.9659258262890683122, 1.000000000000000000, 0.9659258262890683122, 1.000000000000000000, 0.9659258262890683122, 1.000000000000000000, 0.9659258262890683122, 1.000000000000000000, 0.9659258262890683122, 1.000000000000000000, 0.9659258262890683122, 1.000000000000000000, 0.9659258262890683122, 1.000000000000000000, 0.9659258262890683122, 1.000000000000000000, 0.9659258262890683122, 1.000000000000000000, 0.9659258262890683122, 1.000000000000000000, 0.9659258262890683122, 1.000000000000000000, 0.9659258262890683122, 1.000000000000000000, 0.9659258262890683122, 1.000000000000000000, 0.9659258262890683122, 1.000000000000000000, 0.9659258262890683122, 1.000000000000000000, 0.9659258262890683122, 1.000000000000000000, 0.9659258262890683122, 1.000000000000000000, 0.9659258262890683122, 1.000000000000000000, 0.9659258262890683122, 1.000000000000000000, 0.9659258262890683122, 1.000000000000000000, 0.9659258262890683122, 1.000000000000000000, 0.9659258262890683122, 1.000000000000000000, 0.9659258262890683122, 1.000000000000000000, 0.9659258262890683122, 1.000000000000000000, 0.9659258262890683122, 1.000000000000000000, 0.9659258262890683122, 1.000000000000000000, 0.9659258262890683122, 1.000000000000000000, 0.9659258262890683122, 1.000000000000000000, 0.9659258262890683122, 1.000000000000000000, 0.9659258262890683122, 1.000000000000000000, 0.9659258262890683122, 1.000000000000000000, 0.9659258262890683122, 1.000000000000000000, 0.9659258262890683122, 1.000000000000000000, 0.9659258262890683122, 1.000000000000000000, 0.9659258262890683122, 1.000000000000000000, 0.9659258262890683122, 1.000000000000000000, 0.9659258262890683122, 1.000000000000000000, 0.9659258262890683122, 1.000000000000000000, 0.9659258262890683122, 1.000000000000000000, 0.9659258262890683122, 1.000000000000000000, 0.9659258262890683122, 1.000000000000000000, 0.9659258262890683122, 1.000000000000000000, 0.9659258262890683122, 1.000000000000000000, 0.9659258262890683122, 1.000000000000000000, 0.9659258262890683122, 1.000000000000000000, 0.9659258262890683122, 1.000000000000000000, 0.9659258262890683122, 1.000000000000000000, 0.9659258262890683122, 1.000000000000000000, 0.9659258262890683122, 1.000000000000000000, 0.9659258262890683122, 1.000000000000000000, 0.9659258262890683122, 1.000000000000000000, 0.9659258262890683122, 1.000000000000000000, 0.9659258262890683122, 1.000000000000000000, 0.9659258262890683122, 1.000000000000000000, 0.9659258262890683122, 1.000000000000000000, 0.9659258262890683122, 1.000000000000000000, 0.9659258262890683122, 1.000000000000000000, 0.9659258262890683122, 1.000000000000000000, 0.9659258262890683122, 1.000000000000000000, 0.9659258262890683122, 1.000000000000000000, 0.9659258262890683122, 1.000000000000000000, 0.9659258262890683122, 1.000000000000000000, 0.9659258262890683122, 1.000000000000000000, 0.9659258262890683122, 1.000000000000000000, 0.9659258262890683122, 1.000000000000000000, 0.9659258262890683122, 1.000000000000000000, 0.9659258262890683122, 1.000000000000000000, 0.9659258262890683122, 1.000000000000000000, 0.9659258262890683122, 1.000000000000000000, 0.9659258262890683122, 1.000000000000000000, 0.9659258262890683122, 1.000000000000000000, 0.9659258262890683122, 1.000000000000000000, 0.9659258262890683122, 1.000000000000000000, 0.9659258262890683122, 1.000000000000000000, 0.9659258262890683122, 1.000000000000000000, 0.9659258262890683122, 1.000000000000000000, 0.9659258262890683122, 1.000000000000000000, 0.9659258262890683122, 1.000000000000000000, 0.9659258262890683122, 1.000000000000000000, 0.9659258262890683122, 1.000000000000000000, 0.9659258262890683122, 1.000000000000000000, 0.9659258262890683122, 1.000000000000000000, 0.9659258262890683122, 1.000000000000000000, 0.9659258262890683122, 1.000000000000000000, 0.9659258262890683122, 1.000000000000000000, 0.9659258262890683122, 1.000000000000000000, 0.9659258262890683122, 1.000000000000000000, 0.9659258262890683122, 1.000000000000000000, 0.9659258262890683122, 1.000000000000000000, 0.9659258262890683122, 1.000000000000000000, 0.9659258262890683122, 1.000000000000000000, 0.9659258262890683122, 1.000000000000000000, 0.9659258262890683122, 1.000000000000000000, 0.9659258262890683122, 1.000000000000000000, 0.9659258262890683122, 1.000000000000000000, 0.9659258262890683122, 1.000000000000000000, 0.9659258262890683122, 1.000000000000000000, 0.9659258262890683122, 1.000000000000000000, 0.9659258262890683122, 1.000000000000000000, 0.9659258262890683122, 1.000000000000000000, 0.9659258262890683122, 1.000000000000000000, 0.9659258262890683122, 1.000000000000000000, 0.9659258262890683122, 1.000000000000000000, 0.9659258262890683122, 1.000000000000000000, 0.9659258262890683122, 1.000000000000000000, 0.9659258262890683122, 1.000000000000000000, 0.9659258262890683122, 1.000000000000000000, 0.9659258262890683122, 1.000000000000000000, 0.9659258262890683122, 1.000000000000000000, 0.9659258262890683122, 1.000000000000000000, 0.9659258262890683122, 1.000000000000000000, 0.9659258262890683122, 1.000000000000000000, 0.9659258262890683122, 1.000000000000000000, 0.9659258262890683122, 1.000000000000000000, 0.9659258262890683122, 1.000000000000000000, 0.9659258262890683122, 1.000000000000000000, 0.9659258262890683122, 1.000000000000000000, 0.9659258262890683122, 1.000000000000000000, 0.9659258262890683122, 1.000000000000000000, 0.9659258262890683122, 1.000000000000000000, 0.9659258262890683122, 1.000000000000000000, 0.9659258262890683122, 1.000000000000000000, 0.9659258262890683122, 1.000000000000000000, 0.9659258262890683122, 1.000000000000000000, 0.9659258262890683122, 1.000000000000000000, 0.9659258262890683122, 1.000000000000000000, 0.9659258262890683122, 1.000000000000000000, 0.9659258262890683122, 1.000000000000000000, 0.9659258262890683122, 1.000000000000000000, 0.9659258262890683122, 1.000000000000000000, 0.9659258262890683122, 1.000000000000000000, 0.9659258262890683122, 1.000000000000000000, 0.9659258262890683122, 1.000000000000000000, 0.9659258262890683122, 1.000000000000000000, 0.9659258262890683122, 1.000000000000000000, 0.9659258262890683122, 1.000000000000000000, 0.9659258262890683122, 1.000000000000000000, 0.9659258262890683122, 1.000000000000000000, 0.9659258262890683122, 1.000000000000000000, 0.9659258262890683122, 1.000000000000000000) ) ) 
 REPRESENTATION_ITEM ( '' )  SURFACE ( )  );
#16372 = AXIS2_PLACEMENT_3D ( 'NONE', #90417, #96980, #97968 ) ;
#16373 = CARTESIAN_POINT ( 'NONE',  ( 0.6178305044545838731, 29.74863466993042138, 9.382169495545420901 ) ) ;
#16374 = CARTESIAN_POINT ( 'NONE',  ( 17.20831665107776587, 9.133931151000787452, -7.208316651077762316 ) ) ;
#16375 = CARTESIAN_POINT ( 'NONE',  ( 11.96291822454879750, 15.00000000000000000, -8.193813980849057543 ) ) ;
#16376 = CARTESIAN_POINT ( 'NONE',  ( 5.076628168052703671, 46.84226448433412315, 8.527530157486179263 ) ) ;
#16377 = CARTESIAN_POINT ( 'NONE',  ( 5.076628168052704559, 35.17559781766745175, -8.527530157486179263 ) ) ;
#16378 = CARTESIAN_POINT ( 'NONE',  ( 22.26659068614895176, 14.72041550158063572, -7.082119434687042414 ) ) ;
#16379 = CARTESIAN_POINT ( 'NONE',  ( 2.035157376598822676, 32.43868534415483396, -7.964842623401177768 ) ) ;
#16380 = CARTESIAN_POINT ( 'NONE',  ( 20.88017736071110519, 5.563685344154837509, 2.639326808657452039E-16 ) ) ;
#16381 = CARTESIAN_POINT ( 'NONE',  ( 17.96484262340118221, 51.18868534415483396, -7.964842623401177768 ) ) ;
#16382 = CARTESIAN_POINT ( 'NONE',  ( 20.88017736071110519, 35.56368534415484106, 2.639326808657452039E-16 ) ) ;
#16383 = VERTEX_POINT ( 'NONE', #42950 ) ;
#16384 = CARTESIAN_POINT ( 'NONE',  ( 6.565887622018943937, 38.08196800326376064, -12.81628187352647608 ) ) ;
#16385 = EDGE_CURVE ( 'NONE', #88245, #43121, #85971, .T. ) ;
#16386 = CARTESIAN_POINT ( 'NONE',  ( 17.96484262340118221, 41.18868534415484106, -7.964842623401177768 ) ) ;
#16387 = VERTEX_POINT ( 'NONE', #20944 ) ;
#16388 = CARTESIAN_POINT ( 'NONE',  ( -1.099225684535947600, 54.54030133659708923, 6.408140936763237150 ) ) ;
#16389 = CARTESIAN_POINT ( 'NONE',  ( 10.00000000000000178, 49.31368534415484106, 10.88017736071110342 ) ) ;
#16390 = AXIS2_PLACEMENT_3D ( 'NONE', #78829, #31838, #23882 ) ;
#16391 = EDGE_LOOP ( 'NONE', ( #77260, #27669, #95687 ) ) ;
#16393 = ADVANCED_FACE ( 'NONE', ( #60404 ), #97446, .T. ) ;
#16392 = CARTESIAN_POINT ( 'NONE',  ( 4.559911319644449179, 53.89701867748817676, 9.422509992056141925 ) ) ;
#16394 = DIRECTION ( 'NONE',  ( 0.000000000000000000, 0.000000000000000000, 1.000000000000000000 ) ) ;
#16395 = SURFACE_STYLE_USAGE ( .BOTH. , #69392 ) ;
#16396 = CARTESIAN_POINT ( 'NONE',  ( 24.16423886937409904, 59.09541550158063217, 3.795296366450317205 ) ) ;
#16397 = CARTESIAN_POINT ( 'NONE',  ( 4.559911319644449179, 67.23035201082150536, -9.422509992056141925 ) ) ;
#16398 = CARTESIAN_POINT ( 'NONE',  ( 19.10478245763055227, 56.02576239577081196, -5.990408912944265474 ) ) ;
#16399 = EDGE_CURVE ( 'NONE', #12669, #27569, #65734, .T. ) ;
#16400 = VECTOR ( 'NONE', #56272, 1000.000000000000000 ) ;
#16401 = FACE_OUTER_BOUND ( 'NONE', #7762, .T. ) ;
#16402 = STYLED_ITEM ( 'NONE', ( #57008 ), #48631 ) ;
#16403 = CARTESIAN_POINT ( 'NONE',  ( -14.75001642003106994, 14.95037105299814506, 0.3071237627328327058 ) ) ;
#16404 = CARTESIAN_POINT ( 'NONE',  ( 12.63842701281683034, 32.46726448433412315, 9.846743663894596210 ) ) ;
#16405 = ORIENTED_EDGE ( 'NONE', *, *, #51871, .T. ) ;
#16406 = VECTOR ( 'NONE', #90913, 1000.000000000000114 ) ;
#16407 = CARTESIAN_POINT ( 'NONE',  ( 0.1532563361054083140, 36.00893115100078745, 1.131784320476157264E-15 ) ) ;
#16408 = COLOUR_RGB ( '', 0.09019608, 0.27058824, 0.51372549) ;
#16409 = CARTESIAN_POINT ( 'NONE',  ( 12.91533473730993009, 41.60535201082149825, -10.88017736071109987 ) ) ;
#16410 = CARTESIAN_POINT ( 'NONE',  ( 18.52753015748618282, 38.92559781766745175, -4.923371831947291888 ) ) ;
#16411 = CARTESIAN_POINT ( 'NONE',  ( 22.81628187352647785, 21.62363466993041783, 6.195893100308588602E-16 ) ) ;
#16413 = DIRECTION ( 'NONE',  ( 0.000000000000000000, 0.000000000000000000, 1.000000000000000000 ) ) ;
#16412 = DIRECTION ( 'NONE',  ( -0.000000000000000000, -0.000000000000000000, 1.000000000000000000 ) ) ;
#16414 = CARTESIAN_POINT ( 'NONE',  ( 17.96484262340118221, 51.18868534415483396, -7.964842623401177768 ) ) ;
#16415 = CARTESIAN_POINT ( 'NONE',  ( 22.26659068614894466, 53.88708216824731068, 7.082119434687054849 ) ) ;
#16416 = VECTOR ( 'NONE', #12666, 1000.000000000000000 ) ;
#16417 = CARTESIAN_POINT ( 'NONE',  ( -1.099225684535947600, 18.70696800326375353, -6.408140936763238038 ) ) ;
#16418 = CARTESIAN_POINT ( 'NONE',  ( 0.1532563361054082862, 51.21726448433412315, 2.638427012816831674 ) ) ;
#16419 = VERTEX_POINT ( 'NONE', #12935 ) ;
#16420 = CARTESIAN_POINT ( 'NONE',  ( 3.591859063236763294, 28.29030133659708568, -11.09922568453595026 ) ) ;
#16421 = CARTESIAN_POINT ( 'NONE',  ( 10.00000000000000178, 19.31368534415484106, 10.88017736071110342 ) ) ;
#16423 = ORIENTED_EDGE ( 'NONE', *, *, #87764, .F. ) ;
#16422 = ADVANCED_FACE ( 'NONE', ( #43915 ), #6925, .T. ) ;
#16424 = VECTOR ( 'NONE', #88045, 1000.000000000000000 ) ;
#16425 = CARTESIAN_POINT ( 'NONE',  ( 5.076628168052703671, 6.842264484334118713, 8.527530157486179263 ) ) ;
#16426 = CARTESIAN_POINT ( 'NONE',  ( 18.52753015748617571, 43.09226448433412315, 4.923371831947298993 ) ) ;
#16427 = CARTESIAN_POINT ( 'NONE',  ( 14.92337183194729633, 42.67559781766745886, 8.527530157486181039 ) ) ;
#16428 = CARTESIAN_POINT ( 'NONE',  ( -12.07856007377814223, 15.00000000000000000, -8.022367888855001183 ) ) ;
#16429 = CARTESIAN_POINT ( 'NONE',  ( 7.361572987183170547, 27.05059781766745175, 9.846743663894590881 ) ) ;
#16430 = CARTESIAN_POINT ( 'NONE',  ( -8.124115902427741176, 75.04369783535877048, 2.900000000000000355 ) ) ;
#16432 = CARTESIAN_POINT ( 'NONE',  ( 12.11331110855135762, 0.04922511925147226436, 8.421032842869534463 ) ) ;
#16431 = CARTESIAN_POINT ( 'NONE',  ( 14.92337183194729633, 7.675597817667451750, 8.527530157486181039 ) ) ;
#16433 = CARTESIAN_POINT ( 'NONE',  ( 18.72515096720571393, 41.07228050351032778, -6.499999999999974243 ) ) ;
#16435 = VERTEX_POINT ( 'NONE', #89919 ) ;
#16434 = CARTESIAN_POINT ( 'NONE',  ( 0.1532563361054082862, 41.21726448433411605, 2.638427012816831674 ) ) ;
#16436 = ADVANCED_FACE ( 'NONE', ( #59413 ), #36427, .T. ) ;
#16437 = CARTESIAN_POINT ( 'NONE',  ( 19.38216949554541557, 62.24863466993041072, -9.382169495545420901 ) ) ;
#16438 = STYLED_ITEM ( 'NONE', ( #45192 ), #83936 ) ;
#16439 = CARTESIAN_POINT ( 'NONE',  ( 21.92686044187656336, 16.97997603579417358, 3.195792623639536423 ) ) ;
#16440 = CARTESIAN_POINT ( 'NONE',  ( 21.09922568453594849, 11.20696800326375531, 6.408140936763242479 ) ) ;
#16441 = CARTESIAN_POINT ( 'NONE',  ( 10.00000000000000178, 54.31368534415484106, 10.88017736071110342 ) ) ;
#16442 = CARTESIAN_POINT ( 'NONE',  ( -4.164238869374099039, 51.80374883491396787, 8.674139862899312516E-16 ) ) ;
#16443 = CARTESIAN_POINT ( 'NONE',  ( 20.00000000000000711, 96.99991098592576577, 4.500000004388789776 ) ) ;
#16444 = CARTESIAN_POINT ( 'NONE',  ( -2.266590686148945544, 41.38708216824729647, -7.082119434687050408 ) ) ;
#16445 = CARTESIAN_POINT ( 'NONE',  ( 22.26659068614895176, 54.72041550158063217, -7.082119434687042414 ) ) ;
#16446 = CARTESIAN_POINT ( 'NONE',  ( 24.16423886937410614, 19.30374883491397142, 8.672049930838204340E-16 ) ) ;
#16448 = DIRECTION ( 'NONE',  ( 0.02970531260815257105, -0.9995586998285053149, -1.030610062851841046E-16 ) ) ;
#16447 = CARTESIAN_POINT ( 'NONE',  ( 2.917880565312948704, 27.63708216824730357, 12.26659068614894643 ) ) ;
#16449 = CARTESIAN_POINT ( 'NONE',  ( 6.004190426492125532, -34.81345361117713111, -3.750000000000000888 ) ) ;
#16451 = CARTESIAN_POINT ( 'NONE',  ( 7.361572987183169658, 44.96726448433412315, -9.846743663894592657 ) ) ;
#16450 = CARTESIAN_POINT ( 'NONE',  ( -7.750000000000000000, 80.07179676972448590, 6.250000000000000000 ) ) ;
#16452 = CARTESIAN_POINT ( 'NONE',  ( 2.035157376598822676, 42.43868534415483396, -7.964842623401177768 ) ) ;
#16453 = DIRECTION ( 'NONE',  ( 0.000000000000000000, 1.000000000000000000, 0.000000000000000000 ) ) ;
#16454 = CARTESIAN_POINT ( 'NONE',  ( 19.84674366389459266, 58.30059781766745886, 2.638427012816836559 ) ) ;
#16455 = FACE_OUTER_BOUND ( 'NONE', #68338, .T. ) ;
#16456 = CARTESIAN_POINT ( 'NONE',  ( 18.52753015748618282, 43.92559781766745175, -4.923371831947291888 ) ) ;
#16457 = CARTESIAN_POINT ( 'NONE',  ( 22.81628187352647785, 61.41530133659709634, 3.434112377981063169 ) ) ;
#16458 = CARTESIAN_POINT ( 'NONE',  ( -12.26659068614894110, -12.77958449841935717, 7.082119434687058401 ) ) ;
#16459 = CARTESIAN_POINT ( 'NONE',  ( 0.1532563361054082862, 36.21726448433410894, 2.638427012816831674 ) ) ;
#16460 = CARTESIAN_POINT ( 'NONE',  ( 2.791683348922240793, 51.63393115100078745, 7.208316651077764092 ) ) ;
#16461 = CARTESIAN_POINT ( 'NONE',  ( -2.266590686148945544, 36.38708216824730357, -7.082119434687050408 ) ) ;
#16462 = ORIENTED_EDGE ( 'NONE', *, *, #2294, .F. ) ;
#16463 = CARTESIAN_POINT ( 'NONE',  ( 20.36894250292379382, 13.67874883491396965, 10.36894250292379205 ) ) ;
#16464 = CARTESIAN_POINT ( 'NONE',  ( -6.382347221874270282, 0.3639313913011587021, -13.57444820018238829 ) ) ;
#16466 = LINE ( 'NONE', #77942, #59999 ) ;
#16465 = CARTESIAN_POINT ( 'NONE',  ( -0.1503990784575294781, 68.10158574516643171, 6.262539305110072618 ) ) ;
#16468 = VECTOR ( 'NONE', #715, 1000.000000000000000 ) ;
#16467 = CARTESIAN_POINT ( 'NONE',  ( 4.559911319644449179, 3.897018677488171434, 9.422509992056141925 ) ) ;
#16469 = CARTESIAN_POINT ( 'NONE',  ( 0.6178305044545818747, 13.49863466993041783, -9.382169495545419124 ) ) ;
#16470 = CIRCLE ( 'NONE', #29219, 0.5000000000000004441 ) ;
#16471 = CARTESIAN_POINT ( 'NONE',  ( 0.1143410931637271200, 55.21691075486304356, 6.480892540919860778 ) ) ;
#16472 = CARTESIAN_POINT ( 'NONE',  ( 20.88017736071110164, 65.35535201082150536, 2.915334737309930979 ) ) ;
#16473 = B_SPLINE_CURVE_WITH_KNOTS ( 'NONE', 3,
 ( #54339, #81370, #27872, #20386, #5395, #35870, #58357, #50877, #88878, #32316 ),
 .UNSPECIFIED., .F., .F.,
 ( 4, 3, 3, 4 ),
 ( 2.173602285337623399E-17, 0.0006253016069560831400, 0.001250604074564932782, 0.002501455912506543068 ),
 .UNSPECIFIED. ) ;
#16474 = MECHANICAL_DESIGN_GEOMETRIC_PRESENTATION_REPRESENTATION (  '', ( #27654 ), #8472 ) ;
#16475 = CARTESIAN_POINT ( 'NONE',  ( -46.94000000000001194, 103.0000000000000000, -5.997726559847112782 ) ) ;
#16476 = EDGE_CURVE ( 'NONE', #69849, #89406, #1339, .T. ) ;
#16477 = CARTESIAN_POINT ( 'NONE',  ( 0.1089645850229078172, 43.16234555792571825, 6.479102184480833415 ) ) ;
#16478 = CARTESIAN_POINT ( 'NONE',  ( 17.08211943468705130, 58.47041550158063927, 12.26659068614894998 ) ) ;
#16479 = DIRECTION ( 'NONE',  ( 0.000000000000000000, 0.000000000000000000, 1.000000000000000000 ) ) ;
#16480 = CARTESIAN_POINT ( 'NONE',  ( 17.96484262340118221, 31.18868534415483751, -7.964842623401177768 ) ) ;
#16482 = STYLED_ITEM ( 'NONE', ( #23332 ), #77518 ) ;
#16481 = CARTESIAN_POINT ( 'NONE',  ( 7.084665262690076126, 22.02201867748817321, -10.88017736071110164 ) ) ;
#16483 = CARTESIAN_POINT ( 'NONE',  ( 10.00000000000000000, 49.75893115100078745, -9.846743663894594434 ) ) ;
#16484 = CARTESIAN_POINT ( 'NONE',  ( 10.00000000000000000, 54.75893115100078745, -9.846743663894594434 ) ) ;
#16485 = CARTESIAN_POINT ( 'NONE',  ( -46.21538524526005176, 104.1852450480875802, -5.851526435683381600 ) ) ;
#16486 = CARTESIAN_POINT ( 'NONE',  ( 12.63842701281683034, 2.467264484334118269, 9.846743663894596210 ) ) ;
#16487 = ORIENTED_EDGE ( 'NONE', *, *, #71397, .T. ) ;
#16488 = EDGE_CURVE ( 'NONE', #43409, #52137, #10944, .T. ) ;
#16489 = CARTESIAN_POINT ( 'NONE',  ( 15.44008868035555260, 34.73035201082151247, 9.422509992056143702 ) ) ;
#16490 = CARTESIAN_POINT ( 'NONE',  ( 21.09922568453594849, 31.20696800326375353, 6.408140936763242479 ) ) ;
#16491 = CARTESIAN_POINT ( 'NONE',  ( -6.732636091893172470, -88.11213685669366669, 2.750000000000000000 ) ) ;
#16492 = CARTESIAN_POINT ( 'NONE',  ( 0.1532563361054100626, 65.80059781766745175, -2.638427012816831230 ) ) ;
#16493 = CARTESIAN_POINT ( 'NONE',  ( 0.5774900079438607392, 43.48035201082151247, 5.440088680355550821 ) ) ;
#16494 = CARTESIAN_POINT ( 'NONE',  ( 12.63842701281683034, 12.46726448433411782, 9.846743663894596210 ) ) ;
#16495 = CARTESIAN_POINT ( 'NONE',  ( 16.40814093676324603, 22.45696800326375353, -11.09922568453594671 ) ) ;
#16497 = CARTESIAN_POINT ( 'NONE',  ( 6.579634127946608402, -87.99828267815712479, 2.750000000000000000 ) ) ;
#16496 = CARTESIAN_POINT ( 'NONE',  ( -0.8801773607111009756, 58.06368534415484106, 1.068504757029289695E-15 ) ) ;
#16498 = CARTESIAN_POINT ( 'NONE',  ( 0.000000000000000000, 15.00000000000000000, 0.000000000000000000 ) ) ;
#16499 = EDGE_LOOP ( 'NONE', ( #43750, #65975, #90272, #26402, #61335, #42109 ) ) ;
#16500 = CARTESIAN_POINT ( 'NONE',  ( 1.274849032794292736, 47.55509018479936856, -6.499999999999977796 ) ) ;
#16501 = LINE ( 'NONE', #8501, #35017 ) ;
#16502 = CARTESIAN_POINT ( 'NONE',  ( 12.91533473730993009, 51.60535201082149825, -10.88017736071109987 ) ) ;
#16504 = CARTESIAN_POINT ( 'NONE',  ( 13.79529636645030344, 13.26208216824729824, 14.16423886937410614 ) ) ;
#16503 = CARTESIAN_POINT ( 'NONE',  ( 13.43411237798106583, 47.66530133659709634, -12.81628187352647252 ) ) ;
#16505 = CARTESIAN_POINT ( 'NONE',  ( 12.63842701281683922, 19.55059781766745175, -9.846743663894590881 ) ) ;
#16506 = CARTESIAN_POINT ( 'NONE',  ( 17.20831665107776587, 64.13393115100079456, -7.208316651077762316 ) ) ;
#16507 = CARTESIAN_POINT ( 'NONE',  ( 12.63842701281683034, 17.46726448433411250, 9.846743663894596210 ) ) ;
#16508 = DIRECTION ( 'NONE',  ( 1.000000000000000000, 0.000000000000000000, 0.000000000000000000 ) ) ;
#16509 = CARTESIAN_POINT ( 'NONE',  ( 6.204703633549690345, 60.76208216824730357, -14.16423886937410259 ) ) ;
#16510 = ORIENTED_EDGE ( 'NONE', *, *, #38726, .T. ) ;
#16511 =( LENGTH_UNIT ( ) NAMED_UNIT ( * ) SI_UNIT ( .MILLI., .METRE. ) );
#16512 = AXIS2_PLACEMENT_3D ( 'NONE', #96655, #90973, #88633 ) ;
#16513 = CARTESIAN_POINT ( 'NONE',  ( 17.96484262340118221, 11.18868534415483929, -7.964842623401177768 ) ) ;
#16514 = CARTESIAN_POINT ( 'NONE',  ( -0.1503990784575242878, 19.24884699246888786, -6.262539305110083276 ) ) ;
#16515 = ORIENTED_EDGE ( 'NONE', *, *, #79817, .T. ) ;
#16516 = CIRCLE ( 'NONE', #64370, 15.00000000000000000 ) ;
#16517 = CARTESIAN_POINT ( 'NONE',  ( 20.88017736071110164, 5.355352010821503583, 2.915334737309930979 ) ) ;
#16519 = ADVANCED_FACE ( 'NONE', ( #22428 ), #80944, .F. ) ;
#16518 = CARTESIAN_POINT ( 'NONE',  ( 4.559911319644449179, 7.230352010821505360, -9.422509992056141925 ) ) ;
#16520 = CARTESIAN_POINT ( 'NONE',  ( 12.63842701281683034, 37.46726448433411605, 9.846743663894596210 ) ) ;
#16521 = CARTESIAN_POINT ( 'NONE',  ( -1.099225684535947600, 33.70696800326375353, -6.408140936763238038 ) ) ;
#16522 = CARTESIAN_POINT ( 'NONE',  ( 19.89220837332772263, 64.74062864464239908, 6.478736007406007857 ) ) ;
#16524 = CARTESIAN_POINT ( 'NONE',  ( -2.266590686148945544, 22.22041550158063572, 7.082119434687048631 ) ) ;
#16523 = CARTESIAN_POINT ( 'NONE',  ( -10.04796213703186503, 15.00000000000000888, 10.62905469192457986 ) ) ;
#16525 = CARTESIAN_POINT ( 'NONE',  ( 17.96484262340118221, 26.18868534415483396, -7.964842623401177768 ) ) ;
#16526 = CARTESIAN_POINT ( 'NONE',  ( 4.559911319644449179, 8.897018677488173211, 9.422509992056141925 ) ) ;
#16527 = CARTESIAN_POINT ( 'NONE',  ( 18.52753015748617571, 48.09226448433412315, 4.923371831947298993 ) ) ;
#16528 = EDGE_CURVE ( 'NONE', #98433, #58154, #44481, .T. ) ;
#16529 = DIRECTION ( 'NONE',  ( 0.000000000000000000, 0.000000000000000000, 1.000000000000000000 ) ) ;
#16530 = CARTESIAN_POINT ( 'NONE',  ( 0.1532563361054083140, 41.00893115100078745, 1.131784320476157264E-15 ) ) ;
#16531 = FILL_AREA_STYLE ('',( #8041 ) ) ;
#16532 = CARTESIAN_POINT ( 'NONE',  ( -9.846743663894596210, 25.80059781766745530, -2.638427012816824124 ) ) ;
#16533 = ORIENTED_EDGE ( 'NONE', *, *, #65807, .F. ) ;
#16534 = CARTESIAN_POINT ( 'NONE',  ( 4.559911319644449179, 3.897018677488170990, 9.422509992056141925 ) ) ;
#16535 = CARTESIAN_POINT ( 'NONE',  ( 10.00000000000000178, 69.31368534415484817, 10.88017736071110342 ) ) ;
#16536 = CARTESIAN_POINT ( 'NONE',  ( -0.8801773607110991993, 37.85535201082151247, -2.915334737309923874 ) ) ;
#16538 = CARTESIAN_POINT ( 'NONE',  ( 6.565887622018943937, 33.08196800326374643, -12.81628187352647608 ) ) ;
#16537 = CARTESIAN_POINT ( 'NONE',  ( 20.88017736071110164, 10.35535201082150714, 2.915334737309930979 ) ) ;
#16539 = CARTESIAN_POINT ( 'NONE',  ( 17.08211943468705130, 23.47041550158063572, 12.26659068614894998 ) ) ;
#16540 = MECHANICAL_DESIGN_GEOMETRIC_PRESENTATION_REPRESENTATION (  '', ( #42094 ), #72391 ) ;
#16541 = ORIENTED_EDGE ( 'NONE', *, *, #79517, .T. ) ;
#16542 = EDGE_CURVE ( 'NONE', #44301, #5283, #67422, .T. ) ;
#16543 = CARTESIAN_POINT ( 'NONE',  ( 21.09922568453594849, 41.20696800326375353, 6.408140936763242479 ) ) ;
#16544 = ORIENTED_EDGE ( 'NONE', *, *, #79929, .T. ) ;
#16545 = CARTESIAN_POINT ( 'NONE',  ( 2.791683348922240793, 41.63393115100078745, 7.208316651077764092 ) ) ;
#16546 = CARTESIAN_POINT ( 'NONE',  ( 2.035157376598822676, 17.43868534415483751, -7.964842623401177768 ) ) ;
#16547 = CIRCLE ( 'NONE', #5415, 0.5000000000000004441 ) ;
#16548 = CARTESIAN_POINT ( 'NONE',  ( -0.8801773607110991993, 17.85535201082150536, -2.915334737309923874 ) ) ;
#16549 = ORIENTED_EDGE ( 'NONE', *, *, #17647, .F. ) ;
#16550 = CARTESIAN_POINT ( 'NONE',  ( -0.8801773607110991993, 62.85535201082150536, -2.915334737309923874 ) ) ;
#16551 =( LENGTH_UNIT ( ) NAMED_UNIT ( * ) SI_UNIT ( .MILLI., .METRE. ) );
#16552 = CARTESIAN_POINT ( 'NONE',  ( 10.32896413005680181, 6.771642702460840546, 5.963430220938278126 ) ) ;
#16553 = CARTESIAN_POINT ( 'NONE',  ( 17.20831665107776587, 2.883931151000785231, 7.208316651077764980 ) ) ;
#16554 = CARTESIAN_POINT ( 'NONE',  ( 7.084665262690076126, 62.02201867748816966, -10.88017736071110164 ) ) ;
#16555 = DIRECTION ( 'NONE',  ( 1.000000000000000000, 0.000000000000000000, 0.000000000000000000 ) ) ;
#16556 = FACE_OUTER_BOUND ( 'NONE', #45420, .T. ) ;
#16558 = EDGE_LOOP ( 'NONE', ( #6810, #96099, #51201, #77028 ) ) ;
#16557 = CARTESIAN_POINT ( 'NONE',  ( 14.92337183194729988, 4.342264484334117824, -8.527530157486177487 ) ) ;
#16559 = CARTESIAN_POINT ( 'NONE',  ( 14.92337183194729988, 39.34226448433412315, -8.527530157486177487 ) ) ;
#16560 = EDGE_LOOP ( 'NONE', ( #38709, #35163 ) ) ;
#16561 = EDGE_LOOP ( 'NONE', ( #38202, #33764, #49099 ) ) ;
#16562 = DIRECTION ( 'NONE',  ( -0.5547001962252290364, -0.8320502943378437211, 0.000000000000000000 ) ) ;
#16563 = CARTESIAN_POINT ( 'NONE',  ( -2.266590686148945544, 12.22041550158063394, 7.082119434687048631 ) ) ;
#16564 = CARTESIAN_POINT ( 'NONE',  ( 19.38216949554541557, 62.24863466993041072, -9.382169495545420901 ) ) ;
#16565 = CARTESIAN_POINT ( 'NONE',  ( 24.16423886937410614, 9.303748834913967869, 8.672049930838204340E-16 ) ) ;
#16566 = CARTESIAN_POINT ( 'NONE',  ( 2.917880565312950480, 25.97041550158063572, -12.26659068614894821 ) ) ;
#16567 = FILL_AREA_STYLE ('',( #77537 ) ) ;
#16569 = CARTESIAN_POINT ( 'NONE',  ( 20.88017736071110164, 60.35535201082151957, 2.915334737309930979 ) ) ;
#16568 = DIRECTION ( 'NONE',  ( 1.000000000000000000, 1.454946622157118376E-15, 0.000000000000000000 ) ) ;
#16570 = CARTESIAN_POINT ( 'NONE',  ( 0.5774900079438607392, 18.48035201082150536, 5.440088680355550821 ) ) ;
#16571 = VERTEX_POINT ( 'NONE', #14433 ) ;
#16572 = CARTESIAN_POINT ( 'NONE',  ( 17.20831665107776587, 4.133931151000785675, -7.208316651077762316 ) ) ;
#16573 = CARTESIAN_POINT ( 'NONE',  ( 5.076628168052703671, 6.842264484334118713, 8.527530157486179263 ) ) ;
#16574 = CARTESIAN_POINT ( 'NONE',  ( 19.38216949554541202, 25.99863466993042138, 9.382169495545424454 ) ) ;
#16575 = CARTESIAN_POINT ( 'NONE',  ( 14.92337183194729633, 27.67559781766745530, 8.527530157486181039 ) ) ;
#16576 = SURFACE_STYLE_FILL_AREA ( #53081 ) ;
#16577 = CARTESIAN_POINT ( 'NONE',  ( 3.591859063236761518, 9.956968003263753531, 11.09922568453594849 ) ) ;
#16578 = CARTESIAN_POINT ( 'NONE',  ( 17.35999999999999943, 37.99999999999997868, 9.500000000000000000 ) ) ;
#16579 = CARTESIAN_POINT ( 'NONE',  ( 14.92337183194729988, 9.342264484334119601, -8.527530157486177487 ) ) ;
#16580 = EDGE_LOOP ( 'NONE', ( #48582, #54977, #4717, #97486 ) ) ;
#16581 = ORIENTED_EDGE ( 'NONE', *, *, #45704, .T. ) ;
#16582 = CARTESIAN_POINT ( 'NONE',  ( 12.91533473730993009, 41.60535201082149825, -10.88017736071109987 ) ) ;
#16583 = CARTESIAN_POINT ( 'NONE',  ( -0.3689425029237898834, 26.17874883491396432, -10.36894250292378850 ) ) ;
#16584 = CARTESIAN_POINT ( 'NONE',  ( 1.472469842513823179, 35.59226448433412315, -4.923371831947296329 ) ) ;
#16585 = CARTESIAN_POINT ( 'NONE',  ( 15.44008868035555793, 66.39701867748817676, -9.422509992056140149 ) ) ;
#16587 = CARTESIAN_POINT ( 'NONE',  ( 14.36343418943213912, 0.04922511925147082107, -3.367173657400652775 ) ) ;
#16586 = CARTESIAN_POINT ( 'NONE',  ( 10.00000000000000000, 52.87363466993041783, -12.81628187352647608 ) ) ;
#16588 = CARTESIAN_POINT ( 'NONE',  ( 10.00000000000000000, 31.81368534415483751, -10.88017736071110342 ) ) ;
#16589 = FILL_AREA_STYLE ('',( #77563 ) ) ;
#16590 = CARTESIAN_POINT ( 'NONE',  ( 10.00000000000000178, 10.37363466993041961, 12.81628187352647608 ) ) ;
#16591 = CARTESIAN_POINT ( 'NONE',  ( 2.791683348922237240, 40.38393115100078035, -7.208316651077763204 ) ) ;
#16592 = CARTESIAN_POINT ( 'NONE',  ( -7.964842623401172439, 3.688685344154841061, 7.964842623401183097 ) ) ;
#16593 = CARTESIAN_POINT ( 'NONE',  ( -1.099225684535947600, 49.54030133659708923, 6.408140936763237150 ) ) ;
#16594 = DIRECTION ( 'NONE',  ( -0.5905099943842175847, -0.8070303256584298035, 0.000000000000000000 ) ) ;
#16596 = CARTESIAN_POINT ( 'NONE',  ( -8.000000000000000000, 75.73428692542562146, 2.900000000000000355 ) ) ;
#16595 = CARTESIAN_POINT ( 'NONE',  ( 17.96484262340118221, 54.93868534415484106, 7.964842623401181321 ) ) ;
#16597 = EDGE_CURVE ( 'NONE', #49769, #39417, #15767, .T. ) ;
#16598 = DIRECTION ( 'NONE',  ( 1.000000000000000000, 0.000000000000000000, 0.000000000000000000 ) ) ;
#16599 = DIRECTION ( 'NONE',  ( -0.000000000000000000, -1.000000000000000000, -0.000000000000000000 ) ) ;
#16600 = CARTESIAN_POINT ( 'NONE',  ( 20.88017736071110519, 50.56368534415484106, 2.639326808657452039E-16 ) ) ;
#16601 = B_SPLINE_CURVE_WITH_KNOTS ( 'NONE', 3,
 ( #80420, #50398, #18439, #95922, #3932, #86927, #88901, #80908, #41456, #49909, #12402, #42908, #27403, #71923, #27893, #3444, #35396, #79913, #20411, #50897, #81392, #12894 ),
 .UNSPECIFIED., .F., .F.,
 ( 4, 2, 2, 2, 2, 2, 2, 2, 2, 2, 4 ),
 ( 0.000000000000000000, 0.005577272106129050298, 0.01115454421225810060, 0.02230908842451620119, 0.04461817684903233300, 0.05577272106129038676, 0.06692726527354844746, 0.07808180948580650815, 0.08365908159193553850, 0.08644771764500004674, 0.08923635369806456885 ),
 .UNSPECIFIED. ) ;
#16602 = CARTESIAN_POINT ( 'NONE',  ( 0.5774900079438607392, 63.48035201082149825, 5.440088680355550821 ) ) ;
#16603 = LINE ( 'NONE', #78576, #31316 ) ;
#16604 = CARTESIAN_POINT ( 'NONE',  ( 0.5774900079438607392, 63.48035201082149825, 5.440088680355550821 ) ) ;
#16605 = CARTESIAN_POINT ( 'NONE',  ( 19.42250999205614193, 5.147018677488171434, 5.440088680355555262 ) ) ;
#16606 = CARTESIAN_POINT ( 'NONE',  ( 1.472469842513823179, 46.42559781766745175, 4.923371831947296329 ) ) ;
#16608 = FACE_OUTER_BOUND ( 'NONE', #75401, .T. ) ;
#16607 = CARTESIAN_POINT ( 'NONE',  ( 7.084665262690076126, 19.10535201082150181, 10.88017736071109987 ) ) ;
#16609 = CARTESIAN_POINT ( 'NONE',  ( 6.565887622018943937, 30.16530133659708568, 12.81628187352647430 ) ) ;
#16610 = ORIENTED_EDGE ( 'NONE', *, *, #60064, .T. ) ;
#16611 = CARTESIAN_POINT ( 'NONE',  ( 2.035157376598822676, 32.43868534415483396, -7.964842623401177768 ) ) ;
#16612 = VECTOR ( 'NONE', #18913, 1000.000000000000000 ) ;
#16614 = FACE_OUTER_BOUND ( 'NONE', #14668, .T. ) ;
#16613 = CARTESIAN_POINT ( 'NONE',  ( 6.565887622018943937, 8.081968003263751754, -12.81628187352647608 ) ) ;
#16615 = CARTESIAN_POINT ( 'NONE',  ( 15.44008868035555260, 14.73035201082150536, 9.422509992056143702 ) ) ;
#16616 = CARTESIAN_POINT ( 'NONE',  ( 19.42250999205614548, 35.98035201082151247, -5.440088680355545492 ) ) ;
#16617 = CARTESIAN_POINT ( 'NONE',  ( 17.08211943468705130, 53.47041550158063217, 12.26659068614894998 ) ) ;
#16618 = CARTESIAN_POINT ( 'NONE',  ( 12.63842701281683034, 22.46726448433411605, 9.846743663894596210 ) ) ;
#16619 = CARTESIAN_POINT ( 'NONE',  ( 20.88017736071110519, 65.56368534415483396, 2.639326808657452039E-16 ) ) ;
#16620 = CARTESIAN_POINT ( 'NONE',  ( 4.020549461440776184, 0.000000000000000000, -3.684154808197036335 ) ) ;
#16621 = CARTESIAN_POINT ( 'NONE',  ( 6.204703633549690345, 22.84541550158062861, 14.16423886937410082 ) ) ;
#16622 = CARTESIAN_POINT ( 'NONE',  ( 5.815488105659760265, 0.2301500539507717324, -13.76235181012718023 ) ) ;
#16623 = FACE_OUTER_BOUND ( 'NONE', #59185, .T. ) ;
#16624 = ORIENTED_EDGE ( 'NONE', *, *, #68918, .F. ) ;
#16625 = ORIENTED_EDGE ( 'NONE', *, *, #75537, .T. ) ;
#16626 = CARTESIAN_POINT ( 'NONE',  ( 22.26659068614894466, 28.88708216824730357, 7.082119434687054849 ) ) ;
#16628 = EDGE_CURVE ( 'NONE', #58305, #3713, #27930, .T. ) ;
#16627 = CARTESIAN_POINT ( 'NONE',  ( 6.204703633549690345, 37.84541550158063927, 14.16423886937410082 ) ) ;
#16629 = CARTESIAN_POINT ( 'NONE',  ( 7.361572987183169658, 4.967264484334119601, -9.846743663894592657 ) ) ;
#16630 = CARTESIAN_POINT ( 'NONE',  ( 3.591859063236763294, 8.290301336597087456, -11.09922568453595026 ) ) ;
#16631 = CARTESIAN_POINT ( 'NONE',  ( 12.63842701281683922, 59.55059781766744464, -9.846743663894590881 ) ) ;
#16632 = CARTESIAN_POINT ( 'NONE',  ( -7.858200837510024073, -3.137962441271501479, 4.000000000000000000 ) ) ;
#16634 = CARTESIAN_POINT ( 'NONE',  ( 3.591859063236763294, 13.29030133659708746, -11.09922568453595026 ) ) ;
#16633 = CARTESIAN_POINT ( 'NONE',  ( 19.42250999205614193, 55.14701867748817676, 5.440088680355555262 ) ) ;
#16635 = CARTESIAN_POINT ( 'NONE',  ( 24.16423886937410614, 24.30374883491396787, 8.672049930838204340E-16 ) ) ;
#16636 = CARTESIAN_POINT ( 'NONE',  ( 7.084665262690076126, 29.10535201082150181, 10.88017736071109987 ) ) ;
#16637 = CARTESIAN_POINT ( 'NONE',  ( 12.91533473730992121, 34.52201867748817676, 10.88017736071110164 ) ) ;
#16638 = ADVANCED_FACE ( 'NONE', ( #83902 ), #60896, .F. ) ;
#16639 = B_SPLINE_CURVE_WITH_KNOTS ( 'NONE', 3,
 ( #41829, #72295, #3826, #34281, #64781, #97803, #21787, #52755, #29264, #20791 ),
 .UNSPECIFIED., .F., .F.,
 ( 4, 2, 2, 2, 4 ),
 ( 8.673617379884034509E-19, 0.001992649090385492476, 0.002988973635578252158, 0.003487135908174629831, 0.003985298180771007504 ),
 .UNSPECIFIED. ) ;
#16640 = CARTESIAN_POINT ( 'NONE',  ( 12.34557190004681360, 0.04922511925147205619, -8.076692058882494862 ) ) ;
#16641 = CARTESIAN_POINT ( 'NONE',  ( 20.88017736071110164, 60.35535201082151957, 2.915334737309930979 ) ) ;
#16642 = CARTESIAN_POINT ( 'NONE',  ( 7.208316651077762316, -15.86606884899921610, -7.208316651077764980 ) ) ;
#16643 = ORIENTED_EDGE ( 'NONE', *, *, #43631, .F. ) ;
#16644 = CARTESIAN_POINT ( 'NONE',  ( -13.03370038005733456, 15.00000000000000000, 9.273621236547603175 ) ) ;
#16645 = ORIENTED_EDGE ( 'NONE', *, *, #90441, .T. ) ;
#16646 = LINE ( 'NONE', #94596, #81257 ) ;
#16647 = VERTEX_POINT ( 'NONE', #37926 ) ;
#16649 = CARTESIAN_POINT ( 'NONE',  ( 2.917880565312948704, 67.63708216824730357, 12.26659068614894643 ) ) ;
#16648 = CARTESIAN_POINT ( 'NONE',  ( 6.204703633549690345, 62.84541550158063927, 14.16423886937410082 ) ) ;
#16651 = CARTESIAN_POINT ( 'NONE',  ( 7.361572987183170547, 67.05059781766746596, 9.846743663894590881 ) ) ;
#16650 = CARTESIAN_POINT ( 'NONE',  ( 0.1532563361054082862, 41.21726448433411605, 2.638427012816831674 ) ) ;
#16652 = DIRECTION ( 'NONE',  ( -0.000000000000000000, -1.000000000000000000, -0.000000000000000000 ) ) ;
#16653 = DIRECTION ( 'NONE',  ( -0.000000000000000000, 1.000000000000000000, -0.000000000000000000 ) ) ;
#16654 = CARTESIAN_POINT ( 'NONE',  ( 21.09922568453594849, 11.20696800326375531, 6.408140936763242479 ) ) ;
#16655 = CARTESIAN_POINT ( 'NONE',  ( -12.81628187352647608, 29.12363466993042493, 3.903127820947815962E-15 ) ) ;
#16656 = VERTEX_POINT ( 'NONE', #70386 ) ;
#16657 = CARTESIAN_POINT ( 'NONE',  ( 6.204703633549690345, 50.76208216824730357, -14.16423886937410259 ) ) ;
#16658 = CARTESIAN_POINT ( 'NONE',  ( -4.164238869374098151, 46.59541550158063927, -3.795296366450310543 ) ) ;
#16659 = VERTEX_POINT ( 'NONE', #46395 ) ;
#16660 = CARTESIAN_POINT ( 'NONE',  ( 17.96484262340118221, 16.18868534415483396, -7.964842623401177768 ) ) ;
#16661 = DIRECTION ( 'NONE',  ( -0.000000000000000000, -1.000000000000000000, -0.000000000000000000 ) ) ;
#16662 = EDGE_CURVE ( 'NONE', #72594, #72857, #33609, .T. ) ;
#16663 = CARTESIAN_POINT ( 'NONE',  ( 17.96484262340118221, 39.93868534415484106, 7.964842623401181321 ) ) ;
#16664 = CARTESIAN_POINT ( 'NONE',  ( 18.52753015748617571, 53.09226448433412315, 4.923371831947298993 ) ) ;
#16665 = CARTESIAN_POINT ( 'NONE',  ( 10.00000000000000000, 36.81368534415484106, -10.88017736071110342 ) ) ;
#16666 = CARTESIAN_POINT ( 'NONE',  ( 10.64017930668199874, 14.63595249122789177, 10.57291749337223052 ) ) ;
#16667 = CARTESIAN_POINT ( 'NONE',  ( 10.00000000000000178, 59.31368534415484106, 10.88017736071110342 ) ) ;
#16668 = CARTESIAN_POINT ( 'NONE',  ( 2.035157376598824452, 28.68868534415484106, 7.964842623401179544 ) ) ;
#16669 = EDGE_CURVE ( 'NONE', #23582, #35712, #59824, .T. ) ;
#16671 = ORIENTED_EDGE ( 'NONE', *, *, #97240, .F. ) ;
#16670 = CARTESIAN_POINT ( 'NONE',  ( 5.500000000000000000, 61.00000000000000711, 6.500000000000000888 ) ) ;
#16672 = AXIS2_PLACEMENT_3D ( 'NONE', #98981, #98485, #53434 ) ;
#16673 = CARTESIAN_POINT ( 'NONE',  ( 10.00000000000000178, 2.258931151000784787, 9.846743663894594434 ) ) ;
#16674 = CARTESIAN_POINT ( 'NONE',  ( -3.585386599411522823, -2.690194976751941969, 2.500000000000404121 ) ) ;
#16675 = ORIENTED_EDGE ( 'NONE', *, *, #37822, .T. ) ;
#16676 = CARTESIAN_POINT ( 'NONE',  ( 9.112672642667108747, -7.236390792799208604, 3.750000000000000000 ) ) ;
#16677 = CARTESIAN_POINT ( 'NONE',  ( 5.076628168052704559, 25.17559781766745175, -8.527530157486179263 ) ) ;
#16678 = CARTESIAN_POINT ( 'NONE',  ( 12.25993886608603489, 14.49999999999999112, 8.642563219313760925 ) ) ;
#16680 = SURFACE_SIDE_STYLE ('',( #70173 ) ) ;
#16679 = AXIS2_PLACEMENT_3D ( 'NONE', #82609, #45097, #32558 ) ;
#16681 = CARTESIAN_POINT ( 'NONE',  ( 11.49999999999999645, 75.00000000000000000, -6.500000000000000888 ) ) ;
#16682 = ORIENTED_EDGE ( 'NONE', *, *, #73651, .T. ) ;
#16683 = CARTESIAN_POINT ( 'NONE',  ( 10.00000000000000178, 67.25893115100079456, 9.846743663894594434 ) ) ;
#16684 = CARTESIAN_POINT ( 'NONE',  ( -43.18361233615330974, 107.2794497428041041, 4.499999999210813506 ) ) ;
#16685 = CARTESIAN_POINT ( 'NONE',  ( 14.92337183194729988, 49.34226448433411605, -8.527530157486177487 ) ) ;
#16686 = CARTESIAN_POINT ( 'NONE',  ( -0.3689425029237898834, 46.17874883491397497, -10.36894250292378850 ) ) ;
#16687 = CARTESIAN_POINT ( 'NONE',  ( 19.84674366389459266, 53.30059781766744464, 2.638427012816836559 ) ) ;
#16688 = CARTESIAN_POINT ( 'NONE',  ( 20.15039907845753220, 41.74884699246887720, 6.262539305110078836 ) ) ;
#16689 = CARTESIAN_POINT ( 'NONE',  ( 7.361572987183169658, 14.96726448433411960, -9.846743663894592657 ) ) ;
#16690 = CARTESIAN_POINT ( 'NONE',  ( 16.40814093676324603, 47.45696800326375353, -11.09922568453594671 ) ) ;
#16691 = CARTESIAN_POINT ( 'NONE',  ( 19.84674366389459266, 63.71726448433412315, -2.638427012816827677 ) ) ;
#16692 = CARTESIAN_POINT ( 'NONE',  ( 4.559911319644449179, 58.89701867748817676, 9.422509992056141925 ) ) ;
#16693 = CARTESIAN_POINT ( 'NONE',  ( 12.63842701281683922, 49.55059781766744464, -9.846743663894590881 ) ) ;
#16694 = CARTESIAN_POINT ( 'NONE',  ( 21.92686044187657046, 15.16212336850780318, 4.562052436263912550E-16 ) ) ;
#16695 = ORIENTED_EDGE ( 'NONE', *, *, #89095, .T. ) ;
#16696 = CARTESIAN_POINT ( 'NONE',  ( 2.917880565312948704, 52.63708216824730357, 12.26659068614894643 ) ) ;
#16697 = CARTESIAN_POINT ( 'NONE',  ( -14.19749592853509768, -0.03417435944610275333, 7.369430493279844008 ) ) ;
#16698 = CARTESIAN_POINT ( 'NONE',  ( 15.44008868035555260, 29.73035201082150891, 9.422509992056143702 ) ) ;
#16700 = CARTESIAN_POINT ( 'NONE',  ( 2.035157376598822676, 62.43868534415483396, -7.964842623401177768 ) ) ;
#16699 = CARTESIAN_POINT ( 'NONE',  ( 13.43411237798105340, 10.58196800326375353, 12.81628187352647963 ) ) ;
#16701 = DIRECTION ( 'NONE',  ( 1.000000000000000000, -0.000000000000000000, 0.000000000000000000 ) ) ;
#16702 = CARTESIAN_POINT ( 'NONE',  ( -3.866352809136307744, 0.04962897115650977131, 14.23757791217067314 ) ) ;
#16703 = CARTESIAN_POINT ( 'NONE',  ( 0.000000000000000000, 15.00000000000000000, 0.000000000000000000 ) ) ;
#16705 = CARTESIAN_POINT ( 'NONE',  ( 1.046131998950049047, 10.73810908735726777, 6.500000000000002665 ) ) ;
#16704 = CARTESIAN_POINT ( 'NONE',  ( -0.8801773607111008646, 58.27201867748816966, 2.915334737309923430 ) ) ;
#16706 = CARTESIAN_POINT ( 'NONE',  ( 14.92337183194729988, 34.34226448433411605, -8.527530157486177487 ) ) ;
#16707 = FACE_OUTER_BOUND ( 'NONE', #97302, .T. ) ;
#16708 = CARTESIAN_POINT ( 'NONE',  ( 3.795296366450306547, 30.34541550158064283, -14.16423886937410259 ) ) ;
#16709 = CARTESIAN_POINT ( 'NONE',  ( 19.38216949554541557, 12.24863466993041961, -9.382169495545420901 ) ) ;
#16710 = CARTESIAN_POINT ( 'NONE',  ( 19.42250999205614193, 15.14701867748817143, 5.440088680355555262 ) ) ;
#16711 = DIRECTION ( 'NONE',  ( 0.000000000000000000, 0.000000000000000000, -1.000000000000000000 ) ) ;
#16712 = MECHANICAL_DESIGN_GEOMETRIC_PRESENTATION_REPRESENTATION (  '', ( #8781 ), #48666 ) ;
#16713 = CARTESIAN_POINT ( 'NONE',  ( 10.00000000000000178, 38.05374883491396787, 14.16423886937410082 ) ) ;
#16714 = EDGE_CURVE ( 'NONE', #25641, #87694, #95610, .T. ) ;
#16715 = CARTESIAN_POINT ( 'NONE',  ( -0.3689425029237881626, 67.42874883491396076, 10.36894250292379027 ) ) ;
#16716 = CARTESIAN_POINT ( 'NONE',  ( 1.472469842513823179, 30.59226448433411960, -4.923371831947296329 ) ) ;
#16717 = CARTESIAN_POINT ( 'NONE',  ( 17.20831665107776587, 19.13393115100078035, -7.208316651077762316 ) ) ;
#16718 = CARTESIAN_POINT ( 'NONE',  ( 19.42250999205614193, 20.14701867748817321, 5.440088680355555262 ) ) ;
#16719 = ORIENTED_EDGE ( 'NONE', *, *, #71522, .F. ) ;
#16720 = CARTESIAN_POINT ( 'NONE',  ( 18.52753015748618282, 43.92559781766745175, -4.923371831947291888 ) ) ;
#16721 = CARTESIAN_POINT ( 'NONE',  ( 2.035157376598822676, 32.43868534415483396, -7.964842623401177768 ) ) ;
#16722 = CARTESIAN_POINT ( 'NONE',  ( 10.00000000000000000, 64.75893115100078035, -9.846743663894594434 ) ) ;
#16724 = CARTESIAN_POINT ( 'NONE',  ( 0.2751277870542909731, 44.36607318730131055, -6.499999999999992006 ) ) ;
#16723 = CARTESIAN_POINT ( 'NONE',  ( 2.917880565312948704, 7.637082168247301794, 12.26659068614894643 ) ) ;
#16725 = CARTESIAN_POINT ( 'NONE',  ( -27.43587634952538323, 44.49999999999997158, 10.00000000000000000 ) ) ;
#16726 = CARTESIAN_POINT ( 'NONE',  ( 18.52753015748617571, 18.09226448433411960, 4.923371831947298993 ) ) ;
#16727 = CARTESIAN_POINT ( 'NONE',  ( 22.81628187352647785, 56.41530133659708213, 3.434112377981063169 ) ) ;
#16728 = CARTESIAN_POINT ( 'NONE',  ( 1.472469842513823179, 61.42559781766745175, 4.923371831947296329 ) ) ;
#16729 = ORIENTED_EDGE ( 'NONE', *, *, #92831, .T. ) ;
#16730 = CARTESIAN_POINT ( 'NONE',  ( 0.1532563361054100626, 15.80059781766745353, -2.638427012816831230 ) ) ;
#16731 = CARTESIAN_POINT ( 'NONE',  ( 9.112669733836950670, -7.236323975091223382, -4.000000000000000000 ) ) ;
#16732 = CARTESIAN_POINT ( 'NONE',  ( 0.000000000000000000, 0.5000000000000004441, 0.000000000000000000 ) ) ;
#16733 = CARTESIAN_POINT ( 'NONE',  ( 0.5774900079438590739, 2.647018677488171434, -5.440088680355550821 ) ) ;
#16734 = CARTESIAN_POINT ( 'NONE',  ( 0.5774900079438607392, 48.48035201082150536, 5.440088680355550821 ) ) ;
#16735 = DIRECTION ( 'NONE',  ( -0.9170600743851212711, 0.000000000000000000, -0.3987490689252527476 ) ) ;
#16736 = CARTESIAN_POINT ( 'NONE',  ( 12.91533473730993009, 61.60535201082150536, -10.88017736071109987 ) ) ;
#16737 = CARTESIAN_POINT ( 'NONE',  ( 7.361572987183170547, 42.05059781766745886, 9.846743663894590881 ) ) ;
#16738 = CARTESIAN_POINT ( 'NONE',  ( 15.44008868035555260, 14.73035201082150536, 9.422509992056143702 ) ) ;
#16739 = CARTESIAN_POINT ( 'NONE',  ( -3.999999999999999112, 78.07179676972445748, -6.250000000000000000 ) ) ;
#16740 = AXIS2_PLACEMENT_3D ( 'NONE', #70288, #84789, #77273 ) ;
#16741 = B_SPLINE_CURVE_WITH_KNOTS ( 'NONE', 3,
 ( #46677, #70182, #48639, #92187 ),
 .UNSPECIFIED., .F., .F.,
 ( 4, 4 ),
 ( 7.410741937918042371E-18, 0.002562518741975316431 ),
 .UNSPECIFIED. ) ;
#16742 =( LENGTH_UNIT ( ) NAMED_UNIT ( * ) SI_UNIT ( .MILLI., .METRE. ) );
#16743 = EDGE_LOOP ( 'NONE', ( #16643, #68066, #82751, #57406 ) ) ;
#16744 = ORIENTED_EDGE ( 'NONE', *, *, #65690, .T. ) ;
#16745 = CARTESIAN_POINT ( 'NONE',  ( -9.240973841163672375, 15.00000000000000000, 11.17382667070363667 ) ) ;
#16746 = EDGE_CURVE ( 'NONE', #6951, #31758, #83136, .T. ) ;
#16747 = PRESENTATION_LAYER_ASSIGNMENT (  '', '', ( #59829 ) ) ;
#16748 = CARTESIAN_POINT ( 'NONE',  ( 10.00000000000000000, 39.75893115100078745, -9.846743663894594434 ) ) ;
#16749 = CARTESIAN_POINT ( 'NONE',  ( 19.84674366389459621, 18.50893115100078745, 7.409399052514197653E-17 ) ) ;
#16750 = CARTESIAN_POINT ( 'NONE',  ( 0.6178305044545818747, 58.49863466993042493, -9.382169495545419124 ) ) ;
#16752 = CARTESIAN_POINT ( 'NONE',  ( 12.63842701281683034, 47.46726448433412315, 9.846743663894596210 ) ) ;
#16751 = CARTESIAN_POINT ( 'NONE',  ( 0.5774900079438607392, 23.48035201082150536, 5.440088680355550821 ) ) ;
#16753 = CARTESIAN_POINT ( 'NONE',  ( -1.926860441876563801, 34.89664270246083788, 3.195792623639529761 ) ) ;
#16754 = CARTESIAN_POINT ( 'NONE',  ( 2.917880565312950480, 45.97041550158063927, -12.26659068614894821 ) ) ;
#16755 = PRESENTATION_LAYER_ASSIGNMENT (  '', '', ( #78979 ) ) ;
#16756 = CARTESIAN_POINT ( 'NONE',  ( 20.36894250292379738, 64.92874883491397497, -10.36894250292379027 ) ) ;
#16757 = FACE_OUTER_BOUND ( 'NONE', #35704, .T. ) ;
#16758 = DIRECTION ( 'NONE',  ( 0.000000000000000000, 0.000000000000000000, 1.000000000000000000 ) ) ;
#16759 = CARTESIAN_POINT ( 'NONE',  ( 12.91533473730992121, 49.52201867748817676, 10.88017736071110164 ) ) ;
#16760 = ADVANCED_FACE ( 'NONE', ( #47368 ), #77866, .F. ) ;
#16761 = PRESENTATION_LAYER_ASSIGNMENT (  '', '', ( #42094 ) ) ;
#16762 = CARTESIAN_POINT ( 'NONE',  ( 18.52753015748618282, 18.92559781766745175, -4.923371831947291888 ) ) ;
#16763 = CARTESIAN_POINT ( 'NONE',  ( -6.868018881897138606, -58.39307134327875559, 3.750000000000000444 ) ) ;
#16764 = ORIENTED_EDGE ( 'NONE', *, *, #52290, .T. ) ;
#16765 = DIRECTION ( 'NONE',  ( -0.000000000000000000, -0.000000000000000000, -1.000000000000000000 ) ) ;
#16766 = ORIENTED_EDGE ( 'NONE', *, *, #40716, .F. ) ;
#16767 = CARTESIAN_POINT ( 'NONE',  ( 19.84674366389459266, 3.717264484334118713, -2.638427012816827677 ) ) ;
#16768 = EDGE_LOOP ( 'NONE', ( #46530, #41818, #70642, #24286, #20469, #89803 ) ) ;
#16769 = CARTESIAN_POINT ( 'NONE',  ( 22.26659068614895176, 19.72041550158063572, -7.082119434687042414 ) ) ;
#16770 = CARTESIAN_POINT ( 'NONE',  ( 12.63842701281683034, 17.46726448433411250, 9.846743663894596210 ) ) ;
#16771 = CARTESIAN_POINT ( 'NONE',  ( 20.88017736071110164, 50.35535201082151247, 2.915334737309930979 ) ) ;
#16772 =( LENGTH_UNIT ( ) NAMED_UNIT ( * ) SI_UNIT ( .MILLI., .METRE. ) );
#16773 = ORIENTED_EDGE ( 'NONE', *, *, #51139, .F. ) ;
#16774 = CARTESIAN_POINT ( 'NONE',  ( 20.88017736071110519, 45.56368534415484106, 2.639326808657452039E-16 ) ) ;
#16775 = AXIS2_PLACEMENT_3D ( 'NONE', #50388, #14885, #45354 ) ;
#16776 = ORIENTED_EDGE ( 'NONE', *, *, #83698, .T. ) ;
#16777 = CARTESIAN_POINT ( 'NONE',  ( 17.08211943468705130, 3.470415501580634388, 12.26659068614894998 ) ) ;
#16778 = ORIENTED_EDGE ( 'NONE', *, *, #92786, .F. ) ;
#16779 = VERTEX_POINT ( 'NONE', #68415 ) ;
#16780 = CARTESIAN_POINT ( 'NONE',  ( 19.38216949554541557, 17.24863466993041783, -9.382169495545420901 ) ) ;
#16781 = CARTESIAN_POINT ( 'NONE',  ( 2.791683348922237240, 5.383931151000785675, -7.208316651077763204 ) ) ;
#16782 = CARTESIAN_POINT ( 'NONE',  ( 2.035157376598822676, 2.438685344154837953, -7.964842623401177768 ) ) ;
#16783 =( REPRESENTATION_RELATIONSHIP ('NONE','NONE', #61309, #51695 ) REPRESENTATION_RELATIONSHIP_WITH_TRANSFORMATION ( #90209 )SHAPE_REPRESENTATION_RELATIONSHIP( ) );
#16784 = CARTESIAN_POINT ( 'NONE',  ( 3.243710765982329214, 0.000000000000000000, -4.383623511354890034 ) ) ;
#16785 = CARTESIAN_POINT ( 'NONE',  ( 18.52753015748617571, 23.09226448433411960, 4.923371831947298993 ) ) ;
#16786 = CARTESIAN_POINT ( 'NONE',  ( -0.8801773607110991993, 32.85535201082151247, -2.915334737309923874 ) ) ;
#16787 = AXIS2_PLACEMENT_3D ( 'NONE', #88574, #49104, #43079 ) ;
#16788 = EDGE_CURVE ( 'NONE', #36938, #87330, #7430, .T. ) ;
#16789 = ORIENTED_EDGE ( 'NONE', *, *, #8372, .F. ) ;
#16790 = CARTESIAN_POINT ( 'NONE',  ( -10.44000000000001194, 92.00000000000000000, -9.500000000000000000 ) ) ;
#16791 = CARTESIAN_POINT ( 'NONE',  ( -0.8801773607111009756, 58.06368534415484106, 1.068504757029289695E-15 ) ) ;
#16792 = LINE ( 'NONE', #1805, #6866 ) ;
#16793 = CARTESIAN_POINT ( 'NONE',  ( 6.565887622018943937, 63.08196800326376064, -12.81628187352647608 ) ) ;
#16794 = CARTESIAN_POINT ( 'NONE',  ( 2.035157376598822676, 67.43868534415484817, -7.964842623401177768 ) ) ;
#16795 = CARTESIAN_POINT ( 'NONE',  ( -2.816281873526471635, 8.915301336597083903, -3.434112377981056508 ) ) ;
#16796 = CARTESIAN_POINT ( 'NONE',  ( -4.289191146912808207E-15, 3.868033628982651795, -11.25000000000000178 ) ) ;
#16797 = CARTESIAN_POINT ( 'NONE',  ( 14.92337183194729988, 34.34226448433411605, -8.527530157486177487 ) ) ;
#16798 = CARTESIAN_POINT ( 'NONE',  ( -1.099225684535947600, 58.70696800326375353, -6.408140936763238038 ) ) ;
#16799 = CARTESIAN_POINT ( 'NONE',  ( -2.266590686148945544, 12.22041550158063394, 7.082119434687048631 ) ) ;
#16800 = CARTESIAN_POINT ( 'NONE',  ( 14.92337183194729633, 17.67559781766745175, 8.527530157486181039 ) ) ;
#16802 = CIRCLE ( 'NONE', #50322, 0.2500000000000002220 ) ;
#16801 = CARTESIAN_POINT ( 'NONE',  ( -1.099225684535947600, 23.70696800326375708, -6.408140936763238038 ) ) ;
#16804 = CARTESIAN_POINT ( 'NONE',  ( -7.079946191729883154, -69.52844198715558832, -2.750000000000000888 ) ) ;
#16803 = DIRECTION ( 'NONE',  ( 0.5807029557109406603, 0.000000000000000000, 0.8141155183563185682 ) ) ;
#16805 = CARTESIAN_POINT ( 'NONE',  ( 20.88017736071110164, 45.35535201082149115, 2.915334737309930979 ) ) ;
#16806 = CARTESIAN_POINT ( 'NONE',  ( 14.92337183194729633, 62.67559781766745886, 8.527530157486181039 ) ) ;
#16807 = DIRECTION ( 'NONE',  ( 0.000000000000000000, 0.000000000000000000, -1.000000000000000000 ) ) ;
#16808 = CARTESIAN_POINT ( 'NONE',  ( 2.791683348922240793, 26.63393115100078745, 7.208316651077764092 ) ) ;
#16809 = CARTESIAN_POINT ( 'NONE',  ( 0.5774900079438590739, 12.64701867748817143, -5.440088680355550821 ) ) ;
#16810 = CARTESIAN_POINT ( 'NONE',  ( 21.09922568453595559, 22.04030133659708923, -6.408140936763230044 ) ) ;
#16811 = CARTESIAN_POINT ( 'NONE',  ( 18.52753015748617571, 23.09226448433411960, 4.923371831947298993 ) ) ;
#16812 = DIRECTION ( 'NONE',  ( 0.000000000000000000, 0.000000000000000000, 1.000000000000000000 ) ) ;
#16813 = CARTESIAN_POINT ( 'NONE',  ( -0.8801773607111009756, 18.06368534415484106, 1.068504757029289695E-15 ) ) ;
#16814 = B_SPLINE_CURVE_WITH_KNOTS ( 'NONE', 3,
 ( #96736, #52201, #89210, #36211 ),
 .UNSPECIFIED., .F., .F.,
 ( 4, 4 ),
 ( 0.000000000000000000, 0.002392975128318465105 ),
 .UNSPECIFIED. ) ;
#16815 = FACE_OUTER_BOUND ( 'NONE', #20673, .T. ) ;
#16817 = CARTESIAN_POINT ( 'NONE',  ( 15.44008868035555793, 16.39701867748817321, -9.422509992056140149 ) ) ;
#16816 = CARTESIAN_POINT ( 'NONE',  ( 1.472469842513823179, 41.42559781766745886, 4.923371831947296329 ) ) ;
#16818 = FILL_AREA_STYLE ('',( #17319 ) ) ;
#16819 = CARTESIAN_POINT ( 'NONE',  ( 12.91533473730993009, 26.60535201082150536, -10.88017736071109987 ) ) ;
#16821 = CARTESIAN_POINT ( 'NONE',  ( -1.926860441876564023, 19.68830936912750573, 1.004413902775740781E-15 ) ) ;
#16820 = CARTESIAN_POINT ( 'NONE',  ( 17.96484262340118221, 14.93868534415484106, 7.964842623401181321 ) ) ;
#16822 = CARTESIAN_POINT ( 'NONE',  ( 7.361572987183169658, 19.96726448433411960, -9.846743663894592657 ) ) ;
#16823 = CARTESIAN_POINT ( 'NONE',  ( 12.63842701281683922, 44.55059781766745175, -9.846743663894590881 ) ) ;
#16824 = CARTESIAN_POINT ( 'NONE',  ( -10.98829462902744680, 46.98606209026556968, 0.000000000000000000 ) ) ;
#16825 = CARTESIAN_POINT ( 'NONE',  ( 20.15039907845753930, 4.722660991849187972, 6.262539305110067289 ) ) ;
#16826 = CARTESIAN_POINT ( 'NONE',  ( 7.361572987183170547, 67.05059781766746596, 9.846743663894590881 ) ) ;
#16827 = DIRECTION ( 'NONE',  ( -0.9975640502598257520, 0.06975647374410356982, 0.000000000000000000 ) ) ;
#16828 = EDGE_CURVE ( 'NONE', #33199, #26706, #48841, .T. ) ;
#16829 =( NAMED_UNIT ( * ) PLANE_ANGLE_UNIT ( ) SI_UNIT ( $, .RADIAN. ) );
#16830 = CARTESIAN_POINT ( 'NONE',  ( -0.3689425029237881626, 27.42874883491397142, 10.36894250292379027 ) ) ;
#16831 = CARTESIAN_POINT ( 'NONE',  ( 0.1532563361054082862, 41.21726448433411605, 2.638427012816831674 ) ) ;
#16832 = FACE_OUTER_BOUND ( 'NONE', #26940, .T. ) ;
#16833 = ORIENTED_EDGE ( 'NONE', *, *, #23445, .T. ) ;
#16834 = AXIS2_PLACEMENT_3D ( 'NONE', #19773, #80777, #12270 ) ;
#16835 = CARTESIAN_POINT ( 'NONE',  ( 6.204703633549690345, 55.76208216824730357, -14.16423886937410259 ) ) ;
#16836 = EDGE_CURVE ( 'NONE', #44051, #40499, #7327, .T. ) ;
#16837 = EDGE_CURVE ( 'NONE', #55655, #39990, #97185, .T. ) ;
#16838 = CARTESIAN_POINT ( 'NONE',  ( 1.472469842513823179, 15.59226448433411960, -4.923371831947296329 ) ) ;
#16839 = CARTESIAN_POINT ( 'NONE',  ( -1.457314710996554519, 0.000000000000000000, 5.254907083456953565 ) ) ;
#16840 = CARTESIAN_POINT ( 'NONE',  ( 19.42250999205614548, 40.98035201082150536, -5.440088680355545492 ) ) ;
#16841 = CARTESIAN_POINT ( 'NONE',  ( 3.591859063236761518, 44.95696800326376064, 11.09922568453594849 ) ) ;
#16842 = CARTESIAN_POINT ( 'NONE',  ( 10.00000000000000178, 14.31368534415483751, 10.88017736071110342 ) ) ;
#16843 = CARTESIAN_POINT ( 'NONE',  ( 6.565887622018943937, 43.08196800326374643, -12.81628187352647608 ) ) ;
#16844 = CARTESIAN_POINT ( 'NONE',  ( 10.00000000000000178, 67.25893115100079456, 9.846743663894594434 ) ) ;
#16845 = CARTESIAN_POINT ( 'NONE',  ( 19.84674366389459266, 8.717264484334116048, -2.638427012816827677 ) ) ;
#16846 = ORIENTED_EDGE ( 'NONE', *, *, #31510, .F. ) ;
#16847 = CARTESIAN_POINT ( 'NONE',  ( -9.990730578767623271, 46.91630561652144138, 2.899999999999999467 ) ) ;
#16848 = CARTESIAN_POINT ( 'NONE',  ( 2.815433093577121682, 14.63595249122789177, -14.73340885523751354 ) ) ;
#16849 = CARTESIAN_POINT ( 'NONE',  ( 20.36894250292379738, 49.92874883491396787, -10.36894250292379027 ) ) ;
#16850 = CARTESIAN_POINT ( 'NONE',  ( 24.16423886937410614, 9.512082168247301794, -3.795296366450302550 ) ) ;
#16851 = CARTESIAN_POINT ( 'NONE',  ( 12.91533473730992121, 19.52201867748816611, 10.88017736071110164 ) ) ;
#16852 = CARTESIAN_POINT ( 'NONE',  ( 17.96484262340118221, 29.93868534415484106, 7.964842623401181321 ) ) ;
#16853 = FACE_OUTER_BOUND ( 'NONE', #45784, .T. ) ;
#16854 = CARTESIAN_POINT ( 'NONE',  ( 4.559911319644449179, 67.23035201082150536, -9.422509992056141925 ) ) ;
#16855 = CARTESIAN_POINT ( 'NONE',  ( -19.19000000000001194, 93.50000000000000000, -10.09898361729590199 ) ) ;
#16856 = CARTESIAN_POINT ( 'NONE',  ( 2.791683348922240793, 21.63393115100078745, 7.208316651077764092 ) ) ;
#16857 = CARTESIAN_POINT ( 'NONE',  ( 2.313926553644105868E-17, 1.839999999999999636, 0.000000000000000000 ) ) ;
#16858 = CYLINDRICAL_SURFACE ( 'NONE', #85043, 0.5000000000000004441 ) ;
#16859 = CARTESIAN_POINT ( 'NONE',  ( 1.472469842513823179, 10.59226448433411782, -4.923371831947296329 ) ) ;
#16860 = CARTESIAN_POINT ( 'NONE',  ( 19.84674366389459266, 38.30059781766745175, 2.638427012816836559 ) ) ;
#16861 = TOROIDAL_SURFACE ( 'NONE', #8856, 14.49999999999999822, 0.5000000000000000000 ) ;
#16862 = CARTESIAN_POINT ( 'NONE',  ( 15.44008868035555260, 9.730352010821505360, 9.422509992056143702 ) ) ;
#16864 = ADVANCED_FACE ( 'NONE', ( #18362 ), #56841, .T. ) ;
#16863 = CARTESIAN_POINT ( 'NONE',  ( 10.00000000000000178, 30.37363466993042138, 12.81628187352647608 ) ) ;
#16865 = TOROIDAL_SURFACE ( 'NONE', #21648, 3.690000000000000391, 0.2500000000000000000 ) ;
#16866 = CARTESIAN_POINT ( 'NONE',  ( 15.44008868035555260, 54.73035201082150536, 9.422509992056143702 ) ) ;
#16868 = CARTESIAN_POINT ( 'NONE',  ( 18.52753015748618282, 13.92559781766745175, -4.923371831947291888 ) ) ;
#16867 = CARTESIAN_POINT ( 'NONE',  ( -0.3689425029237898834, 46.17874883491397497, -10.36894250292378850 ) ) ;
#16869 = PLANE ( 'NONE',  #31041 ) ;
#16870 = CARTESIAN_POINT ( 'NONE',  ( 10.00000000000000000, 49.75893115100078745, -9.846743663894594434 ) ) ;
#16872 = CARTESIAN_POINT ( 'NONE',  ( 2.917880565312948704, 12.63708216824730179, 12.26659068614894643 ) ) ;
#16871 = CARTESIAN_POINT ( 'NONE',  ( 18.52753015748617571, 28.09226448433411960, 4.923371831947298993 ) ) ;
#16873 = CARTESIAN_POINT ( 'NONE',  ( 6.204703633549690345, 22.84541550158062861, 14.16423886937410082 ) ) ;
#16874 = CARTESIAN_POINT ( 'NONE',  ( 19.42250999205614193, 40.14701867748817676, 5.440088680355555262 ) ) ;
#16875 = CARTESIAN_POINT ( 'NONE',  ( 10.00000000000000178, 9.313685344154839285, 10.88017736071110342 ) ) ;
#16876 = EDGE_CURVE ( 'NONE', #45246, #27971, #83967, .T. ) ;
#16877 = CARTESIAN_POINT ( 'NONE',  ( -0.8801773607110991993, 42.85535201082150536, -2.915334737309923874 ) ) ;
#16878 = CARTESIAN_POINT ( 'NONE',  ( 4.559911319644449179, 23.89701867748817321, 9.422509992056141925 ) ) ;
#16879 = ORIENTED_EDGE ( 'NONE', *, *, #53879, .T. ) ;
#16880 = CARTESIAN_POINT ( 'NONE',  ( 10.00000000000000178, 39.31368534415484106, 10.88017736071110342 ) ) ;
#16881 = ORIENTED_EDGE ( 'NONE', *, *, #76973, .T. ) ;
#16882 = CARTESIAN_POINT ( 'NONE',  ( 19.38216949554541557, 62.24863466993041072, -9.382169495545420901 ) ) ;
#16883 = CARTESIAN_POINT ( 'NONE',  ( 17.96484262340118221, 56.18868534415484817, -7.964842623401177768 ) ) ;
#16884 = VECTOR ( 'NONE', #17006, 1000.000000000000000 ) ;
#16885 = VERTEX_POINT ( 'NONE', #72815 ) ;
#16886 =( BOUNDED_SURFACE ( )  B_SPLINE_SURFACE ( 1, 2, ( 
 ( #64649, #42185, #6632, #91616, #68133, #92104, #15635, #84609, #84123, #16110, #68623, #45619, #14651, #53117, #53606, #98153, #45114, #98660, #60614, #46118, #15141, #22139, #153, #54094, #75622, #8121, #91112, #7134, #30602, #22636, #61107, #83625, #46596, #29126, #83123, #23133, #30108, #90122, #97659, #37148, #67644, #60116, #21650, #29611, #90615, #23635, #52135, #59627, #38616, #77095, #44630, #14146, #76116, #7645, #76605, #75125, #38136, #69117, #648, #52623, #37636, #31097, #61591, #36647, #67134, #82630, #40092, #94071, #26077, #48562, #39611, #86087, #70100, #62083, #54583, #1625, #25592, #92590, #70592, #17597, #48066, #79062, #2118, #16607, #94559, #32073, #62575, #47591, #9097, #32577, #87062, #77581, #63073, #78085, #93079, #78581, #1126, #24113, #47086, #10091, #39115, #2612, #56084, #3095, #24609, #85595, #64046, #10576, #55076, #40590, #93574, #17108, #9589, #56571, #18572, #25109, #55592, #41086, #71583, #71087, #18086, #31588, #85098, #33067, #86578, #63563, #49065, #33550, #8607, #69605, #73030, #58027, #28027, #5048, #19550, #35531, #66526, #96552, #59019, #11552, #34040, #26552, #42072, #58523, #64536, #12045, #88535, #20036, #51026, #4563, #87550, #97053, #72533, #4067, #50045, #80048, #42545, #89526, #49539, #35026, #80548, #34530, #50538, #72054, #95044, #19061, #81032, #11067, #73520, #89031, #74017, #65024, #57539, #36024, #81519, #95552, #12539, #65527, #27040, #88036, #28527, #21035, #96050, #27534, #13026, #43522, #43040, #20541, #3583, #57048, #66025, #5547, #79569, #41588, #76495, #29494, #22032, #45001, #29995, #40, #75999, #90497, #7527, #38506, #68510, #30982, #60502, #60003, #68016, #30489, #14034, #52506, #83013, #75506, #60987, #90992, #37025, #15026, #69003, #14531, #23020, #7020, #37526, #83509, #98543, #45499, #22522, #61481, #44011, #98039, #38017, #52994, #6035, #13529, #21531, #82516, #75011, #36534, #52024, #44512, #8008, #67023, #74515, #53489, #535, #59516, #29006, #91499, #84000, #15524, #90010, #46005, #91986, #51525, #67522, #6516, #82017, #97544, #25485, #40973, #71471, #54958, #9975, #2984, #63456, #54472, #1999, #84979, #76981, #69493, #16496, #40480, #8495, #85479, #32464, #62959, #93960, #16988, #31471, #10463, #46973, #77467, #62459, #23999, #47467, #33432, #92473, #77967, #92962, #8978, #93465, #15997, #38998, #61974, #24991, #53988, #17486, #70977, #17968, #39495, #1510, #78952, #55970, #69985, #55474, #9474, #31957, #24495, #63929, #23518, #39977, #70478, #86470, #48454, #85976, #32952, #46485, #1009, #47952, #2498, #78462, #84496, #20426, #72422, #64911 ),
 ( #3948, #11934, #12419, #56934, #34421, #26930, #19438, #42926, #72921, #79932, #57914, #12911, #95436, #65907, #49926, #57428, #27420, #80436, #88424, #42439, #73907, #86945, #41959, #80926, #87921, #48941, #56459, #64426, #26436, #18951, #79450, #94933, #87436, #50913, #10949, #18458, #96438, #81409, #3464, #71941, #4451, #34916, #73406, #33920, #65413, #95938, #19924, #11439, #49428, #27908, #50417, #58401, #43408, #5437, #4934, #35414, #35909, #88919, #94444, #25956, #41474, #45382, #74894, #83884, #91376, #44395, #36908, #59887, #44882, #14911, #90879, #6393, #22407, #53374, #83392, #45894, #75384, #67400, #82895, #75888, #28889, #97927, #29386, #90378, #7411, #6901, #51908, #29879, #15411, #21917, #37907, #52395, #14411, #98425, #37414, #60381, #67901, #76381, #58907, #13917, #52882, #68396, #20921, #28412, #36410, #97423, #89896, #51410, #66904, #59393, #22903, #81898, #89405, #98917, #7896, #74393, #43893, #30372, #60876, #66406, #5917, #96937, #13408, #21413, #82393, #8379, #40362, #32344, #70863, #55852, #86347, #69873, #24870, #17850, #78342, #69376, #16871, #898, #91879, #84391, #31360, #55352, #23400, #1393, #47345, #77848, #9863, #31848, #46375, #25367, #61860, #92364, #77352, #38888, #62346, #48335, #23891, #92851, #8863, #54356, #9357, #30873, #53884, #76864, #39862, #68893, #62847, #85858, #32833, #84868, #16377, #93840, #2378, #46859, #70368, #24379, #39379, #54845, #78839, #38390, #85359, #1886, #63335, #421, #93346, #47839, #61369, #15890, #17370, #58153, #67152, #59646, #89161, #80679, #21165, #35162, #12175, #42680, #90136, #50169, #73160, #51667, #20670, #88663, #21666, #13656, #74143, #94326, #5182, #13159, #5676, #51166, #52151, #82145, #44139, #58659, #10350, #97187, #81649, #43657, #28655, #4699, #74649, #73654, #35668, #36160, #27667, #50675, #66662, #65661, #28164, #97676, #40850, #6160, #89654, #36664, #2872, #71353, #29140, #20170, #66152, #12667, #96686, #33321, #81166, #96184, #63816, #25847, #43167, #59146, #57673, #88168, #19682, #22154, #61606, #67659, #75638, #14666, #52638, #46612, #76132, #23150, #53132, #22654, #8623, #53622, #83141, #38151, #1144, #44646, #62098, #83641, #92122, #68638, #45133, #167, #98169, #7150, #84142, #60132, #30615, #61123, #15155, #45634, #37653, #38631, #7660, #39133, #23650, #31604, #31112, #92606, #15651, #69134, #75140, #46134, #90630, #91632, #60628, #76620, #68151, #98674, #16127, #30123, #91130, #54111, #662, #8140, #84624, #77110, #24131, #69620, #82645, #14162, #6648, #37165, #29626, #25129, #48085, #33085, #3113, #79082, #93590, #10594, #41604 ) ),
 .UNSPECIFIED., .F., .F., .F. ) 
 B_SPLINE_SURFACE_WITH_KNOTS ( ( 2, 2 ),
 ( 3, 2, 2, 2, 2, 2, 2, 2, 2, 2, 2, 2, 2, 2, 2, 2, 2, 2, 2, 2, 2, 2, 2, 2, 2, 2, 2, 2, 2, 2, 2, 2, 2, 2, 2, 2, 2, 2, 2, 2, 2, 2, 2, 2, 2, 2, 2, 2, 2, 2, 2, 2, 2, 2, 2, 2, 2, 2, 2, 2, 2, 2, 2, 2, 2, 2, 2, 2, 2, 2, 2, 2, 2, 2, 2, 2, 2, 2, 2, 2, 2, 2, 2, 2, 2, 2, 2, 2, 2, 2, 2, 2, 2, 2, 2, 2, 2, 2, 2, 2, 2, 2, 2, 2, 2, 2, 2, 2, 2, 2, 2, 2, 2, 2, 2, 2, 2, 2, 2, 2, 2, 2, 2, 2, 2, 2, 2, 2, 2, 2, 2, 2, 2, 2, 2, 2, 2, 2, 2, 2, 2, 2, 2, 2, 2, 2, 2, 2, 2, 2, 2, 2, 2, 2, 2, 2, 2, 2, 2, 2, 2, 2, 3 ),
 ( 0.000000000000000000, 1.000000000000000000 ),
 ( 0.000000000000000000, 0.005952380952380952051, 0.01190476190476190410, 0.01785714285714285615, 0.02380952380952380820, 0.02976190476190476025, 0.03571428571428571230, 0.04166666666666666435, 0.04761904761904761640, 0.05357142857142856845, 0.05952380952380952051, 0.06547619047619047949, 0.07142857142857142461, 0.07738095238095238360, 0.08333333333333332871, 0.08928571428571428770, 0.09523809523809523281, 0.1011904761904761918, 0.1071428571428571369, 0.1130952380952380959, 0.1190476190476190410, 0.1250000000000000000, 0.1309523809523809590, 0.1369047619047619180, 0.1428571428571428492, 0.1488095238095238082, 0.1547619047619047672, 0.1607142857142857262, 0.1666666666666666574, 0.1726190476190476164, 0.1785714285714285754, 0.1845238095238095344, 0.1904761904761904656, 0.1964285714285714246, 0.2023809523809523836, 0.2083333333333333426, 0.2142857142857142738, 0.2202380952380952328, 0.2261904761904761918, 0.2321428571428571508, 0.2380952380952380820, 0.2440476190476190410, 0.2500000000000000000, 0.2559523809523809312, 0.2619047619047619180, 0.2678571428571428492, 0.2738095238095238360, 0.2797619047619047672, 0.2857142857142856984, 0.2916666666666666852, 0.2976190476190476164, 0.3035714285714285476, 0.3095238095238095344, 0.3154761904761904656, 0.3214285714285714524, 0.3273809523809523836, 0.3333333333333333148, 0.3392857142857143016, 0.3452380952380952328, 0.3511904761904761640, 0.3571428571428571508, 0.3630952380952380820, 0.3690476190476190688, 0.3750000000000000000, 0.3809523809523809312, 0.3869047619047619180, 0.3928571428571428492, 0.3988095238095238360, 0.4047619047619047672, 0.4107142857142856984, 0.4166666666666666852, 0.4226190476190476164, 0.4285714285714285476, 0.4345238095238095344, 0.4404761904761904656, 0.4464285714285714524, 0.4523809523809523836, 0.4583333333333333148, 0.4642857142857143016, 0.4702380952380952328, 0.4761904761904761640, 0.4821428571428571508, 0.4880952380952380820, 0.4940476190476190688, 0.5000000000000000000, 0.5059523809523809312, 0.5119047619047618625, 0.5178571428571429047, 0.5238095238095238360, 0.5297619047619047672, 0.5357142857142856984, 0.5416666666666666297, 0.5476190476190476719, 0.5535714285714286031, 0.5595238095238095344, 0.5654761904761904656, 0.5714285714285713969, 0.5773809523809523281, 0.5833333333333333703, 0.5892857142857143016, 0.5952380952380952328, 0.6011904761904761640, 0.6071428571428570953, 0.6130952380952381375, 0.6190476190476190688, 0.6250000000000000000, 0.6309523809523809312, 0.6369047619047618625, 0.6428571428571429047, 0.6488095238095238360, 0.6547619047619047672, 0.6607142857142856984, 0.6666666666666666297, 0.6726190476190476719, 0.6785714285714286031, 0.6845238095238095344, 0.6904761904761904656, 0.6964285714285713969, 0.7023809523809523281, 0.7083333333333333703, 0.7142857142857143016, 0.7202380952380952328, 0.7261904761904761640, 0.7321428571428570953, 0.7380952380952381375, 0.7440476190476190688, 0.7500000000000000000, 0.7559523809523809312, 0.7619047619047618625, 0.7678571428571429047, 0.7738095238095238360, 0.7797619047619047672, 0.7857142857142856984, 0.7916666666666666297, 0.7976190476190476719, 0.8035714285714286031, 0.8095238095238095344, 0.8154761904761904656, 0.8214285714285713969, 0.8273809523809523281, 0.8333333333333333703, 0.8392857142857143016, 0.8452380952380952328, 0.8511904761904761640, 0.8571428571428570953, 0.8630952380952381375, 0.8690476190476190688, 0.8750000000000000000, 0.8809523809523809312, 0.8869047619047618625, 0.8928571428571429047, 0.8988095238095238360, 0.9047619047619047672, 0.9107142857142856984, 0.9166666666666666297, 0.9226190476190476719, 0.9285714285714286031, 0.9345238095238095344, 0.9404761904761904656, 0.9464285714285713969, 0.9523809523809523281, 0.9583333333333333703, 0.9642857142857143016 ),
 .UNSPECIFIED. ) 
 GEOMETRIC_REPRESENTATION_ITEM ( )  RATIONAL_B_SPLINE_SURFACE ( (
 ( 1.000000000000000000, 0.9659258262890683122, 1.000000000000000000, 0.9659258262890683122, 1.000000000000000000, 0.9659258262890683122, 1.000000000000000000, 0.9659258262890683122, 1.000000000000000000, 0.9659258262890683122, 1.000000000000000000, 0.9659258262890683122, 1.000000000000000000, 0.9659258262890683122, 1.000000000000000000, 0.9659258262890683122, 1.000000000000000000, 0.9659258262890683122, 1.000000000000000000, 0.9659258262890683122, 1.000000000000000000, 0.9659258262890683122, 1.000000000000000000, 0.9659258262890683122, 1.000000000000000000, 0.9659258262890683122, 1.000000000000000000, 0.9659258262890683122, 1.000000000000000000, 0.9659258262890683122, 1.000000000000000000, 0.9659258262890683122, 1.000000000000000000, 0.9659258262890683122, 1.000000000000000000, 0.9659258262890683122, 1.000000000000000000, 0.9659258262890683122, 1.000000000000000000, 0.9659258262890683122, 1.000000000000000000, 0.9659258262890683122, 1.000000000000000000, 0.9659258262890683122, 1.000000000000000000, 0.9659258262890683122, 1.000000000000000000, 0.9659258262890683122, 1.000000000000000000, 0.9659258262890683122, 1.000000000000000000, 0.9659258262890683122, 1.000000000000000000, 0.9659258262890683122, 1.000000000000000000, 0.9659258262890683122, 1.000000000000000000, 0.9659258262890683122, 1.000000000000000000, 0.9659258262890683122, 1.000000000000000000, 0.9659258262890683122, 1.000000000000000000, 0.9659258262890683122, 1.000000000000000000, 0.9659258262890683122, 1.000000000000000000, 0.9659258262890683122, 1.000000000000000000, 0.9659258262890683122, 1.000000000000000000, 0.9659258262890683122, 1.000000000000000000, 0.9659258262890683122, 1.000000000000000000, 0.9659258262890683122, 1.000000000000000000, 0.9659258262890683122, 1.000000000000000000, 0.9659258262890683122, 1.000000000000000000, 0.9659258262890683122, 1.000000000000000000, 0.9659258262890683122, 1.000000000000000000, 0.9659258262890683122, 1.000000000000000000, 0.9659258262890683122, 1.000000000000000000, 0.9659258262890683122, 1.000000000000000000, 0.9659258262890683122, 1.000000000000000000, 0.9659258262890683122, 1.000000000000000000, 0.9659258262890683122, 1.000000000000000000, 0.9659258262890683122, 1.000000000000000000, 0.9659258262890683122, 1.000000000000000000, 0.9659258262890683122, 1.000000000000000000, 0.9659258262890683122, 1.000000000000000000, 0.9659258262890683122, 1.000000000000000000, 0.9659258262890683122, 1.000000000000000000, 0.9659258262890683122, 1.000000000000000000, 0.9659258262890683122, 1.000000000000000000, 0.9659258262890683122, 1.000000000000000000, 0.9659258262890683122, 1.000000000000000000, 0.9659258262890683122, 1.000000000000000000, 0.9659258262890683122, 1.000000000000000000, 0.9659258262890683122, 1.000000000000000000, 0.9659258262890683122, 1.000000000000000000, 0.9659258262890683122, 1.000000000000000000, 0.9659258262890683122, 1.000000000000000000, 0.9659258262890683122, 1.000000000000000000, 0.9659258262890683122, 1.000000000000000000, 0.9659258262890683122, 1.000000000000000000, 0.9659258262890683122, 1.000000000000000000, 0.9659258262890683122, 1.000000000000000000, 0.9659258262890683122, 1.000000000000000000, 0.9659258262890683122, 1.000000000000000000, 0.9659258262890683122, 1.000000000000000000, 0.9659258262890683122, 1.000000000000000000, 0.9659258262890683122, 1.000000000000000000, 0.9659258262890683122, 1.000000000000000000, 0.9659258262890683122, 1.000000000000000000, 0.9659258262890683122, 1.000000000000000000, 0.9659258262890683122, 1.000000000000000000, 0.9659258262890683122, 1.000000000000000000, 0.9659258262890683122, 1.000000000000000000, 0.9659258262890683122, 1.000000000000000000, 0.9659258262890683122, 1.000000000000000000, 0.9659258262890683122, 1.000000000000000000, 0.9659258262890683122, 1.000000000000000000, 0.9659258262890683122, 1.000000000000000000, 0.9659258262890683122, 1.000000000000000000, 0.9659258262890683122, 1.000000000000000000, 0.9659258262890683122, 1.000000000000000000, 0.9659258262890683122, 1.000000000000000000, 0.9659258262890683122, 1.000000000000000000, 0.9659258262890683122, 1.000000000000000000, 0.9659258262890683122, 1.000000000000000000, 0.9659258262890683122, 1.000000000000000000, 0.9659258262890683122, 1.000000000000000000, 0.9659258262890683122, 1.000000000000000000, 0.9659258262890683122, 1.000000000000000000, 0.9659258262890683122, 1.000000000000000000, 0.9659258262890683122, 1.000000000000000000, 0.9659258262890683122, 1.000000000000000000, 0.9659258262890683122, 1.000000000000000000, 0.9659258262890683122, 1.000000000000000000, 0.9659258262890683122, 1.000000000000000000, 0.9659258262890683122, 1.000000000000000000, 0.9659258262890683122, 1.000000000000000000, 0.9659258262890683122, 1.000000000000000000, 0.9659258262890683122, 1.000000000000000000, 0.9659258262890683122, 1.000000000000000000, 0.9659258262890683122, 1.000000000000000000, 0.9659258262890683122, 1.000000000000000000, 0.9659258262890683122, 1.000000000000000000, 0.9659258262890683122, 1.000000000000000000, 0.9659258262890683122, 1.000000000000000000, 0.9659258262890683122, 1.000000000000000000, 0.9659258262890683122, 1.000000000000000000, 0.9659258262890683122, 1.000000000000000000, 0.9659258262890683122, 1.000000000000000000, 0.9659258262890683122, 1.000000000000000000, 0.9659258262890683122, 1.000000000000000000, 0.9659258262890683122, 1.000000000000000000, 0.9659258262890683122, 1.000000000000000000, 0.9659258262890683122, 1.000000000000000000, 0.9659258262890683122, 1.000000000000000000, 0.9659258262890683122, 1.000000000000000000, 0.9659258262890683122, 1.000000000000000000, 0.9659258262890683122, 1.000000000000000000, 0.9659258262890683122, 1.000000000000000000, 0.9659258262890683122, 1.000000000000000000, 0.9659258262890683122, 1.000000000000000000, 0.9659258262890683122, 1.000000000000000000, 0.9659258262890683122, 1.000000000000000000, 0.9659258262890683122, 1.000000000000000000, 0.9659258262890683122, 1.000000000000000000, 0.9659258262890683122, 1.000000000000000000, 0.9659258262890683122, 1.000000000000000000, 0.9659258262890683122, 1.000000000000000000, 0.9659258262890683122, 1.000000000000000000, 0.9659258262890683122, 1.000000000000000000, 0.9659258262890683122, 1.000000000000000000, 0.9659258262890683122, 1.000000000000000000, 0.9659258262890683122, 1.000000000000000000, 0.9659258262890683122, 1.000000000000000000, 0.9659258262890683122, 1.000000000000000000, 0.9659258262890683122, 1.000000000000000000, 0.9659258262890683122, 1.000000000000000000, 0.9659258262890683122, 1.000000000000000000, 0.9659258262890683122, 1.000000000000000000, 0.9659258262890683122, 1.000000000000000000, 0.9659258262890683122, 1.000000000000000000, 0.9659258262890683122, 1.000000000000000000, 0.9659258262890683122, 1.000000000000000000, 0.9659258262890683122, 1.000000000000000000, 0.9659258262890683122, 1.000000000000000000, 0.9659258262890683122, 1.000000000000000000, 0.9659258262890683122, 1.000000000000000000, 0.9659258262890683122, 1.000000000000000000, 0.9659258262890683122, 1.000000000000000000, 0.9659258262890683122, 1.000000000000000000, 0.9659258262890683122, 1.000000000000000000, 0.9659258262890683122, 1.000000000000000000, 0.9659258262890683122, 1.000000000000000000, 0.9659258262890683122, 1.000000000000000000, 0.9659258262890683122, 1.000000000000000000),
 ( 1.000000000000000000, 0.9659258262890683122, 1.000000000000000000, 0.9659258262890683122, 1.000000000000000000, 0.9659258262890683122, 1.000000000000000000, 0.9659258262890683122, 1.000000000000000000, 0.9659258262890683122, 1.000000000000000000, 0.9659258262890683122, 1.000000000000000000, 0.9659258262890683122, 1.000000000000000000, 0.9659258262890683122, 1.000000000000000000, 0.9659258262890683122, 1.000000000000000000, 0.9659258262890683122, 1.000000000000000000, 0.9659258262890683122, 1.000000000000000000, 0.9659258262890683122, 1.000000000000000000, 0.9659258262890683122, 1.000000000000000000, 0.9659258262890683122, 1.000000000000000000, 0.9659258262890683122, 1.000000000000000000, 0.9659258262890683122, 1.000000000000000000, 0.9659258262890683122, 1.000000000000000000, 0.9659258262890683122, 1.000000000000000000, 0.9659258262890683122, 1.000000000000000000, 0.9659258262890683122, 1.000000000000000000, 0.9659258262890683122, 1.000000000000000000, 0.9659258262890683122, 1.000000000000000000, 0.9659258262890683122, 1.000000000000000000, 0.9659258262890683122, 1.000000000000000000, 0.9659258262890683122, 1.000000000000000000, 0.9659258262890683122, 1.000000000000000000, 0.9659258262890683122, 1.000000000000000000, 0.9659258262890683122, 1.000000000000000000, 0.9659258262890683122, 1.000000000000000000, 0.9659258262890683122, 1.000000000000000000, 0.9659258262890683122, 1.000000000000000000, 0.9659258262890683122, 1.000000000000000000, 0.9659258262890683122, 1.000000000000000000, 0.9659258262890683122, 1.000000000000000000, 0.9659258262890683122, 1.000000000000000000, 0.9659258262890683122, 1.000000000000000000, 0.9659258262890683122, 1.000000000000000000, 0.9659258262890683122, 1.000000000000000000, 0.9659258262890683122, 1.000000000000000000, 0.9659258262890683122, 1.000000000000000000, 0.9659258262890683122, 1.000000000000000000, 0.9659258262890683122, 1.000000000000000000, 0.9659258262890683122, 1.000000000000000000, 0.9659258262890683122, 1.000000000000000000, 0.9659258262890683122, 1.000000000000000000, 0.9659258262890683122, 1.000000000000000000, 0.9659258262890683122, 1.000000000000000000, 0.9659258262890683122, 1.000000000000000000, 0.9659258262890683122, 1.000000000000000000, 0.9659258262890683122, 1.000000000000000000, 0.9659258262890683122, 1.000000000000000000, 0.9659258262890683122, 1.000000000000000000, 0.9659258262890683122, 1.000000000000000000, 0.9659258262890683122, 1.000000000000000000, 0.9659258262890683122, 1.000000000000000000, 0.9659258262890683122, 1.000000000000000000, 0.9659258262890683122, 1.000000000000000000, 0.9659258262890683122, 1.000000000000000000, 0.9659258262890683122, 1.000000000000000000, 0.9659258262890683122, 1.000000000000000000, 0.9659258262890683122, 1.000000000000000000, 0.9659258262890683122, 1.000000000000000000, 0.9659258262890683122, 1.000000000000000000, 0.9659258262890683122, 1.000000000000000000, 0.9659258262890683122, 1.000000000000000000, 0.9659258262890683122, 1.000000000000000000, 0.9659258262890683122, 1.000000000000000000, 0.9659258262890683122, 1.000000000000000000, 0.9659258262890683122, 1.000000000000000000, 0.9659258262890683122, 1.000000000000000000, 0.9659258262890683122, 1.000000000000000000, 0.9659258262890683122, 1.000000000000000000, 0.9659258262890683122, 1.000000000000000000, 0.9659258262890683122, 1.000000000000000000, 0.9659258262890683122, 1.000000000000000000, 0.9659258262890683122, 1.000000000000000000, 0.9659258262890683122, 1.000000000000000000, 0.9659258262890683122, 1.000000000000000000, 0.9659258262890683122, 1.000000000000000000, 0.9659258262890683122, 1.000000000000000000, 0.9659258262890683122, 1.000000000000000000, 0.9659258262890683122, 1.000000000000000000, 0.9659258262890683122, 1.000000000000000000, 0.9659258262890683122, 1.000000000000000000, 0.9659258262890683122, 1.000000000000000000, 0.9659258262890683122, 1.000000000000000000, 0.9659258262890683122, 1.000000000000000000, 0.9659258262890683122, 1.000000000000000000, 0.9659258262890683122, 1.000000000000000000, 0.9659258262890683122, 1.000000000000000000, 0.9659258262890683122, 1.000000000000000000, 0.9659258262890683122, 1.000000000000000000, 0.9659258262890683122, 1.000000000000000000, 0.9659258262890683122, 1.000000000000000000, 0.9659258262890683122, 1.000000000000000000, 0.9659258262890683122, 1.000000000000000000, 0.9659258262890683122, 1.000000000000000000, 0.9659258262890683122, 1.000000000000000000, 0.9659258262890683122, 1.000000000000000000, 0.9659258262890683122, 1.000000000000000000, 0.9659258262890683122, 1.000000000000000000, 0.9659258262890683122, 1.000000000000000000, 0.9659258262890683122, 1.000000000000000000, 0.9659258262890683122, 1.000000000000000000, 0.9659258262890683122, 1.000000000000000000, 0.9659258262890683122, 1.000000000000000000, 0.9659258262890683122, 1.000000000000000000, 0.9659258262890683122, 1.000000000000000000, 0.9659258262890683122, 1.000000000000000000, 0.9659258262890683122, 1.000000000000000000, 0.9659258262890683122, 1.000000000000000000, 0.9659258262890683122, 1.000000000000000000, 0.9659258262890683122, 1.000000000000000000, 0.9659258262890683122, 1.000000000000000000, 0.9659258262890683122, 1.000000000000000000, 0.9659258262890683122, 1.000000000000000000, 0.9659258262890683122, 1.000000000000000000, 0.9659258262890683122, 1.000000000000000000, 0.9659258262890683122, 1.000000000000000000, 0.9659258262890683122, 1.000000000000000000, 0.9659258262890683122, 1.000000000000000000, 0.9659258262890683122, 1.000000000000000000, 0.9659258262890683122, 1.000000000000000000, 0.9659258262890683122, 1.000000000000000000, 0.9659258262890683122, 1.000000000000000000, 0.9659258262890683122, 1.000000000000000000, 0.9659258262890683122, 1.000000000000000000, 0.9659258262890683122, 1.000000000000000000, 0.9659258262890683122, 1.000000000000000000, 0.9659258262890683122, 1.000000000000000000, 0.9659258262890683122, 1.000000000000000000, 0.9659258262890683122, 1.000000000000000000, 0.9659258262890683122, 1.000000000000000000, 0.9659258262890683122, 1.000000000000000000, 0.9659258262890683122, 1.000000000000000000, 0.9659258262890683122, 1.000000000000000000, 0.9659258262890683122, 1.000000000000000000, 0.9659258262890683122, 1.000000000000000000, 0.9659258262890683122, 1.000000000000000000, 0.9659258262890683122, 1.000000000000000000, 0.9659258262890683122, 1.000000000000000000, 0.9659258262890683122, 1.000000000000000000, 0.9659258262890683122, 1.000000000000000000, 0.9659258262890683122, 1.000000000000000000, 0.9659258262890683122, 1.000000000000000000, 0.9659258262890683122, 1.000000000000000000, 0.9659258262890683122, 1.000000000000000000, 0.9659258262890683122, 1.000000000000000000, 0.9659258262890683122, 1.000000000000000000, 0.9659258262890683122, 1.000000000000000000, 0.9659258262890683122, 1.000000000000000000, 0.9659258262890683122, 1.000000000000000000, 0.9659258262890683122, 1.000000000000000000, 0.9659258262890683122, 1.000000000000000000, 0.9659258262890683122, 1.000000000000000000, 0.9659258262890683122, 1.000000000000000000, 0.9659258262890683122, 1.000000000000000000, 0.9659258262890683122, 1.000000000000000000, 0.9659258262890683122, 1.000000000000000000, 0.9659258262890683122, 1.000000000000000000, 0.9659258262890683122, 1.000000000000000000, 0.9659258262890683122, 1.000000000000000000) ) ) 
 REPRESENTATION_ITEM ( '' )  SURFACE ( )  );
#16887 = CARTESIAN_POINT ( 'NONE',  ( 20.88017736071110164, 45.35535201082149115, 2.915334737309930979 ) ) ;
#16888 = VECTOR ( 'NONE', #68464, 1000.000000000000000 ) ;
#16889 = CARTESIAN_POINT ( 'NONE',  ( -0.2418659066527510948, 24.26028685723174050, -6.114288769123079170 ) ) ;
#16890 = CARTESIAN_POINT ( 'NONE',  ( 20.36894250292379382, 53.67874883491397497, 10.36894250292379205 ) ) ;
#16891 = CARTESIAN_POINT ( 'NONE',  ( 4.559911319644449179, 63.89701867748817676, 9.422509992056141925 ) ) ;
#16892 = VERTEX_POINT ( 'NONE', #55375 ) ;
#16893 = CARTESIAN_POINT ( 'NONE',  ( -4.164238869374099927, 12.01208216824730357, 3.795296366450308767 ) ) ;
#16894 = STYLED_ITEM ( 'NONE', ( #15018 ), #86133 ) ;
#16895 = CARTESIAN_POINT ( 'NONE',  ( -6.281451360760612168, -39.80862496263591055, -3.999999999999998224 ) ) ;
#16896 = CARTESIAN_POINT ( 'NONE',  ( 7.084665262690076126, 9.105352010821503583, 10.88017736071109987 ) ) ;
#16897 = CARTESIAN_POINT ( 'NONE',  ( 17.20831665107776587, 52.88393115100078035, 7.208316651077764980 ) ) ;
#16898 = VERTEX_POINT ( 'NONE', #87340 ) ;
#16899 = CARTESIAN_POINT ( 'NONE',  ( 19.84674366389459266, 48.71726448433413026, -2.638427012816827677 ) ) ;
#16900 = CARTESIAN_POINT ( 'NONE',  ( 0.5774900079438607392, 63.48035201082149825, 5.440088680355550821 ) ) ;
#16901 = CARTESIAN_POINT ( 'NONE',  ( 4.559911319644449179, 37.23035201082150536, -9.422509992056141925 ) ) ;
#16902 = CARTESIAN_POINT ( 'NONE',  ( 10.00000000000000178, 32.25893115100078745, 9.846743663894594434 ) ) ;
#16903 = CARTESIAN_POINT ( 'NONE',  ( 22.81628187352648496, 31.83196800326375353, -3.434112377981050290 ) ) ;
#16905 = DIRECTION ( 'NONE',  ( 1.000000000000000000, 0.000000000000000000, 0.000000000000000000 ) ) ;
#16904 = CARTESIAN_POINT ( 'NONE',  ( 0.000000000000000000, 14.49999999999999822, 0.000000000000000000 ) ) ;
#16906 = CARTESIAN_POINT ( 'NONE',  ( -0.8801773607110991993, 42.85535201082150536, -2.915334737309923874 ) ) ;
#16907 = CARTESIAN_POINT ( 'NONE',  ( 17.08211943468705130, 58.47041550158063927, 12.26659068614894998 ) ) ;
#16908 = ADVANCED_FACE ( 'NONE', ( #2398 ), #7403, .T. ) ;
#16909 = VECTOR ( 'NONE', #85688, 1000.000000000000000 ) ;
#16910 = CARTESIAN_POINT ( 'NONE',  ( 21.09922568453595559, 17.04030133659708923, -6.408140936763230044 ) ) ;
#16911 = LINE ( 'NONE', #53917, #22803 ) ;
#16912 = ORIENTED_EDGE ( 'NONE', *, *, #68349, .T. ) ;
#16913 = CARTESIAN_POINT ( 'NONE',  ( -2.816281873526473856, 29.33196800326376064, 3.434112377981055619 ) ) ;
#16914 = CARTESIAN_POINT ( 'NONE',  ( 19.42250999205614193, 20.14701867748817321, 5.440088680355555262 ) ) ;
#16915 = ORIENTED_EDGE ( 'NONE', *, *, #28276, .T. ) ;
#16916 = CARTESIAN_POINT ( 'NONE',  ( 0.1532563361054100626, 45.80059781766745886, -2.638427012816831230 ) ) ;
#16918 = CARTESIAN_POINT ( 'NONE',  ( 14.92337183194729988, 39.34226448433412315, -8.527530157486177487 ) ) ;
#16917 = CARTESIAN_POINT ( 'NONE',  ( 1.472469842513823179, 15.59226448433411960, -4.923371831947296329 ) ) ;
#16919 = DIRECTION ( 'NONE',  ( -0.9799247046208282574, 0.000000000000000000, -0.1993679344172039347 ) ) ;
#16920 = CARTESIAN_POINT ( 'NONE',  ( 0.000000000000000000, 0.5000000000000004441, 0.000000000000000000 ) ) ;
#16921 = CARTESIAN_POINT ( 'NONE',  ( 10.00000000000000178, 22.25893115100078745, 9.846743663894594434 ) ) ;
#16922 = LINE ( 'NONE', #77900, #87541 ) ;
#16923 = VECTOR ( 'NONE', #16701, 1000.000000000000000 ) ;
#16924 = CARTESIAN_POINT ( 'NONE',  ( 0.000000000000000000, 14.49999999999999822, 0.000000000000000000 ) ) ;
#16926 = CARTESIAN_POINT ( 'NONE',  ( 0.1532563361054100626, 0.8005978176674514168, -2.638427012816831230 ) ) ;
#16925 = CARTESIAN_POINT ( 'NONE',  ( 0.1532563361054100626, 25.80059781766744820, -2.638427012816831230 ) ) ;
#16928 = ORIENTED_EDGE ( 'NONE', *, *, #7933, .F. ) ;
#16927 = CARTESIAN_POINT ( 'NONE',  ( 5.076628168052703671, 41.84226448433411605, 8.527530157486179263 ) ) ;
#16929 = CARTESIAN_POINT ( 'NONE',  ( 19.80427997160309417, 7.757339608395445119, -6.499999999999999112 ) ) ;
#16930 = CARTESIAN_POINT ( 'NONE',  ( 19.38216949554541202, 30.99863466993042138, 9.382169495545424454 ) ) ;
#16931 = CARTESIAN_POINT ( 'NONE',  ( -13.77612262535527954, 90.93158326518027934, 7.883772450803742338 ) ) ;
#16932 = CARTESIAN_POINT ( 'NONE',  ( 10.00000000000000000, 50.55374883491396787, -14.16423886937410082 ) ) ;
#16933 = CARTESIAN_POINT ( 'NONE',  ( 19.84674366389459621, 23.50893115100078390, 7.409399052514197653E-17 ) ) ;
#16934 = DIRECTION ( 'NONE',  ( 0.000000000000000000, 0.000000000000000000, 1.000000000000000000 ) ) ;
#16935 = CARTESIAN_POINT ( 'NONE',  ( 10.00000000000000178, 43.05374883491397497, 14.16423886937410082 ) ) ;
#16936 = CARTESIAN_POINT ( 'NONE',  ( 14.92337183194729633, 57.67559781766745886, 8.527530157486181039 ) ) ;
#16937 = CARTESIAN_POINT ( 'NONE',  ( 6.204703633549690345, 52.84541550158062506, 14.16423886937410082 ) ) ;
#16938 = CARTESIAN_POINT ( 'NONE',  ( -4.164238869374098151, 26.59541550158063217, -3.795296366450310543 ) ) ;
#16939 = CARTESIAN_POINT ( 'NONE',  ( -0.3689425029237898834, 26.17874883491396432, -10.36894250292378850 ) ) ;
#16940 = PLANE ( 'NONE',  #91476 ) ;
#16941 = EDGE_CURVE ( 'NONE', #89575, #72583, #44057, .T. ) ;
#16943 = CARTESIAN_POINT ( 'NONE',  ( 2.791683348922237240, 45.38393115100079456, -7.208316651077763204 ) ) ;
#16942 = CARTESIAN_POINT ( 'NONE',  ( 4.380000000000000782, 1.019547802438464545, 2.750000000000000000 ) ) ;
#16944 = CARTESIAN_POINT ( 'NONE',  ( 20.88017736071110164, 30.35535201082151247, 2.915334737309930979 ) ) ;
#16945 = FACE_OUTER_BOUND ( 'NONE', #18151, .T. ) ;
#16946 = CARTESIAN_POINT ( 'NONE',  ( 12.00809552683962700, 14.63606912728062959, -8.989195838243558612 ) ) ;
#16947 = CARTESIAN_POINT ( 'NONE',  ( 7.361572987183170547, 37.05059781766744464, 9.846743663894590881 ) ) ;
#16948 = CARTESIAN_POINT ( 'NONE',  ( 21.09922568453594849, 51.20696800326375353, 6.408140936763242479 ) ) ;
#16950 = CIRCLE ( 'NONE', #45707, 0.4999999999999967248 ) ;
#16949 = CARTESIAN_POINT ( 'NONE',  ( -10.36894250292378317, -12.57125116508602325, 10.36894250292379560 ) ) ;
#16951 = CARTESIAN_POINT ( 'NONE',  ( 18.52753015748617571, 48.09226448433412315, 4.923371831947298993 ) ) ;
#16952 = CARTESIAN_POINT ( 'NONE',  ( 13.55255535720595184, 15.00000000000000000, -4.403492169842965431 ) ) ;
#16953 = CIRCLE ( 'NONE', #66399, 0.2500000000000002220 ) ;
#16954 = EDGE_CURVE ( 'NONE', #45188, #42998, #41860, .T. ) ;
#16955 = EDGE_LOOP ( 'NONE', ( #3205, #68800, #25713, #12668 ) ) ;
#16956 = CARTESIAN_POINT ( 'NONE',  ( 24.16423886937409904, 9.095415501580633943, 3.795296366450317205 ) ) ;
#16957 = EDGE_CURVE ( 'NONE', #87897, #98547, #79835, .T. ) ;
#16958 = CIRCLE ( 'NONE', #91963, 0.5000000000000004441 ) ;
#16959 = EDGE_CURVE ( 'NONE', #89913, #39436, #31273, .T. ) ;
#16960 = CARTESIAN_POINT ( 'NONE',  ( -12.83294900548056994, 14.49999999999999112, -7.766300266068596692 ) ) ;
#16962 = CARTESIAN_POINT ( 'NONE',  ( 18.72515096720571037, 50.05509018479936856, 6.499999999999982236 ) ) ;
#16961 = CARTESIAN_POINT ( 'NONE',  ( 14.03351048042395632, -0.03417435944610275333, 2.474486531753810059 ) ) ;
#16963 = CARTESIAN_POINT ( 'NONE',  ( 17.96484262340118221, 6.188685344154837509, -7.964842623401177768 ) ) ;
#16964 = CARTESIAN_POINT ( 'NONE',  ( 13.43411237798105340, 15.58196800326374998, 12.81628187352647963 ) ) ;
#16965 =( BOUNDED_CURVE ( )  B_SPLINE_CURVE ( 2, ( #65388, #79906, #81384, #57403, #80411, #88401, #49406, #11415, #64883 ),
 .UNSPECIFIED., .F., .T. ) 
 B_SPLINE_CURVE_WITH_KNOTS ( ( 3, 2, 2, 2, 3 ),
 ( 0.04728379408308854698, 0.04761904761904767192, 0.05357142857142860315, 0.05952380952380953438, 0.05985906305976865238 ),
 .UNSPECIFIED. ) 
 CURVE ( )  GEOMETRIC_REPRESENTATION_ITEM ( )  RATIONAL_B_SPLINE_CURVE ( ( 0.9963778908391762723, 0.9980808541467921513, 1.000000000000000000, 0.9659258262890683122, 1.000000000000000000, 0.9659258262890683122, 1.000000000000000000, 0.9980808541467921513, 0.9963778908391762723 ) ) 
 REPRESENTATION_ITEM ( '' )  );
#16966 = DIRECTION ( 'NONE',  ( 0.06975647374412544122, 0.9975640502598241977, -0.000000000000000000 ) ) ;
#16967 = CARTESIAN_POINT ( 'NONE',  ( 10.00000000000000000, 61.81368534415484106, -10.88017736071110342 ) ) ;
#16968 = CARTESIAN_POINT ( 'NONE',  ( 0.9940297508536876103, 15.00000000000000000, 14.21528771620250353 ) ) ;
#16969 = DIRECTION ( 'NONE',  ( 0.000000000000000000, -0.000000000000000000, 1.000000000000000000 ) ) ;
#16970 = CARTESIAN_POINT ( 'NONE',  ( 12.80781515976314822, 15.00000000000000000, -6.246788841744324472 ) ) ;
#16971 = CARTESIAN_POINT ( 'NONE',  ( -4.164238869374099927, 67.01208216824728936, 3.795296366450308767 ) ) ;
#16972 = CARTESIAN_POINT ( 'NONE',  ( -3.541595367958631169, 0.000000000000000000, -4.146675399920641603 ) ) ;
#16973 = CARTESIAN_POINT ( 'NONE',  ( 20.88017736071110519, 25.56368534415483751, 2.639326808657452039E-16 ) ) ;
#16974 = CARTESIAN_POINT ( 'NONE',  ( 10.00000000000000178, 44.31368534415484106, 10.88017736071110342 ) ) ;
#16975 = CARTESIAN_POINT ( 'NONE',  ( 22.81628187352647785, 6.623634669930420493, 6.195893100308588602E-16 ) ) ;
#16976 = CARTESIAN_POINT ( 'NONE',  ( 19.84674366389459266, 53.30059781766744464, 2.638427012816836559 ) ) ;
#16977 = CARTESIAN_POINT ( 'NONE',  ( 6.565887622018943937, 58.08196800326376064, -12.81628187352647608 ) ) ;
#16978 =( LENGTH_UNIT ( ) NAMED_UNIT ( * ) SI_UNIT ( .MILLI., .METRE. ) );
#16979 = ORIENTED_EDGE ( 'NONE', *, *, #63943, .F. ) ;
#16980 = EDGE_CURVE ( 'NONE', #45794, #79527, #64810, .T. ) ;
#16981 = CARTESIAN_POINT ( 'NONE',  ( 20.88017736071110164, 35.35535201082150536, 2.915334737309930979 ) ) ;
#16982 = CARTESIAN_POINT ( 'NONE',  ( 22.81628187352648496, 31.83196800326375353, -3.434112377981050290 ) ) ;
#16983 = DIRECTION ( 'NONE',  ( 0.000000000000000000, 1.000000000000000000, 0.000000000000000000 ) ) ;
#16984 = CARTESIAN_POINT ( 'NONE',  ( 17.20831665107776587, 62.88393115100078745, 7.208316651077764980 ) ) ;
#16985 = CARTESIAN_POINT ( 'NONE',  ( 12.91533473730992121, 54.52201867748816255, 10.88017736071110164 ) ) ;
#16986 = CARTESIAN_POINT ( 'NONE',  ( 12.63842701281683034, 17.46726448433411250, 9.846743663894596210 ) ) ;
#16987 = CARTESIAN_POINT ( 'NONE',  ( 22.81628187352647785, 36.41530133659707502, 3.434112377981063169 ) ) ;
#16989 = CARTESIAN_POINT ( 'NONE',  ( 14.03351048042397231, 15.00000000000000000, -2.474486531753715024 ) ) ;
#16988 = CARTESIAN_POINT ( 'NONE',  ( 12.91533473730992121, 59.52201867748816966, 10.88017736071110164 ) ) ;
#16990 = CYLINDRICAL_SURFACE ( 'NONE', #56153, 15.00000000000000000 ) ;
#16991 = CARTESIAN_POINT ( 'NONE',  ( -1.099225684535947600, 63.70696800326376774, -6.408140936763238038 ) ) ;
#16992 = ORIENTED_EDGE ( 'NONE', *, *, #57910, .T. ) ;
#16993 = CARTESIAN_POINT ( 'NONE',  ( 0.000000000000000000, 15.00000000000000000, 0.000000000000000000 ) ) ;
#16994 = LINE ( 'NONE', #47473, #92553 ) ;
#16995 = CARTESIAN_POINT ( 'NONE',  ( -0.8801773607110991993, 2.855352010821504471, -2.915334737309923874 ) ) ;
#16996 = CARTESIAN_POINT ( 'NONE',  ( 16.40814093676323893, 45.79030133659708923, 11.09922568453595026 ) ) ;
#16997 = EDGE_CURVE ( 'NONE', #78552, #6506, #63249, .T. ) ;
#16998 = CARTESIAN_POINT ( 'NONE',  ( 5.076628168052703671, 16.84226448433411960, 8.527530157486179263 ) ) ;
#16999 = CARTESIAN_POINT ( 'NONE',  ( -0.8801773607111009756, 8.063685344154837509, 1.068504757029289695E-15 ) ) ;
#17000 = CARTESIAN_POINT ( 'NONE',  ( 1.472469842513823179, 26.42559781766745175, 4.923371831947296329 ) ) ;
#17001 = CARTESIAN_POINT ( 'NONE',  ( 20.36894250292379382, 53.67874883491397497, 10.36894250292379205 ) ) ;
#17002 = ORIENTED_EDGE ( 'NONE', *, *, #42681, .F. ) ;
#17003 = AXIS2_PLACEMENT_3D ( 'NONE', #15137, #84116, #7127 ) ;
#17004 = CARTESIAN_POINT ( 'NONE',  ( 7.084665262690076126, 12.02201867748817143, -10.88017736071110164 ) ) ;
#17005 = EDGE_CURVE ( 'NONE', #44298, #76727, #13255, .T. ) ;
#17006 = DIRECTION ( 'NONE',  ( -0.3826834323650877279, 0.000000000000000000, 0.9238795325112876267 ) ) ;
#17007 = VERTEX_POINT ( 'NONE', #40382 ) ;
#17008 = CARTESIAN_POINT ( 'NONE',  ( 20.88017736071110519, 5.563685344154838397, 2.639326808657452039E-16 ) ) ;
#17009 = CARTESIAN_POINT ( 'NONE',  ( 10.00000000000000000, 11.81368534415483751, -10.88017736071110342 ) ) ;
#17010 = CARTESIAN_POINT ( 'NONE',  ( 5.076628168052703671, 41.84226448433411605, 8.527530157486179263 ) ) ;
#17011 = CARTESIAN_POINT ( 'NONE',  ( 0.6178305044545838731, 54.74863466993042493, 9.382169495545420901 ) ) ;
#17012 = DIRECTION ( 'NONE',  ( 1.000000000000000000, 0.000000000000000000, 0.000000000000000000 ) ) ;
#17014 = CARTESIAN_POINT ( 'NONE',  ( -4.164238869374098151, 16.59541550158063927, -3.795296366450310543 ) ) ;
#17013 = DIRECTION ( 'NONE',  ( 0.000000000000000000, 1.000000000000000000, 0.000000000000000000 ) ) ;
#17015 = CARTESIAN_POINT ( 'NONE',  ( 4.559911319644449179, 28.89701867748817321, 9.422509992056141925 ) ) ;
#17016 = CARTESIAN_POINT ( 'NONE',  ( 10.00000000000000178, 9.313685344154839285, 10.88017736071110342 ) ) ;
#17017 = CARTESIAN_POINT ( 'NONE',  ( 2.791683348922240793, 61.63393115100079456, 7.208316651077764092 ) ) ;
#17018 = PRESENTATION_LAYER_ASSIGNMENT (  '', '', ( #45776 ) ) ;
#17019 = DIRECTION ( 'NONE',  ( -0.6755902076156540259, 0.000000000000000000, -0.7372773368101297464 ) ) ;
#17020 = CARTESIAN_POINT ( 'NONE',  ( 12.63842701281683034, 32.46726448433412315, 9.846743663894596210 ) ) ;
#17021 = DIRECTION ( 'NONE',  ( 0.000000000000000000, 0.000000000000000000, -1.000000000000000000 ) ) ;
#17022 = CARTESIAN_POINT ( 'NONE',  ( 7.361572987183169658, -0.03273551566588185635, -9.846743663894592657 ) ) ;
#17023 = CARTESIAN_POINT ( 'NONE',  ( 8.527530157486179263, 23.09226448433413026, 4.923371831947292776 ) ) ;
#17024 = ORIENTED_EDGE ( 'NONE', *, *, #84469, .T. ) ;
#17025 = CARTESIAN_POINT ( 'NONE',  ( -13.55255535720589322, 15.00000000000000000, -4.403492169843143067 ) ) ;
#17026 = CARTESIAN_POINT ( 'NONE',  ( 19.42250999205614548, 65.98035201082151957, -5.440088680355545492 ) ) ;
#17027 = CARTESIAN_POINT ( 'NONE',  ( 10.00000000000000178, 0.3736346699304200492, 12.81628187352647608 ) ) ;
#17028 = CARTESIAN_POINT ( 'NONE',  ( 19.42250999205614548, 50.98035201082151247, -5.440088680355545492 ) ) ;
#17030 = CARTESIAN_POINT ( 'NONE',  ( 21.09922568453594849, 41.20696800326375353, 6.408140936763242479 ) ) ;
#17029 = CARTESIAN_POINT ( 'NONE',  ( 10.00000000000000000, 1.813685344154837731, -10.88017736071110342 ) ) ;
#17031 = VECTOR ( 'NONE', #40688, 1000.000000000000000 ) ;
#17032 = CARTESIAN_POINT ( 'NONE',  ( -4.164238869374098151, 21.59541550158063217, -3.795296366450310543 ) ) ;
#17033 = AXIS2_PLACEMENT_3D ( 'NONE', #27253, #4282, #65246 ) ;
#17034 = B_SPLINE_CURVE_WITH_KNOTS ( 'NONE', 3,
 ( #1233, #56180, #31686, #25689, #9197, #18178 ),
 .UNSPECIFIED., .F., .F.,
 ( 4, 2, 4 ),
 ( 5.780498387344536870E-18, 0.0002626113303185893724, 0.0005252226606371728900 ),
 .UNSPECIFIED. ) ;
#17035 = ORIENTED_EDGE ( 'NONE', *, *, #82411, .F. ) ;
#17036 = CARTESIAN_POINT ( 'NONE',  ( -2.816281873526471635, 48.91530133659708213, -3.434112377981056508 ) ) ;
#17037 = ORIENTED_EDGE ( 'NONE', *, *, #3351, .T. ) ;
#17038 = CARTESIAN_POINT ( 'NONE',  ( 10.00000000000000178, 57.25893115100078745, 9.846743663894594434 ) ) ;
#17039 = CARTESIAN_POINT ( 'NONE',  ( 4.559911319644449179, 17.23035201082150536, -9.422509992056141925 ) ) ;
#17040 = CARTESIAN_POINT ( 'NONE',  ( 0.5774900079438607392, 33.48035201082150536, 5.440088680355550821 ) ) ;
#17041 = ORIENTED_EDGE ( 'NONE', *, *, #52861, .F. ) ;
#17042 = CARTESIAN_POINT ( 'NONE',  ( 7.361572987183169658, 9.967264484334119601, -9.846743663894592657 ) ) ;
#17043 = CARTESIAN_POINT ( 'NONE',  ( 4.559911319644449179, 68.89701867748817676, 9.422509992056141925 ) ) ;
#17045 = EDGE_CURVE ( 'NONE', #78351, #42731, #86368, .T. ) ;
#17044 = CARTESIAN_POINT ( 'NONE',  ( -46.34323875807881166, 103.6109741468810483, 6.190393423093146552 ) ) ;
#17046 = CARTESIAN_POINT ( 'NONE',  ( 12.63842701281683034, 7.467264484334118713, 9.846743663894596210 ) ) ;
#17047 = CARTESIAN_POINT ( 'NONE',  ( 12.91533473730992121, 64.52201867748817676, 10.88017736071110164 ) ) ;
#17048 =( NAMED_UNIT ( * ) SI_UNIT ( $, .STERADIAN. ) SOLID_ANGLE_UNIT ( ) );
#17049 = EDGE_CURVE ( 'NONE', #89452, #59664, #63354, .T. ) ;
#17050 = CARTESIAN_POINT ( 'NONE',  ( 20.88017736071110875, 60.77201867748817676, -2.915334737309920765 ) ) ;
#17052 = ORIENTED_EDGE ( 'NONE', *, *, #65798, .T. ) ;
#17051 = CARTESIAN_POINT ( 'NONE',  ( 14.92337183194729633, 7.675597817667451750, 8.527530157486181039 ) ) ;
#17053 = TOROIDAL_SURFACE ( 'NONE', #1074, 14.49999999999999822, 0.5000000000000000000 ) ;
#17054 = TOROIDAL_SURFACE ( 'NONE', #96857, 14.49999999999999822, 0.5000000000000000000 ) ;
#17055 = CARTESIAN_POINT ( 'NONE',  ( 14.92337183194729988, 49.34226448433411605, -8.527530157486177487 ) ) ;
#17056 = ORIENTED_EDGE ( 'NONE', *, *, #65475, .T. ) ;
#17057 = EDGE_LOOP ( 'NONE', ( #80966, #98877, #39779, #1270, #91553 ) ) ;
#17058 = CARTESIAN_POINT ( 'NONE',  ( 4.630000000000003446, 1.019547802438464323, -3.750000000000000000 ) ) ;
#17059 = CARTESIAN_POINT ( 'NONE',  ( 10.00000000000000000, 0.5537488349139675359, -14.16423886937410082 ) ) ;
#17060 = CARTESIAN_POINT ( 'NONE',  ( 3.591859063236761518, 54.95696800326376064, 11.09922568453594849 ) ) ;
#17061 = CARTESIAN_POINT ( 'NONE',  ( -0.3689425029237881626, 2.428748834913967869, 10.36894250292379027 ) ) ;
#17062 = CARTESIAN_POINT ( 'NONE',  ( 10.00000000000000178, 13.05374883491396787, 14.16423886937410082 ) ) ;
#17063 = CARTESIAN_POINT ( 'NONE',  ( 3.115783986955559470, 4.823715477197806954E-16, -14.16128137375397777 ) ) ;
#17065 = CARTESIAN_POINT ( 'NONE',  ( -0.8801773607111008646, 58.27201867748816966, 2.915334737309923430 ) ) ;
#17064 = CARTESIAN_POINT ( 'NONE',  ( 20.20021275402702443, 69.97534054108130874, 6.181800700215005939 ) ) ;
#17066 = CARTESIAN_POINT ( 'NONE',  ( 7.084665262690076126, 24.10535201082150181, 10.88017736071109987 ) ) ;
#17067 = ORIENTED_EDGE ( 'NONE', *, *, #33608, .F. ) ;
#17068 = CARTESIAN_POINT ( 'NONE',  ( 17.20831665107776587, 7.883931151000784787, 7.208316651077764980 ) ) ;
#17069 = CARTESIAN_POINT ( 'NONE',  ( 10.00000000000000000, 4.758931151000784787, -9.846743663894594434 ) ) ;
#17070 = CARTESIAN_POINT ( 'NONE',  ( 21.09922568453594849, 31.20696800326375353, 6.408140936763242479 ) ) ;
#17071 = CARTESIAN_POINT ( 'NONE',  ( 14.92337183194729633, 37.67559781766745175, 8.527530157486181039 ) ) ;
#17072 = DIRECTION ( 'NONE',  ( -0.000000000000000000, 0.000000000000000000, 1.000000000000000000 ) ) ;
#17073 = CARTESIAN_POINT ( 'NONE',  ( 0.6178305044545818747, 18.49863466993041428, -9.382169495545419124 ) ) ;
#17074 = CARTESIAN_POINT ( 'NONE',  ( -13.21236992757677164, 0.000000000000000000, 5.338143956176621074 ) ) ;
#17075 = AXIS2_PLACEMENT_3D ( 'NONE', #39174, #1190, #31649 ) ;
#17076 = CARTESIAN_POINT ( 'NONE',  ( 17.20831665107776587, 22.88393115100078745, 7.208316651077764980 ) ) ;
#17077 = EDGE_CURVE ( 'NONE', #92463, #28728, #94347, .T. ) ;
#17078 = CARTESIAN_POINT ( 'NONE',  ( 17.20831665107776587, 4.133931151000785675, -7.208316651077762316 ) ) ;
#17079 = VERTEX_POINT ( 'NONE', #10370 ) ;
#17080 = VERTEX_POINT ( 'NONE', #40871 ) ;
#17081 = EDGE_CURVE ( 'NONE', #46987, #5600, #71376, .T. ) ;
#17082 = VECTOR ( 'NONE', #34407, 1000.000000000000000 ) ;
#17083 = CARTESIAN_POINT ( 'NONE',  ( 2.035157376598822676, 42.43868534415483396, -7.964842623401177768 ) ) ;
#17084 = CARTESIAN_POINT ( 'NONE',  ( -4.164238869374098151, 26.59541550158063217, -3.795296366450310543 ) ) ;
#17085 = CARTESIAN_POINT ( 'NONE',  ( 17.20831665107776587, 44.13393115100078745, -7.208316651077762316 ) ) ;
#17086 = CARTESIAN_POINT ( 'NONE',  ( 10.00000000000000178, 17.25893115100078745, 9.846743663894594434 ) ) ;
#17088 = CARTESIAN_POINT ( 'NONE',  ( 0.000000000000000000, 0.5000000000000004441, 0.000000000000000000 ) ) ;
#17087 = CARTESIAN_POINT ( 'NONE',  ( -2.816281873526473856, 49.33196800326374643, 3.434112377981055619 ) ) ;
#17089 = CARTESIAN_POINT ( 'NONE',  ( 0.5774900079438590739, 27.64701867748817676, -5.440088680355550821 ) ) ;
#17090 = LINE ( 'NONE', #1107, #54992 ) ;
#17091 = CARTESIAN_POINT ( 'NONE',  ( 13.43411237798106583, 27.66530133659708568, -12.81628187352647252 ) ) ;
#17092 = CARTESIAN_POINT ( 'NONE',  ( 0.1532563361054100626, 40.80059781766745886, -2.638427012816831230 ) ) ;
#17093 = CARTESIAN_POINT ( 'NONE',  ( 7.964842623401177768, 6.188685344154841061, -7.964842623401181321 ) ) ;
#17094 = CARTESIAN_POINT ( 'NONE',  ( 16.40814093676323893, 45.79030133659708923, 11.09922568453595026 ) ) ;
#17095 = CARTESIAN_POINT ( 'NONE',  ( 4.850115630859686888, 14.95077488074853456, -13.93278430610806495 ) ) ;
#17097 = DIRECTION ( 'NONE',  ( -1.000000000000000000, 0.000000000000000000, 0.000000000000000000 ) ) ;
#17096 = CARTESIAN_POINT ( 'NONE',  ( 19.42250999205614548, 50.98035201082151247, -5.440088680355545492 ) ) ;
#17098 = CARTESIAN_POINT ( 'NONE',  ( -11.23896940083325013, -88.22260584720305587, 4.000000000000000000 ) ) ;
#17099 = FACE_OUTER_BOUND ( 'NONE', #98057, .T. ) ;
#17100 = CARTESIAN_POINT ( 'NONE',  ( 4.559911319644449179, 48.89701867748817676, 9.422509992056141925 ) ) ;
#17101 = CARTESIAN_POINT ( 'NONE',  ( 2.035157376598824452, 53.68868534415484817, 7.964842623401179544 ) ) ;
#17102 = DIRECTION ( 'NONE',  ( 0.000000000000000000, 0.000000000000000000, -1.000000000000000000 ) ) ;
#17103 = DIRECTION ( 'NONE',  ( -0.9961946980917462113, 0.08715574274765140739, -0.000000000000000000 ) ) ;
#17104 = EDGE_CURVE ( 'NONE', #39677, #68278, #52069, .T. ) ;
#17105 = AXIS2_PLACEMENT_3D ( 'NONE', #58093, #58598, #27606 ) ;
#17106 = CARTESIAN_POINT ( 'NONE',  ( 4.559911319644449179, 3.897018677488171434, 9.422509992056141925 ) ) ;
#17107 = CARTESIAN_POINT ( 'NONE',  ( 1.472469842513823179, 61.42559781766745175, 4.923371831947296329 ) ) ;
#17109 = CARTESIAN_POINT ( 'NONE',  ( 18.04007052943773459, 24.00257860105348939, -5.767676674365828760 ) ) ;
#17108 = CARTESIAN_POINT ( 'NONE',  ( 17.96484262340118221, 24.93868534415484461, 7.964842623401181321 ) ) ;
#17110 = CARTESIAN_POINT ( 'NONE',  ( 21.92686044187656691, 52.18830936912750929, 4.562052436263911564E-16 ) ) ;
#17111 = CARTESIAN_POINT ( 'NONE',  ( -2.816281873526473856, 24.33196800326375353, 3.434112377981055619 ) ) ;
#17112 = ORIENTED_EDGE ( 'NONE', *, *, #81084, .F. ) ;
#17113 = CARTESIAN_POINT ( 'NONE',  ( 12.91533473730992121, 34.52201867748817676, 10.88017736071110164 ) ) ;
#17114 = CARTESIAN_POINT ( 'NONE',  ( 1.472469842513823179, 41.42559781766745886, 4.923371831947296329 ) ) ;
#17116 = LINE ( 'NONE', #86585, #70175 ) ;
#17115 = CARTESIAN_POINT ( 'NONE',  ( -1.099225684535947600, 4.540301336597087456, 6.408140936763237150 ) ) ;
#17117 = EDGE_CURVE ( 'NONE', #35522, #46963, #29704, .T. ) ;
#17118 = CARTESIAN_POINT ( 'NONE',  ( 0.5774900079438590739, 12.64701867748817143, -5.440088680355550821 ) ) ;
#17119 = CARTESIAN_POINT ( 'NONE',  ( 10.00000000000000000, 41.81368534415484106, -10.88017736071110342 ) ) ;
#17120 = CARTESIAN_POINT ( 'NONE',  ( 24.16423886937410614, 49.30374883491396787, 8.672049930838204340E-16 ) ) ;
#17121 = CARTESIAN_POINT ( 'NONE',  ( 12.63842701281683034, 42.46726448433412315, 9.846743663894596210 ) ) ;
#17122 = CARTESIAN_POINT ( 'NONE',  ( 20.88017736071110875, 60.77201867748817676, -2.915334737309920765 ) ) ;
#17123 = CARTESIAN_POINT ( 'NONE',  ( 19.50000000000000355, 70.00000000000000000, -4.500000000000001776 ) ) ;
#17124 = CARTESIAN_POINT ( 'NONE',  ( 6.204703633549690345, 15.76208216824730179, -14.16423886937410259 ) ) ;
#17125 = AXIS2_PLACEMENT_3D ( 'NONE', #41535, #33987, #47539 ) ;
#17126 = UNCERTAINTY_MEASURE_WITH_UNIT (LENGTH_MEASURE( 1.000000000000000082E-05 ), #1365, 'distance_accuracy_value', 'NONE');
#17127 = DIRECTION ( 'NONE',  ( 1.000000000000000000, 0.000000000000000000, 0.000000000000000000 ) ) ;
#17128 = CIRCLE ( 'NONE', #21912, 3.000000000000000000 ) ;
#17129 = VERTEX_POINT ( 'NONE', #14186 ) ;
#17130 = ORIENTED_EDGE ( 'NONE', *, *, #2099, .F. ) ;
#17131 = CARTESIAN_POINT ( 'NONE',  ( 2.917880565312950480, 35.97041550158063217, -12.26659068614894821 ) ) ;
#17132 = CARTESIAN_POINT ( 'NONE',  ( 13.79529636645030344, 33.26208216824730357, 14.16423886937410614 ) ) ;
#17133 = CARTESIAN_POINT ( 'NONE',  ( 19.84674366389459266, 8.717264484334116048, -2.638427012816827677 ) ) ;
#17134 = CARTESIAN_POINT ( 'NONE',  ( 0.6178305044545838731, 19.74863466993042138, 9.382169495545420901 ) ) ;
#17135 = CARTESIAN_POINT ( 'NONE',  ( 1.472469842513823179, 60.59226448433412315, -4.923371831947296329 ) ) ;
#17136 = DIRECTION ( 'NONE',  ( -0.000000000000000000, 0.000000000000000000, 1.000000000000000000 ) ) ;
#17138 = CARTESIAN_POINT ( 'NONE',  ( 3.591859063236763294, 38.29030133659708923, -11.09922568453595026 ) ) ;
#17137 = CARTESIAN_POINT ( 'NONE',  ( 15.44008868035555260, 64.73035201082151957, 9.422509992056143702 ) ) ;
#17139 = CARTESIAN_POINT ( 'NONE',  ( 24.16423886937410614, 29.51208216824729647, -3.795296366450302550 ) ) ;
#17140 = CARTESIAN_POINT ( 'NONE',  ( 15.44008868035555260, 24.73035201082150891, 9.422509992056143702 ) ) ;
#17141 = CARTESIAN_POINT ( 'NONE',  ( -8.721827932831924812, 15.00000000000000178, 11.74045266257169473 ) ) ;
#17142 = CARTESIAN_POINT ( 'NONE',  ( 2.791683348922240793, 1.633931151000784565, 7.208316651077764092 ) ) ;
#17143 = B_SPLINE_CURVE_WITH_KNOTS ( 'NONE', 3,
 ( #22889, #83868, #7883, #38375, #68876, #26797 ),
 .UNSPECIFIED., .F., .F.,
 ( 4, 2, 4 ),
 ( 0.0002800225282622548998, 0.0006862279780598551935, 0.001092433427857455487 ),
 .UNSPECIFIED. ) ;
#17144 = CARTESIAN_POINT ( 'NONE',  ( -3.469446951953614189E-15, -15.24106884899921077, -9.846743663894594434 ) ) ;
#17145 = ORIENTED_EDGE ( 'NONE', *, *, #78846, .T. ) ;
#17146 = DIRECTION ( 'NONE',  ( 0.000000000000000000, 0.000000000000000000, -1.000000000000000000 ) ) ;
#17147 = CARTESIAN_POINT ( 'NONE',  ( -0.1503990784575282014, 42.22266099184918886, -6.262539305110077947 ) ) ;
#17148 = ORIENTED_EDGE ( 'NONE', *, *, #95568, .F. ) ;
#17149 = PRODUCT_DEFINITION_SHAPE ( 'NONE', 'NONE',  #98991 ) ;
#17151 = CARTESIAN_POINT ( 'NONE',  ( 20.88017736071110519, 10.56368534415483929, 2.639326808657452039E-16 ) ) ;
#17150 = CARTESIAN_POINT ( 'NONE',  ( 7.084665262690076126, 7.022018677488170546, -10.88017736071110164 ) ) ;
#17153 = CARTESIAN_POINT ( 'NONE',  ( 0.6178305044545818747, 8.498634669930421381, -9.382169495545419124 ) ) ;
#17152 = CARTESIAN_POINT ( 'NONE',  ( 0.1532563361054100626, 35.80059781766745175, -2.638427012816831230 ) ) ;
#17154 = FACE_OUTER_BOUND ( 'NONE', #84879, .T. ) ;
#17155 = CARTESIAN_POINT ( 'NONE',  ( 20.15039907845753930, 1.748846992468885198, 6.262539305110068177 ) ) ;
#17156 = CARTESIAN_POINT ( 'NONE',  ( 13.43411237798105340, 0.5819680032637533085, 12.81628187352647963 ) ) ;
#17157 = AXIS2_PLACEMENT_3D ( 'NONE', #60371, #82885, #58898 ) ;
#17158 = ORIENTED_EDGE ( 'NONE', *, *, #21840, .F. ) ;
#17159 = CARTESIAN_POINT ( 'NONE',  ( 13.79529636645030344, 43.26208216824730357, 14.16423886937410614 ) ) ;
#17160 = ORIENTED_EDGE ( 'NONE', *, *, #54038, .T. ) ;
#17161 = CARTESIAN_POINT ( 'NONE',  ( -0.3689425029237881626, 62.42874883491396787, 10.36894250292379027 ) ) ;
#17162 = VERTEX_POINT ( 'NONE', #67178 ) ;
#17163 = CARTESIAN_POINT ( 'NONE',  ( 19.42250999205614548, 25.98035201082150891, -5.440088680355545492 ) ) ;
#17164 = CARTESIAN_POINT ( 'NONE',  ( 20.88017736071110875, 35.77201867748816966, -2.915334737309920765 ) ) ;
#17165 = CARTESIAN_POINT ( 'NONE',  ( -5.419894505350674407, 0.5000000000000004441, 13.98659156302455031 ) ) ;
#17166 = CARTESIAN_POINT ( 'NONE',  ( 12.91533473730993009, 36.60535201082151247, -10.88017736071109987 ) ) ;
#17167 =( BOUNDED_SURFACE ( )  B_SPLINE_SURFACE ( 1, 2, ( 
 ( #3731, #4219, #13181, #74161, #42216, #34690, #66173, #96706, #87693, #35688, #87206, #18730, #34192, #65183, #20693, #50187, #95705, #27687, #80698, #50693, #42701, #5695, #49211, #27188, #28184, #72683, #57691, #49691, #51185, #65680, #88189, #79714, #64685, #57196, #81667, #12192, #81187, #96204, #35179, #11706, #72203, #58171, #12688, #58680, #43674, #11214, #41732, #98690, #52170, #36683, #68655, #60647, #184, #84163, #15668, #98187, #53151, #46153, #7675, #97696, #45152, #29160, #21185, #13676, #59663, #83657, #51685, #29645, #75657, #7168, #38168, #21685, #6669, #82664, #91649, #90154, #37188, #67172, #60152, #76637, #14180, #90649, #67678, #30632, #82163, #44663, #91146, #6180, #37671, #97206, #22672, #15174, #61141, #75158, #22175, #23167, #53645, #52656, #68171, #83159, #74670, #14683, #8156, #66681, #30139, #45655, #28674, #59167, #76151, #89673, #44160, #61623, #77129, #17632, #47115, #56115, #63595, #16642, #9127, #32105, #17144, #86121, #63106, #48594, #79098, #77615, #62604, #18122, #47622, #39643, #55107, #55623, #1161, #70136, #1656, #93112, #48103, #78118, #24145, #8638, #38648, #92141, #39148, #78616, #24639, #86612, #94101, #85627, #9626, #40125, #70625, #10125, #93609, #69153, #678, #2153, #32610, #31127, #25146, #40622, #71120, #2647, #31622, #33101, #25624, #23666, #54127, #84640, #54613, #69637, #16142, #46628, #62114, #92623, #85133, #42581, #65058, #4596, #57571, #89062, #3124, #11586, #50572, #57084, #19091, #3609, #66058, #80580, #49571, #64076, #79598, #11100, #96585, #87578, #65558, #12075, #19581, #18605, #87093, #72565, #34564, #27566, #49095, #95585, #4102, #73063, #95077, #41618, #12570, #35059, #43071, #28060, #58556, #42102, #96084, #20577, #81068, #72084, #88068, #34074, #94592, #56603, #64568, #58061, #26109, #27071, #50078, #88565, #73556, #26583, #80081, #20068, #35566, #5079, #51061, #10611, #41123, #71613, #33582, #6551, #52057, #22559, #36060, #29042, #75542, #21067, #60037, #13061, #7058, #30028, #76033, #13560, #59550, #38053, #83543, #44047, #52541, #37062, #89560, #90046, #77, #61025, #21568, #82550, #53028, #15066, #74550, #91029, #74049, #51564, #82049, #45536, #98578, #14067, #44548, #6067, #91537, #75043, #14566, #23053, #67560, #5584, #83047, #98071, #68544, #30524, #90533, #36567, #7566, #67055, #97581, #29531, #22067, #45033, #37560, #68050, #60536, #81552, #43553, #66561, #97090, #28560, #59055, #54994, #17023, #31990, #32986, #25024, #93992, #70512, #46517, #55509, #24534, #62496, #2036, #92021, #86009, #16532, #77499, #47500, #15556, #63489, #24035, #93000, #47008, #39032, #40513, #9011, #32497, #47988, #46042, #2532, #92505, #39527, #78003, #70021, #1545, #71010, #1042, #8532, #17521, #78498, #54022, #85512, #54505, #53524, #84036, #23552, #62995 ),
 ( #8042, #571, #16029, #93499, #38542, #85018, #9508, #40010, #10012, #69527, #76526, #31505, #69037, #84531, #31017, #77018, #61513, #62007, #94475, #49460, #94964, #65445, #78985, #71972, #19470, #63962, #3984, #56001, #49961, #72951, #19954, #56488, #3495, #80955, #27453, #86976, #95470, #79966, #11471, #56965, #87467, #25993, #80465, #42468, #18487, #41989, #86505, #4479, #73440, #57461, #11964, #18003, #87954, #3016, #18982, #33953, #72453, #33465, #79483, #57946, #48975, #10983, #95969, #34946, #64456, #34451, #41504, #4966, #64943, #88453, #65943, #26961, #48483, #50448, #26465, #12453, #35447, #42959, #25515, #10492, #41003, #71503, #28443, #81931, #5952, #66436, #44424, #6428, #43926, #7439, #98453, #59918, #81441, #89928, #97957, #90406, #74929, #75915, #67933, #37936, #14443, #89441, #29909, #67436, #36940, #44913, #35940, #60415, #59425, #21443, #21948, #58434, #96470, #66936, #29413, #51941, #13439, #83422, #82425, #75420, #90910, #88949, #45410, #36443, #13950, #52426, #82925, #6935, #14941, #74424, #51442, #22438, #52909, #96971, #37442, #97457, #27942, #20456, #58941, #50947, #12943, #20954, #28922, #43439, #73940, #5468, #10258, #40262, #9763, #94728, #40751, #7924, #25278, #87219, #30403, #49227, #70769, #79232, #55758, #32743, #79728, #71737, #60906, #71255, #45920, #17763, #98948, #63726, #18249, #64212, #1789, #47750, #26234, #3246, #32244, #2778, #93743, #76408, #78247, #18743, #11227, #17275, #2284, #41263, #33713, #62747, #10745, #91408, #22935, #39774, #48728, #63239, #68425, #56729, #86251, #48240, #78752, #33233, #53403, #94227, #83912, #15440, #25759, #56252, #70272, #86745, #93249, #24773, #55249, #85764, #50200, #73195, #65695, #58691, #20203, #27203, #11718, #41747, #12206, #66693, #96218, #80711, #73683, #27699, #35699, #88695, #21200, #34207, #42713, #81679, #88203, #4727, #34702, #97220, #12701, #35191, #95209, #42231, #72697, #28687, #19713, #96719, #43196, #50707, #49704, #19223, #58183, #81200, #89194, #80212, #5219, #66184, #28195, #57703, #4232, #43688, #20705, #74174, #59180, #89684, #51198, #13194, #51698, #5707, #65196, #36195, #95718, #26715, #87708, #82180, #72216, #57211, #3747, #64697, #53167, #84176, #67692, #52672, #29661, #38664, #44678, #83174, #14197, #45169, #92155, #82678, #37688, #14699, #53659, #67188, #60170, #7687, #52184, #91161, #68185, #75671, #45670, #98204, #75173, #15683, #38185, #46168, #31145, #61635, #7184, #198, #23680, #76652, #6683, #22687, #37201, #97712, #59677, #90666, #30648, #29177, #98706, #83672, #15187, #8172, #22193, #30156, #60660, #69168, #76167, #68671, #61156, #91665, #54144, #23182, #691, #13691, #44175, #90168, #74684, #6196, #36700, #21700, #16161, #78632, #33113, #79114, #16655, #62618, #41139, #86625, #47129, #55635, #9642 ) ),
 .UNSPECIFIED., .F., .F., .F. ) 
 B_SPLINE_SURFACE_WITH_KNOTS ( ( 2, 2 ),
 ( 3, 2, 2, 2, 2, 2, 2, 2, 2, 2, 2, 2, 2, 2, 2, 2, 2, 2, 2, 2, 2, 2, 2, 2, 2, 2, 2, 2, 2, 2, 2, 2, 2, 2, 2, 2, 2, 2, 2, 2, 2, 2, 2, 2, 2, 2, 2, 2, 2, 2, 2, 2, 2, 2, 2, 2, 2, 2, 2, 2, 2, 2, 2, 2, 2, 2, 2, 2, 2, 2, 2, 2, 2, 2, 2, 2, 2, 2, 2, 2, 2, 2, 2, 2, 2, 2, 2, 2, 2, 2, 2, 2, 2, 2, 2, 2, 2, 2, 2, 2, 2, 2, 2, 2, 2, 2, 2, 2, 2, 2, 2, 2, 2, 2, 2, 2, 2, 2, 2, 2, 2, 2, 2, 2, 2, 2, 2, 2, 2, 2, 2, 2, 2, 2, 2, 2, 2, 2, 2, 2, 2, 2, 2, 2, 2, 2, 2, 2, 2, 2, 2, 2, 2, 2, 2, 2, 2, 2, 2, 2, 2, 2, 2, 2, 2, 2, 2, 2, 2, 2, 2, 2, 2, 2, 3 ),
 ( 0.000000000000000000, 1.000000000000000000 ),
 ( 0.000000000000000000, 0.005555555555555555768, 0.01111111111111111154, 0.01666666666666666644, 0.02222222222222222307, 0.02777777777777777624, 0.03333333333333333287, 0.03888888888888888951, 0.04444444444444444614, 0.05000000000000000278, 0.05555555555555555247, 0.06111111111111110911, 0.06666666666666666574, 0.07222222222222221544, 0.07777777777777777901, 0.08333333333333332871, 0.08888888888888889228, 0.09444444444444444198, 0.1000000000000000056, 0.1055555555555555552, 0.1111111111111111049, 0.1166666666666666685, 0.1222222222222222182, 0.1277777777777777679, 0.1333333333333333315, 0.1388888888888888951, 0.1444444444444444309, 0.1499999999999999944, 0.1555555555555555580, 0.1611111111111111216, 0.1666666666666666574, 0.1722222222222222210, 0.1777777777777777846, 0.1833333333333333204, 0.1888888888888888840, 0.1944444444444444475, 0.2000000000000000111, 0.2055555555555555469, 0.2111111111111111105, 0.2166666666666666741, 0.2222222222222222099, 0.2277777777777777735, 0.2333333333333333370, 0.2388888888888889006, 0.2444444444444444364, 0.2500000000000000000, 0.2555555555555555358, 0.2611111111111111271, 0.2666666666666666630, 0.2722222222222221988, 0.2777777777777777901, 0.2833333333333333259, 0.2888888888888888618, 0.2944444444444444531, 0.2999999999999999889, 0.3055555555555555802, 0.3111111111111111160, 0.3166666666666666519, 0.3222222222222222432, 0.3277777777777777790, 0.3333333333333333148, 0.3388888888888889062, 0.3444444444444444420, 0.3499999999999999778, 0.3555555555555555691, 0.3611111111111111049, 0.3666666666666666408, 0.3722222222222222321, 0.3777777777777777679, 0.3833333333333333592, 0.3888888888888888951, 0.3944444444444444309, 0.4000000000000000222, 0.4055555555555555580, 0.4111111111111110938, 0.4166666666666666852, 0.4222222222222222210, 0.4277777777777777568, 0.4333333333333333481, 0.4388888888888888840, 0.4444444444444444198, 0.4500000000000000111, 0.4555555555555555469, 0.4611111111111111382, 0.4666666666666666741, 0.4722222222222222099, 0.4777777777777778012, 0.4833333333333333370, 0.4888888888888888729, 0.4944444444444444642, 0.5000000000000000000, 0.5055555555555555358, 0.5111111111111110716, 0.5166666666666667185, 0.5222222222222222543, 0.5277777777777777901, 0.5333333333333333259, 0.5388888888888888618, 0.5444444444444443976, 0.5500000000000000444, 0.5555555555555555802, 0.5611111111111111160, 0.5666666666666666519, 0.5722222222222221877, 0.5777777777777777235, 0.5833333333333333703, 0.5888888888888889062, 0.5944444444444444420, 0.5999999999999999778, 0.6055555555555555136, 0.6111111111111111605, 0.6166666666666666963, 0.6222222222222222321, 0.6277777777777777679, 0.6333333333333333037, 0.6388888888888888395, 0.6444444444444444864, 0.6500000000000000222, 0.6555555555555555580, 0.6611111111111110938, 0.6666666666666666297, 0.6722222222222222765, 0.6777777777777778123, 0.6833333333333333481, 0.6888888888888888840, 0.6944444444444444198, 0.6999999999999999556, 0.7055555555555556024, 0.7111111111111111382, 0.7166666666666666741, 0.7222222222222222099, 0.7277777777777777457, 0.7333333333333332815, 0.7388888888888889284, 0.7444444444444444642, 0.7500000000000000000, 0.7555555555555555358, 0.7611111111111110716, 0.7666666666666667185, 0.7722222222222222543, 0.7777777777777777901, 0.7833333333333333259, 0.7888888888888888618, 0.7944444444444443976, 0.8000000000000000444, 0.8055555555555555802, 0.8111111111111111160, 0.8166666666666666519, 0.8222222222222221877, 0.8277777777777777235, 0.8333333333333333703, 0.8388888888888889062, 0.8444444444444444420, 0.8499999999999999778, 0.8555555555555555136, 0.8611111111111111605, 0.8666666666666666963, 0.8722222222222222321, 0.8777777777777777679, 0.8833333333333333037, 0.8888888888888888395, 0.8944444444444444864, 0.9000000000000000222, 0.9055555555555555580, 0.9111111111111110938, 0.9166666666666666297, 0.9222222222222222765, 0.9277777777777778123, 0.9333333333333333481, 0.9388888888888888840, 0.9444444444444444198, 0.9499999999999999556, 0.9555555555555556024, 0.9611111111111111382, 0.9666666666666666741 ),
 .UNSPECIFIED. ) 
 GEOMETRIC_REPRESENTATION_ITEM ( )  RATIONAL_B_SPLINE_SURFACE ( (
 ( 1.000000000000000000, 0.9659258262890683122, 1.000000000000000000, 0.9659258262890683122, 1.000000000000000000, 0.9659258262890683122, 1.000000000000000000, 0.9659258262890683122, 1.000000000000000000, 0.9659258262890683122, 1.000000000000000000, 0.9659258262890683122, 1.000000000000000000, 0.9659258262890683122, 1.000000000000000000, 0.9659258262890683122, 1.000000000000000000, 0.9659258262890683122, 1.000000000000000000, 0.9659258262890683122, 1.000000000000000000, 0.9659258262890683122, 1.000000000000000000, 0.9659258262890683122, 1.000000000000000000, 0.9659258262890683122, 1.000000000000000000, 0.9659258262890683122, 1.000000000000000000, 0.9659258262890683122, 1.000000000000000000, 0.9659258262890683122, 1.000000000000000000, 0.9659258262890683122, 1.000000000000000000, 0.9659258262890683122, 1.000000000000000000, 0.9659258262890683122, 1.000000000000000000, 0.9659258262890683122, 1.000000000000000000, 0.9659258262890683122, 1.000000000000000000, 0.9659258262890683122, 1.000000000000000000, 0.9659258262890683122, 1.000000000000000000, 0.9659258262890683122, 1.000000000000000000, 0.9659258262890683122, 1.000000000000000000, 0.9659258262890683122, 1.000000000000000000, 0.9659258262890683122, 1.000000000000000000, 0.9659258262890683122, 1.000000000000000000, 0.9659258262890683122, 1.000000000000000000, 0.9659258262890683122, 1.000000000000000000, 0.9659258262890683122, 1.000000000000000000, 0.9659258262890683122, 1.000000000000000000, 0.9659258262890683122, 1.000000000000000000, 0.9659258262890683122, 1.000000000000000000, 0.9659258262890683122, 1.000000000000000000, 0.9659258262890683122, 1.000000000000000000, 0.9659258262890683122, 1.000000000000000000, 0.9659258262890683122, 1.000000000000000000, 0.9659258262890683122, 1.000000000000000000, 0.9659258262890683122, 1.000000000000000000, 0.9659258262890683122, 1.000000000000000000, 0.9659258262890683122, 1.000000000000000000, 0.9659258262890683122, 1.000000000000000000, 0.9659258262890683122, 1.000000000000000000, 0.9659258262890683122, 1.000000000000000000, 0.9659258262890683122, 1.000000000000000000, 0.9659258262890683122, 1.000000000000000000, 0.9659258262890683122, 1.000000000000000000, 0.9659258262890683122, 1.000000000000000000, 0.9659258262890683122, 1.000000000000000000, 0.9659258262890683122, 1.000000000000000000, 0.9659258262890683122, 1.000000000000000000, 0.9659258262890683122, 1.000000000000000000, 0.9659258262890683122, 1.000000000000000000, 0.9659258262890683122, 1.000000000000000000, 0.9659258262890683122, 1.000000000000000000, 0.9659258262890683122, 1.000000000000000000, 0.9659258262890683122, 1.000000000000000000, 0.9659258262890683122, 1.000000000000000000, 0.9659258262890683122, 1.000000000000000000, 0.9659258262890683122, 1.000000000000000000, 0.9659258262890683122, 1.000000000000000000, 0.9659258262890683122, 1.000000000000000000, 0.9659258262890683122, 1.000000000000000000, 0.9659258262890683122, 1.000000000000000000, 0.9659258262890683122, 1.000000000000000000, 0.9659258262890683122, 1.000000000000000000, 0.9659258262890683122, 1.000000000000000000, 0.9659258262890683122, 1.000000000000000000, 0.9659258262890683122, 1.000000000000000000, 0.9659258262890683122, 1.000000000000000000, 0.9659258262890683122, 1.000000000000000000, 0.9659258262890683122, 1.000000000000000000, 0.9659258262890683122, 1.000000000000000000, 0.9659258262890683122, 1.000000000000000000, 0.9659258262890683122, 1.000000000000000000, 0.9659258262890683122, 1.000000000000000000, 0.9659258262890683122, 1.000000000000000000, 0.9659258262890683122, 1.000000000000000000, 0.9659258262890683122, 1.000000000000000000, 0.9659258262890683122, 1.000000000000000000, 0.9659258262890683122, 1.000000000000000000, 0.9659258262890683122, 1.000000000000000000, 0.9659258262890683122, 1.000000000000000000, 0.9659258262890683122, 1.000000000000000000, 0.9659258262890683122, 1.000000000000000000, 0.9659258262890683122, 1.000000000000000000, 0.9659258262890683122, 1.000000000000000000, 0.9659258262890683122, 1.000000000000000000, 0.9659258262890683122, 1.000000000000000000, 0.9659258262890683122, 1.000000000000000000, 0.9659258262890683122, 1.000000000000000000, 0.9659258262890683122, 1.000000000000000000, 0.9659258262890683122, 1.000000000000000000, 0.9659258262890683122, 1.000000000000000000, 0.9659258262890683122, 1.000000000000000000, 0.9659258262890683122, 1.000000000000000000, 0.9659258262890683122, 1.000000000000000000, 0.9659258262890683122, 1.000000000000000000, 0.9659258262890683122, 1.000000000000000000, 0.9659258262890683122, 1.000000000000000000, 0.9659258262890683122, 1.000000000000000000, 0.9659258262890683122, 1.000000000000000000, 0.9659258262890683122, 1.000000000000000000, 0.9659258262890683122, 1.000000000000000000, 0.9659258262890683122, 1.000000000000000000, 0.9659258262890683122, 1.000000000000000000, 0.9659258262890683122, 1.000000000000000000, 0.9659258262890683122, 1.000000000000000000, 0.9659258262890683122, 1.000000000000000000, 0.9659258262890683122, 1.000000000000000000, 0.9659258262890683122, 1.000000000000000000, 0.9659258262890683122, 1.000000000000000000, 0.9659258262890683122, 1.000000000000000000, 0.9659258262890683122, 1.000000000000000000, 0.9659258262890683122, 1.000000000000000000, 0.9659258262890683122, 1.000000000000000000, 0.9659258262890683122, 1.000000000000000000, 0.9659258262890683122, 1.000000000000000000, 0.9659258262890683122, 1.000000000000000000, 0.9659258262890683122, 1.000000000000000000, 0.9659258262890683122, 1.000000000000000000, 0.9659258262890683122, 1.000000000000000000, 0.9659258262890683122, 1.000000000000000000, 0.9659258262890683122, 1.000000000000000000, 0.9659258262890683122, 1.000000000000000000, 0.9659258262890683122, 1.000000000000000000, 0.9659258262890683122, 1.000000000000000000, 0.9659258262890683122, 1.000000000000000000, 0.9659258262890683122, 1.000000000000000000, 0.9659258262890683122, 1.000000000000000000, 0.9659258262890683122, 1.000000000000000000, 0.9659258262890683122, 1.000000000000000000, 0.9659258262890683122, 1.000000000000000000, 0.9659258262890683122, 1.000000000000000000, 0.9659258262890683122, 1.000000000000000000, 0.9659258262890683122, 1.000000000000000000, 0.9659258262890683122, 1.000000000000000000, 0.9659258262890683122, 1.000000000000000000, 0.9659258262890683122, 1.000000000000000000, 0.9659258262890683122, 1.000000000000000000, 0.9659258262890683122, 1.000000000000000000, 0.9659258262890683122, 1.000000000000000000, 0.9659258262890683122, 1.000000000000000000, 0.9659258262890683122, 1.000000000000000000, 0.9659258262890683122, 1.000000000000000000, 0.9659258262890683122, 1.000000000000000000, 0.9659258262890683122, 1.000000000000000000, 0.9659258262890683122, 1.000000000000000000, 0.9659258262890683122, 1.000000000000000000, 0.9659258262890683122, 1.000000000000000000, 0.9659258262890683122, 1.000000000000000000, 0.9659258262890683122, 1.000000000000000000, 0.9659258262890683122, 1.000000000000000000, 0.9659258262890683122, 1.000000000000000000, 0.9659258262890683122, 1.000000000000000000, 0.9659258262890683122, 1.000000000000000000, 0.9659258262890683122, 1.000000000000000000, 0.9659258262890683122, 1.000000000000000000, 0.9659258262890683122, 1.000000000000000000, 0.9659258262890683122, 1.000000000000000000, 0.9659258262890683122, 1.000000000000000000, 0.9659258262890683122, 1.000000000000000000, 0.9659258262890683122, 1.000000000000000000, 0.9659258262890683122, 1.000000000000000000, 0.9659258262890683122, 1.000000000000000000, 0.9659258262890683122, 1.000000000000000000, 0.9659258262890683122, 1.000000000000000000, 0.9659258262890683122, 1.000000000000000000, 0.9659258262890683122, 1.000000000000000000, 0.9659258262890683122, 1.000000000000000000, 0.9659258262890683122, 1.000000000000000000, 0.9659258262890683122, 1.000000000000000000, 0.9659258262890683122, 1.000000000000000000),
 ( 1.000000000000000000, 0.9659258262890683122, 1.000000000000000000, 0.9659258262890683122, 1.000000000000000000, 0.9659258262890683122, 1.000000000000000000, 0.9659258262890683122, 1.000000000000000000, 0.9659258262890683122, 1.000000000000000000, 0.9659258262890683122, 1.000000000000000000, 0.9659258262890683122, 1.000000000000000000, 0.9659258262890683122, 1.000000000000000000, 0.9659258262890683122, 1.000000000000000000, 0.9659258262890683122, 1.000000000000000000, 0.9659258262890683122, 1.000000000000000000, 0.9659258262890683122, 1.000000000000000000, 0.9659258262890683122, 1.000000000000000000, 0.9659258262890683122, 1.000000000000000000, 0.9659258262890683122, 1.000000000000000000, 0.9659258262890683122, 1.000000000000000000, 0.9659258262890683122, 1.000000000000000000, 0.9659258262890683122, 1.000000000000000000, 0.9659258262890683122, 1.000000000000000000, 0.9659258262890683122, 1.000000000000000000, 0.9659258262890683122, 1.000000000000000000, 0.9659258262890683122, 1.000000000000000000, 0.9659258262890683122, 1.000000000000000000, 0.9659258262890683122, 1.000000000000000000, 0.9659258262890683122, 1.000000000000000000, 0.9659258262890683122, 1.000000000000000000, 0.9659258262890683122, 1.000000000000000000, 0.9659258262890683122, 1.000000000000000000, 0.9659258262890683122, 1.000000000000000000, 0.9659258262890683122, 1.000000000000000000, 0.9659258262890683122, 1.000000000000000000, 0.9659258262890683122, 1.000000000000000000, 0.9659258262890683122, 1.000000000000000000, 0.9659258262890683122, 1.000000000000000000, 0.9659258262890683122, 1.000000000000000000, 0.9659258262890683122, 1.000000000000000000, 0.9659258262890683122, 1.000000000000000000, 0.9659258262890683122, 1.000000000000000000, 0.9659258262890683122, 1.000000000000000000, 0.9659258262890683122, 1.000000000000000000, 0.9659258262890683122, 1.000000000000000000, 0.9659258262890683122, 1.000000000000000000, 0.9659258262890683122, 1.000000000000000000, 0.9659258262890683122, 1.000000000000000000, 0.9659258262890683122, 1.000000000000000000, 0.9659258262890683122, 1.000000000000000000, 0.9659258262890683122, 1.000000000000000000, 0.9659258262890683122, 1.000000000000000000, 0.9659258262890683122, 1.000000000000000000, 0.9659258262890683122, 1.000000000000000000, 0.9659258262890683122, 1.000000000000000000, 0.9659258262890683122, 1.000000000000000000, 0.9659258262890683122, 1.000000000000000000, 0.9659258262890683122, 1.000000000000000000, 0.9659258262890683122, 1.000000000000000000, 0.9659258262890683122, 1.000000000000000000, 0.9659258262890683122, 1.000000000000000000, 0.9659258262890683122, 1.000000000000000000, 0.9659258262890683122, 1.000000000000000000, 0.9659258262890683122, 1.000000000000000000, 0.9659258262890683122, 1.000000000000000000, 0.9659258262890683122, 1.000000000000000000, 0.9659258262890683122, 1.000000000000000000, 0.9659258262890683122, 1.000000000000000000, 0.9659258262890683122, 1.000000000000000000, 0.9659258262890683122, 1.000000000000000000, 0.9659258262890683122, 1.000000000000000000, 0.9659258262890683122, 1.000000000000000000, 0.9659258262890683122, 1.000000000000000000, 0.9659258262890683122, 1.000000000000000000, 0.9659258262890683122, 1.000000000000000000, 0.9659258262890683122, 1.000000000000000000, 0.9659258262890683122, 1.000000000000000000, 0.9659258262890683122, 1.000000000000000000, 0.9659258262890683122, 1.000000000000000000, 0.9659258262890683122, 1.000000000000000000, 0.9659258262890683122, 1.000000000000000000, 0.9659258262890683122, 1.000000000000000000, 0.9659258262890683122, 1.000000000000000000, 0.9659258262890683122, 1.000000000000000000, 0.9659258262890683122, 1.000000000000000000, 0.9659258262890683122, 1.000000000000000000, 0.9659258262890683122, 1.000000000000000000, 0.9659258262890683122, 1.000000000000000000, 0.9659258262890683122, 1.000000000000000000, 0.9659258262890683122, 1.000000000000000000, 0.9659258262890683122, 1.000000000000000000, 0.9659258262890683122, 1.000000000000000000, 0.9659258262890683122, 1.000000000000000000, 0.9659258262890683122, 1.000000000000000000, 0.9659258262890683122, 1.000000000000000000, 0.9659258262890683122, 1.000000000000000000, 0.9659258262890683122, 1.000000000000000000, 0.9659258262890683122, 1.000000000000000000, 0.9659258262890683122, 1.000000000000000000, 0.9659258262890683122, 1.000000000000000000, 0.9659258262890683122, 1.000000000000000000, 0.9659258262890683122, 1.000000000000000000, 0.9659258262890683122, 1.000000000000000000, 0.9659258262890683122, 1.000000000000000000, 0.9659258262890683122, 1.000000000000000000, 0.9659258262890683122, 1.000000000000000000, 0.9659258262890683122, 1.000000000000000000, 0.9659258262890683122, 1.000000000000000000, 0.9659258262890683122, 1.000000000000000000, 0.9659258262890683122, 1.000000000000000000, 0.9659258262890683122, 1.000000000000000000, 0.9659258262890683122, 1.000000000000000000, 0.9659258262890683122, 1.000000000000000000, 0.9659258262890683122, 1.000000000000000000, 0.9659258262890683122, 1.000000000000000000, 0.9659258262890683122, 1.000000000000000000, 0.9659258262890683122, 1.000000000000000000, 0.9659258262890683122, 1.000000000000000000, 0.9659258262890683122, 1.000000000000000000, 0.9659258262890683122, 1.000000000000000000, 0.9659258262890683122, 1.000000000000000000, 0.9659258262890683122, 1.000000000000000000, 0.9659258262890683122, 1.000000000000000000, 0.9659258262890683122, 1.000000000000000000, 0.9659258262890683122, 1.000000000000000000, 0.9659258262890683122, 1.000000000000000000, 0.9659258262890683122, 1.000000000000000000, 0.9659258262890683122, 1.000000000000000000, 0.9659258262890683122, 1.000000000000000000, 0.9659258262890683122, 1.000000000000000000, 0.9659258262890683122, 1.000000000000000000, 0.9659258262890683122, 1.000000000000000000, 0.9659258262890683122, 1.000000000000000000, 0.9659258262890683122, 1.000000000000000000, 0.9659258262890683122, 1.000000000000000000, 0.9659258262890683122, 1.000000000000000000, 0.9659258262890683122, 1.000000000000000000, 0.9659258262890683122, 1.000000000000000000, 0.9659258262890683122, 1.000000000000000000, 0.9659258262890683122, 1.000000000000000000, 0.9659258262890683122, 1.000000000000000000, 0.9659258262890683122, 1.000000000000000000, 0.9659258262890683122, 1.000000000000000000, 0.9659258262890683122, 1.000000000000000000, 0.9659258262890683122, 1.000000000000000000, 0.9659258262890683122, 1.000000000000000000, 0.9659258262890683122, 1.000000000000000000, 0.9659258262890683122, 1.000000000000000000, 0.9659258262890683122, 1.000000000000000000, 0.9659258262890683122, 1.000000000000000000, 0.9659258262890683122, 1.000000000000000000, 0.9659258262890683122, 1.000000000000000000, 0.9659258262890683122, 1.000000000000000000, 0.9659258262890683122, 1.000000000000000000, 0.9659258262890683122, 1.000000000000000000, 0.9659258262890683122, 1.000000000000000000, 0.9659258262890683122, 1.000000000000000000, 0.9659258262890683122, 1.000000000000000000, 0.9659258262890683122, 1.000000000000000000, 0.9659258262890683122, 1.000000000000000000, 0.9659258262890683122, 1.000000000000000000, 0.9659258262890683122, 1.000000000000000000, 0.9659258262890683122, 1.000000000000000000, 0.9659258262890683122, 1.000000000000000000, 0.9659258262890683122, 1.000000000000000000, 0.9659258262890683122, 1.000000000000000000, 0.9659258262890683122, 1.000000000000000000, 0.9659258262890683122, 1.000000000000000000, 0.9659258262890683122, 1.000000000000000000, 0.9659258262890683122, 1.000000000000000000, 0.9659258262890683122, 1.000000000000000000, 0.9659258262890683122, 1.000000000000000000, 0.9659258262890683122, 1.000000000000000000, 0.9659258262890683122, 1.000000000000000000, 0.9659258262890683122, 1.000000000000000000, 0.9659258262890683122, 1.000000000000000000, 0.9659258262890683122, 1.000000000000000000, 0.9659258262890683122, 1.000000000000000000) ) ) 
 REPRESENTATION_ITEM ( '' )  SURFACE ( )  );
#17168 = CARTESIAN_POINT ( 'NONE',  ( 12.91533473730993009, 61.60535201082150536, -10.88017736071109987 ) ) ;
#17169 = CARTESIAN_POINT ( 'NONE',  ( 19.42250999205614193, 30.14701867748817321, 5.440088680355555262 ) ) ;
#17170 = EDGE_CURVE ( 'NONE', #70499, #63050, #37678, .T. ) ;
#17171 = CARTESIAN_POINT ( 'NONE',  ( -18.89999999999999147, 91.00000000000000000, 7.750000000000000000 ) ) ;
#17172 = CARTESIAN_POINT ( 'NONE',  ( 19.84674366389459266, 3.717264484334118713, -2.638427012816827677 ) ) ;
#17173 = CARTESIAN_POINT ( 'NONE',  ( -14.35840480524203144, 0.5000000000000004441, 4.340070442838751319 ) ) ;
#17174 = ORIENTED_EDGE ( 'NONE', *, *, #17906, .F. ) ;
#17175 = PLANE ( 'NONE',  #15833 ) ;
#17176 = CARTESIAN_POINT ( 'NONE',  ( 14.92337183194729633, 47.67559781766745175, 8.527530157486181039 ) ) ;
#17177 = DIRECTION ( 'NONE',  ( 0.000000000000000000, 0.000000000000000000, 1.000000000000000000 ) ) ;
#17178 = CARTESIAN_POINT ( 'NONE',  ( 22.81628187352647785, 46.62363466993041783, 6.195893100308588602E-16 ) ) ;
#17179 = FACE_OUTER_BOUND ( 'NONE', #98946, .T. ) ;
#17180 = DIRECTION ( 'NONE',  ( 0.3173046564050899243, -0.000000000000000000, 0.9483236552061999891 ) ) ;
#17181 = VECTOR ( 'NONE', #7082, 1000.000000000000000 ) ;
#17182 = ORIENTED_EDGE ( 'NONE', *, *, #67760, .T. ) ;
#17183 = DIRECTION ( 'NONE',  ( 2.107602052970794797E-16, -1.000000000000000000, 0.000000000000000000 ) ) ;
#17184 = CARTESIAN_POINT ( 'NONE',  ( -0.8801773607110990882, 52.85535201082151247, -2.915334737309924318 ) ) ;
#17185 = CARTESIAN_POINT ( 'NONE',  ( 10.00000000000000178, 52.25893115100078745, 9.846743663894594434 ) ) ;
#17186 = CARTESIAN_POINT ( 'NONE',  ( 22.26659068614894466, 53.88708216824731068, 7.082119434687054849 ) ) ;
#17187 = CARTESIAN_POINT ( 'NONE',  ( 18.52753015748618282, 63.92559781766745886, -4.923371831947291888 ) ) ;
#17188 = ORIENTED_EDGE ( 'NONE', *, *, #36018, .F. ) ;
#17189 = CARTESIAN_POINT ( 'NONE',  ( 10.00000000000000000, 19.75893115100078390, -9.846743663894594434 ) ) ;
#17190 = CIRCLE ( 'NONE', #98650, 15.00000000000000000 ) ;
#17191 = CARTESIAN_POINT ( 'NONE',  ( 22.81628187352647785, 46.41530133659708213, 3.434112377981063169 ) ) ;
#17192 = CARTESIAN_POINT ( 'NONE',  ( 19.84674366389459266, 63.30059781766745886, 2.638427012816836559 ) ) ;
#17193 = CARTESIAN_POINT ( 'NONE',  ( 2.035157376598822676, 62.43868534415483396, -7.964842623401177768 ) ) ;
#17194 = VECTOR ( 'NONE', #4386, 1000.000000000000000 ) ;
#17195 = AXIS2_PLACEMENT_3D ( 'NONE', #92977, #60514, #30994 ) ;
#17196 = CARTESIAN_POINT ( 'NONE',  ( 4.920090861807432603, -13.81657824355479036, -2.750000000000000000 ) ) ;
#17197 = EDGE_CURVE ( 'NONE', #4683, #78530, #44167, .T. ) ;
#17198 = ORIENTED_EDGE ( 'NONE', *, *, #80382, .F. ) ;
#17199 = EDGE_CURVE ( 'NONE', #63596, #33570, #53158, .T. ) ;
#17200 = CARTESIAN_POINT ( 'NONE',  ( -2.266590686148945544, 57.22041550158063217, 7.082119434687048631 ) ) ;
#17201 = FILL_AREA_STYLE ('',( #54671 ) ) ;
#17202 = CARTESIAN_POINT ( 'NONE',  ( 19.42250999205614193, 30.14701867748817321, 5.440088680355555262 ) ) ;
#17204 = CARTESIAN_POINT ( 'NONE',  ( 0.5774900079438590739, 52.64701867748817676, -5.440088680355550821 ) ) ;
#17203 = CARTESIAN_POINT ( 'NONE',  ( 3.591859063236763294, 13.29030133659708746, -11.09922568453595026 ) ) ;
#17205 = CARTESIAN_POINT ( 'NONE',  ( 18.72515096720591643, 66.07228050351029935, -6.499999999999699796 ) ) ;
#17206 = CARTESIAN_POINT ( 'NONE',  ( -0.4427729075171641382, 14.61885305295417048, 9.500000000000000000 ) ) ;
#17207 = DIRECTION ( 'NONE',  ( -0.9914448613738093830, 0.000000000000000000, -0.1305261922200583180 ) ) ;
#17208 = CARTESIAN_POINT ( 'NONE',  ( 5.817157072110704874, 0.5000000000000004441, 13.82608706751090821 ) ) ;
#17209 = CARTESIAN_POINT ( 'NONE',  ( 19.84674366389459266, 48.71726448433413026, -2.638427012816827677 ) ) ;
#17210 = CARTESIAN_POINT ( 'NONE',  ( 12.63842701281683034, 2.467264484334118269, 9.846743663894596210 ) ) ;
#17211 = CARTESIAN_POINT ( 'NONE',  ( 14.16423886937410082, 29.51208216824729291, -3.795296366450314096 ) ) ;
#17212 = CARTESIAN_POINT ( 'NONE',  ( 6.565887622018943937, 3.081968003263753531, -12.81628187352647608 ) ) ;
#17213 = CARTESIAN_POINT ( 'NONE',  ( 7.084665262690076126, 12.02201867748817321, -10.88017736071110164 ) ) ;
#17214 = DIRECTION ( 'NONE',  ( 1.000000000000000000, 0.000000000000000000, 0.000000000000000000 ) ) ;
#17215 = CARTESIAN_POINT ( 'NONE',  ( 2.917880565312948704, 42.63708216824729647, 12.26659068614894643 ) ) ;
#17216 = CARTESIAN_POINT ( 'NONE',  ( -2.266590686148945544, 36.38708216824730357, -7.082119434687050408 ) ) ;
#17217 = CARTESIAN_POINT ( 'NONE',  ( -0.3689425029237898834, 61.17874883491396076, -10.36894250292378850 ) ) ;
#17218 = CARTESIAN_POINT ( 'NONE',  ( 1.472469842513823179, 16.42559781766745175, 4.923371831947296329 ) ) ;
#17219 = CARTESIAN_POINT ( 'NONE',  ( 10.00000000000000000, 11.81368534415483751, -10.88017736071110342 ) ) ;
#17220 = ORIENTED_EDGE ( 'NONE', *, *, #2973, .T. ) ;
#17221 = CARTESIAN_POINT ( 'NONE',  ( 5.076628168052703671, 31.84226448433412315, 8.527530157486179263 ) ) ;
#17222 = CARTESIAN_POINT ( 'NONE',  ( 10.00000000000000178, 34.31368534415484106, 10.88017736071110342 ) ) ;
#17223 = CARTESIAN_POINT ( 'NONE',  ( 1.472469842513823179, 61.42559781766745175, 4.923371831947296329 ) ) ;
#17225 = CARTESIAN_POINT ( 'NONE',  ( -0.3289641300567998083, 18.07879003517447103, 5.963430220938281678 ) ) ;
#17224 = CARTESIAN_POINT ( 'NONE',  ( 22.26659068614895176, 24.72041550158063572, -7.082119434687042414 ) ) ;
#17226 = CARTESIAN_POINT ( 'NONE',  ( 9.972640495195376431, -0.03417435944610275333, -12.50695158660345818 ) ) ;
#17227 = UNCERTAINTY_MEASURE_WITH_UNIT (LENGTH_MEASURE( 1.000000000000000082E-05 ), #48315, 'distance_accuracy_value', 'NONE');
#17228 = CARTESIAN_POINT ( 'NONE',  ( 19.84674366389459266, 8.717264484334116048, -2.638427012816827677 ) ) ;
#17229 = CARTESIAN_POINT ( 'NONE',  ( 13.43411237798105340, 50.58196800326375353, 12.81628187352647963 ) ) ;
#17230 = CARTESIAN_POINT ( 'NONE',  ( 10.00000000000000000, 49.75893115100078745, -9.846743663894594434 ) ) ;
#17231 = VERTEX_POINT ( 'NONE', #97701 ) ;
#17232 = CARTESIAN_POINT ( 'NONE',  ( 8.900267061692415993, -1.043551099208791966, -4.000000000000000000 ) ) ;
#17233 = CARTESIAN_POINT ( 'NONE',  ( 20.88017736071110519, 5.563685344154838397, 2.639326808657452039E-16 ) ) ;
#17234 = CARTESIAN_POINT ( 'NONE',  ( -0.3689425029237881626, 17.42874883491397142, 10.36894250292379027 ) ) ;
#17235 = CARTESIAN_POINT ( 'NONE',  ( 4.559911319644449179, 67.23035201082150536, -9.422509992056141925 ) ) ;
#17236 = CARTESIAN_POINT ( 'NONE',  ( 19.84674366389459266, 43.30059781766744464, 2.638427012816836559 ) ) ;
#17237 = CARTESIAN_POINT ( 'NONE',  ( 20.88017736071110519, 15.56368534415483751, 2.639326808657452039E-16 ) ) ;
#17238 = CARTESIAN_POINT ( 'NONE',  ( 14.99999999999998046, 70.25000000000000000, -6.250000000000000000 ) ) ;
#17239 = CARTESIAN_POINT ( 'NONE',  ( 19.84674366389459621, 63.50893115100078745, 7.409399052514197653E-17 ) ) ;
#17240 = EDGE_CURVE ( 'NONE', #98676, #90778, #16025, .T. ) ;
#17241 = CARTESIAN_POINT ( 'NONE',  ( 7.361572987183170547, 2.050597817667451750, 9.846743663894590881 ) ) ;
#17242 = CIRCLE ( 'NONE', #15681, 0.2500000000000002220 ) ;
#17243 = CARTESIAN_POINT ( 'NONE',  ( 16.40814093676324603, 57.45696800326375353, -11.09922568453594671 ) ) ;
#17244 = ORIENTED_EDGE ( 'NONE', *, *, #92884, .F. ) ;
#17245 = VERTEX_POINT ( 'NONE', #88326 ) ;
#17246 = CARTESIAN_POINT ( 'NONE',  ( -5.817157072110618721, 15.00000000000000000, -13.82608706751094552 ) ) ;
#17247 = LINE ( 'NONE', #29881, #46316 ) ;
#17248 = CARTESIAN_POINT ( 'NONE',  ( 24.16423886937410614, 44.51208216824730357, -3.795296366450302550 ) ) ;
#17249 = CARTESIAN_POINT ( 'NONE',  ( 18.52753015748618282, 38.92559781766745175, -4.923371831947291888 ) ) ;
#17250 = CARTESIAN_POINT ( 'NONE',  ( 19.84674366389459266, 23.30059781766745530, 2.638427012816836559 ) ) ;
#17251 = CARTESIAN_POINT ( 'NONE',  ( -0.1503990784575280903, 38.10158574516643171, 6.262539305110076171 ) ) ;
#17253 = CARTESIAN_POINT ( 'NONE',  ( 1.472469842513823179, 56.42559781766745886, 4.923371831947296329 ) ) ;
#17252 = CARTESIAN_POINT ( 'NONE',  ( 7.084665262690076126, 24.10535201082150181, 10.88017736071109987 ) ) ;
#17254 = CARTESIAN_POINT ( 'NONE',  ( 0.000000000000000000, 0.5000000000000004441, 0.000000000000000000 ) ) ;
#17255 = CARTESIAN_POINT ( 'NONE',  ( 24.16423886937410614, 44.51208216824730357, -3.795296366450302550 ) ) ;
#17256 = CARTESIAN_POINT ( 'NONE',  ( 13.79529636645030344, 53.26208216824730357, 14.16423886937410614 ) ) ;
#17257 = CARTESIAN_POINT ( 'NONE',  ( -4.431036607602373500, 0.5000000000000004441, -14.33059365769916838 ) ) ;
#17258 = CARTESIAN_POINT ( 'NONE',  ( -11.75209714983963849, 14.95077488074851502, -8.918201205062176840 ) ) ;
#17259 = CARTESIAN_POINT ( 'NONE',  ( -0.8801773607111009756, 68.06368534415484817, 1.068504757029289695E-15 ) ) ;
#17260 = CARTESIAN_POINT ( 'NONE',  ( 19.84674366389459621, 13.50893115100078568, 7.409399052514197653E-17 ) ) ;
#17261 = CARTESIAN_POINT ( 'NONE',  ( -4.511928667084688094, -13.83795187542449412, 4.000000000000000000 ) ) ;
#17262 = VERTEX_POINT ( 'NONE', #75164 ) ;
#17263 = CARTESIAN_POINT ( 'NONE',  ( 20.24186590665277663, 29.73410085661204150, 6.114288769123037426 ) ) ;
#17264 = ORIENTED_EDGE ( 'NONE', *, *, #65835, .F. ) ;
#17265 = CARTESIAN_POINT ( 'NONE',  ( 0.1532563361054100626, 15.80059781766745353, -2.638427012816831230 ) ) ;
#17266 = ORIENTED_EDGE ( 'NONE', *, *, #57339, .T. ) ;
#17267 = CARTESIAN_POINT ( 'NONE',  ( 24.16423886937410614, 24.51208216824730002, -3.795296366450302550 ) ) ;
#17268 = CARTESIAN_POINT ( 'NONE',  ( 12.63842701281683922, 19.55059781766745175, -9.846743663894590881 ) ) ;
#17269 = CARTESIAN_POINT ( 'NONE',  ( -0.8801773607111009756, 38.06368534415484106, 1.068504757029289695E-15 ) ) ;
#17270 = VECTOR ( 'NONE', #50022, 1000.000000000000000 ) ;
#17271 = CARTESIAN_POINT ( 'NONE',  ( -11.96291822454869802, 15.00000000000000000, -8.193813980849247613 ) ) ;
#17272 = ORIENTED_EDGE ( 'NONE', *, *, #50576, .F. ) ;
#17273 = AXIS2_PLACEMENT_3D ( 'NONE', #26219, #4218, #71720 ) ;
#17274 = CARTESIAN_POINT ( 'NONE',  ( -0.8801773607110991993, 47.85535201082150536, -2.915334737309923874 ) ) ;
#17275 = CARTESIAN_POINT ( 'NONE',  ( 3.434112377981060948, -4.418031996736250022, 12.81628187352647430 ) ) ;
#17276 = ORIENTED_EDGE ( 'NONE', *, *, #21144, .T. ) ;
#17277 = CARTESIAN_POINT ( 'NONE',  ( 2.035157376598824452, 43.68868534415484106, 7.964842623401179544 ) ) ;
#17278 = CARTESIAN_POINT ( 'NONE',  ( 13.79529636645030344, 8.262082168247300018, 14.16423886937410614 ) ) ;
#17279 = ORIENTED_EDGE ( 'NONE', *, *, #34885, .T. ) ;
#17280 = ORIENTED_EDGE ( 'NONE', *, *, #54333, .T. ) ;
#17281 = CARTESIAN_POINT ( 'NONE',  ( 10.00000000000000000, 27.87363466993042138, -12.81628187352647608 ) ) ;
#17282 = CARTESIAN_POINT ( 'NONE',  ( 19.84674366389459621, 3.508931151000785231, 7.409399052514197653E-17 ) ) ;
#17283 = CARTESIAN_POINT ( 'NONE',  ( 10.00000000000000178, 45.37363466993041783, 12.81628187352647608 ) ) ;
#17284 = DIRECTION ( 'NONE',  ( 1.000000000000000000, -5.818595309480553908E-17, 0.000000000000000000 ) ) ;
#17285 = CARTESIAN_POINT ( 'NONE',  ( 19.84674366389459621, 28.50893115100078745, 7.409399052514197653E-17 ) ) ;
#17286 = CARTESIAN_POINT ( 'NONE',  ( 20.88017736071110519, 50.56368534415484106, 2.639326808657452039E-16 ) ) ;
#17287 = EDGE_CURVE ( 'NONE', #12526, #33705, #60654, .T. ) ;
#17288 = ORIENTED_EDGE ( 'NONE', *, *, #93247, .T. ) ;
#17289 = CARTESIAN_POINT ( 'NONE',  ( -6.382347221874545617, 14.63606860869883164, 13.57444820018226217 ) ) ;
#17290 = CARTESIAN_POINT ( 'NONE',  ( -0.8801773607111008646, 53.27201867748816966, 2.915334737309923430 ) ) ;
#17291 = CARTESIAN_POINT ( 'NONE',  ( -14.49440716394870599, 15.00000000000000000, -0.4026921475168267484 ) ) ;
#17292 = DIRECTION ( 'NONE',  ( 0.000000000000000000, 0.000000000000000000, 1.000000000000000000 ) ) ;
#17293 = CARTESIAN_POINT ( 'NONE',  ( 18.52753015748618282, 8.925597817667451750, -4.923371831947291888 ) ) ;
#17294 = CARTESIAN_POINT ( 'NONE',  ( 3.591859063236763294, 13.29030133659708746, -11.09922568453595026 ) ) ;
#17295 = LINE ( 'NONE', #18269, #38738 ) ;
#17296 = AXIS2_PLACEMENT_3D ( 'NONE', #43269, #73764, #36271 ) ;
#17297 = CARTESIAN_POINT ( 'NONE',  ( 2.791683348922240793, 36.63393115100078035, 7.208316651077764092 ) ) ;
#17298 = CARTESIAN_POINT ( 'NONE',  ( 10.00000000000000000, 62.87363466993042493, -12.81628187352647608 ) ) ;
#17299 = CARTESIAN_POINT ( 'NONE',  ( -4.164238869374099927, 12.01208216824730357, 3.795296366450308767 ) ) ;
#17300 = CARTESIAN_POINT ( 'NONE',  ( 19.84674366389459266, 13.71726448433411782, -2.638427012816827677 ) ) ;
#17301 = CARTESIAN_POINT ( 'NONE',  ( 19.38216949554541557, 22.24863466993041428, -9.382169495545420901 ) ) ;
#17303 = CARTESIAN_POINT ( 'NONE',  ( -4.536330484516918560, -17.54398402260299861, -2.750000000000000000 ) ) ;
#17302 = DIRECTION ( 'NONE',  ( 0.000000000000000000, 0.000000000000000000, 1.000000000000000000 ) ) ;
#17304 = CARTESIAN_POINT ( 'NONE',  ( 15.44008868035555793, 46.39701867748817676, -9.422509992056140149 ) ) ;
#17305 = CARTESIAN_POINT ( 'NONE',  ( 17.20831665107776587, 62.88393115100078745, 7.208316651077764980 ) ) ;
#17306 = DIRECTION ( 'NONE',  ( 1.000000000000000000, -0.000000000000000000, 0.000000000000000000 ) ) ;
#17307 = CARTESIAN_POINT ( 'NONE',  ( 18.52753015748618282, 23.92559781766745530, -4.923371831947291888 ) ) ;
#17308 = CARTESIAN_POINT ( 'NONE',  ( 10.00000000000000000, 16.81368534415483751, -10.88017736071110342 ) ) ;
#17309 = CARTESIAN_POINT ( 'NONE',  ( 6.565887622018943937, 18.08196800326375708, -12.81628187352647608 ) ) ;
#17310 = CARTESIAN_POINT ( 'NONE',  ( 19.84674366389459621, 18.50893115100078745, 7.409399052514197653E-17 ) ) ;
#17311 = DIRECTION ( 'NONE',  ( -0.000000000000000000, -1.000000000000000000, -0.000000000000000000 ) ) ;
#17312 = EDGE_CURVE ( 'NONE', #47751, #5309, #26498, .T. ) ;
#17313 = CARTESIAN_POINT ( 'NONE',  ( 20.88017736071110875, 20.77201867748816611, -2.915334737309920765 ) ) ;
#17314 = CARTESIAN_POINT ( 'NONE',  ( 19.42250999205614548, 55.98035201082150536, -5.440088680355545492 ) ) ;
#17315 = DIRECTION ( 'NONE',  ( 1.000000000000000000, 0.000000000000000000, 0.000000000000000000 ) ) ;
#17316 = EDGE_CURVE ( 'NONE', #73495, #7776, #95837, .T. ) ;
#17318 = CARTESIAN_POINT ( 'NONE',  ( 20.88017736071110875, 10.77201867748817143, -2.915334737309920765 ) ) ;
#17317 = CARTESIAN_POINT ( 'NONE',  ( 18.52753015748618282, 48.92559781766745886, -4.923371831947291888 ) ) ;
#17319 = FILL_AREA_STYLE_COLOUR ( '', #64710 ) ;
#17320 = CARTESIAN_POINT ( 'NONE',  ( 7.084665262690076126, 52.02201867748816255, -10.88017736071110164 ) ) ;
#17321 = AXIS2_PLACEMENT_3D ( 'NONE', #74925, #59420, #11102 ) ;
#17323 = FACE_OUTER_BOUND ( 'NONE', #53241, .T. ) ;
#17322 = CARTESIAN_POINT ( 'NONE',  ( 20.88017736071110519, 10.56368534415483929, 2.639326808657452039E-16 ) ) ;
#17324 = CARTESIAN_POINT ( 'NONE',  ( 17.20831665107776587, 19.13393115100078035, -7.208316651077762316 ) ) ;
#17325 = CARTESIAN_POINT ( 'NONE',  ( 12.63842701281683034, 37.46726448433411605, 9.846743663894596210 ) ) ;
#17326 = DIRECTION ( 'NONE',  ( 0.000000000000000000, 1.000000000000000000, 0.000000000000000000 ) ) ;
#17327 = CARTESIAN_POINT ( 'NONE',  ( 11.62719953690058361, 0.5000000000000004441, 9.476720473301874392 ) ) ;
#17328 = CARTESIAN_POINT ( 'NONE',  ( -1.099225684535947600, -1.293031996736246469, -6.408140936763238038 ) ) ;
#17330 = DIRECTION ( 'NONE',  ( -0.000000000000000000, -0.000000000000000000, -1.000000000000000000 ) ) ;
#17329 = COLOUR_RGB ( '', 0.66274510, 0.83137255, 0.94901961) ;
#17331 = AXIS2_PLACEMENT_3D ( 'NONE', #18602, #49567, #19578 ) ;
#17332 = CARTESIAN_POINT ( 'NONE',  ( 20.36894250292379738, 19.92874883491396787, -10.36894250292379027 ) ) ;
#17333 = CARTESIAN_POINT ( 'NONE',  ( 2.791683348922240793, 41.63393115100078745, 7.208316651077764092 ) ) ;
#17334 = FACE_OUTER_BOUND ( 'NONE', #70409, .T. ) ;
#17335 = VERTEX_POINT ( 'NONE', #15674 ) ;
#17336 = CARTESIAN_POINT ( 'NONE',  ( -0.3689425029237898834, 56.17874883491396076, -10.36894250292378850 ) ) ;
#17337 = CARTESIAN_POINT ( 'NONE',  ( 17.20831665107776587, 17.88393115100078745, 7.208316651077764980 ) ) ;
#17339 = CARTESIAN_POINT ( 'NONE',  ( 4.879999999999991900, 76.07179676972444327, 4.250000000000000000 ) ) ;
#17338 = CARTESIAN_POINT ( 'NONE',  ( -0.1503990784575328643, 70.00000000000000000, 6.262539305110068177 ) ) ;
#17340 = CARTESIAN_POINT ( 'NONE',  ( 17.96484262340118221, 46.18868534415484106, -7.964842623401177768 ) ) ;
#17341 = CARTESIAN_POINT ( 'NONE',  ( 10.00000000000000000, 62.87363466993042493, -12.81628187352647608 ) ) ;
#17342 = CARTESIAN_POINT ( 'NONE',  ( -0.8801773607110991993, 17.85535201082150536, -2.915334737309923874 ) ) ;
#17343 = CARTESIAN_POINT ( 'NONE',  ( 22.81628187352647785, 46.62363466993041783, 6.195893100308588602E-16 ) ) ;
#17344 = CARTESIAN_POINT ( 'NONE',  ( -2.816281873526473856, 9.331968003263753531, 3.434112377981055619 ) ) ;
#17345 = CARTESIAN_POINT ( 'NONE',  ( 10.00000000000000000, 9.758931151000785675, -9.846743663894594434 ) ) ;
#17346 = ORIENTED_EDGE ( 'NONE', *, *, #23549, .F. ) ;
#17347 = CARTESIAN_POINT ( 'NONE',  ( -6.000000000000012434, 79.82179676972448590, -6.250000000000000000 ) ) ;
#17348 = DIRECTION ( 'NONE',  ( 0.000000000000000000, -0.000000000000000000, -1.000000000000000000 ) ) ;
#17349 = CARTESIAN_POINT ( 'NONE',  ( 13.79529636645030344, 53.26208216824730357, 14.16423886937410614 ) ) ;
#17350 = CARTESIAN_POINT ( 'NONE',  ( -4.164238869374099039, 21.80374883491396787, 8.674139862899312516E-16 ) ) ;
#17351 = CARTESIAN_POINT ( 'NONE',  ( 4.559911319644449179, 22.23035201082150536, -9.422509992056141925 ) ) ;
#17352 = CARTESIAN_POINT ( 'NONE',  ( 12.91533473730992121, 49.52201867748817676, 10.88017736071110164 ) ) ;
#17353 = PLANE ( 'NONE',  #3208 ) ;
#17354 = ADVANCED_FACE ( 'NONE', ( #76642 ), #83663, .T. ) ;
#17355 = CARTESIAN_POINT ( 'NONE',  ( 6.000000000000000000, 11.00000000000000000, -5.000000000000000000 ) ) ;
#17356 = CARTESIAN_POINT ( 'NONE',  ( 10.00000000000000178, 2.258931151000784787, 9.846743663894594434 ) ) ;
#17357 =( LENGTH_UNIT ( ) NAMED_UNIT ( * ) SI_UNIT ( .MILLI., .METRE. ) );
#17358 = CARTESIAN_POINT ( 'NONE',  ( 0.1532563361054082862, 16.21726448433411960, 2.638427012816831674 ) ) ;
#17359 = CARTESIAN_POINT ( 'NONE',  ( 18.52753015748618282, 28.92559781766745175, -4.923371831947291888 ) ) ;
#17360 = CARTESIAN_POINT ( 'NONE',  ( 14.92337183194729633, 52.67559781766745175, 8.527530157486181039 ) ) ;
#17361 = EDGE_CURVE ( 'NONE', #36347, #67137, #60084, .T. ) ;
#17362 = CARTESIAN_POINT ( 'NONE',  ( -0.8801773607110991993, 17.85535201082150536, -2.915334737309923874 ) ) ;
#17363 = CARTESIAN_POINT ( 'NONE',  ( 3.591859063236761518, 29.95696800326375708, 11.09922568453594849 ) ) ;
#17364 = CARTESIAN_POINT ( 'NONE',  ( 0.5774900079438590739, 47.64701867748817676, -5.440088680355550821 ) ) ;
#17365 = CARTESIAN_POINT ( 'NONE',  ( 17.20831665107776587, 24.13393115100078035, -7.208316651077762316 ) ) ;
#17367 = CARTESIAN_POINT ( 'NONE',  ( 18.52753015748617571, 8.092264484334117824, 4.923371831947298993 ) ) ;
#17366 = CARTESIAN_POINT ( 'NONE',  ( -2.266590686148945544, 41.38708216824729647, -7.082119434687050408 ) ) ;
#17368 = DIRECTION ( 'NONE',  ( 0.7808688094430307203, -0.6246950475544238435, 0.000000000000000000 ) ) ;
#17369 = CARTESIAN_POINT ( 'NONE',  ( 18.52753015748617571, 53.09226448433412315, 4.923371831947298993 ) ) ;
#17370 = CARTESIAN_POINT ( 'NONE',  ( 18.52753015748618282, 38.92559781766745175, -4.923371831947291888 ) ) ;
#17371 = CARTESIAN_POINT ( 'NONE',  ( 2.917880565312950480, 15.97041550158063217, -12.26659068614894821 ) ) ;
#17372 = CARTESIAN_POINT ( 'NONE',  ( 2.791683348922237240, 30.38393115100078390, -7.208316651077763204 ) ) ;
#17373 = CARTESIAN_POINT ( 'NONE',  ( 20.88017736071110519, 50.56368534415484106, 2.639326808657452039E-16 ) ) ;
#17374 = CARTESIAN_POINT ( 'NONE',  ( 0.5774900079438590739, 7.647018677488171434, -5.440088680355550821 ) ) ;
#17375 = ADVANCED_FACE ( 'NONE', ( #60160 ), #93592, .T. ) ;
#17376 = CARTESIAN_POINT ( 'NONE',  ( 2.035157376598822676, 47.43868534415484817, -7.964842623401177768 ) ) ;
#17377 = CARTESIAN_POINT ( 'NONE',  ( 15.44008868035555260, 24.73035201082150891, 9.422509992056143702 ) ) ;
#17378 = ORIENTED_EDGE ( 'NONE', *, *, #73140, .T. ) ;
#17379 = CARTESIAN_POINT ( 'NONE',  ( 6.565887622018943937, 33.08196800326374643, -12.81628187352647608 ) ) ;
#17380 = CARTESIAN_POINT ( 'NONE',  ( 0.5774900079438590739, 42.64701867748816966, -5.440088680355550821 ) ) ;
#17381 = ORIENTED_EDGE ( 'NONE', *, *, #47163, .F. ) ;
#17382 = CARTESIAN_POINT ( 'NONE',  ( 18.00000000000000355, 73.00000000000001421, 6.250000000000000000 ) ) ;
#17383 = CARTESIAN_POINT ( 'NONE',  ( 20.88017736071110875, 60.77201867748817676, -2.915334737309920765 ) ) ;
#17384 = ORIENTED_EDGE ( 'NONE', *, *, #5213, .T. ) ;
#17385 = CARTESIAN_POINT ( 'NONE',  ( 4.559911319644449179, 43.89701867748816966, 9.422509992056141925 ) ) ;
#17386 = CARTESIAN_POINT ( 'NONE',  ( 4.559911319644449179, 3.897018677488170990, 9.422509992056141925 ) ) ;
#17387 = CARTESIAN_POINT ( 'NONE',  ( 20.88017736071110519, 40.56368534415484106, 2.639326808657452039E-16 ) ) ;
#17388 = DIRECTION ( 'NONE',  ( 0.000000000000000000, 0.000000000000000000, -1.000000000000000000 ) ) ;
#17389 = CARTESIAN_POINT ( 'NONE',  ( 10.00000000000000178, 63.05374883491396076, 14.16423886937410082 ) ) ;
#17390 = CARTESIAN_POINT ( 'NONE',  ( 10.00000000000000000, 4.758931151000784787, -9.846743663894594434 ) ) ;
#17391 = CARTESIAN_POINT ( 'NONE',  ( 20.36894250292379738, 9.928748834913966093, -10.36894250292379027 ) ) ;
#17392 = CARTESIAN_POINT ( 'NONE',  ( 0.1532563361054082862, 11.21726448433411605, 2.638427012816831674 ) ) ;
#17393 = EDGE_CURVE ( 'NONE', #12985, #24643, #12154, .T. ) ;
#17394 = CARTESIAN_POINT ( 'NONE',  ( 12.91533473730993009, 16.60535201082150891, -10.88017736071109987 ) ) ;
#17395 = CARTESIAN_POINT ( 'NONE',  ( 17.20831665107776587, 44.13393115100078745, -7.208316651077762316 ) ) ;
#17396 = ORIENTED_EDGE ( 'NONE', *, *, #79500, .F. ) ;
#17397 = CARTESIAN_POINT ( 'NONE',  ( 0.1532563361054082862, 51.21726448433412315, 2.638427012816831674 ) ) ;
#17398 = CIRCLE ( 'NONE', #86046, 18.93999999999999773 ) ;
#17399 = CARTESIAN_POINT ( 'NONE',  ( 8.209432707284918251, 14.49999999999999112, -12.55409154915490255 ) ) ;
#17400 = CARTESIAN_POINT ( 'NONE',  ( 0.5774900079438607392, 38.48035201082150536, 5.440088680355550821 ) ) ;
#17401 = CARTESIAN_POINT ( 'NONE',  ( 0.1532563361054082862, 56.21726448433411605, 2.638427012816831674 ) ) ;
#17402 = CARTESIAN_POINT ( 'NONE',  ( 19.38216949554541557, 32.24863466993041783, -9.382169495545420901 ) ) ;
#17403 = CARTESIAN_POINT ( 'NONE',  ( 6.189644032515678518, 14.95077488074853456, 13.39157970158800204 ) ) ;
#17404 = CARTESIAN_POINT ( 'NONE',  ( 12.91533473730993009, 41.60535201082149825, -10.88017736071109987 ) ) ;
#17405 = CARTESIAN_POINT ( 'NONE',  ( 15.44008868035555260, 4.730352010821505360, 9.422509992056143702 ) ) ;
#17406 = CIRCLE ( 'NONE', #57266, 0.2500000000000002220 ) ;
#17407 = ADVANCED_FACE ( 'NONE', ( #27320 ), #8963, .T. ) ;
#17408 = AXIS2_PLACEMENT_3D ( 'NONE', #11737, #26249, #95739 ) ;
#17409 = CARTESIAN_POINT ( 'NONE',  ( -2.816281873526473856, 19.12363466993042138, 9.499525473075851096E-16 ) ) ;
#17410 = DIRECTION ( 'NONE',  ( 0.000000000000000000, 0.000000000000000000, 1.000000000000000000 ) ) ;
#17411 = EDGE_CURVE ( 'NONE', #60629, #6181, #16953, .T. ) ;
#17412 = ORIENTED_EDGE ( 'NONE', *, *, #69776, .F. ) ;
#17413 = CARTESIAN_POINT ( 'NONE',  ( -1.099225684535947600, 23.70696800326375708, -6.408140936763238038 ) ) ;
#17414 = CARTESIAN_POINT ( 'NONE',  ( 0.5774900079438590739, 17.64701867748817321, -5.440088680355550821 ) ) ;
#17415 = ORIENTED_EDGE ( 'NONE', *, *, #4488, .T. ) ;
#17416 = CARTESIAN_POINT ( 'NONE',  ( 19.84674366389459266, 3.300597817667451750, 2.638427012816836559 ) ) ;
#17417 = CARTESIAN_POINT ( 'NONE',  ( 14.92337183194729988, 54.34226448433412315, -8.527530157486177487 ) ) ;
#17419 = CARTESIAN_POINT ( 'NONE',  ( 18.52753015748618282, 43.92559781766745175, -4.923371831947291888 ) ) ;
#17418 = CARTESIAN_POINT ( 'NONE',  ( 19.84674366389459266, 13.71726448433411782, -2.638427012816827677 ) ) ;
#17420 = CARTESIAN_POINT ( 'NONE',  ( 17.85999999999999233, 22.49999999999995026, 10.00000000000000000 ) ) ;
#17421 = PRESENTATION_STYLE_ASSIGNMENT (( #944 ) ) ;
#17422 = CARTESIAN_POINT ( 'NONE',  ( 0.1532563361054100626, 25.80059781766744820, -2.638427012816831230 ) ) ;
#17423 = CARTESIAN_POINT ( 'NONE',  ( -0.1503990784575328088, 3.101585745166421493, 6.262539305110068177 ) ) ;
#17424 = DIRECTION ( 'NONE',  ( 0.000000000000000000, 1.000000000000000000, 0.000000000000000000 ) ) ;
#17426 = CARTESIAN_POINT ( 'NONE',  ( -0.1503990784575328643, 70.00000000000000000, 6.262539305110068177 ) ) ;
#17425 = CARTESIAN_POINT ( 'NONE',  ( 1.472469842513823179, 21.42559781766745175, 4.923371831947296329 ) ) ;
#17428 = ORIENTED_EDGE ( 'NONE', *, *, #36807, .T. ) ;
#17427 = CARTESIAN_POINT ( 'NONE',  ( 12.63842701281683922, 39.55059781766744464, -9.846743663894590881 ) ) ;
#17429 = CARTESIAN_POINT ( 'NONE',  ( -2.849309504156474215, 0.000000000000000000, -4.649650521509827605 ) ) ;
#17430 = CARTESIAN_POINT ( 'NONE',  ( 3.591859063236761518, 29.95696800326375708, 11.09922568453594849 ) ) ;
#17431 = EDGE_CURVE ( 'NONE', #13947, #48651, #48837, .T. ) ;
#17432 = CARTESIAN_POINT ( 'NONE',  ( -1.881645754503658452, 15.00000000000000533, -14.50406564081099603 ) ) ;
#17433 = CARTESIAN_POINT ( 'NONE',  ( -0.3689425029237881626, 47.42874883491396787, 10.36894250292379027 ) ) ;
#17434 = CARTESIAN_POINT ( 'NONE',  ( 12.63842701281683034, 17.46726448433411250, 9.846743663894596210 ) ) ;
#17435 = CARTESIAN_POINT ( 'NONE',  ( 5.076628168052704559, 5.175597817667451750, -8.527530157486179263 ) ) ;
#17436 = CARTESIAN_POINT ( 'NONE',  ( -12.50534872682737664, 4.247830340245585198E-16, 7.339363270777436554 ) ) ;
#17437 = EDGE_CURVE ( 'NONE', #47708, #69540, #24883, .T. ) ;
#17438 = CARTESIAN_POINT ( 'NONE',  ( 24.16423886937410614, 44.30374883491397497, 8.672049930838204340E-16 ) ) ;
#17439 = CARTESIAN_POINT ( 'NONE',  ( 17.20831665107776587, 64.13393115100079456, -7.208316651077762316 ) ) ;
#17440 = CARTESIAN_POINT ( 'NONE',  ( 17.96484262340118221, 11.18868534415484106, -7.964842623401177768 ) ) ;
#17441 = CARTESIAN_POINT ( 'NONE',  ( -0.3689425029237881626, 27.42874883491397142, 10.36894250292379027 ) ) ;
#17442 = CARTESIAN_POINT ( 'NONE',  ( 10.00000000000000000, 40.55374883491397497, -14.16423886937410082 ) ) ;
#17443 = CARTESIAN_POINT ( 'NONE',  ( -42.94000000000001194, 92.00000000000000000, 9.500000000000000000 ) ) ;
#17444 = AXIS2_PLACEMENT_3D ( 'NONE', #65032, #41094, #50052 ) ;
#17446 = CARTESIAN_POINT ( 'NONE',  ( 17.20831665107776587, 54.13393115100079456, -7.208316651077762316 ) ) ;
#17445 = CARTESIAN_POINT ( 'NONE',  ( 4.380000000000000782, 0.09385850579273792571, 2.750000000000000000 ) ) ;
#17447 = ORIENTED_EDGE ( 'NONE', *, *, #96429, .F. ) ;
#17448 = CARTESIAN_POINT ( 'NONE',  ( 7.084665262690076126, 34.10535201082151247, 10.88017736071109987 ) ) ;
#17449 = CARTESIAN_POINT ( 'NONE',  ( 20.03447792253739124, 22.65514106990690379, -6.401564815979733147 ) ) ;
#17450 = CARTESIAN_POINT ( 'NONE',  ( 19.64232630867097384, 93.02620456798111093, -5.304930624720125998 ) ) ;
#17451 = CARTESIAN_POINT ( 'NONE',  ( 5.076628168052703671, 41.84226448433411605, 8.527530157486179263 ) ) ;
#17452 = CARTESIAN_POINT ( 'NONE',  ( 0.2751277870542911397, 35.30223176428830811, 6.499999999999992006 ) ) ;
#17453 = CARTESIAN_POINT ( 'NONE',  ( 14.16423886937410259, -10.69625116508603213, -2.602085213965210642E-15 ) ) ;
#17454 = CARTESIAN_POINT ( 'NONE',  ( 7.361572987183170547, 42.05059781766745886, 9.846743663894590881 ) ) ;
#17455 = CARTESIAN_POINT ( 'NONE',  ( 10.00000000000000000, 64.75893115100078035, -9.846743663894594434 ) ) ;
#17456 = ORIENTED_EDGE ( 'NONE', *, *, #53096, .T. ) ;
#17457 = CARTESIAN_POINT ( 'NONE',  ( 24.16423886937410614, 9.512082168247301794, -3.795296366450302550 ) ) ;
#17458 = CARTESIAN_POINT ( 'NONE',  ( -10.93781366033333136, 15.00000000000000000, -10.26470809774080628 ) ) ;
#17460 = DIRECTION ( 'NONE',  ( 1.000000000000000000, 0.000000000000000000, 0.000000000000000000 ) ) ;
#17459 = FACE_OUTER_BOUND ( 'NONE', #22656, .T. ) ;
#17461 = CARTESIAN_POINT ( 'NONE',  ( -0.3689425029237898834, 66.17874883491396076, -10.36894250292378850 ) ) ;
#17462 = CARTESIAN_POINT ( 'NONE',  ( -2.816281873526473856, 29.33196800326376064, 3.434112377981055619 ) ) ;
#17463 = CARTESIAN_POINT ( 'NONE',  ( 1.472469842513823179, 0.5922644843341181575, -4.923371831947296329 ) ) ;
#17464 =( LENGTH_UNIT ( ) NAMED_UNIT ( * ) SI_UNIT ( .MILLI., .METRE. ) );
#17465 = VECTOR ( 'NONE', #94715, 1000.000000000000000 ) ;
#17466 = CARTESIAN_POINT ( 'NONE',  ( -0.1503990784575328643, 10.12777174578612716, 6.262539305110068177 ) ) ;
#17467 = CARTESIAN_POINT ( 'NONE',  ( -46.44000000000001194, 103.0000000000000000, -8.999999999999998224 ) ) ;
#17468 = CARTESIAN_POINT ( 'NONE',  ( 6.204703633549690345, 65.76208216824731778, -14.16423886937410259 ) ) ;
#17469 = CARTESIAN_POINT ( 'NONE',  ( -0.1503990784575282014, 42.22266099184918886, -6.262539305110077947 ) ) ;
#17470 = CARTESIAN_POINT ( 'NONE',  ( 10.00000000000000000, 26.81368534415484106, -10.88017736071110342 ) ) ;
#17471 = CARTESIAN_POINT ( 'NONE',  ( 10.00000000000000000, 31.81368534415483751, -10.88017736071110342 ) ) ;
#17472 = CARTESIAN_POINT ( 'NONE',  ( 2.791683348922237240, 65.38393115100078035, -7.208316651077763204 ) ) ;
#17473 = CARTESIAN_POINT ( 'NONE',  ( 21.09922568453595559, 62.04030133659709634, -6.408140936763230044 ) ) ;
#17474 = SURFACE_SIDE_STYLE ('',( #23990 ) ) ;
#17475 = ORIENTED_EDGE ( 'NONE', *, *, #33005, .T. ) ;
#17476 = TOROIDAL_SURFACE ( 'NONE', #49354, 0.5000000000000000000, 0.2500000000000000000 ) ;
#17477 = CARTESIAN_POINT ( 'NONE',  ( 10.00000000000000000, 36.81368534415484106, -10.88017736071110342 ) ) ;
#17478 = EDGE_CURVE ( 'NONE', #52153, #49358, #57812, .T. ) ;
#17479 = CARTESIAN_POINT ( 'NONE',  ( 3.591859063236761518, 29.95696800326375708, 11.09922568453594849 ) ) ;
#17480 = CARTESIAN_POINT ( 'NONE',  ( 18.72515096720573879, 35.05509018479936145, 6.499999999999937828 ) ) ;
#17481 = UNCERTAINTY_MEASURE_WITH_UNIT (LENGTH_MEASURE( 1.000000000000000082E-05 ), #34309, 'distance_accuracy_value', 'NONE');
#17482 = CARTESIAN_POINT ( 'NONE',  ( 10.00000000000000000, 59.75893115100078745, -9.846743663894594434 ) ) ;
#17483 = CARTESIAN_POINT ( 'NONE',  ( 20.88017736071110519, 50.56368534415484106, 2.639326808657452039E-16 ) ) ;
#17484 = CARTESIAN_POINT ( 'NONE',  ( 1.472469842513823179, 15.59226448433411960, -4.923371831947296329 ) ) ;
#17485 = CARTESIAN_POINT ( 'NONE',  ( 13.43411237798105340, 30.58196800326374998, 12.81628187352647963 ) ) ;
#17487 = FILL_AREA_STYLE_COLOUR ( '', #32083 ) ;
#17486 = CARTESIAN_POINT ( 'NONE',  ( 0.5774900079438607392, 63.48035201082149825, 5.440088680355550821 ) ) ;
#17488 = DIRECTION ( 'NONE',  ( 0.000000000000000000, 0.000000000000000000, -1.000000000000000000 ) ) ;
#17489 = CARTESIAN_POINT ( 'NONE',  ( 10.00000000000000178, 65.37363466993042493, 12.81628187352647608 ) ) ;
#17490 = ORIENTED_EDGE ( 'NONE', *, *, #28357, .F. ) ;
#17491 = DIRECTION ( 'NONE',  ( 0.000000000000000000, 1.000000000000000000, 0.000000000000000000 ) ) ;
#17492 = DIRECTION ( 'NONE',  ( 1.257568779154408793E-17, 1.000000000000000000, -0.000000000000000000 ) ) ;
#17493 = CARTESIAN_POINT ( 'NONE',  ( 17.96484262340118221, 6.188685344154836621, -7.964842623401177768 ) ) ;
#17495 = CARTESIAN_POINT ( 'NONE',  ( 17.08211943468705130, 18.47041550158063572, 12.26659068614894998 ) ) ;
#17494 = CARTESIAN_POINT ( 'NONE',  ( 22.81628187352647785, 51.62363466993042493, 6.195893100308588602E-16 ) ) ;
#17496 = CARTESIAN_POINT ( 'NONE',  ( 2.791683348922237240, 20.38393115100078745, -7.208316651077763204 ) ) ;
#17497 = AXIS2_PLACEMENT_3D ( 'NONE', #92634, #56130, #10622 ) ;
#17498 = CARTESIAN_POINT ( 'NONE',  ( -0.8801773607111009756, 3.063685344154837509, 1.068504757029289695E-15 ) ) ;
#17499 = CARTESIAN_POINT ( 'NONE',  ( 10.00000000000000000, 14.75893115100078568, -9.846743663894594434 ) ) ;
#17500 = CARTESIAN_POINT ( 'NONE',  ( 22.26659068614894466, 53.88708216824731068, 7.082119434687054849 ) ) ;
#17501 = ORIENTED_EDGE ( 'NONE', *, *, #36990, .T. ) ;
#17502 = CARTESIAN_POINT ( 'NONE',  ( 0.5774900079438590739, 2.647018677488170990, -5.440088680355550821 ) ) ;
#17503 = MECHANICAL_DESIGN_GEOMETRIC_PRESENTATION_REPRESENTATION (  '', ( #20701 ), #59013 ) ;
#17504 = CARTESIAN_POINT ( 'NONE',  ( 19.42250999205614548, 15.98035201082150714, -5.440088680355545492 ) ) ;
#17505 = DIRECTION ( 'NONE',  ( 0.000000000000000000, -1.000000000000000000, 0.000000000000000000 ) ) ;
#17506 = VERTEX_POINT ( 'NONE', #66299 ) ;
#17507 = ORIENTED_EDGE ( 'NONE', *, *, #40802, .T. ) ;
#17508 = CARTESIAN_POINT ( 'NONE',  ( -0.8801773607110991993, 17.85535201082150536, -2.915334737309923874 ) ) ;
#17509 = CARTESIAN_POINT ( 'NONE',  ( 12.91533473730992121, 14.52201867748817143, 10.88017736071110164 ) ) ;
#17510 = CARTESIAN_POINT ( 'NONE',  ( 14.92337183194729633, 57.67559781766745886, 8.527530157486181039 ) ) ;
#17511 = CARTESIAN_POINT ( 'NONE',  ( 22.81628187352648496, 46.83196800326376064, -3.434112377981050290 ) ) ;
#17512 = CARTESIAN_POINT ( 'NONE',  ( -13.07751017357388257, 4.569076162262063760E-16, 6.263284095430414311 ) ) ;
#17513 = CARTESIAN_POINT ( 'NONE',  ( 24.16423886937410614, 14.51208216824730179, -3.795296366450302550 ) ) ;
#17514 = CARTESIAN_POINT ( 'NONE',  ( 20.88017736071110519, 20.56368534415484106, 2.639326808657452039E-16 ) ) ;
#17515 = CARTESIAN_POINT ( 'NONE',  ( 12.91533473730992121, 14.52201867748817143, 10.88017736071110164 ) ) ;
#17516 = CARTESIAN_POINT ( 'NONE',  ( 19.84674366389459621, 53.50893115100078745, 7.409399052514197653E-17 ) ) ;
#17517 = CARTESIAN_POINT ( 'NONE',  ( 12.30000000000000249, 99.99999999999998579, -8.000000000000000000 ) ) ;
#17518 = CARTESIAN_POINT ( 'NONE',  ( 2.791683348922237240, 35.38393115100079456, -7.208316651077763204 ) ) ;
#17519 = FACE_OUTER_BOUND ( 'NONE', #26732, .T. ) ;
#17520 = CARTESIAN_POINT ( 'NONE',  ( 14.92337183194729633, 7.675597817667451750, 8.527530157486181039 ) ) ;
#17521 = CARTESIAN_POINT ( 'NONE',  ( -8.527530157486182816, 30.59226448433413736, -4.923371831947288335 ) ) ;
#17522 = ORIENTED_EDGE ( 'NONE', *, *, #68890, .T. ) ;
#17523 = AXIS2_PLACEMENT_3D ( 'NONE', #52349, #30327, #76334 ) ;
#17524 = FILL_AREA_STYLE_COLOUR ( '', #71702 ) ;
#17525 = CARTESIAN_POINT ( 'NONE',  ( 19.84674366389459266, 8.300597817667451750, 2.638427012816836559 ) ) ;
#17526 = CARTESIAN_POINT ( 'NONE',  ( 3.591859063236761518, 4.956968003263753531, 11.09922568453594849 ) ) ;
#17527 = CARTESIAN_POINT ( 'NONE',  ( 12.91533473730993009, 46.60535201082150536, -10.88017736071109987 ) ) ;
#17529 = CARTESIAN_POINT ( 'NONE',  ( 16.40814093676323893, 45.79030133659708923, 11.09922568453595026 ) ) ;
#17528 =( NAMED_UNIT ( * ) PLANE_ANGLE_UNIT ( ) SI_UNIT ( $, .RADIAN. ) );
#17530 = CARTESIAN_POINT ( 'NONE',  ( 13.79529636645031943, 20.34541550158063572, -14.16423886937409904 ) ) ;
#17531 = EDGE_CURVE ( 'NONE', #59664, #77130, #21813, .T. ) ;
#17532 = CARTESIAN_POINT ( 'NONE',  ( 21.09922568453595559, 57.04030133659708923, -6.408140936763230044 ) ) ;
#17533 = EDGE_CURVE ( 'NONE', #4322, #33828, #29290, .T. ) ;
#17534 = ORIENTED_EDGE ( 'NONE', *, *, #72028, .F. ) ;
#17535 = CARTESIAN_POINT ( 'NONE',  ( 19.84674366389459621, 53.50893115100078745, 7.409399052514197653E-17 ) ) ;
#17536 = CARTESIAN_POINT ( 'NONE',  ( 17.96484262340118221, 19.93868534415484106, 7.964842623401181321 ) ) ;
#17537 = ORIENTED_EDGE ( 'NONE', *, *, #48650, .F. ) ;
#17538 = CARTESIAN_POINT ( 'NONE',  ( 10.00000000000000178, 69.31368534415484817, 10.88017736071110342 ) ) ;
#17539 = CARTESIAN_POINT ( 'NONE',  ( 15.00000000000000000, 60.50000000000000711, -6.000000000000000000 ) ) ;
#17540 = DIRECTION ( 'NONE',  ( 0.000000000000000000, 1.000000000000000000, 0.000000000000000000 ) ) ;
#17541 = CARTESIAN_POINT ( 'NONE',  ( 10.00000000000000000, 14.75893115100078568, -9.846743663894594434 ) ) ;
#17542 = CARTESIAN_POINT ( 'NONE',  ( 18.52753015748617571, 3.092264484334118269, 4.923371831947298993 ) ) ;
#17543 = DIRECTION ( 'NONE',  ( 0.000000000000000000, 9.540979117872431131E-15, 1.000000000000000000 ) ) ;
#17544 = CARTESIAN_POINT ( 'NONE',  ( 17.96484262340118221, 61.18868534415482685, -7.964842623401177768 ) ) ;
#17545 = CARTESIAN_POINT ( 'NONE',  ( 0.5774900079438590739, 62.64701867748817676, -5.440088680355550821 ) ) ;
#17547 = ORIENTED_EDGE ( 'NONE', *, *, #76347, .T. ) ;
#17546 = CARTESIAN_POINT ( 'NONE',  ( 5.076628168052703671, 6.842264484334118713, 8.527530157486179263 ) ) ;
#17548 = CARTESIAN_POINT ( 'NONE',  ( 5.817157072110708427, 14.49999999999999112, 13.82608706751097749 ) ) ;
#17550 = EDGE_CURVE ( 'NONE', #48910, #4697, #81313, .T. ) ;
#17549 = CARTESIAN_POINT ( 'NONE',  ( 7.361572987183170547, 52.05059781766745175, 9.846743663894590881 ) ) ;
#17551 = VERTEX_POINT ( 'NONE', #36309 ) ;
#17552 = ORIENTED_EDGE ( 'NONE', *, *, #23066, .T. ) ;
#17553 = LINE ( 'NONE', #1574, #49000 ) ;
#17554 = CARTESIAN_POINT ( 'NONE',  ( -0.3689425029237898834, 1.178748834913967869, -10.36894250292378850 ) ) ;
#17555 = CARTESIAN_POINT ( 'NONE',  ( 21.09922568453594849, 56.20696800326375353, 6.408140936763242479 ) ) ;
#17556 = ADVANCED_FACE ( 'NONE', ( #28311 ), #21312, .F. ) ;
#17557 = AXIS2_PLACEMENT_3D ( 'NONE', #8362, #45368, #29864 ) ;
#17558 = CARTESIAN_POINT ( 'NONE',  ( -2.266590686148945544, 16.38708216824730357, -7.082119434687050408 ) ) ;
#17559 = CARTESIAN_POINT ( 'NONE',  ( 20.36894250292379738, 4.928748834913967869, -10.36894250292379027 ) ) ;
#17560 = CARTESIAN_POINT ( 'NONE',  ( 20.88017736071110164, 15.35535201082150358, 2.915334737309930979 ) ) ;
#17561 = CARTESIAN_POINT ( 'NONE',  ( -28.94000000000001549, 93.50000000000000000, 9.500000000000000000 ) ) ;
#17562 = ORIENTED_EDGE ( 'NONE', *, *, #40260, .T. ) ;
#17563 = CARTESIAN_POINT ( 'NONE',  ( 2.791683348922237240, 5.383931151000785675, -7.208316651077763204 ) ) ;
#17565 = VECTOR ( 'NONE', #82804, 1000.000000000000000 ) ;
#17564 = CARTESIAN_POINT ( 'NONE',  ( 18.52753015748617571, 13.09226448433411960, 4.923371831947298993 ) ) ;
#17566 = CARTESIAN_POINT ( 'NONE',  ( -1.099225684535947600, 33.70696800326375353, -6.408140936763238038 ) ) ;
#17567 = CARTESIAN_POINT ( 'NONE',  ( 5.076628168052703671, 31.84226448433412315, 8.527530157486179263 ) ) ;
#17568 = CARTESIAN_POINT ( 'NONE',  ( 0.000000000000000000, 14.49999999999999822, 0.000000000000000000 ) ) ;
#17569 = CARTESIAN_POINT ( 'NONE',  ( 6.565887622018943937, 33.08196800326374643, -12.81628187352647608 ) ) ;
#17570 = DIRECTION ( 'NONE',  ( -0.9990482215818576872, 0.000000000000000000, -0.04361938736533987893 ) ) ;
#17571 = CARTESIAN_POINT ( 'NONE',  ( 5.076628168052703671, 31.84226448433412315, 8.527530157486179263 ) ) ;
#17572 = CARTESIAN_POINT ( 'NONE',  ( 6.204703633549690345, 12.84541550158063572, 14.16423886937410082 ) ) ;
#17573 = ORIENTED_EDGE ( 'NONE', *, *, #15567, .F. ) ;
#17574 = ORIENTED_EDGE ( 'NONE', *, *, #36512, .T. ) ;
#17575 = CARTESIAN_POINT ( 'NONE',  ( 0.5774900079438607392, 33.48035201082150536, 5.440088680355550821 ) ) ;
#17576 = CARTESIAN_POINT ( 'NONE',  ( 20.36894250292379382, 28.67874883491396787, 10.36894250292379205 ) ) ;
#17577 = CARTESIAN_POINT ( 'NONE',  ( 19.84674366389459266, 58.30059781766745886, 2.638427012816836559 ) ) ;
#17578 = CARTESIAN_POINT ( 'NONE',  ( 0.1532563361054100626, 15.80059781766745353, -2.638427012816831230 ) ) ;
#17580 = DIRECTION ( 'NONE',  ( -0.000000000000000000, -1.000000000000000000, 0.000000000000000000 ) ) ;
#17579 = CARTESIAN_POINT ( 'NONE',  ( -2.816281873526473856, 54.12363466993041783, 9.499525473075851096E-16 ) ) ;
#17581 = CARTESIAN_POINT ( 'NONE',  ( 19.42250999205614548, 30.98035201082150536, -5.440088680355545492 ) ) ;
#17582 = CARTESIAN_POINT ( 'NONE',  ( -13.82192141328815715, 4.664367351173465489E-16, 4.382292601468585680 ) ) ;
#17583 = CARTESIAN_POINT ( 'NONE',  ( 13.43411237798105340, 20.58196800326374643, 12.81628187352647963 ) ) ;
#17584 = CARTESIAN_POINT ( 'NONE',  ( 10.00000000000000000, 27.87363466993042138, -12.81628187352647608 ) ) ;
#17585 = CARTESIAN_POINT ( 'NONE',  ( 0.1532563361054100626, 45.80059781766745886, -2.638427012816831230 ) ) ;
#17586 = CARTESIAN_POINT ( 'NONE',  ( 5.440088680355549045, 6.397018677488181204, -9.422509992056141925 ) ) ;
#17587 = CARTESIAN_POINT ( 'NONE',  ( 21.09922568453594849, 51.20696800326375353, 6.408140936763242479 ) ) ;
#17588 = FILL_AREA_STYLE_COLOUR ( '', #18121 ) ;
#17590 = CARTESIAN_POINT ( 'NONE',  ( 20.10493008474207244, 9.716974130838785584, 6.336235997365739614 ) ) ;
#17589 = CARTESIAN_POINT ( 'NONE',  ( 20.88017736071110164, 50.35535201082151247, 2.915334737309930979 ) ) ;
#17591 = CARTESIAN_POINT ( 'NONE',  ( -45.94000000000000483, 93.00000000000000000, 9.500000000000000000 ) ) ;
#17592 = CARTESIAN_POINT ( 'NONE',  ( 17.96484262340118221, 51.18868534415483396, -7.964842623401177768 ) ) ;
#17593 = CARTESIAN_POINT ( 'NONE',  ( 15.44008868035555793, 51.39701867748816966, -9.422509992056140149 ) ) ;
#17594 = DIRECTION ( 'NONE',  ( -0.000000000000000000, -0.000000000000000000, 1.000000000000000000 ) ) ;
#17595 = CARTESIAN_POINT ( 'NONE',  ( 7.084665262690076126, 9.105352010821503583, 10.88017736071109987 ) ) ;
#17596 = CARTESIAN_POINT ( 'NONE',  ( 0.1532563361054100626, 65.80059781766745175, -2.638427012816831230 ) ) ;
#17598 = CARTESIAN_POINT ( 'NONE',  ( 0.2751277870542983006, 13.21833443783938122, 6.500000000000002665 ) ) ;
#17597 = CARTESIAN_POINT ( 'NONE',  ( -0.8801773607111008646, 18.27201867748817321, 2.915334737309923430 ) ) ;
#17599 = LINE ( 'NONE', #87064, #73614 ) ;
#17600 = CARTESIAN_POINT ( 'NONE',  ( 22.81628187352648496, 26.83196800326374998, -3.434112377981050290 ) ) ;
#17601 = ORIENTED_EDGE ( 'NONE', *, *, #1722, .T. ) ;
#17602 = CARTESIAN_POINT ( 'NONE',  ( 7.084665262690076126, 47.02201867748818387, -10.88017736071110164 ) ) ;
#17603 = CARTESIAN_POINT ( 'NONE',  ( 2.791683348922237240, 40.38393115100078035, -7.208316651077763204 ) ) ;
#17605 = CARTESIAN_POINT ( 'NONE',  ( 8.921421356237301481, 27.04185244743870697, 2.999999999999998668 ) ) ;
#17604 = CARTESIAN_POINT ( 'NONE',  ( -1.099225684535947600, 13.70696800326375353, -6.408140936763238038 ) ) ;
#17606 = CARTESIAN_POINT ( 'NONE',  ( 12.91533473730992121, 19.52201867748816611, 10.88017736071110164 ) ) ;
#17607 = CARTESIAN_POINT ( 'NONE',  ( 19.42250999205614193, 35.14701867748816966, 5.440088680355555262 ) ) ;
#17608 = CARTESIAN_POINT ( 'NONE',  ( 2.917880565312948704, 47.63708216824730357, 12.26659068614894643 ) ) ;
#17609 = CARTESIAN_POINT ( 'NONE',  ( 2.791683348922237240, 35.38393115100079456, -7.208316651077763204 ) ) ;
#17610 = CARTESIAN_POINT ( 'NONE',  ( 2.035157376598824452, 58.68868534415482685, 7.964842623401179544 ) ) ;
#17611 = SURFACE_SIDE_STYLE ('',( #48081 ) ) ;
#17612 = CARTESIAN_POINT ( 'NONE',  ( 22.26659068614894466, 13.88708216824730179, 7.082119434687054849 ) ) ;
#17613 = EDGE_CURVE ( 'NONE', #73208, #65699, #2560, .T. ) ;
#17614 = CARTESIAN_POINT ( 'NONE',  ( -6.732636091893170693, -88.11213685669366669, -2.750000000000000000 ) ) ;
#17615 = LINE ( 'NONE', #86596, #55184 ) ;
#17616 = AXIS2_PLACEMENT_3D ( 'NONE', #45127, #12663, #58655 ) ;
#17617 = ORIENTED_EDGE ( 'NONE', *, *, #72463, .F. ) ;
#17618 = EDGE_LOOP ( 'NONE', ( #91652, #60083, #59534, #49137 ) ) ;
#17619 = CARTESIAN_POINT ( 'NONE',  ( 13.79529636645030344, 43.26208216824730357, 14.16423886937410614 ) ) ;
#17620 = CARTESIAN_POINT ( 'NONE',  ( 24.16423886937410614, 39.30374883491396787, 8.672049930838204340E-16 ) ) ;
#17621 = CARTESIAN_POINT ( 'NONE',  ( 14.92337183194729988, 19.34226448433411960, -8.527530157486177487 ) ) ;
#17622 = CARTESIAN_POINT ( 'NONE',  ( 22.81628187352647785, 16.62363466993042138, 6.195893100308588602E-16 ) ) ;
#17623 = LINE ( 'NONE', #23157, #73088 ) ;
#17624 = CARTESIAN_POINT ( 'NONE',  ( 11.34661744925197624, 54.08985607419764818, 2.900000000000000355 ) ) ;
#17626 = CARTESIAN_POINT ( 'NONE',  ( 21.09922568453594849, 36.20696800326375353, 6.408140936763242479 ) ) ;
#17625 = CARTESIAN_POINT ( 'NONE',  ( -0.8801773607111008646, 63.27201867748817676, 2.915334737309923430 ) ) ;
#17627 = CARTESIAN_POINT ( 'NONE',  ( 17.08211943468705840, 30.13708216824730357, -12.26659068614894466 ) ) ;
#17628 = CARTESIAN_POINT ( 'NONE',  ( 12.91533473730992121, 29.52201867748817321, 10.88017736071110164 ) ) ;
#17629 = DIRECTION ( 'NONE',  ( -0.000000000000000000, -1.000000000000000000, -0.000000000000000000 ) ) ;
#17630 = CARTESIAN_POINT ( 'NONE',  ( 19.42250999205614193, 65.14701867748817676, 5.440088680355555262 ) ) ;
#17631 = VECTOR ( 'NONE', #46119, 999.9999999999998863 ) ;
#17632 = CARTESIAN_POINT ( 'NONE',  ( 9.846743663894590881, -16.69940218233254470, 2.638427012816828565 ) ) ;
#17633 = CARTESIAN_POINT ( 'NONE',  ( 1.472469842513823179, 5.592264484334118713, -4.923371831947296329 ) ) ;
#17634 = VERTEX_POINT ( 'NONE', #35311 ) ;
#17635 = FACE_OUTER_BOUND ( 'NONE', #41878, .T. ) ;
#17637 = EDGE_CURVE ( 'NONE', #92892, #2722, #90280, .T. ) ;
#17636 = PLANE ( 'NONE',  #97215 ) ;
#17638 = AXIS2_PLACEMENT_3D ( 'NONE', #74696, #37698, #89696 ) ;
#17639 = ORIENTED_EDGE ( 'NONE', *, *, #95368, .F. ) ;
#17640 = CARTESIAN_POINT ( 'NONE',  ( -4.164238869374099927, 2.012082168247300906, 3.795296366450308767 ) ) ;
#17642 = CARTESIAN_POINT ( 'NONE',  ( 2.035157376598822676, 7.438685344154837509, -7.964842623401177768 ) ) ;
#17641 = CARTESIAN_POINT ( 'NONE',  ( 7.084665262690076126, 4.105352010821503583, 10.88017736071109987 ) ) ;
#17644 = CARTESIAN_POINT ( 'NONE',  ( 10.00000000000000178, 10.37363466993041961, 12.81628187352647608 ) ) ;
#17643 = CARTESIAN_POINT ( 'NONE',  ( 18.52753015748617571, 38.09226448433412315, 4.923371831947298993 ) ) ;
#17645 = CARTESIAN_POINT ( 'NONE',  ( -14.24131928502210975, -0.03417435944610275333, -0.4973178280107823923 ) ) ;
#17646 = CARTESIAN_POINT ( 'NONE',  ( 1.472469842513823179, 6.425597817667451750, 4.923371831947296329 ) ) ;
#17647 = EDGE_CURVE ( 'NONE', #71473, #36285, #79174, .T. ) ;
#17648 = CARTESIAN_POINT ( 'NONE',  ( 3.591859063236761518, -0.04303199673624671928, 11.09922568453594849 ) ) ;
#17649 = ADVANCED_FACE ( 'NONE', ( #82793 ), #91959, .T. ) ;
#17650 = ORIENTED_EDGE ( 'NONE', *, *, #11523, .F. ) ;
#17651 = CARTESIAN_POINT ( 'NONE',  ( -4.164238869374099039, 51.80374883491396787, 8.674139862899312516E-16 ) ) ;
#17652 = ORIENTED_EDGE ( 'NONE', *, *, #23633, .F. ) ;
#17653 = CARTESIAN_POINT ( 'NONE',  ( -0.3689425029237898834, 51.17874883491397497, -10.36894250292378850 ) ) ;
#17654 = ORIENTED_EDGE ( 'NONE', *, *, #62796, .T. ) ;
#17655 = CARTESIAN_POINT ( 'NONE',  ( 20.88017736071110875, 40.77201867748818387, -2.915334737309920765 ) ) ;
#17656 = CARTESIAN_POINT ( 'NONE',  ( 7.084665262690076126, 34.10535201082151247, 10.88017736071109987 ) ) ;
#17657 = CARTESIAN_POINT ( 'NONE',  ( 15.44008868035555793, 36.39701867748816966, -9.422509992056140149 ) ) ;
#17658 = CARTESIAN_POINT ( 'NONE',  ( -44.70923076923077133, 101.8461538461538396, -9.500000000000000000 ) ) ;
#17659 = CARTESIAN_POINT ( 'NONE',  ( -0.8801773607111009756, 28.06368534415484106, 1.068504757029289695E-15 ) ) ;
#17660 = DIRECTION ( 'NONE',  ( 0.000000000000000000, 0.000000000000000000, -1.000000000000000000 ) ) ;
#17661 = AXIS2_PLACEMENT_3D ( 'NONE', #34610, #5622, #64122 ) ;
#17662 = CARTESIAN_POINT ( 'NONE',  ( 2.791683348922240793, 21.63393115100078745, 7.208316651077764092 ) ) ;
#17663 = CARTESIAN_POINT ( 'NONE',  ( -3.500000000000000444, 1.019547802438453887, 2.750000000000000000 ) ) ;
#17664 = ORIENTED_EDGE ( 'NONE', *, *, #83306, .F. ) ;
#17665 = CARTESIAN_POINT ( 'NONE',  ( 18.52753015748618282, 38.92559781766745175, -4.923371831947291888 ) ) ;
#17666 = PLANE ( 'NONE',  #22902 ) ;
#17667 = SURFACE_STYLE_FILL_AREA ( #55146 ) ;
#17668 = EDGE_CURVE ( 'NONE', #75865, #21055, #76931, .T. ) ;
#17669 = CARTESIAN_POINT ( 'NONE',  ( -3.500000000000000444, 1.019547802438453887, 2.750000000000000000 ) ) ;
#17670 = CARTESIAN_POINT ( 'NONE',  ( -1.881370533971078673, 6.047815243395702449E-16, -14.50512983964831371 ) ) ;
#17671 = CARTESIAN_POINT ( 'NONE',  ( -46.21538524526005887, 104.1852450480875660, 5.851526435683383376 ) ) ;
#17672 = CARTESIAN_POINT ( 'NONE',  ( 1.472469842513823179, 50.59226448433411605, -4.923371831947296329 ) ) ;
#17673 = CARTESIAN_POINT ( 'NONE',  ( -4.164238869374099927, 52.01208216824729647, 3.795296366450308767 ) ) ;
#17674 = CARTESIAN_POINT ( 'NONE',  ( -0.5000000000000073275, 80.99999999999994316, -1.249999999999987121 ) ) ;
#17675 = ORIENTED_EDGE ( 'NONE', *, *, #71490, .T. ) ;
#17676 = CYLINDRICAL_SURFACE ( 'NONE', #83173, 0.2500000000000002220 ) ;
#17677 = CARTESIAN_POINT ( 'NONE',  ( 5.076628168052704559, 15.17559781766745175, -8.527530157486179263 ) ) ;
#17678 = CARTESIAN_POINT ( 'NONE',  ( -2.816281873526473856, 64.12363466993042493, 9.499525473075851096E-16 ) ) ;
#17679 = CARTESIAN_POINT ( 'NONE',  ( 18.52753015748617571, 63.09226448433412315, 4.923371831947298993 ) ) ;
#17680 = CARTESIAN_POINT ( 'NONE',  ( 5.076628168052704559, 0.1755978176674514724, -8.527530157486179263 ) ) ;
#17681 = CARTESIAN_POINT ( 'NONE',  ( 0.1532563361054100626, 50.80059781766745175, -2.638427012816831230 ) ) ;
#17682 = EDGE_CURVE ( 'NONE', #80255, #75354, #4599, .T. ) ;
#17683 = DIRECTION ( 'NONE',  ( 0.000000000000000000, -0.000000000000000000, 1.000000000000000000 ) ) ;
#17684 = CIRCLE ( 'NONE', #30432, 14.49999999999999822 ) ;
#17685 = VERTEX_POINT ( 'NONE', #97326 ) ;
#17686 = CARTESIAN_POINT ( 'NONE',  ( 22.26659068614894466, 58.88708216824729647, 7.082119434687054849 ) ) ;
#17687 = CARTESIAN_POINT ( 'NONE',  ( 6.869455772997054233, -0.03417435944610275333, 14.44603661281844431 ) ) ;
#17688 = CARTESIAN_POINT ( 'NONE',  ( 19.42250999205614548, 45.98035201082150536, -5.440088680355545492 ) ) ;
#17689 = VECTOR ( 'NONE', #77951, 1000.000000000000000 ) ;
#17691 = CARTESIAN_POINT ( 'NONE',  ( 5.084766917237454109, 13.12107973746817358, -10.74788037306357324 ) ) ;
#17690 = CARTESIAN_POINT ( 'NONE',  ( 3.591859063236763294, 18.29030133659708568, -11.09922568453595026 ) ) ;
#17692 = CARTESIAN_POINT ( 'NONE',  ( 10.76445796112984787, -3.045506961852835686E-15, -9.901260316209842927 ) ) ;
#17693 = CARTESIAN_POINT ( 'NONE',  ( -3.836325488036276266, 0.3639308251242951986, 14.50112432709423516 ) ) ;
#17694 = VECTOR ( 'NONE', #29495, 1000.000000000000000 ) ;
#17695 = CARTESIAN_POINT ( 'NONE',  ( -0.04068437667222131460, 62.21974360917720048, -6.396802510829771471 ) ) ;
#17696 = CARTESIAN_POINT ( 'NONE',  ( 17.20831665107776587, 49.13393115100078745, -7.208316651077762316 ) ) ;
#17697 = LINE ( 'NONE', #79162, #55343 ) ;
#17698 = CARTESIAN_POINT ( 'NONE',  ( 7.964842623401177768, -33.81131465584515894, -7.964842623401181321 ) ) ;
#17699 = CARTESIAN_POINT ( 'NONE',  ( 21.09922568453595559, 12.04030133659708746, -6.408140936763230044 ) ) ;
#17700 = AXIS2_PLACEMENT_3D ( 'NONE', #13190, #43683, #59176 ) ;
#17702 = CARTESIAN_POINT ( 'NONE',  ( 1.383448333479232906, 67.37718327197430312, -6.499999999999977796 ) ) ;
#17701 = CARTESIAN_POINT ( 'NONE',  ( 17.96484262340118221, 11.18868534415484106, -7.964842623401177768 ) ) ;
#17703 = CARTESIAN_POINT ( 'NONE',  ( 2.618367889266248100E-15, 44.99999999999999289, -7.000000000000000000 ) ) ;
#17704 = CARTESIAN_POINT ( 'NONE',  ( 22.26659068614895176, 34.72041550158063927, -7.082119434687042414 ) ) ;
#17705 = CARTESIAN_POINT ( 'NONE',  ( 20.36894250292379738, 34.92874883491396076, -10.36894250292379027 ) ) ;
#17706 = CARTESIAN_POINT ( 'NONE',  ( 2.917880565312948704, 57.63708216824731068, 12.26659068614894643 ) ) ;
#17707 = CARTESIAN_POINT ( 'NONE',  ( -2.816281873526471635, 38.91530133659708213, -3.434112377981056508 ) ) ;
#17708 = CARTESIAN_POINT ( 'NONE',  ( -0.8801773607111009756, 8.063685344154837509, 1.068504757029289695E-15 ) ) ;
#17709 = ORIENTED_EDGE ( 'NONE', *, *, #37974, .F. ) ;
#17710 = CARTESIAN_POINT ( 'NONE',  ( 0.1532563361054082862, 41.21726448433411605, 2.638427012816831674 ) ) ;
#17711 = CARTESIAN_POINT ( 'NONE',  ( 7.084665262690076126, 47.02201867748818387, -10.88017736071110164 ) ) ;
#17712 = CARTESIAN_POINT ( 'NONE',  ( 12.63842701281683034, 62.46726448433410894, 9.846743663894596210 ) ) ;
#17714 = CARTESIAN_POINT ( 'NONE',  ( -39.69000000000001194, 92.00000000000000000, -10.09898361729590199 ) ) ;
#17713 = CARTESIAN_POINT ( 'NONE',  ( 22.26659068614894466, 18.88708216824730002, 7.082119434687054849 ) ) ;
#17715 = CARTESIAN_POINT ( 'NONE',  ( 18.39792806157249672, 34.52224192338640307, 6.500000000000000888 ) ) ;
#17716 = CARTESIAN_POINT ( 'NONE',  ( 0.1532563361054100626, 25.80059781766744820, -2.638427012816831230 ) ) ;
#17717 = CARTESIAN_POINT ( 'NONE',  ( 16.40814093676324603, 47.45696800326375353, -11.09922568453594671 ) ) ;
#17718 = CARTESIAN_POINT ( 'NONE',  ( 19.84674366389459266, 48.71726448433413026, -2.638427012816827677 ) ) ;
#17719 = ORIENTED_EDGE ( 'NONE', *, *, #28572, .F. ) ;
#17720 = DIRECTION ( 'NONE',  ( -1.000000000000000000, -2.569960705150826877E-16, 0.000000000000000000 ) ) ;
#17721 = CARTESIAN_POINT ( 'NONE',  ( 17.08211943468705840, 65.13708216824730357, -12.26659068614894466 ) ) ;
#17722 = CARTESIAN_POINT ( 'NONE',  ( 19.42250999205614193, 60.14701867748817676, 5.440088680355555262 ) ) ;
#17723 = CARTESIAN_POINT ( 'NONE',  ( 24.16423886937410614, 14.51208216824730179, -3.795296366450302550 ) ) ;
#17724 = CARTESIAN_POINT ( 'NONE',  ( 1.472469842513823179, 1.425597817667451528, 4.923371831947296329 ) ) ;
#17725 = CARTESIAN_POINT ( 'NONE',  ( 7.361572987183170547, 47.05059781766745175, 9.846743663894590881 ) ) ;
#17726 = CARTESIAN_POINT ( 'NONE',  ( 20.88017736071110519, 20.56368534415484106, 2.639326808657452039E-16 ) ) ;
#17727 = CARTESIAN_POINT ( 'NONE',  ( -7.640985187756077046, 14.95037103177797633, -12.62032702733663392 ) ) ;
#17728 = CARTESIAN_POINT ( 'NONE',  ( 2.791683348922240793, 61.63393115100079456, 7.208316651077764092 ) ) ;
#17729 = CIRCLE ( 'NONE', #59172, 15.00000000000000000 ) ;
#17730 = EDGE_CURVE ( 'NONE', #28561, #56172, #25035, .T. ) ;
#17731 = CARTESIAN_POINT ( 'NONE',  ( -8.209432707284987529, 14.63606883728482622, 12.55409154915482972 ) ) ;
#17732 = EDGE_LOOP ( 'NONE', ( #98471, #85004, #60041, #35568 ) ) ;
#17733 = ORIENTED_EDGE ( 'NONE', *, *, #95494, .F. ) ;
#17734 = CARTESIAN_POINT ( 'NONE',  ( -27.43587634952537968, 11.50000000000000000, -9.500000000000000000 ) ) ;
#17735 = CARTESIAN_POINT ( 'NONE',  ( -18.89999999999999147, 91.25000000000000000, -8.000000000000000000 ) ) ;
#17736 =( NAMED_UNIT ( * ) PLANE_ANGLE_UNIT ( ) SI_UNIT ( $, .RADIAN. ) );
#17737 = CARTESIAN_POINT ( 'NONE',  ( 19.84674366389459266, 63.71726448433412315, -2.638427012816827677 ) ) ;
#17738 = CARTESIAN_POINT ( 'NONE',  ( 2.791683348922240793, 21.63393115100078745, 7.208316651077764092 ) ) ;
#17740 = CARTESIAN_POINT ( 'NONE',  ( 1.472469842513823179, 60.59226448433412315, -4.923371831947296329 ) ) ;
#17739 = CARTESIAN_POINT ( 'NONE',  ( 20.88017736071110519, 20.56368534415484106, 2.639326808657452039E-16 ) ) ;
#17741 = DIRECTION ( 'NONE',  ( -1.000000000000000000, 0.000000000000000000, 0.000000000000000000 ) ) ;
#17742 = CARTESIAN_POINT ( 'NONE',  ( 24.16423886937409904, 39.09541550158062506, 3.795296366450317205 ) ) ;
#17743 = CARTESIAN_POINT ( 'NONE',  ( 17.08211943468705840, 65.13708216824730357, -12.26659068614894466 ) ) ;
#17744 = CARTESIAN_POINT ( 'NONE',  ( 1.472469842513823179, 66.42559781766745175, 4.923371831947296329 ) ) ;
#17745 = DIRECTION ( 'NONE',  ( -1.000000000000000000, 0.000000000000000000, 0.000000000000000000 ) ) ;
#17746 = CARTESIAN_POINT ( 'NONE',  ( 4.559911319644449179, 68.89701867748817676, 9.422509992056141925 ) ) ;
#17747 = CARTESIAN_POINT ( 'NONE',  ( 1.472469842513823179, 11.42559781766745175, 4.923371831947296329 ) ) ;
#17748 = CARTESIAN_POINT ( 'NONE',  ( 20.15039907845753220, 61.74884699246888431, 6.262539305110078836 ) ) ;
#17749 = ORIENTED_EDGE ( 'NONE', *, *, #49339, .F. ) ;
#17750 = CARTESIAN_POINT ( 'NONE',  ( -1.354709868695428421, 0.3639309939382821546, -14.93870011653156915 ) ) ;
#17751 =( BOUNDED_CURVE ( )  B_SPLINE_CURVE ( 2, ( #87339, #27319, #81795, #12327, #88325, #88817, #42831, #81317, #4840, #36313, #41859 ),
 .UNSPECIFIED., .F., .T. ) 
 B_SPLINE_CURVE_WITH_KNOTS ( ( 3, 2, 2, 2, 2, 3 ),
 ( 0.6666666666666667407, 0.6722222222222223875, 0.6777777777777779233, 0.6833333333333333481, 0.6888888888888888840, 0.6902146981917277602 ),
 .UNSPECIFIED. ) 
 CURVE ( )  GEOMETRIC_REPRESENTATION_ITEM ( )  RATIONAL_B_SPLINE_CURVE ( ( 0.9999999999999993339, 0.9659258262890688673, 1.000000000000000000, 0.9659258262890682012, 1.000000000000000000, 0.9659258262890682012, 1.000000000000000000, 0.9659258262890682012, 1.000000000000000000, 0.9918683458313497514, 0.9876178598506348827 ) ) 
 REPRESENTATION_ITEM ( '' )  );
#17752 = ORIENTED_EDGE ( 'NONE', *, *, #8025, .T. ) ;
#17753 = COLOUR_RGB ( '', 0.09019608, 0.27058824, 0.51372549) ;
#17754 = CARTESIAN_POINT ( 'NONE',  ( 7.361572987183169658, 24.96726448433412315, -9.846743663894592657 ) ) ;
#17755 = ORIENTED_EDGE ( 'NONE', *, *, #21925, .T. ) ;
#17756 = CARTESIAN_POINT ( 'NONE',  ( -4.164238869374099039, 31.80374883491396432, 8.674139862899312516E-16 ) ) ;
#17757 = CARTESIAN_POINT ( 'NONE',  ( 18.52753015748618282, 38.92559781766745175, -4.923371831947291888 ) ) ;
#17758 = CARTESIAN_POINT ( 'NONE',  ( 4.559911319644449179, 38.89701867748817676, 9.422509992056141925 ) ) ;
#17759 = ORIENTED_EDGE ( 'NONE', *, *, #45045, .F. ) ;
#17760 =( BOUNDED_CURVE ( )  B_SPLINE_CURVE ( 2, ( #10186, #40680, #93172, #84703, #70690, #32669, #79157, #25204, #71180 ),
 .UNSPECIFIED., .F., .T. ) 
 B_SPLINE_CURVE_WITH_KNOTS ( ( 3, 2, 2, 2, 3 ),
 ( 0.08299807979737425234, 0.08333333333333337034, 0.08928571428571430157, 0.09523809523809523281, 0.09557334877405435081 ),
 .UNSPECIFIED. ) 
 CURVE ( )  GEOMETRIC_REPRESENTATION_ITEM ( )  RATIONAL_B_SPLINE_CURVE ( ( 0.9963778908391762723, 0.9980808541467921513, 1.000000000000000000, 0.9659258262890682012, 1.000000000000000000, 0.9659258262890682012, 1.000000000000000000, 0.9980808541467921513, 0.9963778908391762723 ) ) 
 REPRESENTATION_ITEM ( '' )  );
#17761 = CARTESIAN_POINT ( 'NONE',  ( 10.00000000000000178, 44.31368534415484106, 10.88017736071110342 ) ) ;
#17762 = EDGE_CURVE ( 'NONE', #10214, #4322, #13809, .T. ) ;
#17763 = CARTESIAN_POINT ( 'NONE',  ( 9.382169495545415572, -7.751365330069575954, -9.382169495545422677 ) ) ;
#17764 = ADVANCED_FACE ( 'NONE', ( #65306 ), #50308, .T. ) ;
#17765 = ORIENTED_EDGE ( 'NONE', *, *, #50585, .F. ) ;
#17766 = VECTOR ( 'NONE', #6273, 1000.000000000000000 ) ;
#17767 = CARTESIAN_POINT ( 'NONE',  ( -4.164238869374099927, 12.01208216824730357, 3.795296366450308767 ) ) ;
#17768 = ORIENTED_EDGE ( 'NONE', *, *, #505, .T. ) ;
#17769 = ORIENTED_EDGE ( 'NONE', *, *, #57907, .F. ) ;
#17770 = CARTESIAN_POINT ( 'NONE',  ( 0.6178305044545818747, 28.49863466993041783, -9.382169495545419124 ) ) ;
#17771 = CARTESIAN_POINT ( 'NONE',  ( 19.84674366389459266, 28.30059781766745886, 2.638427012816836559 ) ) ;
#17772 = CARTESIAN_POINT ( 'NONE',  ( 6.382347221874334231, 0.5000000000000004441, 13.57444820018231724 ) ) ;
#17773 = CARTESIAN_POINT ( 'NONE',  ( -8.375939845167836850, -0.03417435944610275333, 11.52849216984293257 ) ) ;
#17774 = CARTESIAN_POINT ( 'NONE',  ( 12.63842701281683034, 27.46726448433411250, 9.846743663894596210 ) ) ;
#17775 = CARTESIAN_POINT ( 'NONE',  ( 12.91533473730992121, 54.52201867748816255, 10.88017736071110164 ) ) ;
#17776 = CARTESIAN_POINT ( 'NONE',  ( 2.377183314879994125, 45.78593319516822646, -6.500000000000057732 ) ) ;
#17777 = LINE ( 'NONE', #33247, #37091 ) ;
#17778 = LINE ( 'NONE', #79250, #62745 ) ;
#17779 = EDGE_CURVE ( 'NONE', #62008, #94783, #10596, .T. ) ;
#17780 = CARTESIAN_POINT ( 'NONE',  ( -2.816281873526473856, 64.33196800326376774, 3.434112377981055619 ) ) ;
#17781 = CARTESIAN_POINT ( 'NONE',  ( 14.92337183194729633, 7.675597817667451750, 8.527530157486181039 ) ) ;
#17782 = CARTESIAN_POINT ( 'NONE',  ( -2.816281873526473856, 9.331968003263753531, 3.434112377981055619 ) ) ;
#17783 = CARTESIAN_POINT ( 'NONE',  ( -26.69000000000001194, 92.00000000000000000, 9.500000000000000000 ) ) ;
#17784 = CARTESIAN_POINT ( 'NONE',  ( 17.20831665107776587, 49.13393115100078745, -7.208316651077762316 ) ) ;
#17785 = LINE ( 'NONE', #26740, #60113 ) ;
#17786 = CARTESIAN_POINT ( 'NONE',  ( -2.266590686148945544, 7.220415501580634832, 7.082119434687048631 ) ) ;
#17787 = CARTESIAN_POINT ( 'NONE',  ( 7.361572987183170547, 17.05059781766745530, 9.846743663894590881 ) ) ;
#17788 = CARTESIAN_POINT ( 'NONE',  ( 0.6178305044545838731, 39.74863466993041072, 9.382169495545420901 ) ) ;
#17790 = LINE ( 'NONE', #86281, #41736 ) ;
#17789 = SURFACE_STYLE_FILL_AREA ( #47278 ) ;
#17791 = CARTESIAN_POINT ( 'NONE',  ( 19.42250999205614548, 45.98035201082150536, -5.440088680355545492 ) ) ;
#17792 = CARTESIAN_POINT ( 'NONE',  ( 6.565887622018943937, 8.081968003263751754, -12.81628187352647608 ) ) ;
#17793 = CARTESIAN_POINT ( 'NONE',  ( 13.48255862862752430, 15.00000000000000000, -5.335786055104087211 ) ) ;
#17794 = CARTESIAN_POINT ( 'NONE',  ( 10.00000000000000178, 17.25893115100078745, 9.846743663894594434 ) ) ;
#17795 = CARTESIAN_POINT ( 'NONE',  ( 7.084665262690076126, 27.02201867748817676, -10.88017736071110164 ) ) ;
#17796 = CARTESIAN_POINT ( 'NONE',  ( 10.00000000000000178, 35.37363466993042493, 12.81628187352647608 ) ) ;
#17797 = CARTESIAN_POINT ( 'NONE',  ( 10.00000000000000000, 19.75893115100078390, -9.846743663894594434 ) ) ;
#17798 = LINE ( 'NONE', #78286, #51864 ) ;
#17799 = CIRCLE ( 'NONE', #22657, 0.2500000000000002220 ) ;
#17800 = CARTESIAN_POINT ( 'NONE',  ( 19.42250999205614193, 20.14701867748817321, 5.440088680355555262 ) ) ;
#17801 = CARTESIAN_POINT ( 'NONE',  ( 12.91533473730993009, 66.60535201082150536, -10.88017736071109987 ) ) ;
#17802 = SURFACE_SIDE_STYLE ('',( #94769 ) ) ;
#17804 = CARTESIAN_POINT ( 'NONE',  ( 19.42250999205614193, 20.14701867748817321, 5.440088680355555262 ) ) ;
#17803 = CARTESIAN_POINT ( 'NONE',  ( 17.20831665107776587, 42.88393115100077324, 7.208316651077764980 ) ) ;
#17805 = CARTESIAN_POINT ( 'NONE',  ( 19.42250999205614193, 45.14701867748817676, 5.440088680355555262 ) ) ;
#17806 = CARTESIAN_POINT ( 'NONE',  ( 19.42250999205614548, 10.98035201082150536, -5.440088680355545492 ) ) ;
#17807 = CARTESIAN_POINT ( 'NONE',  ( 14.92337183194729633, 32.67559781766745175, 8.527530157486181039 ) ) ;
#17808 = DIRECTION ( 'NONE',  ( -1.000000000000000000, -2.653152395358074805E-16, -0.000000000000000000 ) ) ;
#17809 = CARTESIAN_POINT ( 'NONE',  ( 3.969999999999999751, 36.75000000000000000, -2.750000000000000000 ) ) ;
#17810 = CARTESIAN_POINT ( 'NONE',  ( 21.09922568453594849, 6.206968003263753531, 6.408140936763242479 ) ) ;
#17811 = LINE ( 'NONE', #26280, #90681 ) ;
#17813 = CARTESIAN_POINT ( 'NONE',  ( 24.16423886937410614, 19.30374883491397142, 8.672049930838204340E-16 ) ) ;
#17812 =( BOUNDED_CURVE ( )  B_SPLINE_CURVE ( 2, ( #46914, #45953, #39438, #53938, #45443, #76440, #69932, #8437, #69432 ),
 .UNSPECIFIED., .F., .F. ) 
 B_SPLINE_CURVE_WITH_KNOTS ( ( 3, 2, 2, 2, 3 ),
 ( 0.5817427861304426129, 0.5833333333333333703, 0.5888888888888889062, 0.5944444444444444420, 0.5999999999999999778 ),
 .UNSPECIFIED. ) 
 CURVE ( )  GEOMETRIC_REPRESENTATION_ITEM ( )  RATIONAL_B_SPLINE_CURVE ( ( 0.9860751345400187162, 0.9902446152963877424, 1.000000000000000000, 0.9659258262890684232, 1.000000000000000000, 0.9659258262890684232, 1.000000000000000000, 0.9659258262890684232, 1.000000000000000000 ) ) 
 REPRESENTATION_ITEM ( '' )  );
#17814 = CIRCLE ( 'NONE', #56145, 2.250000000000001332 ) ;
#17815 = LINE ( 'NONE', #69837, #59235 ) ;
#17816 = CARTESIAN_POINT ( 'NONE',  ( 20.36894250292379738, 64.92874883491397497, -10.36894250292379027 ) ) ;
#17817 = CARTESIAN_POINT ( 'NONE',  ( 1.472469842513823179, 26.42559781766745175, 4.923371831947296329 ) ) ;
#17819 = CARTESIAN_POINT ( 'NONE',  ( -8.636324037029986300, 86.94567068113131825, -4.522730969307667159 ) ) ;
#17818 = LINE ( 'NONE', #48300, #14846 ) ;
#17820 = CARTESIAN_POINT ( 'NONE',  ( 7.084665262690076126, 47.02201867748818387, -10.88017736071110164 ) ) ;
#17821 = CARTESIAN_POINT ( 'NONE',  ( 3.591859063236763294, 58.29030133659708923, -11.09922568453595026 ) ) ;
#17822 = CARTESIAN_POINT ( 'NONE',  ( 7.084665262690076126, 29.10535201082150181, 10.88017736071109987 ) ) ;
#17823 = AXIS2_PLACEMENT_3D ( 'NONE', #27536, #96052, #97055 ) ;
#17824 = CARTESIAN_POINT ( 'NONE',  ( 10.00000000000000178, 70.00000000000000000, 0.000000000000000000 ) ) ;
#17825 = CARTESIAN_POINT ( 'NONE',  ( 3.591859063236761518, 14.95696800326375531, 11.09922568453594849 ) ) ;
#17826 = CARTESIAN_POINT ( 'NONE',  ( 7.361572987183169658, 14.96726448433411960, -9.846743663894592657 ) ) ;
#17827 = ORIENTED_EDGE ( 'NONE', *, *, #28143, .T. ) ;
#17828 = DIRECTION ( 'NONE',  ( -0.9426414910921759871, 0.000000000000000000, -0.3338068592337775642 ) ) ;
#17829 = CARTESIAN_POINT ( 'NONE',  ( 6.204703633549690345, 57.84541550158063927, 14.16423886937410082 ) ) ;
#17830 = CARTESIAN_POINT ( 'NONE',  ( -2.266590686148945544, 22.22041550158063572, 7.082119434687048631 ) ) ;
#17831 = CARTESIAN_POINT ( 'NONE',  ( -0.8801773607111008646, 13.27201867748817143, 2.915334737309923430 ) ) ;
#17832 = CARTESIAN_POINT ( 'NONE',  ( 19.42250999205614548, 55.98035201082150536, -5.440088680355545492 ) ) ;
#17833 = SURFACE_STYLE_USAGE ( .BOTH. , #62829 ) ;
#17834 = CARTESIAN_POINT ( 'NONE',  ( 8.630000000000000782, 1.019547802438458550, -4.000000000000000000 ) ) ;
#17835 = CARTESIAN_POINT ( 'NONE',  ( 1.472469842513823179, 16.42559781766745175, 4.923371831947296329 ) ) ;
#17836 = DIRECTION ( 'NONE',  ( 1.000000000000000000, 0.000000000000000000, 0.000000000000000000 ) ) ;
#17837 = CARTESIAN_POINT ( 'NONE',  ( 10.00000000000000178, 22.25893115100078745, 9.846743663894594434 ) ) ;
#17838 = CARTESIAN_POINT ( 'NONE',  ( 7.551349515323185990, 15.00000000000000000, -12.08468537022906020 ) ) ;
#17839 = CARTESIAN_POINT ( 'NONE',  ( 10.00000000000000000, 29.75893115100078745, -9.846743663894594434 ) ) ;
#17840 = CARTESIAN_POINT ( 'NONE',  ( 14.92337183194729988, 44.34226448433412315, -8.527530157486177487 ) ) ;
#17841 = EDGE_CURVE ( 'NONE', #59148, #79187, #70926, .T. ) ;
#17842 = CARTESIAN_POINT ( 'NONE',  ( 7.084665262690076126, 24.10535201082150181, 10.88017736071109987 ) ) ;
#17843 = CARTESIAN_POINT ( 'NONE',  ( 22.81628187352647785, 36.62363466993041783, 6.195893100308588602E-16 ) ) ;
#17844 = CARTESIAN_POINT ( 'NONE',  ( 19.42250999205614548, 50.98035201082151247, -5.440088680355545492 ) ) ;
#17845 = CARTESIAN_POINT ( 'NONE',  ( 19.84674366389459266, 23.71726448433412315, -2.638427012816827677 ) ) ;
#17847 = CARTESIAN_POINT ( 'NONE',  ( 18.52753015748618282, 28.92559781766745175, -4.923371831947291888 ) ) ;
#17846 = CARTESIAN_POINT ( 'NONE',  ( -4.164238869374099927, 42.01208216824728936, 3.795296366450308767 ) ) ;
#17848 = CARTESIAN_POINT ( 'NONE',  ( 11.10000000000000142, 98.49999999999998579, -8.525133428036873795 ) ) ;
#17849 = CARTESIAN_POINT ( 'NONE',  ( 7.361572987183170547, 52.05059781766745175, 9.846743663894590881 ) ) ;
#17851 = CARTESIAN_POINT ( 'NONE',  ( 22.26659068614894466, 8.887082168247300018, 7.082119434687054849 ) ) ;
#17850 = CARTESIAN_POINT ( 'NONE',  ( 12.63842701281683034, 27.46726448433411250, 9.846743663894596210 ) ) ;
#17852 = CARTESIAN_POINT ( 'NONE',  ( 2.917880565312948704, 12.63708216824730179, 12.26659068614894643 ) ) ;
#17853 = CARTESIAN_POINT ( 'NONE',  ( 5.076628168052704559, 30.17559781766745175, -8.527530157486179263 ) ) ;
#17854 = CARTESIAN_POINT ( 'NONE',  ( 20.88017736071110519, 45.56368534415484106, 2.639326808657452039E-16 ) ) ;
#17855 = CARTESIAN_POINT ( 'NONE',  ( -0.8801773607111009756, 23.06368534415484106, 1.068504757029289695E-15 ) ) ;
#17856 = CARTESIAN_POINT ( 'NONE',  ( 4.559911319644449179, 38.89701867748817676, 9.422509992056141925 ) ) ;
#17857 = CARTESIAN_POINT ( 'NONE',  ( 7.084665262690076126, 24.10535201082150181, 10.88017736071109987 ) ) ;
#17858 = ORIENTED_EDGE ( 'NONE', *, *, #82331, .T. ) ;
#17859 = CARTESIAN_POINT ( 'NONE',  ( 17.96484262340118221, 56.18868534415484817, -7.964842623401177768 ) ) ;
#17860 = ORIENTED_EDGE ( 'NONE', *, *, #18879, .F. ) ;
#17861 = SURFACE_STYLE_FILL_AREA ( #42333 ) ;
#17862 = CARTESIAN_POINT ( 'NONE',  ( 15.44008868035555793, 66.39701867748817676, -9.422509992056140149 ) ) ;
#17863 = B_SPLINE_CURVE_WITH_KNOTS ( 'NONE', 3,
 ( #83003, #52015, #44502, #21026, #51515, #67510 ),
 .UNSPECIFIED., .F., .F.,
 ( 4, 2, 4 ),
 ( 3.409110551496135434E-05, 0.0004400426677367878184, 0.0008459942299586143029 ),
 .UNSPECIFIED. ) ;
#17864 = ORIENTED_EDGE ( 'NONE', *, *, #78014, .F. ) ;
#17865 = CARTESIAN_POINT ( 'NONE',  ( 20.88017736071110875, 65.77201867748817676, -2.915334737309920765 ) ) ;
#17866 = AXIS2_PLACEMENT_3D ( 'NONE', #85251, #49206, #79214 ) ;
#17867 = EDGE_CURVE ( 'NONE', #75287, #49705, #9023, .T. ) ;
#17868 = DIRECTION ( 'NONE',  ( 1.000000000000000000, 0.000000000000000000, 0.000000000000000000 ) ) ;
#17869 = DIRECTION ( 'NONE',  ( -0.6755902076156541369, 0.000000000000000000, -0.7372773368101296354 ) ) ;
#17870 = CARTESIAN_POINT ( 'NONE',  ( 24.16423886937409904, 64.09541550158064638, 3.795296366450317205 ) ) ;
#17871 = CARTESIAN_POINT ( 'NONE',  ( 12.63842701281683034, 12.46726448433411782, 9.846743663894596210 ) ) ;
#17872 =( NAMED_UNIT ( * ) SI_UNIT ( $, .STERADIAN. ) SOLID_ANGLE_UNIT ( ) );
#17873 = EDGE_CURVE ( 'NONE', #93548, #10214, #23300, .T. ) ;
#17874 = CARTESIAN_POINT ( 'NONE',  ( 5.076628168052703671, 6.842264484334118713, 8.527530157486179263 ) ) ;
#17875 = CARTESIAN_POINT ( 'NONE',  ( 2.035157376598824452, 8.688685344154839285, 7.964842623401179544 ) ) ;
#17876 = CARTESIAN_POINT ( 'NONE',  ( 14.92337183194729633, 47.67559781766745175, 8.527530157486181039 ) ) ;
#17877 = ORIENTED_EDGE ( 'NONE', *, *, #44488, .T. ) ;
#17878 = CARTESIAN_POINT ( 'NONE',  ( 12.63842701281683922, 44.55059781766745175, -9.846743663894590881 ) ) ;
#17879 = VERTEX_POINT ( 'NONE', #804 ) ;
#17880 = CARTESIAN_POINT ( 'NONE',  ( 17.85158348494331904, 29.73726573380435667, -6.499999999999992895 ) ) ;
#17881 = CARTESIAN_POINT ( 'NONE',  ( 2.035157376598822676, 57.43868534415484106, -7.964842623401177768 ) ) ;
#17882 = CARTESIAN_POINT ( 'NONE',  ( 1.472469842513823179, 46.42559781766745175, 4.923371831947296329 ) ) ;
#17884 = CARTESIAN_POINT ( 'NONE',  ( 2.035157376598822676, 67.43868534415484817, -7.964842623401177768 ) ) ;
#17883 = CARTESIAN_POINT ( 'NONE',  ( -14.02068044289382875, 0.5000000000000004441, 5.331089937175565119 ) ) ;
#17885 = CARTESIAN_POINT ( 'NONE',  ( 10.00000000000000178, 59.31368534415484106, 10.88017736071110342 ) ) ;
#17886 = CARTESIAN_POINT ( 'NONE',  ( 10.00000000000000178, 68.05374883491397497, 14.16423886937410082 ) ) ;
#17887 = CIRCLE ( 'NONE', #78629, 15.00000000000000000 ) ;
#17888 = CIRCLE ( 'NONE', #89683, 15.00000000000000000 ) ;
#17889 = CARTESIAN_POINT ( 'NONE',  ( -2.816281873526473856, 39.12363466993041783, 9.499525473075851096E-16 ) ) ;
#17890 = EDGE_LOOP ( 'NONE', ( #22801, #7299, #65119, #43073, #9129, #6026 ) ) ;
#17891 = CARTESIAN_POINT ( 'NONE',  ( 6.565887622018943937, 25.16530133659708213, 12.81628187352647430 ) ) ;
#17892 = CARTESIAN_POINT ( 'NONE',  ( 4.559911319644449179, 28.89701867748817321, 9.422509992056141925 ) ) ;
#17893 = AXIS2_PLACEMENT_3D ( 'NONE', #82302, #72828, #73325 ) ;
#17894 = ORIENTED_EDGE ( 'NONE', *, *, #543, .F. ) ;
#17895 = EDGE_CURVE ( 'NONE', #88123, #62008, #39283, .T. ) ;
#17896 = CARTESIAN_POINT ( 'NONE',  ( 17.96484262340118221, 66.18868534415483396, -7.964842623401177768 ) ) ;
#17897 = VECTOR ( 'NONE', #68488, 1000.000000000000227 ) ;
#17898 = CARTESIAN_POINT ( 'NONE',  ( 5.076628168052704559, 60.17559781766745175, -8.527530157486179263 ) ) ;
#17900 = CARTESIAN_POINT ( 'NONE',  ( 2.791683348922240793, 41.63393115100078745, 7.208316651077764092 ) ) ;
#17899 = CARTESIAN_POINT ( 'NONE',  ( 0.1532563361054100626, 15.80059781766745353, -2.638427012816831230 ) ) ;
#17901 = CARTESIAN_POINT ( 'NONE',  ( -11.16113486365330587, -52.93448945038705489, 3.750000000000000444 ) ) ;
#17902 = CARTESIAN_POINT ( 'NONE',  ( 19.05914839598885635, 14.96693863883975872, 6.499999999999962697 ) ) ;
#17903 = CARTESIAN_POINT ( 'NONE',  ( 19.84674366389459266, 38.30059781766745175, 2.638427012816836559 ) ) ;
#17904 = CARTESIAN_POINT ( 'NONE',  ( 0.000000000000000000, 0.5000000000000004441, 0.000000000000000000 ) ) ;
#17905 = CARTESIAN_POINT ( 'NONE',  ( 13.21236992757670059, 15.00000000000000000, 5.338143956176803151 ) ) ;
#17906 = EDGE_CURVE ( 'NONE', #94698, #21605, #66468, .T. ) ;
#17907 = CARTESIAN_POINT ( 'NONE',  ( 14.92337183194729988, 29.34226448433411960, -8.527530157486177487 ) ) ;
#17908 = FACE_OUTER_BOUND ( 'NONE', #50832, .T. ) ;
#17910 = ORIENTED_EDGE ( 'NONE', *, *, #14111, .T. ) ;
#17909 = CARTESIAN_POINT ( 'NONE',  ( 1.472469842513823179, 41.42559781766745886, 4.923371831947296329 ) ) ;
#17911 = SURFACE_STYLE_FILL_AREA ( #40425 ) ;
#17912 = CARTESIAN_POINT ( 'NONE',  ( -2.816281873526473856, 19.12363466993042138, 9.499525473075851096E-16 ) ) ;
#17913 = CARTESIAN_POINT ( 'NONE',  ( 10.00000000000000000, 49.75893115100078745, -9.846743663894594434 ) ) ;
#17914 = DIRECTION ( 'NONE',  ( -0.000000000000000000, -0.000000000000000000, 1.000000000000000000 ) ) ;
#17915 = CARTESIAN_POINT ( 'NONE',  ( 22.26659068614895176, 44.72041550158063927, -7.082119434687042414 ) ) ;
#17916 = CARTESIAN_POINT ( 'NONE',  ( 18.52753015748617571, 13.09226448433411960, 4.923371831947298993 ) ) ;
#17917 = ORIENTED_EDGE ( 'NONE', *, *, #80043, .F. ) ;
#17918 = CARTESIAN_POINT ( 'NONE',  ( 0.1532563361054083140, 6.008931151000784787, 1.131784320476157264E-15 ) ) ;
#17919 = CARTESIAN_POINT ( 'NONE',  ( -13.75801628063885040, 4.154966894009843400E-16, 4.578972376164368363 ) ) ;
#17920 = CARTESIAN_POINT ( 'NONE',  ( 13.79529636645031943, 45.34541550158062506, -14.16423886937409904 ) ) ;
#17921 = CARTESIAN_POINT ( 'NONE',  ( 12.63842701281683034, 62.46726448433410894, 9.846743663894596210 ) ) ;
#17922 = CARTESIAN_POINT ( 'NONE',  ( 2.035157376598822676, 2.438685344154838397, -7.964842623401177768 ) ) ;
#17923 = CARTESIAN_POINT ( 'NONE',  ( 22.26659068614894466, 23.88708216824730357, 7.082119434687054849 ) ) ;
#17924 = CARTESIAN_POINT ( 'NONE',  ( 6.204703633549690345, 42.84541550158063217, 14.16423886937410082 ) ) ;
#17925 = FACE_OUTER_BOUND ( 'NONE', #57915, .T. ) ;
#17927 = CARTESIAN_POINT ( 'NONE',  ( 19.84674366389459621, 58.50893115100078745, 7.409399052514197653E-17 ) ) ;
#17926 = LINE ( 'NONE', #19882, #13318 ) ;
#17928 = ORIENTED_EDGE ( 'NONE', *, *, #5887, .T. ) ;
#17929 = CARTESIAN_POINT ( 'NONE',  ( 15.44008868035555793, 36.39701867748816966, -9.422509992056140149 ) ) ;
#17930 = CARTESIAN_POINT ( 'NONE',  ( 3.836325488036183451, 0.5000000000000004441, -14.50112432709422627 ) ) ;
#17931 = CARTESIAN_POINT ( 'NONE',  ( 20.00000000000000355, 95.46878211396317226, -5.047406989011700595 ) ) ;
#17932 = DIRECTION ( 'NONE',  ( 0.000000000000000000, -1.000000000000000000, 0.000000000000000000 ) ) ;
#17933 = CARTESIAN_POINT ( 'NONE',  ( -3.795296366450300773, 12.84541550158064283, 14.16423886937410437 ) ) ;
#17934 = CARTESIAN_POINT ( 'NONE',  ( 0.1532563361054100626, 50.80059781766745175, -2.638427012816831230 ) ) ;
#17935 = CARTESIAN_POINT ( 'NONE',  ( 12.63842701281683034, 62.46726448433410894, 9.846743663894596210 ) ) ;
#17936 = AXIS2_PLACEMENT_3D ( 'NONE', #76421, #8899, #62381 ) ;
#17937 = ORIENTED_EDGE ( 'NONE', *, *, #90627, .F. ) ;
#17938 = CARTESIAN_POINT ( 'NONE',  ( -4.164238869374099927, 22.01208216824730357, 3.795296366450308767 ) ) ;
#17939 = CARTESIAN_POINT ( 'NONE',  ( -19.00000000000000000, 75.76920769491739804, 2.900000000000000355 ) ) ;
#17940 = CARTESIAN_POINT ( 'NONE',  ( -5.328486666281219364, -28.65465727419595510, -2.500000000001614264 ) ) ;
#17941 = CARTESIAN_POINT ( 'NONE',  ( 20.88017736071110164, 10.35535201082150714, 2.915334737309930979 ) ) ;
#17942 = CARTESIAN_POINT ( 'NONE',  ( 0.6178305044545818747, 23.49863466993041783, -9.382169495545419124 ) ) ;
#17943 =( NAMED_UNIT ( * ) SI_UNIT ( $, .STERADIAN. ) SOLID_ANGLE_UNIT ( ) );
#17944 = CARTESIAN_POINT ( 'NONE',  ( 2.791683348922240793, 16.63393115100078745, 7.208316651077764092 ) ) ;
#17945 = CARTESIAN_POINT ( 'NONE',  ( 4.380000001274070520, 0.08775168531748565870, -4.000000000000000000 ) ) ;
#17946 = CARTESIAN_POINT ( 'NONE',  ( 0.1532563361054100626, 20.80059781766744820, -2.638427012816831230 ) ) ;
#17947 = DIRECTION ( 'NONE',  ( 0.000000000000000000, 1.000000000000000000, 0.000000000000000000 ) ) ;
#17948 = CARTESIAN_POINT ( 'NONE',  ( 17.96484262340118221, 6.188685344154837509, -7.964842623401177768 ) ) ;
#17949 = FACE_OUTER_BOUND ( 'NONE', #62263, .T. ) ;
#17950 = PLANE ( 'NONE',  #20826 ) ;
#17951 = CARTESIAN_POINT ( 'NONE',  ( 12.91533473730993009, 31.60535201082150891, -10.88017736071109987 ) ) ;
#17952 = CARTESIAN_POINT ( 'NONE',  ( 0.5774900079438590739, 42.64701867748816966, -5.440088680355550821 ) ) ;
#17953 = CARTESIAN_POINT ( 'NONE',  ( 14.92337183194729988, 64.34226448433412315, -8.527530157486177487 ) ) ;
#17954 = CARTESIAN_POINT ( 'NONE',  ( 10.00000000000000000, 64.75893115100078035, -9.846743663894594434 ) ) ;
#17955 = CARTESIAN_POINT ( 'NONE',  ( -44.75051794150706286, 105.1827308279087703, -5.400450157393513528 ) ) ;
#17956 = CARTESIAN_POINT ( 'NONE',  ( 1.472469842513823179, 10.59226448433411782, -4.923371831947296329 ) ) ;
#17957 = ORIENTED_EDGE ( 'NONE', *, *, #1732, .F. ) ;
#17958 = CARTESIAN_POINT ( 'NONE',  ( 4.559911319644449179, 32.23035201082150536, -9.422509992056141925 ) ) ;
#17959 = EDGE_CURVE ( 'NONE', #90631, #8762, #48239, .T. ) ;
#17960 = CARTESIAN_POINT ( 'NONE',  ( 10.00000000000000000, 27.87363466993042138, -12.81628187352647608 ) ) ;
#17961 = DIRECTION ( 'NONE',  ( 2.569960705150826877E-16, -1.000000000000000000, 0.000000000000000000 ) ) ;
#17962 = VECTOR ( 'NONE', #26921, 1000.000000000000000 ) ;
#17963 = CARTESIAN_POINT ( 'NONE',  ( 14.92337183194729988, 59.34226448433412315, -8.527530157486177487 ) ) ;
#17964 = CARTESIAN_POINT ( 'NONE',  ( -0.8801773607111009756, 58.06368534415484106, 1.068504757029289695E-15 ) ) ;
#17965 = CARTESIAN_POINT ( 'NONE',  ( 2.791683348922240793, 6.633931151000785675, 7.208316651077764092 ) ) ;
#17966 = CARTESIAN_POINT ( 'NONE',  ( 3.591859063236761518, 34.95696800326375353, 11.09922568453594849 ) ) ;
#17967 = VECTOR ( 'NONE', #1809, 1000.000000000000000 ) ;
#17969 = CARTESIAN_POINT ( 'NONE',  ( 0.000000000000000000, 14.49999999999999822, 0.000000000000000000 ) ) ;
#17968 = CARTESIAN_POINT ( 'NONE',  ( 4.559911319644449179, 63.89701867748817676, 9.422509992056141925 ) ) ;
#17970 = VECTOR ( 'NONE', #89599, 1000.000000000000000 ) ;
#17971 = CARTESIAN_POINT ( 'NONE',  ( 13.43411237798106583, 62.66530133659708923, -12.81628187352647252 ) ) ;
#17972 = EDGE_LOOP ( 'NONE', ( #43303, #574, #59057, #95117 ) ) ;
#17973 = DIRECTION ( 'NONE',  ( 6.394884621840901673E-14, 0.000000000000000000, 1.000000000000000000 ) ) ;
#17974 = SURFACE_STYLE_FILL_AREA ( #79453 ) ;
#17975 = CARTESIAN_POINT ( 'NONE',  ( 10.00000000000000000, 62.87363466993042493, -12.81628187352647608 ) ) ;
#17976 = CARTESIAN_POINT ( 'NONE',  ( 12.63842701281683922, 14.55059781766744997, -9.846743663894590881 ) ) ;
#17977 = TOROIDAL_SURFACE ( 'NONE', #446, 14.49999999999999822, 0.5000000000000000000 ) ;
#17978 = CARTESIAN_POINT ( 'NONE',  ( 19.42250999205614193, 10.14701867748816966, 5.440088680355555262 ) ) ;
#17979 = CARTESIAN_POINT ( 'NONE',  ( 2.791683348922240793, 21.63393115100078745, 7.208316651077764092 ) ) ;
#17980 = CARTESIAN_POINT ( 'NONE',  ( 24.16423886937410614, 54.30374883491396787, 8.672049930838204340E-16 ) ) ;
#17981 = EDGE_LOOP ( 'NONE', ( #46384, #84413, #44549, #5794 ) ) ;
#17982 = AXIS2_PLACEMENT_3D ( 'NONE', #83361, #61827, #84359 ) ;
#17983 = CARTESIAN_POINT ( 'NONE',  ( 15.44008868035555793, 11.39701867748817143, -9.422509992056140149 ) ) ;
#17984 = CARTESIAN_POINT ( 'NONE',  ( 19.42250999205614193, 25.14701867748817321, 5.440088680355555262 ) ) ;
#17985 = CARTESIAN_POINT ( 'NONE',  ( -11.64999999999999680, 98.49999999999998579, -8.525133428036873795 ) ) ;
#17986 = CIRCLE ( 'NONE', #5214, 0.2500000000000002220 ) ;
#17987 = ORIENTED_EDGE ( 'NONE', *, *, #42164, .T. ) ;
#17988 = VERTEX_POINT ( 'NONE', #91779 ) ;
#17989 = CARTESIAN_POINT ( 'NONE',  ( 20.88017736071110519, 25.56368534415483751, 2.639326808657452039E-16 ) ) ;
#17990 = CARTESIAN_POINT ( 'NONE',  ( 12.63842701281683922, 59.55059781766744464, -9.846743663894590881 ) ) ;
#17991 = ADVANCED_FACE ( 'NONE', ( #84295 ), #2633, .T. ) ;
#17992 = CARTESIAN_POINT ( 'NONE',  ( 6.565887622018943937, 53.08196800326374643, -12.81628187352647608 ) ) ;
#17993 = CARTESIAN_POINT ( 'NONE',  ( 13.40508947812163143, 3.998652394537887614E-16, 5.527528931046191474 ) ) ;
#17994 = CARTESIAN_POINT ( 'NONE',  ( 24.16423886937409904, 24.09541550158063927, 3.795296366450317205 ) ) ;
#17995 = CARTESIAN_POINT ( 'NONE',  ( -0.8801773607111009756, 43.06368534415484106, 1.068504757029289695E-15 ) ) ;
#17996 = CARTESIAN_POINT ( 'NONE',  ( 19.42250999205614548, 15.98035201082150714, -5.440088680355545492 ) ) ;
#17997 = CARTESIAN_POINT ( 'NONE',  ( 18.52753015748617571, 58.09226448433411605, 4.923371831947298993 ) ) ;
#17998 = CARTESIAN_POINT ( 'NONE',  ( -8.000000000000000000, 1.019547802438458550, -3.750000000000000000 ) ) ;
#17999 = CARTESIAN_POINT ( 'NONE',  ( 0.1532563361054082862, 36.21726448433410894, 2.638427012816831674 ) ) ;
#18000 = EDGE_CURVE ( 'NONE', #91280, #15586, #71267, .T. ) ;
#18001 = DIRECTION ( 'NONE',  ( 0.000000000000000000, 0.000000000000000000, 1.000000000000000000 ) ) ;
#18002 = CARTESIAN_POINT ( 'NONE',  ( 17.20831665107776587, 4.133931151000785675, -7.208316651077762316 ) ) ;
#18003 = CARTESIAN_POINT ( 'NONE',  ( -9.382169495545422677, -31.50136533006957862, -9.382169495545417348 ) ) ;
#18004 = VERTEX_POINT ( 'NONE', #17271 ) ;
#18005 = CARTESIAN_POINT ( 'NONE',  ( 10.00000000000000000, 14.75893115100078568, -9.846743663894594434 ) ) ;
#18006 = CARTESIAN_POINT ( 'NONE',  ( 6.565887622018943937, 0.1653013365970866511, 12.81628187352647430 ) ) ;
#18008 = CARTESIAN_POINT ( 'NONE',  ( -0.8801773607111009756, 48.06368534415484817, 1.068504757029289695E-15 ) ) ;
#18007 = CARTESIAN_POINT ( 'NONE',  ( 20.88017736071110875, 45.77201867748816966, -2.915334737309920765 ) ) ;
#18010 = CARTESIAN_POINT ( 'NONE',  ( 19.38216949554541202, 45.99863466993041072, 9.382169495545424454 ) ) ;
#18009 = CARTESIAN_POINT ( 'NONE',  ( 7.084665262690076126, 22.02201867748817321, -10.88017736071110164 ) ) ;
#18011 = CARTESIAN_POINT ( 'NONE',  ( -2.266590686148945544, 36.38708216824730357, -7.082119434687050408 ) ) ;
#18012 = VECTOR ( 'NONE', #36718, 1000.000000000000000 ) ;
#18013 = CARTESIAN_POINT ( 'NONE',  ( -1.099225684535947600, 59.54030133659708923, 6.408140936763237150 ) ) ;
#18014 = ORIENTED_EDGE ( 'NONE', *, *, #32320, .F. ) ;
#18015 = CARTESIAN_POINT ( 'NONE',  ( 17.20831665107776587, 62.88393115100078745, 7.208316651077764980 ) ) ;
#18016 = CARTESIAN_POINT ( 'NONE',  ( 15.44008868035555793, 31.39701867748817676, -9.422509992056140149 ) ) ;
#18017 = ORIENTED_EDGE ( 'NONE', *, *, #29705, .F. ) ;
#18018 = CARTESIAN_POINT ( 'NONE',  ( 7.361572987183169658, -0.03273551566588185635, -9.846743663894592657 ) ) ;
#18019 = CARTESIAN_POINT ( 'NONE',  ( 66.56412365047464164, 14.00000000000000888, 9.500000000000000000 ) ) ;
#18020 = CARTESIAN_POINT ( 'NONE',  ( 19.84674366389459266, 8.717264484334116048, -2.638427012816827677 ) ) ;
#18021 = CARTESIAN_POINT ( 'NONE',  ( 18.52753015748618282, 3.925597817667451306, -4.923371831947291888 ) ) ;
#18022 = PRESENTATION_STYLE_ASSIGNMENT (( #55532 ) ) ;
#18023 = EDGE_CURVE ( 'NONE', #24535, #60677, #71250, .T. ) ;
#18025 = FILL_AREA_STYLE ('',( #3520 ) ) ;
#18024 = CARTESIAN_POINT ( 'NONE',  ( 20.88017736071110519, 60.56368534415484106, 2.639326808657452039E-16 ) ) ;
#18026 = CARTESIAN_POINT ( 'NONE',  ( 20.88017736071110875, 65.77201867748817676, -2.915334737309920765 ) ) ;
#18029 = ORIENTED_EDGE ( 'NONE', *, *, #27641, .T. ) ;
#18028 = MECHANICAL_DESIGN_GEOMETRIC_PRESENTATION_REPRESENTATION (  '', ( #37163 ), #43491 ) ;
#18027 = CARTESIAN_POINT ( 'NONE',  ( 1.472469842513823179, 10.59226448433411782, -4.923371831947296329 ) ) ;
#18030 = CARTESIAN_POINT ( 'NONE',  ( 41.74544750096863055, 57.05211158465706944, -8.000000000000000000 ) ) ;
#18031 = CARTESIAN_POINT ( 'NONE',  ( 14.92337183194729633, 52.67559781766745175, 8.527530157486181039 ) ) ;
#18032 = ORIENTED_EDGE ( 'NONE', *, *, #45261, .F. ) ;
#18033 = VERTEX_POINT ( 'NONE', #56724 ) ;
#18034 = CARTESIAN_POINT ( 'NONE',  ( 6.000000000000000000, 11.50000000000000000, -6.500000000000000888 ) ) ;
#18035 = CIRCLE ( 'NONE', #22820, 14.49999999999999822 ) ;
#18036 = CARTESIAN_POINT ( 'NONE',  ( 13.79529636645030344, 8.262082168247300018, 14.16423886937410614 ) ) ;
#18037 = MECHANICAL_DESIGN_GEOMETRIC_PRESENTATION_REPRESENTATION (  '', ( #43568 ), #13234 ) ;
#18038 = TOROIDAL_SURFACE ( 'NONE', #8401, 14.49999999999999822, 0.5000000000000000000 ) ;
#18039 = CARTESIAN_POINT ( 'NONE',  ( 3.591859063236763294, 58.29030133659708923, -11.09922568453595026 ) ) ;
#18040 = CARTESIAN_POINT ( 'NONE',  ( -4.164238869374098151, 1.595415501580634388, -3.795296366450310543 ) ) ;
#18041 = CARTESIAN_POINT ( 'NONE',  ( 2.917880565312950480, 35.97041550158063217, -12.26659068614894821 ) ) ;
#18042 = SURFACE_STYLE_USAGE ( .BOTH. , #12005 ) ;
#18043 = CARTESIAN_POINT ( 'NONE',  ( 12.91533473730993009, 26.60535201082150536, -10.88017736071109987 ) ) ;
#18044 = SURFACE_STYLE_USAGE ( .BOTH. , #86539 ) ;
#18045 = VERTEX_POINT ( 'NONE', #77748 ) ;
#18047 = STYLED_ITEM ( 'NONE', ( #58053 ), #76824 ) ;
#18046 = CARTESIAN_POINT ( 'NONE',  ( 7.361572987183169658, -0.03273551566588185635, -9.846743663894592657 ) ) ;
#18048 = CARTESIAN_POINT ( 'NONE',  ( 19.84674366389459266, 18.30059781766745175, 2.638427012816836559 ) ) ;
#18049 = CARTESIAN_POINT ( 'NONE',  ( 19.38216949554541557, 47.24863466993041783, -9.382169495545420901 ) ) ;
#18050 = CARTESIAN_POINT ( 'NONE',  ( 0.1532563361054083140, 36.00893115100078745, 1.131784320476157264E-15 ) ) ;
#18051 = DIRECTION ( 'NONE',  ( 0.000000000000000000, 0.000000000000000000, 1.000000000000000000 ) ) ;
#18052 = CARTESIAN_POINT ( 'NONE',  ( 20.88017736071110519, 55.56368534415484817, 2.639326808657452039E-16 ) ) ;
#18053 = CARTESIAN_POINT ( 'NONE',  ( 5.076628168052703671, 21.84226448433411960, 8.527530157486179263 ) ) ;
#18054 = CARTESIAN_POINT ( 'NONE',  ( 0.6178305044545838731, 34.74863466993042493, 9.382169495545420901 ) ) ;
#18055 = CARTESIAN_POINT ( 'NONE',  ( 14.92337183194729633, 22.67559781766745175, 8.527530157486181039 ) ) ;
#18056 = CARTESIAN_POINT ( 'NONE',  ( 22.26659068614894466, 8.887082168247300018, 7.082119434687054849 ) ) ;
#18057 = ORIENTED_EDGE ( 'NONE', *, *, #55358, .T. ) ;
#18058 = CARTESIAN_POINT ( 'NONE',  ( 19.42250999205614193, 35.14701867748816966, 5.440088680355555262 ) ) ;
#18059 = CARTESIAN_POINT ( 'NONE',  ( -0.3689425029237881626, 32.42874883491395366, 10.36894250292379027 ) ) ;
#18060 = CARTESIAN_POINT ( 'NONE',  ( 19.84674366389459266, 48.71726448433413026, -2.638427012816827677 ) ) ;
#18061 = EDGE_CURVE ( 'NONE', #86010, #76841, #36132, .T. ) ;
#18062 = CARTESIAN_POINT ( 'NONE',  ( 14.92337183194729988, 9.342264484334119601, -8.527530157486177487 ) ) ;
#18064 = CARTESIAN_POINT ( 'NONE',  ( -10.79772875661416265, 89.74400587740485946, 6.349085400557794578 ) ) ;
#18063 = CARTESIAN_POINT ( 'NONE',  ( 0.6178305044545818747, 53.49863466993041072, -9.382169495545419124 ) ) ;
#18065 = CARTESIAN_POINT ( 'NONE',  ( 0.5774900079438607392, 28.48035201082150891, 5.440088680355550821 ) ) ;
#18066 =( NAMED_UNIT ( * ) SI_UNIT ( $, .STERADIAN. ) SOLID_ANGLE_UNIT ( ) );
#18067 = CARTESIAN_POINT ( 'NONE',  ( 3.591859063236763294, 23.29030133659708568, -11.09922568453595026 ) ) ;
#18068 = CARTESIAN_POINT ( 'NONE',  ( 7.361572987183169658, 39.96726448433411605, -9.846743663894592657 ) ) ;
#18069 = CARTESIAN_POINT ( 'NONE',  ( -10.88017736071110342, -1.936314655845157384, 3.903127820947815962E-15 ) ) ;
#18071 = CARTESIAN_POINT ( 'NONE',  ( 19.72487221294569792, 32.80223176428832232, -6.500000000000008882 ) ) ;
#18070 = CARTESIAN_POINT ( 'NONE',  ( 19.42250999205614548, 60.98035201082151247, -5.440088680355545492 ) ) ;
#18072 = CIRCLE ( 'NONE', #79369, 0.5000000000000004441 ) ;
#18073 = CARTESIAN_POINT ( 'NONE',  ( -13.34989199099671353, 0.04962897297196560559, -6.279943681065631722 ) ) ;
#18074 = EDGE_CURVE ( 'NONE', #41505, #39745, #55412, .T. ) ;
#18075 = DIRECTION ( 'NONE',  ( 0.000000000000000000, 0.000000000000000000, 1.000000000000000000 ) ) ;
#18076 = CARTESIAN_POINT ( 'NONE',  ( 10.00000000000000178, 54.31368534415484106, 10.88017736071110342 ) ) ;
#18078 = CARTESIAN_POINT ( 'NONE',  ( 20.88017736071110519, 60.56368534415484106, 2.639326808657452039E-16 ) ) ;
#18077 = AXIS2_PLACEMENT_3D ( 'NONE', #28705, #50215, #96737 ) ;
#18079 = CARTESIAN_POINT ( 'NONE',  ( 19.80448550324510038, 56.82703681773343618, 6.500000000002678746 ) ) ;
#18080 = B_SPLINE_CURVE_WITH_KNOTS ( 'NONE', 3,
 ( #33894, #64399, #63428, #56907, #79903, #25459 ),
 .UNSPECIFIED., .F., .F.,
 ( 4, 2, 4 ),
 ( 0.0002800245631443565872, 0.0006862300328522100146, 0.001092435502560063550 ),
 .UNSPECIFIED. ) ;
#18081 = CARTESIAN_POINT ( 'NONE',  ( 2.393480905993186969, 14.49999999999999112, -14.80781041047757185 ) ) ;
#18082 = EDGE_CURVE ( 'NONE', #4700, #15469, #40258, .T. ) ;
#18083 = EDGE_CURVE ( 'NONE', #7679, #49977, #24352, .T. ) ;
#18084 = CARTESIAN_POINT ( 'NONE',  ( 7.084665262690076126, 7.022018677488170546, -10.88017736071110164 ) ) ;
#18085 = CARTESIAN_POINT ( 'NONE',  ( 2.791683348922240793, 61.63393115100079456, 7.208316651077764092 ) ) ;
#18087 = CARTESIAN_POINT ( 'NONE',  ( -3.585700563647884032, -2.697940300814421377, -3.750000000000000888 ) ) ;
#18086 = CARTESIAN_POINT ( 'NONE',  ( 10.00000000000000000, 26.81368534415484106, -10.88017736071110342 ) ) ;
#18088 =( NAMED_UNIT ( * ) SI_UNIT ( $, .STERADIAN. ) SOLID_ANGLE_UNIT ( ) );
#18089 = CARTESIAN_POINT ( 'NONE',  ( -1.099225684535947600, 29.54030133659708923, 6.408140936763237150 ) ) ;
#18090 = VERTEX_POINT ( 'NONE', #41743 ) ;
#18091 = CARTESIAN_POINT ( 'NONE',  ( 4.559911319644449179, 57.23035201082150536, -9.422509992056141925 ) ) ;
#18092 = CARTESIAN_POINT ( 'NONE',  ( 18.52753015748617571, 43.09226448433412315, 4.923371831947298993 ) ) ;
#18094 = LINE ( 'NONE', #69123, #60538 ) ;
#18093 = CARTESIAN_POINT ( 'NONE',  ( 13.43411237798106583, 7.665301336597086568, -12.81628187352647252 ) ) ;
#18095 = CARTESIAN_POINT ( 'NONE',  ( -0.8801773607111009756, 28.06368534415484106, 1.068504757029289695E-15 ) ) ;
#18096 = CARTESIAN_POINT ( 'NONE',  ( 7.084665262690076126, 42.02201867748816966, -10.88017736071110164 ) ) ;
#18097 = CARTESIAN_POINT ( 'NONE',  ( 10.00000000000000178, 48.05374883491396787, 14.16423886937410082 ) ) ;
#18098 = CARTESIAN_POINT ( 'NONE',  ( 7.361572987183170547, 37.05059781766744464, 9.846743663894590881 ) ) ;
#18099 = CARTESIAN_POINT ( 'NONE',  ( 17.96484262340118221, 59.93868534415484106, 7.964842623401181321 ) ) ;
#18100 = CARTESIAN_POINT ( 'NONE',  ( 19.42250999205614193, 45.14701867748817676, 5.440088680355555262 ) ) ;
#18101 = DIRECTION ( 'NONE',  ( 0.000000000000000000, 0.000000000000000000, -1.000000000000000000 ) ) ;
#18102 = CARTESIAN_POINT ( 'NONE',  ( 22.26659068614895176, 19.72041550158063572, -7.082119434687042414 ) ) ;
#18103 = CARTESIAN_POINT ( 'NONE',  ( 15.00000000000000000, 77.07179676972447169, 4.250000000000000000 ) ) ;
#18104 = CARTESIAN_POINT ( 'NONE',  ( 2.849309504156442685, 0.000000000000000000, 4.649650521509849810 ) ) ;
#18105 = ORIENTED_EDGE ( 'NONE', *, *, #70206, .F. ) ;
#18106 = VERTEX_POINT ( 'NONE', #72213 ) ;
#18107 = CARTESIAN_POINT ( 'NONE',  ( 22.26659068614895176, 49.72041550158063927, -7.082119434687042414 ) ) ;
#18108 = CARTESIAN_POINT ( 'NONE',  ( 2.917880565312948704, 37.63708216824731068, 12.26659068614894643 ) ) ;
#18109 = CARTESIAN_POINT ( 'NONE',  ( 0.1532563361054082862, 21.21726448433412315, 2.638427012816831674 ) ) ;
#18110 = ADVANCED_FACE ( 'NONE', ( #10739, #93738 ), #25274, .F. ) ;
#18111 = CARTESIAN_POINT ( 'NONE',  ( 22.81628187352648496, 11.83196800326375531, -3.434112377981050290 ) ) ;
#18112 = DIRECTION ( 'NONE',  ( -0.000000000000000000, 0.000000000000000000, -1.000000000000000000 ) ) ;
#18113 = CARTESIAN_POINT ( 'NONE',  ( 0.9413316022086140045, 58.45508385108959004, 6.499999999999978684 ) ) ;
#18115 = CARTESIAN_POINT ( 'NONE',  ( -2.816281873526473856, 34.33196800326376064, 3.434112377981055619 ) ) ;
#18114 = CARTESIAN_POINT ( 'NONE',  ( 10.00000000000000178, 4.313685344154837509, 10.88017736071110342 ) ) ;
#18116 = CARTESIAN_POINT ( 'NONE',  ( -0.3689425029237898834, 46.17874883491397497, -10.36894250292378850 ) ) ;
#18117 = AXIS2_PLACEMENT_3D ( 'NONE', #41649, #25177, #10159 ) ;
#18118 = CARTESIAN_POINT ( 'NONE',  ( -0.08248232600719085372, 0.1423898869303599768, 6.349449577244200782 ) ) ;
#18119 = CARTESIAN_POINT ( 'NONE',  ( 20.88017736071110875, 65.77201867748817676, -2.915334737309920765 ) ) ;
#18120 = EDGE_CURVE ( 'NONE', #4498, #82904, #60573, .T. ) ;
#18121 = COLOUR_RGB ( '', 0.40784314, 0.44705882, 0.49803922) ;
#18122 = CARTESIAN_POINT ( 'NONE',  ( -9.846743663894590881, -13.78273551566587862, 2.638427012816840111 ) ) ;
#18123 = CARTESIAN_POINT ( 'NONE',  ( 12.63842701281683034, 7.467264484334118713, 9.846743663894596210 ) ) ;
#18124 = EDGE_LOOP ( 'NONE', ( #68296, #81325, #2818, #20406 ) ) ;
#18125 = CARTESIAN_POINT ( 'NONE',  ( 12.63842701281683922, 14.55059781766744997, -9.846743663894590881 ) ) ;
#18126 = AXIS2_PLACEMENT_3D ( 'NONE', #95870, #27352, #57845 ) ;
#18127 = DIRECTION ( 'NONE',  ( 0.000000000000000000, 0.000000000000000000, 1.000000000000000000 ) ) ;
#18128 = ORIENTED_EDGE ( 'NONE', *, *, #14111, .F. ) ;
#18129 = CARTESIAN_POINT ( 'NONE',  ( -4.164238869374099927, 7.012082168247302683, 3.795296366450308767 ) ) ;
#18131 = CARTESIAN_POINT ( 'NONE',  ( 4.559911319644449179, 12.23035201082150714, -9.422509992056141925 ) ) ;
#18130 = CARTESIAN_POINT ( 'NONE',  ( 2.035157376598824452, 8.688685344154839285, 7.964842623401179544 ) ) ;
#18133 = CARTESIAN_POINT ( 'NONE',  ( -1.099225684535947600, 4.540301336597087456, 6.408140936763237150 ) ) ;
#18132 = CARTESIAN_POINT ( 'NONE',  ( 0.1532563361054083140, 36.00893115100078745, 1.131784320476157264E-15 ) ) ;
#18134 = FILL_AREA_STYLE_COLOUR ( '', #50229 ) ;
#18135 = DIRECTION ( 'NONE',  ( 0.9848077530122084644, 0.1736481776669282495, 0.000000000000000000 ) ) ;
#18136 = B_SPLINE_CURVE_WITH_KNOTS ( 'NONE', 3,
 ( #56305, #70326, #94283, #93796, #86799, #48783, #79291, #26278, #41317, #71789 ),
 .UNSPECIFIED., .F., .F.,
 ( 4, 3, 3, 4 ),
 ( 1.528532816688728551E-17, 0.0006253016069560878021, 0.001250604074564932566, 0.002501455912506543068 ),
 .UNSPECIFIED. ) ;
#18137 = CARTESIAN_POINT ( 'NONE',  ( 16.40814093676324603, 17.45696800326375353, -11.09922568453594671 ) ) ;
#18138 = ORIENTED_EDGE ( 'NONE', *, *, #75431, .F. ) ;
#18139 =( BOUNDED_SURFACE ( )  B_SPLINE_SURFACE ( 1, 2, ( 
 ( #58251, #36767, #20774, #6758, #51763, #51265, #97786, #37272, #82247, #13762, #88767, #20278, #67761, #81749, #98280, #29735, #5289, #67259, #22266, #81267, #96788, #13263, #5776, #36265, #52739, #60731, #7759, #1253, #39238, #47203, #68744, #91736, #23257, #84729, #32195, #46238, #69240, #54702, #30723, #46715, #85713, #30227, #70222, #17228, #70718, #38740, #16235, #1741, #53732, #93197, #77704, #9216, #62696, #91232, #31708, #762, #61230, #83742, #47705, #31215, #22756, #53238, #276, #23752, #15266, #84251, #15753, #39728, #8720, #24723, #76724, #45747, #55199, #78199, #92226, #69726, #9711, #8243, #76243, #40211, #61710, #54212, #77215, #62203, #38252, #92709, #24235, #85223, #16726, #19666, #40703, #55708, #86696, #57655, #86205, #87171, #94680, #95161, #64162, #78702, #10698, #50155, #27154, #79184, #71690, #42184, #88152, #33665, #34654, #2729, #25229, #72648, #26668, #41212, #42664, #18694, #41697, #19173, #63676, #3202, #26188, #56203, #4183, #80664, #71207, #17716, #56680, #93694, #32692, #49178, #79679, #34156, #11177, #33184, #57162, #12159, #72168, #48681, #87660, #3695, #48189, #63189, #94181, #25710, #18202, #10211, #65149, #64648, #49653, #80163, #2234, #11674, #95668, #52134, #21148, #74124, #4680, #35143, #96166, #98152, #12649, #6144, #58644, #43146, #75124, #67133, #20153, #58136, #82128, #29125, #60115, #29610, #22138, #73143, #5660, #88645, #59626, #36142, #66646, #81633, #6631, #90614, #50656, #90121, #52622, #83122, #67643, #65642, #44122, #13142, #27649, #28637, #14650, #81145, #73635, #35649, #74632, #43639, #37147, #51648, #5163, #36646, #97658, #21649, #66135, #59127, #96667, #82629, #89637, #28148, #89143, #13637, #20653, #51147, #97170, #14145, #44629, #69604, #16109, #46595, #24112, #45618, #93078, #24608, #16606, #68132, #83624, #54582, #85097, #70099, #76604, #77580, #76115, #98659, #47085, #39114, #84122, #85594, #31096, #84608, #62082, #7644, #53605, #8120, #152, #9096, #1624, #15140, #60613, #38615, #37635, #75621, #647, #15634, #77094, #61590, #38135, #1125, #55075, #92103, #91615, #31587, #69116, #30107, #7133, #68622, #30601, #61106, #22635, #39610, #8606, #53116, #23634, #45113, #92589, #91111, #32072, #54093, #46117, #23132, #62574, #40091, #42071, #55591, #49064, #2611, #86086, #19060, #11066, #63072, #2117, #26076, #72053, #4066, #72532, #65023, #17107, #18085, #32576, #3582, #48561, #79061, #25591, #49538, #34529, #93573, #34039, #95551, #27039, #11551, #78084, #87061, #56083, #9588, #71582, #57538, #47590, #17596, #78580, #18571, #86577, #80047, #64045, #48065, #79568 ),
 ( #25108, #33549, #70591, #10090, #41587, #10575, #33066, #94558, #64535, #40589, #71086, #95043, #57047, #41085, #63562, #26551, #94070, #3094, #56570, #87549, #58026, #82016, #28026, #29493, #74016, #28526, #6034, #50537, #96551, #20540, #43039, #59515, #14033, #88534, #4562, #51025, #80547, #19549, #43521, #58522, #21034, #5546, #20035, #13528, #67521, #36023, #35530, #74514, #81518, #42544, #50044, #81031, #12538, #73519, #65526, #21530, #89525, #96049, #66525, #37024, #36533, #98038, #67022, #97052, #89030, #12044, #73029, #35025, #44511, #27533, #51524, #5047, #66024, #90009, #44010, #13025, #59018, #97543, #29005, #75010, #6515, #88035, #52023, #82515, #75505, #46484, #91498, #23019, #68509, #92472, #46972, #37525, #15996, #84977, #8977, #54471, #22031, #30981, #39, #52505, #15523, #77466, #39494, #60501, #22521, #61480, #30488, #23998, #8007, #90991, #91985, #53987, #76980, #69984, #46004, #98542, #69492, #76494, #16495, #52993, #38505, #45000, #15025, #53488, #83999, #23517, #84495, #8494, #38997, #1008, #83508, #1509, #60002, #31470, #83012, #29994, #61973, #60986, #90496, #14530, #38016, #69002, #7019, #68015, #534, #45498, #75998, #7526, #71940, #55969, #48940, #47466, #48453, #94932, #24494, #2983, #93959, #17485, #10462, #79449, #93464, #70477, #18457, #3463, #86469, #54957, #33431, #78461, #87435, #79931, #40972, #1997, #56458, #32951, #32463, #71470, #10948, #25484, #17966, #11438, #18950, #94443, #62958, #86944, #25955, #16987, #78951, #63928, #92960, #49427, #39976, #85478, #31956, #26435, #62458, #9473, #41473, #33918, #64425, #24990, #55473, #85975, #56933, #41957, #47951, #70976, #72421, #9974, #77966, #40479, #2497, #63455, #89894, #44394, #12418, #58400, #74392, #95937, #66903, #20920, #81896, #5916, #64910, #73905, #42925, #4450, #57427, #21412, #73405, #3947, #34420, #42438, #96437, #95435, #27419, #57912, #51409, #81408, #36409, #88423, #26929, #97422, #13407, #65905, #12910, #51907, #72920, #87920, #28888, #34915, #35413, #65412, #19923, #43892, #19437, #80435, #96936, #66405, #82392, #50416, #49924, #80925, #59392, #11933, #88918, #27907, #28411, #20425, #4933, #50912, #13916, #58906, #43407, #5436, #35908, #89404, #9726, #67399, #45893, #37906, #60380, #53373, #24736, #37413, #14410, #61368, #17243, #98916, #97925, #76380, #22406, #32708, #25243, #83883, #44881, #420, #75887, #75383, #15410, #55213, #68395, #30371, #55727, #63205, #38389, #6899, #30871, #68892, #59886, #60875, #7895, #36907, #93708, #82894, #29385, #74893, #40226, #6392, #52394, #91878, #85729, #47719, #67900, #98424, #29878 ) ),
 .UNSPECIFIED., .F., .F., .F. ) 
 B_SPLINE_SURFACE_WITH_KNOTS ( ( 2, 2 ),
 ( 3, 2, 2, 2, 2, 2, 2, 2, 2, 2, 2, 2, 2, 2, 2, 2, 2, 2, 2, 2, 2, 2, 2, 2, 2, 2, 2, 2, 2, 2, 2, 2, 2, 2, 2, 2, 2, 2, 2, 2, 2, 2, 2, 2, 2, 2, 2, 2, 2, 2, 2, 2, 2, 2, 2, 2, 2, 2, 2, 2, 2, 2, 2, 2, 2, 2, 2, 2, 2, 2, 2, 2, 2, 2, 2, 2, 2, 2, 2, 2, 2, 2, 2, 2, 2, 2, 2, 2, 2, 2, 2, 2, 2, 2, 2, 2, 2, 2, 2, 2, 2, 2, 2, 2, 2, 2, 2, 2, 2, 2, 2, 2, 2, 2, 2, 2, 2, 2, 2, 2, 2, 2, 2, 2, 2, 2, 2, 2, 2, 2, 2, 2, 2, 2, 2, 2, 2, 2, 2, 2, 2, 2, 2, 2, 2, 2, 2, 2, 2, 2, 2, 2, 2, 2, 2, 2, 2, 2, 2, 2, 2, 2, 3 ),
 ( 0.000000000000000000, 1.000000000000000000 ),
 ( 0.000000000000000000, 0.005952380952380952051, 0.01190476190476190410, 0.01785714285714285615, 0.02380952380952380820, 0.02976190476190476025, 0.03571428571428571230, 0.04166666666666666435, 0.04761904761904761640, 0.05357142857142856845, 0.05952380952380952051, 0.06547619047619047949, 0.07142857142857142461, 0.07738095238095238360, 0.08333333333333332871, 0.08928571428571428770, 0.09523809523809523281, 0.1011904761904761918, 0.1071428571428571369, 0.1130952380952380959, 0.1190476190476190410, 0.1250000000000000000, 0.1309523809523809590, 0.1369047619047619180, 0.1428571428571428492, 0.1488095238095238082, 0.1547619047619047672, 0.1607142857142857262, 0.1666666666666666574, 0.1726190476190476164, 0.1785714285714285754, 0.1845238095238095344, 0.1904761904761904656, 0.1964285714285714246, 0.2023809523809523836, 0.2083333333333333426, 0.2142857142857142738, 0.2202380952380952328, 0.2261904761904761918, 0.2321428571428571508, 0.2380952380952380820, 0.2440476190476190410, 0.2500000000000000000, 0.2559523809523809312, 0.2619047619047619180, 0.2678571428571428492, 0.2738095238095238360, 0.2797619047619047672, 0.2857142857142856984, 0.2916666666666666852, 0.2976190476190476164, 0.3035714285714285476, 0.3095238095238095344, 0.3154761904761904656, 0.3214285714285714524, 0.3273809523809523836, 0.3333333333333333148, 0.3392857142857143016, 0.3452380952380952328, 0.3511904761904761640, 0.3571428571428571508, 0.3630952380952380820, 0.3690476190476190688, 0.3750000000000000000, 0.3809523809523809312, 0.3869047619047619180, 0.3928571428571428492, 0.3988095238095238360, 0.4047619047619047672, 0.4107142857142856984, 0.4166666666666666852, 0.4226190476190476164, 0.4285714285714285476, 0.4345238095238095344, 0.4404761904761904656, 0.4464285714285714524, 0.4523809523809523836, 0.4583333333333333148, 0.4642857142857143016, 0.4702380952380952328, 0.4761904761904761640, 0.4821428571428571508, 0.4880952380952380820, 0.4940476190476190688, 0.5000000000000000000, 0.5059523809523809312, 0.5119047619047618625, 0.5178571428571429047, 0.5238095238095238360, 0.5297619047619047672, 0.5357142857142856984, 0.5416666666666666297, 0.5476190476190476719, 0.5535714285714286031, 0.5595238095238095344, 0.5654761904761904656, 0.5714285714285713969, 0.5773809523809523281, 0.5833333333333333703, 0.5892857142857143016, 0.5952380952380952328, 0.6011904761904761640, 0.6071428571428570953, 0.6130952380952381375, 0.6190476190476190688, 0.6250000000000000000, 0.6309523809523809312, 0.6369047619047618625, 0.6428571428571429047, 0.6488095238095238360, 0.6547619047619047672, 0.6607142857142856984, 0.6666666666666666297, 0.6726190476190476719, 0.6785714285714286031, 0.6845238095238095344, 0.6904761904761904656, 0.6964285714285713969, 0.7023809523809523281, 0.7083333333333333703, 0.7142857142857143016, 0.7202380952380952328, 0.7261904761904761640, 0.7321428571428570953, 0.7380952380952381375, 0.7440476190476190688, 0.7500000000000000000, 0.7559523809523809312, 0.7619047619047618625, 0.7678571428571429047, 0.7738095238095238360, 0.7797619047619047672, 0.7857142857142856984, 0.7916666666666666297, 0.7976190476190476719, 0.8035714285714286031, 0.8095238095238095344, 0.8154761904761904656, 0.8214285714285713969, 0.8273809523809523281, 0.8333333333333333703, 0.8392857142857143016, 0.8452380952380952328, 0.8511904761904761640, 0.8571428571428570953, 0.8630952380952381375, 0.8690476190476190688, 0.8750000000000000000, 0.8809523809523809312, 0.8869047619047618625, 0.8928571428571429047, 0.8988095238095238360, 0.9047619047619047672, 0.9107142857142856984, 0.9166666666666666297, 0.9226190476190476719, 0.9285714285714286031, 0.9345238095238095344, 0.9404761904761904656, 0.9464285714285713969, 0.9523809523809523281, 0.9583333333333333703, 0.9642857142857143016 ),
 .UNSPECIFIED. ) 
 GEOMETRIC_REPRESENTATION_ITEM ( )  RATIONAL_B_SPLINE_SURFACE ( (
 ( 1.000000000000000000, 0.9659258262890683122, 1.000000000000000000, 0.9659258262890683122, 1.000000000000000000, 0.9659258262890683122, 1.000000000000000000, 0.9659258262890683122, 1.000000000000000000, 0.9659258262890683122, 1.000000000000000000, 0.9659258262890683122, 1.000000000000000000, 0.9659258262890683122, 1.000000000000000000, 0.9659258262890683122, 1.000000000000000000, 0.9659258262890683122, 1.000000000000000000, 0.9659258262890683122, 1.000000000000000000, 0.9659258262890683122, 1.000000000000000000, 0.9659258262890683122, 1.000000000000000000, 0.9659258262890683122, 1.000000000000000000, 0.9659258262890683122, 1.000000000000000000, 0.9659258262890683122, 1.000000000000000000, 0.9659258262890683122, 1.000000000000000000, 0.9659258262890683122, 1.000000000000000000, 0.9659258262890683122, 1.000000000000000000, 0.9659258262890683122, 1.000000000000000000, 0.9659258262890683122, 1.000000000000000000, 0.9659258262890683122, 1.000000000000000000, 0.9659258262890683122, 1.000000000000000000, 0.9659258262890683122, 1.000000000000000000, 0.9659258262890683122, 1.000000000000000000, 0.9659258262890683122, 1.000000000000000000, 0.9659258262890683122, 1.000000000000000000, 0.9659258262890683122, 1.000000000000000000, 0.9659258262890683122, 1.000000000000000000, 0.9659258262890683122, 1.000000000000000000, 0.9659258262890683122, 1.000000000000000000, 0.9659258262890683122, 1.000000000000000000, 0.9659258262890683122, 1.000000000000000000, 0.9659258262890683122, 1.000000000000000000, 0.9659258262890683122, 1.000000000000000000, 0.9659258262890683122, 1.000000000000000000, 0.9659258262890683122, 1.000000000000000000, 0.9659258262890683122, 1.000000000000000000, 0.9659258262890683122, 1.000000000000000000, 0.9659258262890683122, 1.000000000000000000, 0.9659258262890683122, 1.000000000000000000, 0.9659258262890683122, 1.000000000000000000, 0.9659258262890683122, 1.000000000000000000, 0.9659258262890683122, 1.000000000000000000, 0.9659258262890683122, 1.000000000000000000, 0.9659258262890683122, 1.000000000000000000, 0.9659258262890683122, 1.000000000000000000, 0.9659258262890683122, 1.000000000000000000, 0.9659258262890683122, 1.000000000000000000, 0.9659258262890683122, 1.000000000000000000, 0.9659258262890683122, 1.000000000000000000, 0.9659258262890683122, 1.000000000000000000, 0.9659258262890683122, 1.000000000000000000, 0.9659258262890683122, 1.000000000000000000, 0.9659258262890683122, 1.000000000000000000, 0.9659258262890683122, 1.000000000000000000, 0.9659258262890683122, 1.000000000000000000, 0.9659258262890683122, 1.000000000000000000, 0.9659258262890683122, 1.000000000000000000, 0.9659258262890683122, 1.000000000000000000, 0.9659258262890683122, 1.000000000000000000, 0.9659258262890683122, 1.000000000000000000, 0.9659258262890683122, 1.000000000000000000, 0.9659258262890683122, 1.000000000000000000, 0.9659258262890683122, 1.000000000000000000, 0.9659258262890683122, 1.000000000000000000, 0.9659258262890683122, 1.000000000000000000, 0.9659258262890683122, 1.000000000000000000, 0.9659258262890683122, 1.000000000000000000, 0.9659258262890683122, 1.000000000000000000, 0.9659258262890683122, 1.000000000000000000, 0.9659258262890683122, 1.000000000000000000, 0.9659258262890683122, 1.000000000000000000, 0.9659258262890683122, 1.000000000000000000, 0.9659258262890683122, 1.000000000000000000, 0.9659258262890683122, 1.000000000000000000, 0.9659258262890683122, 1.000000000000000000, 0.9659258262890683122, 1.000000000000000000, 0.9659258262890683122, 1.000000000000000000, 0.9659258262890683122, 1.000000000000000000, 0.9659258262890683122, 1.000000000000000000, 0.9659258262890683122, 1.000000000000000000, 0.9659258262890683122, 1.000000000000000000, 0.9659258262890683122, 1.000000000000000000, 0.9659258262890683122, 1.000000000000000000, 0.9659258262890683122, 1.000000000000000000, 0.9659258262890683122, 1.000000000000000000, 0.9659258262890683122, 1.000000000000000000, 0.9659258262890683122, 1.000000000000000000, 0.9659258262890683122, 1.000000000000000000, 0.9659258262890683122, 1.000000000000000000, 0.9659258262890683122, 1.000000000000000000, 0.9659258262890683122, 1.000000000000000000, 0.9659258262890683122, 1.000000000000000000, 0.9659258262890683122, 1.000000000000000000, 0.9659258262890683122, 1.000000000000000000, 0.9659258262890683122, 1.000000000000000000, 0.9659258262890683122, 1.000000000000000000, 0.9659258262890683122, 1.000000000000000000, 0.9659258262890683122, 1.000000000000000000, 0.9659258262890683122, 1.000000000000000000, 0.9659258262890683122, 1.000000000000000000, 0.9659258262890683122, 1.000000000000000000, 0.9659258262890683122, 1.000000000000000000, 0.9659258262890683122, 1.000000000000000000, 0.9659258262890683122, 1.000000000000000000, 0.9659258262890683122, 1.000000000000000000, 0.9659258262890683122, 1.000000000000000000, 0.9659258262890683122, 1.000000000000000000, 0.9659258262890683122, 1.000000000000000000, 0.9659258262890683122, 1.000000000000000000, 0.9659258262890683122, 1.000000000000000000, 0.9659258262890683122, 1.000000000000000000, 0.9659258262890683122, 1.000000000000000000, 0.9659258262890683122, 1.000000000000000000, 0.9659258262890683122, 1.000000000000000000, 0.9659258262890683122, 1.000000000000000000, 0.9659258262890683122, 1.000000000000000000, 0.9659258262890683122, 1.000000000000000000, 0.9659258262890683122, 1.000000000000000000, 0.9659258262890683122, 1.000000000000000000, 0.9659258262890683122, 1.000000000000000000, 0.9659258262890683122, 1.000000000000000000, 0.9659258262890683122, 1.000000000000000000, 0.9659258262890683122, 1.000000000000000000, 0.9659258262890683122, 1.000000000000000000, 0.9659258262890683122, 1.000000000000000000, 0.9659258262890683122, 1.000000000000000000, 0.9659258262890683122, 1.000000000000000000, 0.9659258262890683122, 1.000000000000000000, 0.9659258262890683122, 1.000000000000000000, 0.9659258262890683122, 1.000000000000000000, 0.9659258262890683122, 1.000000000000000000, 0.9659258262890683122, 1.000000000000000000, 0.9659258262890683122, 1.000000000000000000, 0.9659258262890683122, 1.000000000000000000, 0.9659258262890683122, 1.000000000000000000, 0.9659258262890683122, 1.000000000000000000, 0.9659258262890683122, 1.000000000000000000, 0.9659258262890683122, 1.000000000000000000, 0.9659258262890683122, 1.000000000000000000, 0.9659258262890683122, 1.000000000000000000, 0.9659258262890683122, 1.000000000000000000, 0.9659258262890683122, 1.000000000000000000, 0.9659258262890683122, 1.000000000000000000, 0.9659258262890683122, 1.000000000000000000, 0.9659258262890683122, 1.000000000000000000, 0.9659258262890683122, 1.000000000000000000, 0.9659258262890683122, 1.000000000000000000, 0.9659258262890683122, 1.000000000000000000, 0.9659258262890683122, 1.000000000000000000, 0.9659258262890683122, 1.000000000000000000, 0.9659258262890683122, 1.000000000000000000, 0.9659258262890683122, 1.000000000000000000, 0.9659258262890683122, 1.000000000000000000, 0.9659258262890683122, 1.000000000000000000, 0.9659258262890683122, 1.000000000000000000, 0.9659258262890683122, 1.000000000000000000, 0.9659258262890683122, 1.000000000000000000, 0.9659258262890683122, 1.000000000000000000, 0.9659258262890683122, 1.000000000000000000, 0.9659258262890683122, 1.000000000000000000, 0.9659258262890683122, 1.000000000000000000),
 ( 1.000000000000000000, 0.9659258262890683122, 1.000000000000000000, 0.9659258262890683122, 1.000000000000000000, 0.9659258262890683122, 1.000000000000000000, 0.9659258262890683122, 1.000000000000000000, 0.9659258262890683122, 1.000000000000000000, 0.9659258262890683122, 1.000000000000000000, 0.9659258262890683122, 1.000000000000000000, 0.9659258262890683122, 1.000000000000000000, 0.9659258262890683122, 1.000000000000000000, 0.9659258262890683122, 1.000000000000000000, 0.9659258262890683122, 1.000000000000000000, 0.9659258262890683122, 1.000000000000000000, 0.9659258262890683122, 1.000000000000000000, 0.9659258262890683122, 1.000000000000000000, 0.9659258262890683122, 1.000000000000000000, 0.9659258262890683122, 1.000000000000000000, 0.9659258262890683122, 1.000000000000000000, 0.9659258262890683122, 1.000000000000000000, 0.9659258262890683122, 1.000000000000000000, 0.9659258262890683122, 1.000000000000000000, 0.9659258262890683122, 1.000000000000000000, 0.9659258262890683122, 1.000000000000000000, 0.9659258262890683122, 1.000000000000000000, 0.9659258262890683122, 1.000000000000000000, 0.9659258262890683122, 1.000000000000000000, 0.9659258262890683122, 1.000000000000000000, 0.9659258262890683122, 1.000000000000000000, 0.9659258262890683122, 1.000000000000000000, 0.9659258262890683122, 1.000000000000000000, 0.9659258262890683122, 1.000000000000000000, 0.9659258262890683122, 1.000000000000000000, 0.9659258262890683122, 1.000000000000000000, 0.9659258262890683122, 1.000000000000000000, 0.9659258262890683122, 1.000000000000000000, 0.9659258262890683122, 1.000000000000000000, 0.9659258262890683122, 1.000000000000000000, 0.9659258262890683122, 1.000000000000000000, 0.9659258262890683122, 1.000000000000000000, 0.9659258262890683122, 1.000000000000000000, 0.9659258262890683122, 1.000000000000000000, 0.9659258262890683122, 1.000000000000000000, 0.9659258262890683122, 1.000000000000000000, 0.9659258262890683122, 1.000000000000000000, 0.9659258262890683122, 1.000000000000000000, 0.9659258262890683122, 1.000000000000000000, 0.9659258262890683122, 1.000000000000000000, 0.9659258262890683122, 1.000000000000000000, 0.9659258262890683122, 1.000000000000000000, 0.9659258262890683122, 1.000000000000000000, 0.9659258262890683122, 1.000000000000000000, 0.9659258262890683122, 1.000000000000000000, 0.9659258262890683122, 1.000000000000000000, 0.9659258262890683122, 1.000000000000000000, 0.9659258262890683122, 1.000000000000000000, 0.9659258262890683122, 1.000000000000000000, 0.9659258262890683122, 1.000000000000000000, 0.9659258262890683122, 1.000000000000000000, 0.9659258262890683122, 1.000000000000000000, 0.9659258262890683122, 1.000000000000000000, 0.9659258262890683122, 1.000000000000000000, 0.9659258262890683122, 1.000000000000000000, 0.9659258262890683122, 1.000000000000000000, 0.9659258262890683122, 1.000000000000000000, 0.9659258262890683122, 1.000000000000000000, 0.9659258262890683122, 1.000000000000000000, 0.9659258262890683122, 1.000000000000000000, 0.9659258262890683122, 1.000000000000000000, 0.9659258262890683122, 1.000000000000000000, 0.9659258262890683122, 1.000000000000000000, 0.9659258262890683122, 1.000000000000000000, 0.9659258262890683122, 1.000000000000000000, 0.9659258262890683122, 1.000000000000000000, 0.9659258262890683122, 1.000000000000000000, 0.9659258262890683122, 1.000000000000000000, 0.9659258262890683122, 1.000000000000000000, 0.9659258262890683122, 1.000000000000000000, 0.9659258262890683122, 1.000000000000000000, 0.9659258262890683122, 1.000000000000000000, 0.9659258262890683122, 1.000000000000000000, 0.9659258262890683122, 1.000000000000000000, 0.9659258262890683122, 1.000000000000000000, 0.9659258262890683122, 1.000000000000000000, 0.9659258262890683122, 1.000000000000000000, 0.9659258262890683122, 1.000000000000000000, 0.9659258262890683122, 1.000000000000000000, 0.9659258262890683122, 1.000000000000000000, 0.9659258262890683122, 1.000000000000000000, 0.9659258262890683122, 1.000000000000000000, 0.9659258262890683122, 1.000000000000000000, 0.9659258262890683122, 1.000000000000000000, 0.9659258262890683122, 1.000000000000000000, 0.9659258262890683122, 1.000000000000000000, 0.9659258262890683122, 1.000000000000000000, 0.9659258262890683122, 1.000000000000000000, 0.9659258262890683122, 1.000000000000000000, 0.9659258262890683122, 1.000000000000000000, 0.9659258262890683122, 1.000000000000000000, 0.9659258262890683122, 1.000000000000000000, 0.9659258262890683122, 1.000000000000000000, 0.9659258262890683122, 1.000000000000000000, 0.9659258262890683122, 1.000000000000000000, 0.9659258262890683122, 1.000000000000000000, 0.9659258262890683122, 1.000000000000000000, 0.9659258262890683122, 1.000000000000000000, 0.9659258262890683122, 1.000000000000000000, 0.9659258262890683122, 1.000000000000000000, 0.9659258262890683122, 1.000000000000000000, 0.9659258262890683122, 1.000000000000000000, 0.9659258262890683122, 1.000000000000000000, 0.9659258262890683122, 1.000000000000000000, 0.9659258262890683122, 1.000000000000000000, 0.9659258262890683122, 1.000000000000000000, 0.9659258262890683122, 1.000000000000000000, 0.9659258262890683122, 1.000000000000000000, 0.9659258262890683122, 1.000000000000000000, 0.9659258262890683122, 1.000000000000000000, 0.9659258262890683122, 1.000000000000000000, 0.9659258262890683122, 1.000000000000000000, 0.9659258262890683122, 1.000000000000000000, 0.9659258262890683122, 1.000000000000000000, 0.9659258262890683122, 1.000000000000000000, 0.9659258262890683122, 1.000000000000000000, 0.9659258262890683122, 1.000000000000000000, 0.9659258262890683122, 1.000000000000000000, 0.9659258262890683122, 1.000000000000000000, 0.9659258262890683122, 1.000000000000000000, 0.9659258262890683122, 1.000000000000000000, 0.9659258262890683122, 1.000000000000000000, 0.9659258262890683122, 1.000000000000000000, 0.9659258262890683122, 1.000000000000000000, 0.9659258262890683122, 1.000000000000000000, 0.9659258262890683122, 1.000000000000000000, 0.9659258262890683122, 1.000000000000000000, 0.9659258262890683122, 1.000000000000000000, 0.9659258262890683122, 1.000000000000000000, 0.9659258262890683122, 1.000000000000000000, 0.9659258262890683122, 1.000000000000000000, 0.9659258262890683122, 1.000000000000000000, 0.9659258262890683122, 1.000000000000000000, 0.9659258262890683122, 1.000000000000000000, 0.9659258262890683122, 1.000000000000000000, 0.9659258262890683122, 1.000000000000000000, 0.9659258262890683122, 1.000000000000000000, 0.9659258262890683122, 1.000000000000000000, 0.9659258262890683122, 1.000000000000000000, 0.9659258262890683122, 1.000000000000000000, 0.9659258262890683122, 1.000000000000000000, 0.9659258262890683122, 1.000000000000000000, 0.9659258262890683122, 1.000000000000000000, 0.9659258262890683122, 1.000000000000000000, 0.9659258262890683122, 1.000000000000000000, 0.9659258262890683122, 1.000000000000000000, 0.9659258262890683122, 1.000000000000000000, 0.9659258262890683122, 1.000000000000000000, 0.9659258262890683122, 1.000000000000000000, 0.9659258262890683122, 1.000000000000000000, 0.9659258262890683122, 1.000000000000000000, 0.9659258262890683122, 1.000000000000000000, 0.9659258262890683122, 1.000000000000000000, 0.9659258262890683122, 1.000000000000000000, 0.9659258262890683122, 1.000000000000000000, 0.9659258262890683122, 1.000000000000000000) ) ) 
 REPRESENTATION_ITEM ( '' )  SURFACE ( )  );
#18140 = CARTESIAN_POINT ( 'NONE',  ( 17.08211943468705130, 53.47041550158063217, 12.26659068614894998 ) ) ;
#18141 = ORIENTED_EDGE ( 'NONE', *, *, #77829, .T. ) ;
#18142 = CARTESIAN_POINT ( 'NONE',  ( 6.204703633549690345, 50.76208216824730357, -14.16423886937410259 ) ) ;
#18143 = ORIENTED_EDGE ( 'NONE', *, *, #97652, .F. ) ;
#18144 = CARTESIAN_POINT ( 'NONE',  ( 19.42250999205614193, 35.14701867748816966, 5.440088680355555262 ) ) ;
#18145 = CARTESIAN_POINT ( 'NONE',  ( 12.91533473730992121, 34.52201867748817676, 10.88017736071110164 ) ) ;
#18146 = CARTESIAN_POINT ( 'NONE',  ( -27.43587634952537968, 29.50000000000000000, -10.00000000000000000 ) ) ;
#18147 = CARTESIAN_POINT ( 'NONE',  ( 12.91533473730993009, 21.60535201082150536, -10.88017736071109987 ) ) ;
#18148 = DIRECTION ( 'NONE',  ( 0.000000000000000000, 0.000000000000000000, 1.000000000000000000 ) ) ;
#18149 = CARTESIAN_POINT ( 'NONE',  ( 1.472469842513823179, 11.42559781766745175, 4.923371831947296329 ) ) ;
#18150 = CARTESIAN_POINT ( 'NONE',  ( -3.250000000000000444, 1.019547802438453887, 2.500000000000000000 ) ) ;
#18151 = EDGE_LOOP ( 'NONE', ( #9563, #88538, #7582, #86643 ) ) ;
#18152 = CARTESIAN_POINT ( 'NONE',  ( 10.89309003818156718, -97.65096242258067605, 3.999999999994602096 ) ) ;
#18153 = CARTESIAN_POINT ( 'NONE',  ( 19.84674366389459266, 38.30059781766745175, 2.638427012816836559 ) ) ;
#18154 = CARTESIAN_POINT ( 'NONE',  ( 11.48952521350018685, 4.805858850777305443E-16, 8.845383562533823962 ) ) ;
#18155 = ORIENTED_EDGE ( 'NONE', *, *, #37205, .T. ) ;
#18156 = CARTESIAN_POINT ( 'NONE',  ( -11.81378540890925066, 15.00000000000000000, -7.968498874458281200 ) ) ;
#18157 = CARTESIAN_POINT ( 'NONE',  ( 8.209432707284802788, 0.3639311627136676552, 12.55409154915494163 ) ) ;
#18158 = CARTESIAN_POINT ( 'NONE',  ( -4.164238869374098151, 46.59541550158063927, -3.795296366450310543 ) ) ;
#18159 = LINE ( 'NONE', #42621, #78635 ) ;
#18160 = ORIENTED_EDGE ( 'NONE', *, *, #66533, .T. ) ;
#18161 = CARTESIAN_POINT ( 'NONE',  ( 20.03743638938529870, 41.75197528031017669, 6.399506433553907137 ) ) ;
#18162 = CARTESIAN_POINT ( 'NONE',  ( 17.20831665107776587, 14.13393115100078568, -7.208316651077762316 ) ) ;
#18163 = FACE_OUTER_BOUND ( 'NONE', #40378, .T. ) ;
#18164 = CARTESIAN_POINT ( 'NONE',  ( 2.791683348922237240, 65.38393115100078035, -7.208316651077763204 ) ) ;
#18165 = CARTESIAN_POINT ( 'NONE',  ( 7.361572987183170547, 2.050597817667451750, 9.846743663894590881 ) ) ;
#18166 = CARTESIAN_POINT ( 'NONE',  ( 19.84674366389459621, 63.50893115100078745, 7.409399052514197653E-17 ) ) ;
#18167 = CARTESIAN_POINT ( 'NONE',  ( 6.757645195923023707, -58.31151720875058686, -2.750000000000000888 ) ) ;
#18168 = MECHANICAL_DESIGN_GEOMETRIC_PRESENTATION_REPRESENTATION (  '', ( #32574 ), #86832 ) ;
#18169 = ORIENTED_EDGE ( 'NONE', *, *, #33841, .T. ) ;
#18170 = CARTESIAN_POINT ( 'NONE',  ( -4.164238869374099927, 67.01208216824728936, 3.795296366450308767 ) ) ;
#18171 = CARTESIAN_POINT ( 'NONE',  ( 19.72487221294570858, 6.866073187300758107, 6.500000000000000888 ) ) ;
#18172 = CARTESIAN_POINT ( 'NONE',  ( 0.5774900079438590739, 37.64701867748817676, -5.440088680355550821 ) ) ;
#18174 = CARTESIAN_POINT ( 'NONE',  ( 20.88017736071110519, 65.56368534415483396, 2.639326808657452039E-16 ) ) ;
#18173 = CARTESIAN_POINT ( 'NONE',  ( 16.40814093676324603, 12.45696800326375353, -11.09922568453594671 ) ) ;
#18175 = DIRECTION ( 'NONE',  ( 0.4461978131098069400, 0.000000000000000000, -0.8949343616020258851 ) ) ;
#18176 = AXIS2_PLACEMENT_3D ( 'NONE', #84984, #92477, #76987 ) ;
#18177 = CARTESIAN_POINT ( 'NONE',  ( -14.91886229468047986, 14.76984964723649973, -0.8060919667646749831 ) ) ;
#18178 = CARTESIAN_POINT ( 'NONE',  ( 0.2751277870542870319, 54.36607318730131055, -6.499999999999985789 ) ) ;
#18179 = CARTESIAN_POINT ( 'NONE',  ( 0.1532563361054082862, 56.21726448433411605, 2.638427012816831674 ) ) ;
#18180 = CARTESIAN_POINT ( 'NONE',  ( 1.472469842513823179, 5.592264484334118713, -4.923371831947296329 ) ) ;
#18181 = CARTESIAN_POINT ( 'NONE',  ( -5.440088680355558814, -32.76964798917848753, -9.422509992056136596 ) ) ;
#18182 = CARTESIAN_POINT ( 'NONE',  ( -2.816281873526473856, 4.123634669930420493, 9.499525473075851096E-16 ) ) ;
#18183 = ADVANCED_FACE ( 'NONE', ( #67183 ), #12697, .F. ) ;
#18184 = CARTESIAN_POINT ( 'NONE',  ( 15.44008868035555793, 21.39701867748817321, -9.422509992056140149 ) ) ;
#18185 = CYLINDRICAL_SURFACE ( 'NONE', #19627, 0.5000000000000004441 ) ;
#18186 = CARTESIAN_POINT ( 'NONE',  ( 6.204703633549690345, 30.76208216824730357, -14.16423886937410259 ) ) ;
#18187 = CARTESIAN_POINT ( 'NONE',  ( -0.3689425029237898834, 31.17874883491396787, -10.36894250292378850 ) ) ;
#18188 = CARTESIAN_POINT ( 'NONE',  ( 10.00000000000000178, 68.05374883491397497, 14.16423886937410082 ) ) ;
#18189 = CARTESIAN_POINT ( 'NONE',  ( 1.472469842513823179, 46.42559781766745175, 4.923371831947296329 ) ) ;
#18190 = CARTESIAN_POINT ( 'NONE',  ( -2.816281873526471635, 43.91530133659708923, -3.434112377981056508 ) ) ;
#18191 = CARTESIAN_POINT ( 'NONE',  ( 0.5774900079438607392, 13.48035201082150358, 5.440088680355550821 ) ) ;
#18192 = ADVANCED_FACE ( 'NONE', ( #57699 ), #96715, .F. ) ;
#18193 = ORIENTED_EDGE ( 'NONE', *, *, #51498, .T. ) ;
#18194 = CARTESIAN_POINT ( 'NONE',  ( 19.84674366389459621, 33.50893115100078745, 7.409399052514197653E-17 ) ) ;
#18195 = CARTESIAN_POINT ( 'NONE',  ( 0.5774900079438590739, 42.64701867748816966, -5.440088680355550821 ) ) ;
#18196 = CARTESIAN_POINT ( 'NONE',  ( 13.43411237798106583, 7.665301336597086568, -12.81628187352647252 ) ) ;
#18198 = LINE ( 'NONE', #48678, #2441 ) ;
#18197 = CARTESIAN_POINT ( 'NONE',  ( 6.204703633549690345, 20.76208216824730357, -14.16423886937410259 ) ) ;
#18199 = DIRECTION ( 'NONE',  ( 0.000000000000000000, 0.000000000000000000, 1.000000000000000000 ) ) ;
#18200 = EDGE_CURVE ( 'NONE', #43658, #68070, #44799, .T. ) ;
#18201 = UNCERTAINTY_MEASURE_WITH_UNIT (LENGTH_MEASURE( 1.000000000000000082E-05 ), #30257, 'distance_accuracy_value', 'NONE');
#18202 = CARTESIAN_POINT ( 'NONE',  ( 10.00000000000000000, 29.75893115100078745, -9.846743663894594434 ) ) ;
#18203 = CARTESIAN_POINT ( 'NONE',  ( 0.6178305044545818747, 53.49863466993041072, -9.382169495545419124 ) ) ;
#18204 = CARTESIAN_POINT ( 'NONE',  ( 12.63842701281683034, 57.46726448433411605, 9.846743663894596210 ) ) ;
#18205 = ORIENTED_EDGE ( 'NONE', *, *, #59715, .F. ) ;
#18206 = CARTESIAN_POINT ( 'NONE',  ( 8.880000001778796559, -0.01161165531860094795, -4.000000000000000000 ) ) ;
#18207 = CARTESIAN_POINT ( 'NONE',  ( 6.930493939446634499, -71.55570417525920845, 2.750000000000000000 ) ) ;
#18208 = CARTESIAN_POINT ( 'NONE',  ( -4.164238869374098151, 61.59541550158063217, -3.795296366450310543 ) ) ;
#18209 = CARTESIAN_POINT ( 'NONE',  ( 2.035157376598824452, 58.68868534415482685, 7.964842623401179544 ) ) ;
#18210 = CARTESIAN_POINT ( 'NONE',  ( 6.204703633549690345, 7.845415501580634832, 14.16423886937410082 ) ) ;
#18211 = CARTESIAN_POINT ( 'NONE',  ( 7.084665262690076126, 69.10535201082151957, 10.88017736071109987 ) ) ;
#18212 = CARTESIAN_POINT ( 'NONE',  ( 19.84674366389459266, 53.71726448433411605, -2.638427012816827677 ) ) ;
#18213 = CARTESIAN_POINT ( 'NONE',  ( 20.88017736071110875, 15.77201867748817143, -2.915334737309920765 ) ) ;
#18214 = CARTESIAN_POINT ( 'NONE',  ( 18.72515096720583827, 65.05509018479936856, 6.499999999999810818 ) ) ;
#18215 = CARTESIAN_POINT ( 'NONE',  ( 5.076628168052704559, 60.17559781766745175, -8.527530157486179263 ) ) ;
#18216 = ORIENTED_EDGE ( 'NONE', *, *, #11642, .T. ) ;
#18217 = ORIENTED_EDGE ( 'NONE', *, *, #81204, .F. ) ;
#18218 = VERTEX_POINT ( 'NONE', #27696 ) ;
#18219 = DIRECTION ( 'NONE',  ( -0.000000000000000000, -1.000000000000000000, -0.000000000000000000 ) ) ;
#18220 = CARTESIAN_POINT ( 'NONE',  ( 17.08211943468705130, 13.47041550158063572, 12.26659068614894998 ) ) ;
#18221 = CARTESIAN_POINT ( 'NONE',  ( -2.266590686148945544, 2.220415501580634388, 7.082119434687048631 ) ) ;
#18222 = CARTESIAN_POINT ( 'NONE',  ( -0.3689425029237898834, 46.17874883491397497, -10.36894250292378850 ) ) ;
#18223 = CARTESIAN_POINT ( 'NONE',  ( 12.63842701281683034, 57.46726448433411605, 9.846743663894596210 ) ) ;
#18224 = CARTESIAN_POINT ( 'NONE',  ( 19.84674366389459266, 23.71726448433412315, -2.638427012816827677 ) ) ;
#18225 = LINE ( 'NONE', #48214, #7183 ) ;
#18227 = CARTESIAN_POINT ( 'NONE',  ( 19.84674366389459621, 58.50893115100078745, 7.409399052514197653E-17 ) ) ;
#18226 = CARTESIAN_POINT ( 'NONE',  ( 10.00000000000000178, 24.31368534415484106, 10.88017736071110342 ) ) ;
#18228 = CARTESIAN_POINT ( 'NONE',  ( -2.266590686148945544, 36.38708216824730357, -7.082119434687050408 ) ) ;
#18229 = CARTESIAN_POINT ( 'NONE',  ( 19.42250999205614548, 5.980352010821504471, -5.440088680355545492 ) ) ;
#18230 = DIRECTION ( 'NONE',  ( 0.000000000000000000, 1.000000000000000000, 0.000000000000000000 ) ) ;
#18231 = DIRECTION ( 'NONE',  ( 1.000000000000000000, -0.000000000000000000, -0.000000000000000000 ) ) ;
#18232 = CARTESIAN_POINT ( 'NONE',  ( -0.8801773607111008646, 63.27201867748817676, 2.915334737309923430 ) ) ;
#18233 = EDGE_CURVE ( 'NONE', #6181, #79829, #11715, .T. ) ;
#18234 = CARTESIAN_POINT ( 'NONE',  ( 10.00000000000000178, 17.25893115100078745, 9.846743663894594434 ) ) ;
#18235 = CARTESIAN_POINT ( 'NONE',  ( -5.070949216186721564, -24.98410106516554308, 3.749999999997579714 ) ) ;
#18236 = ORIENTED_EDGE ( 'NONE', *, *, #1305, .F. ) ;
#18237 = FACE_OUTER_BOUND ( 'NONE', #85765, .T. ) ;
#18238 = ORIENTED_EDGE ( 'NONE', *, *, #73708, .T. ) ;
#18239 = CARTESIAN_POINT ( 'NONE',  ( 2.791683348922240793, 21.63393115100078745, 7.208316651077764092 ) ) ;
#18240 = VERTEX_POINT ( 'NONE', #36190 ) ;
#18241 = CARTESIAN_POINT ( 'NONE',  ( 20.36894250292379382, 38.67874883491396076, 10.36894250292379205 ) ) ;
#18242 = CARTESIAN_POINT ( 'NONE',  ( 2.791683348922237240, 35.38393115100079456, -7.208316651077763204 ) ) ;
#18243 = CARTESIAN_POINT ( 'NONE',  ( 12.91533473730992121, 49.52201867748817676, 10.88017736071110164 ) ) ;
#18244 =( NAMED_UNIT ( * ) SI_UNIT ( $, .STERADIAN. ) SOLID_ANGLE_UNIT ( ) );
#18245 = CARTESIAN_POINT ( 'NONE',  ( 17.96484262340118221, 36.18868534415484106, -7.964842623401177768 ) ) ;
#18246 = CARTESIAN_POINT ( 'NONE',  ( 20.15039907845753220, 37.62777174578614847, -6.262539305110077947 ) ) ;
#18247 = ORIENTED_EDGE ( 'NONE', *, *, #29663, .T. ) ;
#18248 = TOROIDAL_SURFACE ( 'NONE', #78900, 6.599999999999995204, 0.2500000000000000000 ) ;
#18249 = CARTESIAN_POINT ( 'NONE',  ( -5.204170427930421283E-15, -7.126365330069578619, -12.81628187352647608 ) ) ;
#18250 = ORIENTED_EDGE ( 'NONE', *, *, #75964, .F. ) ;
#18251 = CARTESIAN_POINT ( 'NONE',  ( -0.8801773607111008646, 43.27201867748817676, 2.915334737309923430 ) ) ;
#18252 = CARTESIAN_POINT ( 'NONE',  ( 20.36894250292379382, 3.678748834913967869, 10.36894250292379205 ) ) ;
#18253 = ORIENTED_EDGE ( 'NONE', *, *, #50359, .T. ) ;
#18254 = VECTOR ( 'NONE', #25206, 999.9999999999998863 ) ;
#18255 = EDGE_LOOP ( 'NONE', ( #2783, #41226, #1001, #29889 ) ) ;
#18256 = CARTESIAN_POINT ( 'NONE',  ( 21.09922568453594849, 31.20696800326375353, 6.408140936763242479 ) ) ;
#18257 = CARTESIAN_POINT ( 'NONE',  ( 10.00000000000000178, 22.25893115100078745, 9.846743663894594434 ) ) ;
#18258 = CARTESIAN_POINT ( 'NONE',  ( -8.134956207566176545, 15.00000000000000000, 13.77315809598633756 ) ) ;
#18259 = CARTESIAN_POINT ( 'NONE',  ( 19.38216949554541202, 45.99863466993041072, 9.382169495545424454 ) ) ;
#18260 = CARTESIAN_POINT ( 'NONE',  ( -4.746257547686221656, 0.000000000000000000, 2.685303318749045154 ) ) ;
#18261 = CARTESIAN_POINT ( 'NONE',  ( 5.076628168052703671, 31.84226448433412315, 8.527530157486179263 ) ) ;
#18262 = CARTESIAN_POINT ( 'NONE',  ( 2.035157376598822676, 62.43868534415483396, -7.964842623401177768 ) ) ;
#18263 =( NAMED_UNIT ( * ) PLANE_ANGLE_UNIT ( ) SI_UNIT ( $, .RADIAN. ) );
#18264 = CARTESIAN_POINT ( 'NONE',  ( 12.91533473730993009, 66.60535201082150536, -10.88017736071109987 ) ) ;
#18265 = CARTESIAN_POINT ( 'NONE',  ( 11.22915323889574601, -0.03417435944610275333, 8.773176023390684364 ) ) ;
#18266 = CARTESIAN_POINT ( 'NONE',  ( 0.6178305044545838731, 64.74863466993043914, 9.382169495545420901 ) ) ;
#18267 = CARTESIAN_POINT ( 'NONE',  ( 0.1532563361054082862, 1.217264484334117824, 2.638427012816831674 ) ) ;
#18268 = CARTESIAN_POINT ( 'NONE',  ( 19.38216949554541202, 15.99863466993042138, 9.382169495545424454 ) ) ;
#18269 = CARTESIAN_POINT ( 'NONE',  ( -45.70923076923077133, 100.3461538461538538, -9.500000000000000000 ) ) ;
#18270 = EDGE_CURVE ( 'NONE', #49843, #30282, #20692, .T. ) ;
#18271 = CARTESIAN_POINT ( 'NONE',  ( 10.00000000000000000, 44.75893115100078745, -9.846743663894594434 ) ) ;
#18272 = DIRECTION ( 'NONE',  ( 1.000000000000000000, 2.107602052970794797E-16, -0.000000000000000000 ) ) ;
#18273 = CARTESIAN_POINT ( 'NONE',  ( 13.79529636645030344, 3.262082168247301350, 14.16423886937410614 ) ) ;
#18274 = CARTESIAN_POINT ( 'NONE',  ( 14.92337183194729988, 39.34226448433412315, -8.527530157486177487 ) ) ;
#18275 = CARTESIAN_POINT ( 'NONE',  ( 10.00000000000000000, 27.87363466993042138, -12.81628187352647608 ) ) ;
#18276 = CARTESIAN_POINT ( 'NONE',  ( 1.274849032794324932, 22.55509018479936145, -6.500000000000021316 ) ) ;
#18277 = CARTESIAN_POINT ( 'NONE',  ( 4.559911319644449179, 48.89701867748817676, 9.422509992056141925 ) ) ;
#18278 = CARTESIAN_POINT ( 'NONE',  ( 21.09922568453595559, 12.04030133659708746, -6.408140936763230044 ) ) ;
#18279 = CARTESIAN_POINT ( 'NONE',  ( 9.876730923139225737, 15.00000000000000000, 11.28938378619069560 ) ) ;
#18281 = EDGE_CURVE ( 'NONE', #86312, #4683, #68578, .T. ) ;
#18280 = CIRCLE ( 'NONE', #58366, 15.00000000000000000 ) ;
#18282 = CARTESIAN_POINT ( 'NONE',  ( 2.791683348922240793, 21.63393115100078745, 7.208316651077764092 ) ) ;
#18283 = CARTESIAN_POINT ( 'NONE',  ( 12.91533473730993009, 26.60535201082150536, -10.88017736071109987 ) ) ;
#18284 = CARTESIAN_POINT ( 'NONE',  ( 19.38216949554541202, 35.99863466993041072, 9.382169495545424454 ) ) ;
#18285 = CARTESIAN_POINT ( 'NONE',  ( 14.92337183194729988, 24.34226448433411960, -8.527530157486177487 ) ) ;
#18286 = CARTESIAN_POINT ( 'NONE',  ( -9.538220187641574199, 88.39559135149089286, 5.063080553069074341 ) ) ;
#18287 = CARTESIAN_POINT ( 'NONE',  ( 15.44008868035555793, 36.39701867748816966, -9.422509992056140149 ) ) ;
#18288 = EDGE_LOOP ( 'NONE', ( #82799, #11230, #22870, #85996 ) ) ;
#18289 = CARTESIAN_POINT ( 'NONE',  ( 19.42250999205614193, 60.14701867748817676, 5.440088680355555262 ) ) ;
#18291 = CARTESIAN_POINT ( 'NONE',  ( 7.084665262690076126, 37.02201867748817676, -10.88017736071110164 ) ) ;
#18290 = CARTESIAN_POINT ( 'NONE',  ( 18.52753015748618282, 43.92559781766745175, -4.923371831947291888 ) ) ;
#18292 = LINE ( 'NONE', #25797, #23218 ) ;
#18293 = CARTESIAN_POINT ( 'NONE',  ( 19.42250999205614548, 45.98035201082150536, -5.440088680355545492 ) ) ;
#18295 = FILL_AREA_STYLE ('',( #24823 ) ) ;
#18294 = CARTESIAN_POINT ( 'NONE',  ( 12.91533473730992121, 9.522018677488171434, 10.88017736071110164 ) ) ;
#18296 = CARTESIAN_POINT ( 'NONE',  ( 10.70613742633258170, 4.237152514796235822E-16, -9.778988772285240216 ) ) ;
#18297 = CARTESIAN_POINT ( 'NONE',  ( 7.361572987183169658, 39.96726448433411605, -9.846743663894592657 ) ) ;
#18299 = CARTESIAN_POINT ( 'NONE',  ( 3.640395162852212874, 107.5383484153110203, 12.00000000000000000 ) ) ;
#18298 = CARTESIAN_POINT ( 'NONE',  ( -2.266590686148945544, 46.38708216824730357, -7.082119434687050408 ) ) ;
#18300 = DIRECTION ( 'NONE',  ( -0.000000000000000000, 0.000000000000000000, 1.000000000000000000 ) ) ;
#18301 = CARTESIAN_POINT ( 'NONE',  ( -12.60589901313211492, 14.63595249122789177, -8.129656208642225934 ) ) ;
#18302 = CARTESIAN_POINT ( 'NONE',  ( 17.08211943468705840, 30.13708216824730357, -12.26659068614894466 ) ) ;
#18303 = B_SPLINE_CURVE_WITH_KNOTS ( 'NONE', 3,
 ( #88437, #80939, #12432, #4947, #42940, #35428 ),
 .UNSPECIFIED., .F., .F.,
 ( 4, 2, 4 ),
 ( 0.0002800047503720793978, 0.0006862100262544194602, 0.001092415302136759414 ),
 .UNSPECIFIED. ) ;
#18304 = EDGE_CURVE ( 'NONE', #87018, #10746, #4928, .T. ) ;
#18305 = CARTESIAN_POINT ( 'NONE',  ( 11.62719953690060137, 14.63606895804700514, 9.476720473301911696 ) ) ;
#18306 = ORIENTED_EDGE ( 'NONE', *, *, #93228, .T. ) ;
#18307 = CARTESIAN_POINT ( 'NONE',  ( 10.00000000000000000, 1.813685344154838175, -10.88017736071110342 ) ) ;
#18308 = CARTESIAN_POINT ( 'NONE',  ( 10.00000000000000000, 34.75893115100078745, -9.846743663894594434 ) ) ;
#18310 = CARTESIAN_POINT ( 'NONE',  ( 6.880000000000007887, 41.24999999999999289, -6.500000000000000888 ) ) ;
#18309 = DIRECTION ( 'NONE',  ( -1.000000000000000000, 0.000000000000000000, 0.000000000000000000 ) ) ;
#18311 = CARTESIAN_POINT ( 'NONE',  ( 7.084665262690076126, 64.10535201082150536, 10.88017736071109987 ) ) ;
#18312 = CARTESIAN_POINT ( 'NONE',  ( 5.419894505350494107, 14.63595249122791664, 13.98659156302463025 ) ) ;
#18313 = AXIS2_PLACEMENT_3D ( 'NONE', #48423, #32434, #47925 ) ;
#18314 = EDGE_CURVE ( 'NONE', #83450, #98073, #82173, .T. ) ;
#18315 = CARTESIAN_POINT ( 'NONE',  ( 15.44008868035555793, 31.39701867748817676, -9.422509992056140149 ) ) ;
#18316 = CARTESIAN_POINT ( 'NONE',  ( 22.81628187352647785, 56.62363466993042493, 6.195893100308588602E-16 ) ) ;
#18317 = CARTESIAN_POINT ( 'NONE',  ( 0.6178305044545818747, 13.49863466993041783, -9.382169495545419124 ) ) ;
#18318 = CARTESIAN_POINT ( 'NONE',  ( 17.20831665107776587, 14.13393115100078568, -7.208316651077762316 ) ) ;
#18319 = ORIENTED_EDGE ( 'NONE', *, *, #42103, .T. ) ;
#18320 = LINE ( 'NONE', #9838, #52613 ) ;
#18321 = CARTESIAN_POINT ( 'NONE',  ( 10.00000000000000000, 6.813685344154838397, -10.88017736071110342 ) ) ;
#18322 = CARTESIAN_POINT ( 'NONE',  ( 6.204703633549690345, 25.76208216824730712, -14.16423886937410259 ) ) ;
#18323 = CARTESIAN_POINT ( 'NONE',  ( 15.44008868035555793, 36.39701867748816966, -9.422509992056140149 ) ) ;
#18324 = CARTESIAN_POINT ( 'NONE',  ( 15.44008868035555793, 46.39701867748817676, -9.422509992056140149 ) ) ;
#18325 = DIRECTION ( 'NONE',  ( 0.000000000000000000, -1.000000000000000000, 0.000000000000000000 ) ) ;
#18326 = CARTESIAN_POINT ( 'NONE',  ( -7.684764310694707667, 0.5000000000000004441, -12.88194075009945472 ) ) ;
#18327 = CARTESIAN_POINT ( 'NONE',  ( 10.00000000000000178, 12.25893115100078568, 9.846743663894594434 ) ) ;
#18328 = PRESENTATION_STYLE_ASSIGNMENT (( #2855 ) ) ;
#18329 = CARTESIAN_POINT ( 'NONE',  ( 1.472469842513823179, 25.59226448433412315, -4.923371831947296329 ) ) ;
#18330 = CARTESIAN_POINT ( 'NONE',  ( 10.00000000000000000, -0.2410688489992152128, -9.846743663894594434 ) ) ;
#18331 =( BOUNDED_CURVE ( )  B_SPLINE_CURVE ( 2, ( #65795, #64801, #95320, #26821, #43300, #66291, #57314, #87807, #80319 ),
 .UNSPECIFIED., .F., .T. ) 
 B_SPLINE_CURVE_WITH_KNOTS ( ( 3, 2, 2, 2, 3 ),
 ( 0.6891432315068940495, 0.6904761904761904656, 0.6964285714285713969, 0.7023809523809523281, 0.7037139113502487442 ),
 .UNSPECIFIED. ) 
 CURVE ( )  GEOMETRIC_REPRESENTATION_ITEM ( )  RATIONAL_B_SPLINE_CURVE ( ( 0.9881565478350733400, 0.9923695281211490915, 1.000000000000000000, 0.9659258262890683122, 1.000000000000000000, 0.9659258262890683122, 1.000000000000000000, 0.9923695281211492025, 0.9881565478350733400 ) ) 
 REPRESENTATION_ITEM ( '' )  );
#18332 = LINE ( 'NONE', #48812, #43139 ) ;
#18333 = CARTESIAN_POINT ( 'NONE',  ( 18.52753015748617571, 18.09226448433411960, 4.923371831947298993 ) ) ;
#18334 = CARTESIAN_POINT ( 'NONE',  ( 0.1532563361054083140, 46.00893115100079456, 1.131784320476157264E-15 ) ) ;
#18335 = CARTESIAN_POINT ( 'NONE',  ( 19.38216949554541557, 42.24863466993041783, -9.382169495545420901 ) ) ;
#18336 = MECHANICAL_DESIGN_GEOMETRIC_PRESENTATION_REPRESENTATION (  '', ( #10343 ), #74190 ) ;
#18337 = CARTESIAN_POINT ( 'NONE',  ( 2.035157376598822676, 52.43868534415483396, -7.964842623401177768 ) ) ;
#18338 = CARTESIAN_POINT ( 'NONE',  ( 7.361572987183169658, 24.96726448433412315, -9.846743663894592657 ) ) ;
#18341 = EDGE_CURVE ( 'NONE', #57109, #72221, #81556, .T. ) ;
#18340 = CARTESIAN_POINT ( 'NONE',  ( 7.361572987183169658, 19.96726448433411960, -9.846743663894592657 ) ) ;
#18339 = CARTESIAN_POINT ( 'NONE',  ( -2.266590686148945544, 51.38708216824730357, -7.082119434687050408 ) ) ;
#18342 = CARTESIAN_POINT ( 'NONE',  ( -0.4427729075171647488, 14.61885305295417758, -9.500000000000000000 ) ) ;
#18343 = CARTESIAN_POINT ( 'NONE',  ( 7.361572987183169658, 59.96726448433410894, -9.846743663894592657 ) ) ;
#18344 = CARTESIAN_POINT ( 'NONE',  ( 2.917880565312950480, 10.97041550158063572, -12.26659068614894821 ) ) ;
#18345 = CARTESIAN_POINT ( 'NONE',  ( 10.00000000000000000, 35.55374883491396787, -14.16423886937410082 ) ) ;
#18346 = CARTESIAN_POINT ( 'NONE',  ( 19.84674366389459266, 28.71726448433411960, -2.638427012816827677 ) ) ;
#18347 = FACE_OUTER_BOUND ( 'NONE', #73572, .T. ) ;
#18348 = CARTESIAN_POINT ( 'NONE',  ( 10.00000000000000178, 24.31368534415484106, 10.88017736071110342 ) ) ;
#18349 = EDGE_CURVE ( 'NONE', #18961, #16062, #74681, .T. ) ;
#18350 = CARTESIAN_POINT ( 'NONE',  ( 15.44008868035555793, 46.39701867748817676, -9.422509992056140149 ) ) ;
#18351 = CARTESIAN_POINT ( 'NONE',  ( 7.084665262690076126, 49.10535201082149825, 10.88017736071109987 ) ) ;
#18352 = VERTEX_POINT ( 'NONE', #28682 ) ;
#18353 = CARTESIAN_POINT ( 'NONE',  ( 21.09922568453594849, 36.20696800326375353, 6.408140936763242479 ) ) ;
#18354 = CARTESIAN_POINT ( 'NONE',  ( 17.96484262340118221, 51.18868534415483396, -7.964842623401177768 ) ) ;
#18355 = ORIENTED_EDGE ( 'NONE', *, *, #22774, .F. ) ;
#18356 = CIRCLE ( 'NONE', #59881, 14.49999999999999822 ) ;
#18357 = CARTESIAN_POINT ( 'NONE',  ( -36.44000000000001194, 92.00000000000000000, 9.500000000000000000 ) ) ;
#18358 = CARTESIAN_POINT ( 'NONE',  ( -0.8801773607111009756, 68.06368534415484817, 1.068504757029289695E-15 ) ) ;
#18359 = ORIENTED_EDGE ( 'NONE', *, *, #67868, .T. ) ;
#18360 = CARTESIAN_POINT ( 'NONE',  ( -0.8801773607111009756, 63.06368534415484106, 1.068504757029289695E-15 ) ) ;
#18361 = CARTESIAN_POINT ( 'NONE',  ( 10.00000000000000178, 4.313685344154837509, 10.88017736071110342 ) ) ;
#18362 = FACE_OUTER_BOUND ( 'NONE', #90298, .T. ) ;
#18363 = CARTESIAN_POINT ( 'NONE',  ( -0.8801773607111008646, 3.272018677488171434, 2.915334737309923430 ) ) ;
#18364 = CARTESIAN_POINT ( 'NONE',  ( 18.52753015748618282, 8.925597817667451750, -4.923371831947291888 ) ) ;
#18365 = CARTESIAN_POINT ( 'NONE',  ( 13.79529636645030344, 8.262082168247300018, 14.16423886937410614 ) ) ;
#18366 = CARTESIAN_POINT ( 'NONE',  ( 7.361572987183170547, 2.050597817667451750, 9.846743663894590881 ) ) ;
#18367 = CARTESIAN_POINT ( 'NONE',  ( 20.88017736071110875, 10.77201867748817143, -2.915334737309920765 ) ) ;
#18368 = CARTESIAN_POINT ( 'NONE',  ( 14.92337183194729633, 42.67559781766745886, 8.527530157486181039 ) ) ;
#18369 = ORIENTED_EDGE ( 'NONE', *, *, #37323, .F. ) ;
#18370 = CARTESIAN_POINT ( 'NONE',  ( 12.63842701281683922, 54.55059781766745175, -9.846743663894590881 ) ) ;
#18371 = ORIENTED_EDGE ( 'NONE', *, *, #25344, .F. ) ;
#18372 = CARTESIAN_POINT ( 'NONE',  ( -10.14667048435130781, 4.359436697371537845E-16, -10.35833375027055148 ) ) ;
#18373 = AXIS2_PLACEMENT_3D ( 'NONE', #37298, #29762, #51293 ) ;
#18374 = CARTESIAN_POINT ( 'NONE',  ( 12.91533473730993009, 51.60535201082149825, -10.88017736071109987 ) ) ;
#18375 = CARTESIAN_POINT ( 'NONE',  ( 17.20831665107776587, 54.13393115100079456, -7.208316651077762316 ) ) ;
#18376 = CARTESIAN_POINT ( 'NONE',  ( 3.591859063236763294, 28.29030133659708568, -11.09922568453595026 ) ) ;
#18378 = CARTESIAN_POINT ( 'NONE',  ( -0.8801773607111009756, 68.06368534415484817, 1.068504757029289695E-15 ) ) ;
#18377 = CARTESIAN_POINT ( 'NONE',  ( -13.55255535720598026, 15.00000000000000000, 4.403492169842870396 ) ) ;
#18379 = CARTESIAN_POINT ( 'NONE',  ( 4.559911319644449179, 62.23035201082150536, -9.422509992056141925 ) ) ;
#18380 = CARTESIAN_POINT ( 'NONE',  ( -2.266590686148945544, 66.38708216824730357, -7.082119434687050408 ) ) ;
#18381 = PRODUCT_DEFINITION_FORMATION_WITH_SPECIFIED_SOURCE ( 'ANY', '', #5926, .NOT_KNOWN. ) ;
#18382 = CARTESIAN_POINT ( 'NONE',  ( 22.81628187352647785, 46.62363466993041783, 6.195893100308588602E-16 ) ) ;
#18383 = ORIENTED_EDGE ( 'NONE', *, *, #36481, .F. ) ;
#18384 = CIRCLE ( 'NONE', #74242, 0.09999999999999939493 ) ;
#18385 = CARTESIAN_POINT ( 'NONE',  ( 0.6178305044545818747, 28.49863466993041783, -9.382169495545419124 ) ) ;
#18386 = CARTESIAN_POINT ( 'NONE',  ( 2.035157376598824452, 38.68868534415483396, 7.964842623401179544 ) ) ;
#18387 = VERTEX_POINT ( 'NONE', #81675 ) ;
#18388 = CARTESIAN_POINT ( 'NONE',  ( 7.361572987183170547, 62.05059781766745886, 9.846743663894590881 ) ) ;
#18390 = CARTESIAN_POINT ( 'NONE',  ( 19.84674366389459621, 48.50893115100078745, 7.409399052514197653E-17 ) ) ;
#18389 = CARTESIAN_POINT ( 'NONE',  ( 0.1532563361054082862, 11.21726448433411605, 2.638427012816831674 ) ) ;
#18391 = CARTESIAN_POINT ( 'NONE',  ( -10.85079341422219734, -98.11281374797032129, 3.750000000000000888 ) ) ;
#18392 = CARTESIAN_POINT ( 'NONE',  ( -14.71525861348289510, 14.63606890215620915, -2.908807992686800237 ) ) ;
#18393 = LINE ( 'NONE', #55407, #72679 ) ;
#18394 = ADVANCED_FACE ( 'NONE', ( #19709 ), #35696, .T. ) ;
#18396 = CARTESIAN_POINT ( 'NONE',  ( 1.472469842513823179, 0.5922644843341181575, -4.923371831947296329 ) ) ;
#18395 = CARTESIAN_POINT ( 'NONE',  ( 19.84674366389459266, 33.71726448433410894, -2.638427012816827677 ) ) ;
#18398 = ORIENTED_EDGE ( 'NONE', *, *, #82949, .T. ) ;
#18397 = CARTESIAN_POINT ( 'NONE',  ( 10.00000000000000178, 57.25893115100078745, 9.846743663894594434 ) ) ;
#18399 = FACE_OUTER_BOUND ( 'NONE', #12583, .T. ) ;
#18400 = CARTESIAN_POINT ( 'NONE',  ( -1.099225684535947600, 23.70696800326375708, -6.408140936763238038 ) ) ;
#18401 = AXIS2_PLACEMENT_3D ( 'NONE', #7257, #98777, #31212 ) ;
#18402 = CARTESIAN_POINT ( 'NONE',  ( 0.1532563361054100626, 50.80059781766745175, -2.638427012816831230 ) ) ;
#18403 = DIRECTION ( 'NONE',  ( 0.000000000000000000, 0.000000000000000000, 1.000000000000000000 ) ) ;
#18404 = CARTESIAN_POINT ( 'NONE',  ( 24.16423886937410614, 49.51208216824730357, -3.795296366450302550 ) ) ;
#18405 = CARTESIAN_POINT ( 'NONE',  ( 5.076628168052704559, 15.17559781766745175, -8.527530157486179263 ) ) ;
#18406 = ORIENTED_EDGE ( 'NONE', *, *, #19779, .T. ) ;
#18407 = DIRECTION ( 'NONE',  ( 0.000000000000000000, 0.000000000000000000, 1.000000000000000000 ) ) ;
#18408 = CARTESIAN_POINT ( 'NONE',  ( -4.164238869374099927, 52.01208216824729647, 3.795296366450308767 ) ) ;
#18409 = CARTESIAN_POINT ( 'NONE',  ( 0.1532563361054083140, 56.00893115100078745, 1.131784320476157264E-15 ) ) ;
#18410 = CARTESIAN_POINT ( 'NONE',  ( 12.91533473730992121, 9.522018677488171434, 10.88017736071110164 ) ) ;
#18411 = CARTESIAN_POINT ( 'NONE',  ( 24.16423886937410614, 39.51208216824731068, -3.795296366450302550 ) ) ;
#18412 = CARTESIAN_POINT ( 'NONE',  ( 24.16423886937410614, 44.30374883491397497, 8.672049930838204340E-16 ) ) ;
#18413 = CARTESIAN_POINT ( 'NONE',  ( -15.00000000000004974, 91.00000000000000000, 7.750000000000000000 ) ) ;
#18415 = CARTESIAN_POINT ( 'NONE',  ( 19.84674366389459266, 58.30059781766745886, 2.638427012816836559 ) ) ;
#18414 = CARTESIAN_POINT ( 'NONE',  ( -13.78891971893215107, 0.3639314269420583781, 5.904717858191459889 ) ) ;
#18416 = VERTEX_POINT ( 'NONE', #51694 ) ;
#18417 = CARTESIAN_POINT ( 'NONE',  ( 10.00000000000000000, 31.81368534415483751, -10.88017736071110342 ) ) ;
#18418 = DIRECTION ( 'NONE',  ( 0.000000000000000000, -1.000000000000000000, 0.000000000000000000 ) ) ;
#18419 = VECTOR ( 'NONE', #96595, 1000.000000000000000 ) ;
#18420 = CARTESIAN_POINT ( 'NONE',  ( 20.00000000000000711, 98.59912998021083297, -4.999999999999999112 ) ) ;
#18421 = CARTESIAN_POINT ( 'NONE',  ( 18.52753015748618282, 53.92559781766745175, -4.923371831947291888 ) ) ;
#18422 = CYLINDRICAL_SURFACE ( 'NONE', #77762, 0.5000000000000004441 ) ;
#18423 = CARTESIAN_POINT ( 'NONE',  ( 14.16423886937410082, 4.512082168247307123, -3.795296366450314096 ) ) ;
#18424 = CARTESIAN_POINT ( 'NONE',  ( 1.472469842513823179, 61.42559781766745175, 4.923371831947296329 ) ) ;
#18425 = LINE ( 'NONE', #79424, #67319 ) ;
#18426 = ADVANCED_FACE ( 'NONE', ( #66180 ), #13686, .T. ) ;
#18427 = ORIENTED_EDGE ( 'NONE', *, *, #95849, .F. ) ;
#18428 = AXIS2_PLACEMENT_3D ( 'NONE', #98278, #15752, #761 ) ;
#18429 = CARTESIAN_POINT ( 'NONE',  ( 13.79529636645030344, 33.26208216824730357, 14.16423886937410614 ) ) ;
#18430 = FACE_OUTER_BOUND ( 'NONE', #34094, .T. ) ;
#18432 = CARTESIAN_POINT ( 'NONE',  ( 19.10478245763052030, 45.10160829253886305, 5.990408912944319653 ) ) ;
#18431 = CARTESIAN_POINT ( 'NONE',  ( -6.356892395138682872, -50.94284410517786910, -2.500000000000000000 ) ) ;
#18433 = CARTESIAN_POINT ( 'NONE',  ( 20.88017736071110519, 15.56368534415483751, 2.639326808657452039E-16 ) ) ;
#18434 = CARTESIAN_POINT ( 'NONE',  ( -1.099225684535947600, 24.54030133659708923, 6.408140936763237150 ) ) ;
#18435 = EDGE_CURVE ( 'NONE', #66580, #30184, #22484, .T. ) ;
#18436 = CARTESIAN_POINT ( 'NONE',  ( 11.29168986245494644, 14.76984976272934169, -9.783658503027382380 ) ) ;
#18437 = CARTESIAN_POINT ( 'NONE',  ( 19.84674366389459621, 13.50893115100078568, 7.409399052514197653E-17 ) ) ;
#18438 = CARTESIAN_POINT ( 'NONE',  ( 0.1532563361054082862, 21.21726448433411605, 2.638427012816831674 ) ) ;
#18439 = CARTESIAN_POINT ( 'NONE',  ( -7.322384435959395255, -84.40865712959148937, 3.999999999999999112 ) ) ;
#18440 = CARTESIAN_POINT ( 'NONE',  ( 4.559911319644449179, 12.23035201082150714, -9.422509992056141925 ) ) ;
#18441 = AXIS2_PLACEMENT_3D ( 'NONE', #46061, #38079, #7587 ) ;
#18442 = DIRECTION ( 'NONE',  ( -0.3665012267243009103, 0.000000000000000000, 0.9304175679820231304 ) ) ;
#18443 = CARTESIAN_POINT ( 'NONE',  ( 10.00000000000000178, 34.31368534415484106, 10.88017736071110342 ) ) ;
#18444 = CARTESIAN_POINT ( 'NONE',  ( 20.88017736071110519, 35.56368534415484106, 2.639326808657452039E-16 ) ) ;
#18445 = CARTESIAN_POINT ( 'NONE',  ( -2.816281873526473856, -0.8763653300695799508, 9.499525473075851096E-16 ) ) ;
#18446 = CARTESIAN_POINT ( 'NONE',  ( -13.03370038005733456, -0.03417435944610275333, 9.273621236547603175 ) ) ;
#18447 = CARTESIAN_POINT ( 'NONE',  ( -46.02116055762927971, 104.3980163073828606, -5.346303181598003995 ) ) ;
#18448 = CARTESIAN_POINT ( 'NONE',  ( 14.92337183194729988, 4.342264484334117824, -8.527530157486177487 ) ) ;
#18449 = ORIENTED_EDGE ( 'NONE', *, *, #9604, .F. ) ;
#18450 = CARTESIAN_POINT ( 'NONE',  ( 10.00000000000000178, 29.31368534415483751, 10.88017736071110342 ) ) ;
#18451 = CARTESIAN_POINT ( 'NONE',  ( 0.6178305044545818747, 33.49863466993042493, -9.382169495545419124 ) ) ;
#18452 = VECTOR ( 'NONE', #62589, 1000.000000000000000 ) ;
#18453 = CARTESIAN_POINT ( 'NONE',  ( 0.1532563361054082862, 66.21726448433413736, 2.638427012816831674 ) ) ;
#18454 = CARTESIAN_POINT ( 'NONE',  ( 0.5774900079438590739, 57.64701867748817676, -5.440088680355550821 ) ) ;
#18455 = VECTOR ( 'NONE', #94059, 1000.000000000000000 ) ;
#18456 = CARTESIAN_POINT ( 'NONE',  ( 7.361572987183170547, 17.05059781766745530, 9.846743663894590881 ) ) ;
#18457 = CARTESIAN_POINT ( 'NONE',  ( 22.81628187352647785, 31.62363466993042138, 6.195893100308588602E-16 ) ) ;
#18458 = CARTESIAN_POINT ( 'NONE',  ( 7.361572987183170547, 7.050597817667451750, 9.846743663894590881 ) ) ;
#18459 = ORIENTED_EDGE ( 'NONE', *, *, #7012, .T. ) ;
#18460 = CYLINDRICAL_SURFACE ( 'NONE', #43029, 1.249999999999987121 ) ;
#18461 = CARTESIAN_POINT ( 'NONE',  ( 10.00000000000000000, 11.81368534415483751, -10.88017736071110342 ) ) ;
#18463 = CARTESIAN_POINT ( 'NONE',  ( -2.266590686148945544, 27.22041550158063572, 7.082119434687048631 ) ) ;
#18462 = CARTESIAN_POINT ( 'NONE',  ( -2.816281873526473856, 54.33196800326376064, 3.434112377981055619 ) ) ;
#18464 = CARTESIAN_POINT ( 'NONE',  ( 0.1532563361054100626, 15.80059781766745353, -2.638427012816831230 ) ) ;
#18465 = CARTESIAN_POINT ( 'NONE',  ( 20.88017736071110875, 10.77201867748817143, -2.915334737309920765 ) ) ;
#18466 = CARTESIAN_POINT ( 'NONE',  ( 5.076628168052703671, 26.84226448433411960, 8.527530157486179263 ) ) ;
#18467 = CARTESIAN_POINT ( 'NONE',  ( -4.164238869374098151, 66.59541550158060375, -3.795296366450310543 ) ) ;
#18468 = ORIENTED_EDGE ( 'NONE', *, *, #90664, .F. ) ;
#18469 = CARTESIAN_POINT ( 'NONE',  ( 15.44008868035555260, 9.730352010821505360, 9.422509992056143702 ) ) ;
#18470 = EDGE_CURVE ( 'NONE', #54853, #62857, #43449, .T. ) ;
#18471 = CARTESIAN_POINT ( 'NONE',  ( 4.559911319644449179, 18.89701867748817321, 9.422509992056141925 ) ) ;
#18472 = CARTESIAN_POINT ( 'NONE',  ( 2.603489959281115151, 16.58210964143323807, 6.499999999999462652 ) ) ;
#18473 = ORIENTED_EDGE ( 'NONE', *, *, #54980, .T. ) ;
#18474 = CARTESIAN_POINT ( 'NONE',  ( 10.00000000000000000, 64.75893115100078035, -9.846743663894594434 ) ) ;
#18475 = CARTESIAN_POINT ( 'NONE',  ( 2.035157376598824452, 28.68868534415484106, 7.964842623401179544 ) ) ;
#18476 = CARTESIAN_POINT ( 'NONE',  ( 14.92337183194729988, 59.34226448433412315, -8.527530157486177487 ) ) ;
#18477 = CIRCLE ( 'NONE', #69577, 0.5000000000000004441 ) ;
#18478 = FACE_OUTER_BOUND ( 'NONE', #5821, .T. ) ;
#18479 = LINE ( 'NONE', #50439, #26850 ) ;
#18480 = CARTESIAN_POINT ( 'NONE',  ( 22.26659068614895176, 39.72041550158063217, -7.082119434687042414 ) ) ;
#18481 = CARTESIAN_POINT ( 'NONE',  ( 12.91533473730992121, 44.52201867748816966, 10.88017736071110164 ) ) ;
#18482 = CARTESIAN_POINT ( 'NONE',  ( 20.88017736071110164, 20.35535201082150891, 2.915334737309930979 ) ) ;
#18483 = CARTESIAN_POINT ( 'NONE',  ( 2.791683348922237240, 55.38393115100078745, -7.208316651077763204 ) ) ;
#18484 = CARTESIAN_POINT ( 'NONE',  ( -11.58008864090154688, -84.10931438318498010, -3.750000000000000444 ) ) ;
#18485 = CARTESIAN_POINT ( 'NONE',  ( 19.84674366389459621, 33.50893115100078745, 7.409399052514197653E-17 ) ) ;
#18486 = CARTESIAN_POINT ( 'NONE',  ( 17.20831665107776587, 2.883931151000785231, 7.208316651077764980 ) ) ;
#18487 = CARTESIAN_POINT ( 'NONE',  ( 11.09922568453594671, -32.95969866340291077, -6.408140936763241591 ) ) ;
#18488 = VERTEX_POINT ( 'NONE', #34699 ) ;
#18489 = CARTESIAN_POINT ( 'NONE',  ( 17.96484262340118221, 14.93868534415483751, 7.964842623401181321 ) ) ;
#18490 = CARTESIAN_POINT ( 'NONE',  ( 14.92337183194729988, 9.342264484334119601, -8.527530157486177487 ) ) ;
#18491 = CARTESIAN_POINT ( 'NONE',  ( -1.099225684535947600, -0.4596986634029132657, 6.408140936763237150 ) ) ;
#18492 = CARTESIAN_POINT ( 'NONE',  ( 20.88017736071110164, 45.35535201082149115, 2.915334737309930979 ) ) ;
#18494 = CARTESIAN_POINT ( 'NONE',  ( 3.591859063236761518, 39.95696800326375353, 11.09922568453594849 ) ) ;
#18493 = CARTESIAN_POINT ( 'NONE',  ( 20.88017736071110164, 15.35535201082150358, 2.915334737309930979 ) ) ;
#18495 = CARTESIAN_POINT ( 'NONE',  ( -4.164238869374099927, 37.01208216824731068, 3.795296366450308767 ) ) ;
#18496 = VECTOR ( 'NONE', #68717, 1000.000000000000000 ) ;
#18497 = CARTESIAN_POINT ( 'NONE',  ( -2.816281873526471635, 63.91530133659708923, -3.434112377981056508 ) ) ;
#18498 = VERTEX_POINT ( 'NONE', #65193 ) ;
#18499 = CARTESIAN_POINT ( 'NONE',  ( 18.52753015748618282, 63.92559781766745886, -4.923371831947291888 ) ) ;
#18500 = CARTESIAN_POINT ( 'NONE',  ( -0.2418659066527494572, 14.26028685723174050, -6.114288769123083611 ) ) ;
#18501 = CARTESIAN_POINT ( 'NONE',  ( 0.5774900079438590739, 32.64701867748816966, -5.440088680355550821 ) ) ;
#18502 = EDGE_LOOP ( 'NONE', ( #41140, #47514, #26704, #55378 ) ) ;
#18504 = CARTESIAN_POINT ( 'NONE',  ( -3.250000000000000888, 0.08822490956012897512, 2.500000000000000000 ) ) ;
#18503 = CARTESIAN_POINT ( 'NONE',  ( 18.52753015748617571, 3.092264484334118269, 4.923371831947298993 ) ) ;
#18505 = CARTESIAN_POINT ( 'NONE',  ( 67.06412365047464164, 26.99999999999997868, -10.00000000000000000 ) ) ;
#18506 = CARTESIAN_POINT ( 'NONE',  ( 19.84674366389459266, 28.71726448433411960, -2.638427012816827677 ) ) ;
#18507 = CARTESIAN_POINT ( 'NONE',  ( 19.84674366389459266, 8.300597817667451750, 2.638427012816836559 ) ) ;
#18508 = CARTESIAN_POINT ( 'NONE',  ( 10.00000000000000178, 7.258931151000785675, 9.846743663894594434 ) ) ;
#18509 = EDGE_CURVE ( 'NONE', #61145, #24437, #73559, .T. ) ;
#18511 = DIRECTION ( 'NONE',  ( 0.2334453638559024768, -0.000000000000000000, 0.9723699203976773342 ) ) ;
#18510 = CARTESIAN_POINT ( 'NONE',  ( 2.035157376598822676, 57.43868534415484106, -7.964842623401177768 ) ) ;
#18512 = CARTESIAN_POINT ( 'NONE',  ( 2.035157376598822676, 62.43868534415483396, -7.964842623401177768 ) ) ;
#18513 = TOROIDAL_SURFACE ( 'NONE', #47262, 1.000000000000000000, 0.5000000000000000000 ) ;
#18515 = ORIENTED_EDGE ( 'NONE', *, *, #43101, .F. ) ;
#18514 = CARTESIAN_POINT ( 'NONE',  ( 10.00000000000000178, 17.25893115100078745, 9.846743663894594434 ) ) ;
#18516 = VECTOR ( 'NONE', #78858, 1000.000000000000000 ) ;
#18517 = FACE_OUTER_BOUND ( 'NONE', #46570, .T. ) ;
#18518 = CARTESIAN_POINT ( 'NONE',  ( 18.52753015748618282, 58.92559781766745886, -4.923371831947291888 ) ) ;
#18519 = VERTEX_POINT ( 'NONE', #96213 ) ;
#18520 = SPHERICAL_SURFACE ( 'NONE', #44213, 0.2500000000000000000 ) ;
#18521 = CARTESIAN_POINT ( 'NONE',  ( 13.79529636645031943, 10.34541550158063394, -14.16423886937409904 ) ) ;
#18522 = UNCERTAINTY_MEASURE_WITH_UNIT (LENGTH_MEASURE( 1.000000000000000082E-05 ), #37169, 'distance_accuracy_value', 'NONE');
#18523 = DIRECTION ( 'NONE',  ( 0.000000000000000000, -1.000000000000000000, 0.000000000000000000 ) ) ;
#18524 =( NAMED_UNIT ( * ) PLANE_ANGLE_UNIT ( ) SI_UNIT ( $, .RADIAN. ) );
#18525 = CARTESIAN_POINT ( 'NONE',  ( -4.164238869374098151, 31.59541550158063927, -3.795296366450310543 ) ) ;
#18526 = CARTESIAN_POINT ( 'NONE',  ( 4.629999999999999893, 4.857171655774867594E-16, -4.250000000000000000 ) ) ;
#18527 = PRESENTATION_STYLE_ASSIGNMENT (( #18042 ) ) ;
#18528 = CARTESIAN_POINT ( 'NONE',  ( 20.88017736071110164, 40.35535201082150536, 2.915334737309930979 ) ) ;
#18529 = SURFACE_STYLE_FILL_AREA ( #78540 ) ;
#18530 = ORIENTED_EDGE ( 'NONE', *, *, #74263, .F. ) ;
#18531 = CARTESIAN_POINT ( 'NONE',  ( 19.84674366389459621, 13.50893115100078568, 7.409399052514197653E-17 ) ) ;
#18533 = CARTESIAN_POINT ( 'NONE',  ( 0.1532563361054083140, 11.00893115100078568, 1.131784320476157264E-15 ) ) ;
#18532 = CARTESIAN_POINT ( 'NONE',  ( -0.8801773607111008646, 58.27201867748816966, 2.915334737309923430 ) ) ;
#18534 = CARTESIAN_POINT ( 'NONE',  ( 19.38216949554541557, 42.24863466993041783, -9.382169495545420901 ) ) ;
#18535 = CARTESIAN_POINT ( 'NONE',  ( 17.20831665107776587, 32.88393115100078745, 7.208316651077764980 ) ) ;
#18536 = DIRECTION ( 'NONE',  ( -1.000000000000000000, 0.000000000000000000, -0.000000000000000000 ) ) ;
#18537 = CARTESIAN_POINT ( 'NONE',  ( 20.88017736071110164, 60.35535201082151957, 2.915334737309930979 ) ) ;
#18538 = CARTESIAN_POINT ( 'NONE',  ( 10.00000000000000178, 22.25893115100078745, 9.846743663894594434 ) ) ;
#18539 = CARTESIAN_POINT ( 'NONE',  ( 22.81628187352648496, 26.83196800326374998, -3.434112377981050290 ) ) ;
#18540 = CARTESIAN_POINT ( 'NONE',  ( 10.36894250292379027, -36.32125116508603213, 10.36894250292378672 ) ) ;
#18541 = CARTESIAN_POINT ( 'NONE',  ( 14.92337183194729988, 24.34226448433411960, -8.527530157486177487 ) ) ;
#18542 = CARTESIAN_POINT ( 'NONE',  ( 17.08211943468705130, 8.470415501580635720, 12.26659068614894998 ) ) ;
#18543 = EDGE_CURVE ( 'NONE', #6107, #37093, #91160, .T. ) ;
#18544 = ORIENTED_EDGE ( 'NONE', *, *, #98083, .F. ) ;
#18545 = CARTESIAN_POINT ( 'NONE',  ( -0.8801773607111008646, 38.27201867748816255, 2.915334737309923430 ) ) ;
#18546 = CARTESIAN_POINT ( 'NONE',  ( 0.5774900079438590739, 57.64701867748817676, -5.440088680355550821 ) ) ;
#18547 = CARTESIAN_POINT ( 'NONE',  ( 10.00000000000000178, 33.05374883491396787, 14.16423886937410082 ) ) ;
#18548 = CARTESIAN_POINT ( 'NONE',  ( 5.076628168052704559, 50.17559781766745886, -8.527530157486179263 ) ) ;
#18549 = CARTESIAN_POINT ( 'NONE',  ( 19.84674366389459266, 13.30059781766745353, 2.638427012816836559 ) ) ;
#18551 = FACE_OUTER_BOUND ( 'NONE', #86699, .T. ) ;
#18550 = DIRECTION ( 'NONE',  ( -0.5905099943842175847, -0.8070303256584298035, 0.000000000000000000 ) ) ;
#18552 = CARTESIAN_POINT ( 'NONE',  ( 19.42250999205614548, 45.98035201082150536, -5.440088680355545492 ) ) ;
#18553 = EDGE_CURVE ( 'NONE', #92036, #40169, #35226, .T. ) ;
#18554 = FACE_OUTER_BOUND ( 'NONE', #73711, .T. ) ;
#18555 = CARTESIAN_POINT ( 'NONE',  ( 22.81628187352647785, 16.62363466993042138, 6.195893100308588602E-16 ) ) ;
#18556 = CARTESIAN_POINT ( 'NONE',  ( 19.38216949554541557, 27.24863466993041783, -9.382169495545420901 ) ) ;
#18557 = CARTESIAN_POINT ( 'NONE',  ( 19.84674366389459266, 53.71726448433411605, -2.638427012816827677 ) ) ;
#18558 = CARTESIAN_POINT ( 'NONE',  ( -10.88017736071109987, 13.27201867748817321, 2.915334737309934532 ) ) ;
#18559 = CARTESIAN_POINT ( 'NONE',  ( 2.035157376598824452, 3.688685344154837953, 7.964842623401179544 ) ) ;
#18561 = CARTESIAN_POINT ( 'NONE',  ( -22.44000000000001194, 93.50000000000000000, -9.500000000000000000 ) ) ;
#18560 = CARTESIAN_POINT ( 'NONE',  ( 20.88017736071110164, 60.35535201082151957, 2.915334737309930979 ) ) ;
#18562 = CIRCLE ( 'NONE', #92001, 15.00000000000000000 ) ;
#18563 = CARTESIAN_POINT ( 'NONE',  ( -10.67064208068036102, -97.55764508346746311, 4.000000000000000000 ) ) ;
#18564 = CARTESIAN_POINT ( 'NONE',  ( 0.5600000000000083800, 105.0000000000000000, -5.000000000000000000 ) ) ;
#18565 = CARTESIAN_POINT ( 'NONE',  ( 17.96484262340118221, 61.18868534415482685, -7.964842623401177768 ) ) ;
#18566 = CARTESIAN_POINT ( 'NONE',  ( 17.96484262340118221, 54.93868534415484106, 7.964842623401181321 ) ) ;
#18567 = CARTESIAN_POINT ( 'NONE',  ( 8.879999999999991900, 69.99999999999998579, -6.250000000000000000 ) ) ;
#18568 = CARTESIAN_POINT ( 'NONE',  ( 17.20831665107776587, 24.13393115100078035, -7.208316651077762316 ) ) ;
#18569 = CARTESIAN_POINT ( 'NONE',  ( 20.88017736071110164, 20.35535201082150891, 2.915334737309930979 ) ) ;
#18570 = CIRCLE ( 'NONE', #37899, 14.49999999999999822 ) ;
#18571 = CARTESIAN_POINT ( 'NONE',  ( 0.1532563361054082862, 66.21726448433413736, 2.638427012816831674 ) ) ;
#18573 = CARTESIAN_POINT ( 'NONE',  ( 1.274849032794131976, 13.57228050351029403, 6.499999999999760192 ) ) ;
#18572 = CARTESIAN_POINT ( 'NONE',  ( 20.88017736071110519, 25.56368534415483751, 2.639326808657452039E-16 ) ) ;
#18574 = DIRECTION ( 'NONE',  ( 0.000000000000000000, 0.000000000000000000, 1.000000000000000000 ) ) ;
#18575 = CARTESIAN_POINT ( 'NONE',  ( 21.09922568453594849, 36.20696800326375353, 6.408140936763242479 ) ) ;
#18576 = ORIENTED_EDGE ( 'NONE', *, *, #49716, .F. ) ;
#18577 = CARTESIAN_POINT ( 'NONE',  ( 12.91533473730992121, 49.52201867748817676, 10.88017736071110164 ) ) ;
#18579 = CARTESIAN_POINT ( 'NONE',  ( 17.39651004071843232, 17.93575266056828355, 6.499999999999984013 ) ) ;
#18578 = CARTESIAN_POINT ( 'NONE',  ( 16.40814093676323893, 15.79030133659708746, 11.09922568453595026 ) ) ;
#18580 = CARTESIAN_POINT ( 'NONE',  ( 10.00000000000000000, 21.81368534415484106, -10.88017736071110342 ) ) ;
#18581 = CARTESIAN_POINT ( 'NONE',  ( 13.79529636645030344, 53.26208216824730357, 14.16423886937410614 ) ) ;
#18582 = CARTESIAN_POINT ( 'NONE',  ( 19.84674366389459266, 38.30059781766745175, 2.638427012816836559 ) ) ;
#18583 = CARTESIAN_POINT ( 'NONE',  ( 2.791683348922240793, 6.633931151000785675, 7.208316651077764092 ) ) ;
#18584 = CARTESIAN_POINT ( 'NONE',  ( 2.035157376598824452, 48.68868534415483396, 7.964842623401179544 ) ) ;
#18585 = DIRECTION ( 'NONE',  ( 0.000000000000000000, 0.000000000000000000, 1.000000000000000000 ) ) ;
#18586 = CARTESIAN_POINT ( 'NONE',  ( 2.917880565312950480, 20.97041550158063217, -12.26659068614894821 ) ) ;
#18587 = AXIS2_PLACEMENT_3D ( 'NONE', #78298, #17326, #857 ) ;
#18588 = EDGE_CURVE ( 'NONE', #13640, #20501, #56569, .T. ) ;
#18589 = SURFACE_STYLE_USAGE ( .BOTH. , #71600 ) ;
#18590 = DIRECTION ( 'NONE',  ( 0.000000000000000000, 1.000000000000000000, 0.000000000000000000 ) ) ;
#18591 = ORIENTED_EDGE ( 'NONE', *, *, #83822, .F. ) ;
#18592 = CARTESIAN_POINT ( 'NONE',  ( 22.26659068614894466, 43.88708216824729647, 7.082119434687054849 ) ) ;
#18593 = CARTESIAN_POINT ( 'NONE',  ( -4.164238869374099039, 56.80374883491397497, 8.674139862899312516E-16 ) ) ;
#18594 = CARTESIAN_POINT ( 'NONE',  ( 0.1532563361054083140, 11.00893115100078568, 1.131784320476157264E-15 ) ) ;
#18595 = CARTESIAN_POINT ( 'NONE',  ( 16.40814093676324603, 17.45696800326375353, -11.09922568453594671 ) ) ;
#18596 = FACE_BOUND ( 'NONE', #58065, .T. ) ;
#18597 = DIRECTION ( 'NONE',  ( 0.000000000000000000, -0.000000000000000000, 1.000000000000000000 ) ) ;
#18599 = CARTESIAN_POINT ( 'NONE',  ( -1.099225684535947600, 29.54030133659708923, 6.408140936763237150 ) ) ;
#18598 = CARTESIAN_POINT ( 'NONE',  ( 17.96484262340118221, 4.938685344154837509, 7.964842623401181321 ) ) ;
#18600 = CARTESIAN_POINT ( 'NONE',  ( 2.917880565312950480, 40.97041550158063217, -12.26659068614894821 ) ) ;
#18601 = VECTOR ( 'NONE', #93768, 1000.000000000000000 ) ;
#18602 = CARTESIAN_POINT ( 'NONE',  ( 2.618367889266248100E-15, 44.99999999999999289, -7.000000000000000000 ) ) ;
#18603 = CARTESIAN_POINT ( 'NONE',  ( -0.8801773607111009756, 68.06368534415484817, 1.068504757029289695E-15 ) ) ;
#18604 = EDGE_CURVE ( 'NONE', #51781, #49599, #91128, .T. ) ;
#18605 = CARTESIAN_POINT ( 'NONE',  ( -9.846743663894596210, 0.8005978176674529712, -2.638427012816824124 ) ) ;
#18606 = VERTEX_POINT ( 'NONE', #52670 ) ;
#18607 = PRESENTATION_STYLE_ASSIGNMENT (( #35061 ) ) ;
#18608 = CARTESIAN_POINT ( 'NONE',  ( 14.92337183194729988, 14.34226448433411782, -8.527530157486177487 ) ) ;
#18609 = B_SPLINE_CURVE_WITH_KNOTS ( 'NONE', 3,
 ( #74388, #51407, #29875, #22403 ),
 .UNSPECIFIED., .F., .F.,
 ( 4, 4 ),
 ( 2.388857365163340366E-16, 0.002392975128318463370 ),
 .UNSPECIFIED. ) ;
#18610 = EDGE_LOOP ( 'NONE', ( #28303, #20056, #41229, #20580 ) ) ;
#18612 = CARTESIAN_POINT ( 'NONE',  ( 12.91533473730992121, 14.52201867748817143, 10.88017736071110164 ) ) ;
#18611 = CARTESIAN_POINT ( 'NONE',  ( -0.8801773607111008646, 3.272018677488171434, 2.915334737309923430 ) ) ;
#18614 = CARTESIAN_POINT ( 'NONE',  ( 13.43411237798105340, 0.5819680032637533085, 12.81628187352647963 ) ) ;
#18613 = CARTESIAN_POINT ( 'NONE',  ( 1.472469842513823179, 50.59226448433411605, -4.923371831947296329 ) ) ;
#18615 = LINE ( 'NONE', #11110, #18419 ) ;
#18616 = DIRECTION ( 'NONE',  ( -1.000000000000000000, -6.938893903907221278E-15, 0.000000000000000000 ) ) ;
#18617 = VECTOR ( 'NONE', #37244, 1000.000000000000000 ) ;
#18618 = AXIS2_PLACEMENT_3D ( 'NONE', #19740, #12728, #35223 ) ;
#18619 = CARTESIAN_POINT ( 'NONE',  ( -2.816281873526473856, 24.12363466993042138, 9.499525473075851096E-16 ) ) ;
#18620 = VERTEX_POINT ( 'NONE', #38660 ) ;
#18621 = CARTESIAN_POINT ( 'NONE',  ( 24.16423886937410614, 59.30374883491397497, 8.672049930838204340E-16 ) ) ;
#18622 = ORIENTED_EDGE ( 'NONE', *, *, #55648, .F. ) ;
#18623 = CARTESIAN_POINT ( 'NONE',  ( 6.204703633549690345, 55.76208216824730357, -14.16423886937410259 ) ) ;
#18624 = VERTEX_POINT ( 'NONE', #53165 ) ;
#18625 = CARTESIAN_POINT ( 'NONE',  ( 2.035157376598822676, 32.43868534415483396, -7.964842623401177768 ) ) ;
#18626 = CARTESIAN_POINT ( 'NONE',  ( 15.44008868035555260, 39.73035201082150536, 9.422509992056143702 ) ) ;
#18627 = FILL_AREA_STYLE ('',( #35593 ) ) ;
#18628 = CARTESIAN_POINT ( 'NONE',  ( 20.88017736071110875, 30.77201867748816966, -2.915334737309920765 ) ) ;
#18629 = B_SPLINE_CURVE_WITH_KNOTS ( 'NONE', 3,
 ( #45657, #76153, #186, #20695, #81669, #36685 ),
 .UNSPECIFIED., .F., .F.,
 ( 4, 2, 4 ),
 ( 1.825722095103865762E-18, 0.0004057005074147820617, 0.0008114010148295622803 ),
 .UNSPECIFIED. ) ;
#18630 =( GEOMETRIC_REPRESENTATION_CONTEXT ( 3 ) GLOBAL_UNCERTAINTY_ASSIGNED_CONTEXT ( ( #97301 ) ) GLOBAL_UNIT_ASSIGNED_CONTEXT ( ( #32129, #41518, #18997 ) ) REPRESENTATION_CONTEXT ( 'NONE', 'WORKASPACE' ) );
#18631 = EDGE_CURVE ( 'NONE', #34917, #59039, #29657, .T. ) ;
#18633 = ORIENTED_EDGE ( 'NONE', *, *, #59927, .T. ) ;
#18632 = DIRECTION ( 'NONE',  ( 0.000000000000000000, 1.000000000000000000, 0.000000000000000000 ) ) ;
#18634 = CARTESIAN_POINT ( 'NONE',  ( 1.472469842513823179, 16.42559781766745175, 4.923371831947296329 ) ) ;
#18635 = VERTEX_POINT ( 'NONE', #60166 ) ;
#18636 = CARTESIAN_POINT ( 'NONE',  ( 11.40632860306172702, -69.21585191270308712, 3.750000000000000000 ) ) ;
#18637 = CARTESIAN_POINT ( 'NONE',  ( 10.00000000000000178, 47.25893115100078745, 9.846743663894594434 ) ) ;
#18638 = EDGE_CURVE ( 'NONE', #11556, #30617, #70749, .T. ) ;
#18639 = CARTESIAN_POINT ( 'NONE',  ( -14.37657372141814172, 2.117582368135750848E-16, -2.693041920167547065 ) ) ;
#18640 = CARTESIAN_POINT ( 'NONE',  ( -2.816281873526473856, 59.33196800326374643, 3.434112377981055619 ) ) ;
#18641 = CARTESIAN_POINT ( 'NONE',  ( -5.112373461513591621, -25.53775085953292390, 3.750000000000000444 ) ) ;
#18642 = VERTEX_POINT ( 'NONE', #14194 ) ;
#18643 = CARTESIAN_POINT ( 'NONE',  ( -46.34161155552018840, 104.0475784593821658, 5.921604558742994406 ) ) ;
#18644 = CARTESIAN_POINT ( 'NONE',  ( 8.879999999999995453, 41.24999999999999289, 6.250000000000000000 ) ) ;
#18645 = DIRECTION ( 'NONE',  ( 0.000000000000000000, 0.000000000000000000, -1.000000000000000000 ) ) ;
#18646 = CARTESIAN_POINT ( 'NONE',  ( 20.36894250292379738, 49.92874883491396787, -10.36894250292379027 ) ) ;
#18647 = DIRECTION ( 'NONE',  ( 0.000000000000000000, 1.000000000000000000, 0.000000000000000000 ) ) ;
#18648 = EDGE_LOOP ( 'NONE', ( #7795, #47485, #56642, #15584, #95017, #79024, #9383, #29334 ) ) ;
#18649 = CYLINDRICAL_SURFACE ( 'NONE', #94287, 0.2500000000000002220 ) ;
#18650 = CARTESIAN_POINT ( 'NONE',  ( 18.52753015748617571, 33.09226448433411605, 4.923371831947298993 ) ) ;
#18651 = EDGE_CURVE ( 'NONE', #94563, #89588, #36193, .T. ) ;
#18653 = VECTOR ( 'NONE', #29346, 999.9999999999998863 ) ;
#18652 = DIRECTION ( 'NONE',  ( -1.000000000000000000, 0.000000000000000000, 0.000000000000000000 ) ) ;
#18654 = CARTESIAN_POINT ( 'NONE',  ( 10.00000000000000178, 10.37363466993041961, 12.81628187352647608 ) ) ;
#18655 = CARTESIAN_POINT ( 'NONE',  ( 10.00000000000000000, 66.81368534415484817, -10.88017736071110342 ) ) ;
#18656 = CARTESIAN_POINT ( 'NONE',  ( 0.2751277870542949144, 4.366073187301309666, -6.499999999999997335 ) ) ;
#18657 = STYLED_ITEM ( 'NONE', ( #26168 ), #35550 ) ;
#18658 = CARTESIAN_POINT ( 'NONE',  ( 19.84674366389459266, 63.30059781766745886, 2.638427012816836559 ) ) ;
#18659 = CARTESIAN_POINT ( 'NONE',  ( 0.000000000000000000, 14.49999999999999822, 0.000000000000000000 ) ) ;
#18660 = CIRCLE ( 'NONE', #2777, 0.5000000000000004441 ) ;
#18661 = ORIENTED_EDGE ( 'NONE', *, *, #10407, .F. ) ;
#18662 = CARTESIAN_POINT ( 'NONE',  ( 4.559911319644449179, 2.230352010821504916, -9.422509992056141925 ) ) ;
#18663 = DIRECTION ( 'NONE',  ( -0.000000000000000000, -0.000000000000000000, -1.000000000000000000 ) ) ;
#18664 = CARTESIAN_POINT ( 'NONE',  ( 0.5774900079438607392, 38.48035201082150536, 5.440088680355550821 ) ) ;
#18666 = CARTESIAN_POINT ( 'NONE',  ( 10.00000000000000000, 66.81368534415484817, -10.88017736071110342 ) ) ;
#18665 = CARTESIAN_POINT ( 'NONE',  ( 0.6178305044545818747, 8.498634669930421381, -9.382169495545419124 ) ) ;
#18667 = CIRCLE ( 'NONE', #84127, 0.09999999999999982514 ) ;
#18668 = CARTESIAN_POINT ( 'NONE',  ( 0.5774900079438607392, 3.480352010821504027, 5.440088680355550821 ) ) ;
#18669 = EDGE_CURVE ( 'NONE', #69653, #62017, #61632, .T. ) ;
#18670 = CARTESIAN_POINT ( 'NONE',  ( 0.000000000000000000, 14.49999999999999822, 0.000000000000000000 ) ) ;
#18671 = CARTESIAN_POINT ( 'NONE',  ( 8.722765153436348839, 2.185345003916094875E-16, -11.74102699209685952 ) ) ;
#18672 = CARTESIAN_POINT ( 'NONE',  ( 7.361572987183169658, 49.96726448433410894, -9.846743663894592657 ) ) ;
#18673 = CARTESIAN_POINT ( 'NONE',  ( 17.20831665107776587, 17.88393115100078745, 7.208316651077764980 ) ) ;
#18674 = CARTESIAN_POINT ( 'NONE',  ( -2.915334737309917656, -20.89464798917849109, 10.88017736071110164 ) ) ;
#18675 = CARTESIAN_POINT ( 'NONE',  ( 3.591859063236763294, 18.29030133659708568, -11.09922568453595026 ) ) ;
#18676 = DIRECTION ( 'NONE',  ( 1.000000000000000000, 0.000000000000000000, -0.000000000000000000 ) ) ;
#18677 = CARTESIAN_POINT ( 'NONE',  ( 7.084665262690076126, 29.10535201082150181, 10.88017736071109987 ) ) ;
#18678 = PRESENTATION_LAYER_ASSIGNMENT (  '', '', ( #85695 ) ) ;
#18679 =( NAMED_UNIT ( * ) PLANE_ANGLE_UNIT ( ) SI_UNIT ( $, .RADIAN. ) );
#18680 = CARTESIAN_POINT ( 'NONE',  ( -0.3689425029237881626, 37.42874883491396787, 10.36894250292379027 ) ) ;
#18681 = CARTESIAN_POINT ( 'NONE',  ( -4.164238869374098151, 31.59541550158063927, -3.795296366450310543 ) ) ;
#18682 = CARTESIAN_POINT ( 'NONE',  ( 2.035157376598822676, 7.438685344154837509, -7.964842623401177768 ) ) ;
#18683 = CARTESIAN_POINT ( 'NONE',  ( 7.361572987183169658, 44.96726448433412315, -9.846743663894592657 ) ) ;
#18684 = TOROIDAL_SURFACE ( 'NONE', #34643, 2.500000000000000888, 0.5000000000000000000 ) ;
#18685 = CARTESIAN_POINT ( 'NONE',  ( 19.38216949554541557, 42.24863466993041783, -9.382169495545420901 ) ) ;
#18686 = CARTESIAN_POINT ( 'NONE',  ( -0.8801773607111008646, 13.27201867748817143, 2.915334737309923430 ) ) ;
#18687 = B_SPLINE_CURVE_WITH_KNOTS ( 'NONE', 3,
 ( #50852, #81345, #12841, #66332, #28344, #96868 ),
 .UNSPECIFIED., .F., .F.,
 ( 4, 2, 4 ),
 ( 0.0002800671705680389686, 0.0006862730573397217773, 0.001092478944111404749 ),
 .UNSPECIFIED. ) ;
#18688 = CARTESIAN_POINT ( 'NONE',  ( 19.84674366389459266, 33.30059781766744464, 2.638427012816836559 ) ) ;
#18689 = AXIS2_PLACEMENT_3D ( 'NONE', #34995, #89002, #82978 ) ;
#18690 = CARTESIAN_POINT ( 'NONE',  ( 0.5774900079438607392, 43.48035201082151247, 5.440088680355550821 ) ) ;
#18691 = CARTESIAN_POINT ( 'NONE',  ( -1.099225684535947600, 9.540301336597087456, 6.408140936763237150 ) ) ;
#18692 = CARTESIAN_POINT ( 'NONE',  ( -4.164238869374099927, 27.01208216824730357, 3.795296366450308767 ) ) ;
#18693 = CARTESIAN_POINT ( 'NONE',  ( -3.749999999999988010, -5.564482262735336175E-16, 4.000000000000000000 ) ) ;
#18694 = CARTESIAN_POINT ( 'NONE',  ( 19.84674366389459266, 23.71726448433412315, -2.638427012816827677 ) ) ;
#18695 = CARTESIAN_POINT ( 'NONE',  ( 22.81628187352647785, 56.62363466993042493, 6.195893100308588602E-16 ) ) ;
#18696 = CARTESIAN_POINT ( 'NONE',  ( 1.472469842513823179, 55.59226448433412315, -4.923371831947296329 ) ) ;
#18697 = ORIENTED_EDGE ( 'NONE', *, *, #64388, .F. ) ;
#18698 = DIRECTION ( 'NONE',  ( 0.000000000000000000, 0.000000000000000000, 1.000000000000000000 ) ) ;
#18699 = CARTESIAN_POINT ( 'NONE',  ( 6.829574850499570360, -88.00372650123708240, 2.749999999999999556 ) ) ;
#18700 = CARTESIAN_POINT ( 'NONE',  ( 0.5774900079438607392, 3.480352010821504916, 5.440088680355550821 ) ) ;
#18701 = CARTESIAN_POINT ( 'NONE',  ( -0.3689425029237898834, 6.178748834913968757, -10.36894250292378850 ) ) ;
#18702 = CARTESIAN_POINT ( 'NONE',  ( 14.92337183194729988, 4.342264484334117824, -8.527530157486177487 ) ) ;
#18703 = CARTESIAN_POINT ( 'NONE',  ( 17.20831665107776587, 49.13393115100078745, -7.208316651077762316 ) ) ;
#18704 = CARTESIAN_POINT ( 'NONE',  ( 12.91533473730992121, 29.52201867748817321, 10.88017736071110164 ) ) ;
#18705 = CARTESIAN_POINT ( 'NONE',  ( -10.19513985507843223, 14.49999999999999112, 11.00268709613216522 ) ) ;
#18706 = CARTESIAN_POINT ( 'NONE',  ( 19.84674366389459266, 63.71726448433412315, -2.638427012816827677 ) ) ;
#18707 =( GEOMETRIC_REPRESENTATION_CONTEXT ( 3 ) GLOBAL_UNCERTAINTY_ASSIGNED_CONTEXT ( ( #58134 ) ) GLOBAL_UNIT_ASSIGNED_CONTEXT ( ( #61346, #44859, #23372 ) ) REPRESENTATION_CONTEXT ( 'NONE', 'WORKASPACE' ) );
#18708 = EDGE_CURVE ( 'NONE', #36109, #17879, #25694, .T. ) ;
#18709 = ORIENTED_EDGE ( 'NONE', *, *, #79080, .F. ) ;
#18710 =( LENGTH_UNIT ( ) NAMED_UNIT ( * ) SI_UNIT ( .MILLI., .METRE. ) );
#18711 = VERTEX_POINT ( 'NONE', #71623 ) ;
#18712 = VERTEX_POINT ( 'NONE', #17155 ) ;
#18713 = CARTESIAN_POINT ( 'NONE',  ( 6.336100170400826848, 0.2301512019179773050, 13.53056138701891875 ) ) ;
#18714 = CARTESIAN_POINT ( 'NONE',  ( -4.164238869374099927, 12.01208216824730357, 3.795296366450308767 ) ) ;
#18715 = CARTESIAN_POINT ( 'NONE',  ( 24.16423886937409904, 14.09541550158063217, 3.795296366450317205 ) ) ;
#18716 = CARTESIAN_POINT ( 'NONE',  ( 22.26659068614895176, 44.72041550158063927, -7.082119434687042414 ) ) ;
#18717 = CARTESIAN_POINT ( 'NONE',  ( 7.361572987183170547, 52.05059781766745175, 9.846743663894590881 ) ) ;
#18718 = CARTESIAN_POINT ( 'NONE',  ( 19.84674366389459266, 33.30059781766744464, 2.638427012816836559 ) ) ;
#18719 = PLANE ( 'NONE',  #24333 ) ;
#18721 = CARTESIAN_POINT ( 'NONE',  ( 14.92337183194729633, 57.67559781766745886, 8.527530157486181039 ) ) ;
#18720 = CARTESIAN_POINT ( 'NONE',  ( 2.035157376598824452, 38.68868534415483396, 7.964842623401179544 ) ) ;
#18722 = CARTESIAN_POINT ( 'NONE',  ( -0.3689425029237898834, 6.178748834913968757, -10.36894250292378850 ) ) ;
#18723 = CARTESIAN_POINT ( 'NONE',  ( -0.3689425029237881626, 42.42874883491396787, 10.36894250292379027 ) ) ;
#18724 = MECHANICAL_DESIGN_GEOMETRIC_PRESENTATION_REPRESENTATION (  '', ( #66596 ), #23585 ) ;
#18725 = CARTESIAN_POINT ( 'NONE',  ( 17.96484262340118221, 4.938685344154837509, 7.964842623401181321 ) ) ;
#18726 = CARTESIAN_POINT ( 'NONE',  ( 0.000000000000000000, 0.000000000000000000, 0.000000000000000000 ) ) ;
#18727 = DIRECTION ( 'NONE',  ( 0.000000000000000000, 0.000000000000000000, 1.000000000000000000 ) ) ;
#18728 = CARTESIAN_POINT ( 'NONE',  ( 17.96484262340118221, 66.18868534415483396, -7.964842623401177768 ) ) ;
#18729 = CARTESIAN_POINT ( 'NONE',  ( 18.52753015748617571, 23.09226448433411960, 4.923371831947298993 ) ) ;
#18730 = CARTESIAN_POINT ( 'NONE',  ( -2.638427012816824124, -37.94940218233255536, 9.846743663894596210 ) ) ;
#18731 = VERTEX_POINT ( 'NONE', #24157 ) ;
#18732 = DIRECTION ( 'NONE',  ( -0.000000000000000000, 1.000000000000000000, 0.000000000000000000 ) ) ;
#18733 = EDGE_LOOP ( 'NONE', ( #43787, #30943, #90788, #12390, #90064, #75776 ) ) ;
#18734 = CARTESIAN_POINT ( 'NONE',  ( 0.1532563361054082862, 21.21726448433412315, 2.638427012816831674 ) ) ;
#18735 = VERTEX_POINT ( 'NONE', #2166 ) ;
#18736 = CARTESIAN_POINT ( 'NONE',  ( -4.164238869374099039, 26.80374883491397142, 8.674139862899312516E-16 ) ) ;
#18737 = CARTESIAN_POINT ( 'NONE',  ( 0.1532563361054082862, 36.21726448433410894, 2.638427012816831674 ) ) ;
#18738 = CARTESIAN_POINT ( 'NONE',  ( 19.42250999205614548, 60.98035201082151247, -5.440088680355545492 ) ) ;
#18739 = CARTESIAN_POINT ( 'NONE',  ( 4.746257547686200340, 0.000000000000000000, -2.685303318749077572 ) ) ;
#18740 = CARTESIAN_POINT ( 'NONE',  ( -0.8801773607111008646, 43.27201867748817676, 2.915334737309923430 ) ) ;
#18741 = CARTESIAN_POINT ( 'NONE',  ( 0.1532563361054082862, 51.21726448433412315, 2.638427012816831674 ) ) ;
#18742 = AXIS2_PLACEMENT_3D ( 'NONE', #18526, #39568, #31547 ) ;
#18743 = CARTESIAN_POINT ( 'NONE',  ( -3.434112377981047626, -4.834698663402913432, 12.81628187352647963 ) ) ;
#18744 = EDGE_LOOP ( 'NONE', ( #84254, #70225, #13266, #95093 ) ) ;
#18745 = CARTESIAN_POINT ( 'NONE',  ( -2.266590686148945544, 22.22041550158063572, 7.082119434687048631 ) ) ;
#18746 = ORIENTED_EDGE ( 'NONE', *, *, #15413, .F. ) ;
#18747 = VERTEX_POINT ( 'NONE', #25156 ) ;
#18748 = CARTESIAN_POINT ( 'NONE',  ( 0.6178305044545838731, 34.74863466993042493, 9.382169495545420901 ) ) ;
#18749 = AXIS2_PLACEMENT_3D ( 'NONE', #47738, #9748, #55237 ) ;
#18750 = CARTESIAN_POINT ( 'NONE',  ( 18.52753015748617571, 23.09226448433411960, 4.923371831947298993 ) ) ;
#18751 = FACE_OUTER_BOUND ( 'NONE', #17057, .T. ) ;
#18752 = CARTESIAN_POINT ( 'NONE',  ( -2.816281873526471635, 48.91530133659708213, -3.434112377981056508 ) ) ;
#18753 = LINE ( 'NONE', #65706, #28814 ) ;
#18754 = CARTESIAN_POINT ( 'NONE',  ( 17.20831665107776587, 24.13393115100078035, -7.208316651077762316 ) ) ;
#18755 = VECTOR ( 'NONE', #47662, 1000.000000000000000 ) ;
#18756 = PRESENTATION_LAYER_ASSIGNMENT (  '', '', ( #65045 ) ) ;
#18757 = CARTESIAN_POINT ( 'NONE',  ( -0.8801773607110991993, 62.85535201082150536, -2.915334737309923874 ) ) ;
#18758 = EDGE_CURVE ( 'NONE', #85730, #48374, #51229, .T. ) ;
#18759 = FACE_OUTER_BOUND ( 'NONE', #48523, .T. ) ;
#18760 = DIRECTION ( 'NONE',  ( 0.000000000000000000, 0.000000000000000000, 1.000000000000000000 ) ) ;
#18761 = LINE ( 'NONE', #18265, #97892 ) ;
#18762 = EDGE_CURVE ( 'NONE', #61441, #13300, #3620, .T. ) ;
#18763 = LINE ( 'NONE', #57229, #66843 ) ;
#18764 = CARTESIAN_POINT ( 'NONE',  ( 10.00000000000000178, 69.31368534415484817, 10.88017736071110342 ) ) ;
#18765 = EDGE_CURVE ( 'NONE', #57516, #14429, #40635, .T. ) ;
#18766 = CARTESIAN_POINT ( 'NONE',  ( 22.81628187352647785, 16.62363466993042138, 6.195893100308588602E-16 ) ) ;
#18767 = DIRECTION ( 'NONE',  ( -1.000000000000000000, 0.000000000000000000, 0.000000000000000000 ) ) ;
#18768 = CARTESIAN_POINT ( 'NONE',  ( 18.52753015748617571, 43.09226448433412315, 4.923371831947298993 ) ) ;
#18769 = CARTESIAN_POINT ( 'NONE',  ( 10.00000000000000178, 65.37363466993042493, 12.81628187352647608 ) ) ;
#18770 = CARTESIAN_POINT ( 'NONE',  ( 2.917880565312948704, 2.637082168247300906, 12.26659068614894643 ) ) ;
#18771 = CARTESIAN_POINT ( 'NONE',  ( 1.472469842513823179, 36.42559781766745175, 4.923371831947296329 ) ) ;
#18772 = CARTESIAN_POINT ( 'NONE',  ( -1.099225684535947600, 29.54030133659708923, 6.408140936763237150 ) ) ;
#18774 = CARTESIAN_POINT ( 'NONE',  ( 7.684764310694791156, 0.5000000000000004441, 12.88194075009940498 ) ) ;
#18773 = FACE_OUTER_BOUND ( 'NONE', #31813, .T. ) ;
#18775 = CARTESIAN_POINT ( 'NONE',  ( 4.559911319644449179, 58.89701867748817676, 9.422509992056141925 ) ) ;
#18776 = CARTESIAN_POINT ( 'NONE',  ( 22.81628187352648496, 6.831968003263753531, -3.434112377981050290 ) ) ;
#18777 = CARTESIAN_POINT ( 'NONE',  ( 1.959929470562282283, 41.50257860105349295, 5.767676674365853629 ) ) ;
#18778 = CARTESIAN_POINT ( 'NONE',  ( 10.00000000000000000, 29.75893115100078745, -9.846743663894594434 ) ) ;
#18779 = CARTESIAN_POINT ( 'NONE',  ( 15.44008868035555260, 29.73035201082150891, 9.422509992056143702 ) ) ;
#18780 = CARTESIAN_POINT ( 'NONE',  ( 0.6178305044545838731, 24.74863466993042493, 9.382169495545420901 ) ) ;
#18781 = CARTESIAN_POINT ( 'NONE',  ( 0.1532563361054100626, 25.80059781766744820, -2.638427012816831230 ) ) ;
#18782 = CARTESIAN_POINT ( 'NONE',  ( -11.82883858055346415, 90.33605471726345115, 7.015824399821311452 ) ) ;
#18783 = CARTESIAN_POINT ( 'NONE',  ( 19.42250999205614193, 30.14701867748817321, 5.440088680355555262 ) ) ;
#18784 = ORIENTED_EDGE ( 'NONE', *, *, #70799, .F. ) ;
#18785 = CARTESIAN_POINT ( 'NONE',  ( 2.035157376598824452, 63.68868534415484106, 7.964842623401179544 ) ) ;
#18786 = CARTESIAN_POINT ( 'NONE',  ( 19.42250999205614193, 5.147018677488171434, 5.440088680355555262 ) ) ;
#18788 = CARTESIAN_POINT ( 'NONE',  ( 2.035157376598822676, 32.43868534415483396, -7.964842623401177768 ) ) ;
#18787 = CARTESIAN_POINT ( 'NONE',  ( 1.472469842513823179, 40.59226448433411605, -4.923371831947296329 ) ) ;
#18789 = EDGE_CURVE ( 'NONE', #7347, #21745, #14800, .T. ) ;
#18790 = CARTESIAN_POINT ( 'NONE',  ( 4.559911319644449179, 47.23035201082150536, -9.422509992056141925 ) ) ;
#18791 = CARTESIAN_POINT ( 'NONE',  ( 4.559911319644449179, 17.23035201082150536, -9.422509992056141925 ) ) ;
#18792 = CYLINDRICAL_SURFACE ( 'NONE', #30739, 15.00000000000000000 ) ;
#18793 = CARTESIAN_POINT ( 'NONE',  ( 18.52753015748617571, 33.09226448433411605, 4.923371831947298993 ) ) ;
#18794 = CARTESIAN_POINT ( 'NONE',  ( -2.266590686148945544, 51.38708216824730357, -7.082119434687050408 ) ) ;
#18795 = CARTESIAN_POINT ( 'NONE',  ( 0.000000000000000000, 14.49999999999999822, 0.000000000000000000 ) ) ;
#18796 = EDGE_CURVE ( 'NONE', #12912, #70565, #72096, .T. ) ;
#18797 = CARTESIAN_POINT ( 'NONE',  ( 13.79529636645030344, 38.26208216824729647, 14.16423886937410614 ) ) ;
#18798 = CIRCLE ( 'NONE', #2905, 3.999999999999999112 ) ;
#18799 = CARTESIAN_POINT ( 'NONE',  ( 11.42891328973218279, 15.00000000000000533, 9.126250717928463985 ) ) ;
#18800 = ORIENTED_EDGE ( 'NONE', *, *, #88065, .F. ) ;
#18801 = CARTESIAN_POINT ( 'NONE',  ( 0.5774900079438607392, 3.480352010821504916, 5.440088680355550821 ) ) ;
#18802 = CARTESIAN_POINT ( 'NONE',  ( 5.076628168052704559, 35.17559781766745175, -8.527530157486179263 ) ) ;
#18804 = CARTESIAN_POINT ( 'NONE',  ( -45.94000000000001194, 99.99999999999998579, 5.000000000000000000 ) ) ;
#18803 = CARTESIAN_POINT ( 'NONE',  ( -3.927832320392065313, 0.000000000000000000, -13.69797916712109398 ) ) ;
#18805 = CARTESIAN_POINT ( 'NONE',  ( -0.8801773607110991993, 57.85535201082149825, -2.915334737309923874 ) ) ;
#18806 = CARTESIAN_POINT ( 'NONE',  ( -2.816281873526473856, 59.12363466993042493, 9.499525473075851096E-16 ) ) ;
#18807 = CARTESIAN_POINT ( 'NONE',  ( 10.00000000000000000, 26.81368534415484106, -10.88017736071110342 ) ) ;
#18808 = CARTESIAN_POINT ( 'NONE',  ( 22.81628187352648496, 61.83196800326376774, -3.434112377981050290 ) ) ;
#18809 = CARTESIAN_POINT ( 'NONE',  ( 10.00000000000000178, 10.37363466993041961, 12.81628187352647608 ) ) ;
#18810 = CARTESIAN_POINT ( 'NONE',  ( 5.076628168052703671, 11.84226448433411960, 8.527530157486179263 ) ) ;
#18811 = ORIENTED_EDGE ( 'NONE', *, *, #94726, .F. ) ;
#18812 = FACE_OUTER_BOUND ( 'NONE', #63093, .T. ) ;
#18813 = CARTESIAN_POINT ( 'NONE',  ( -0.3093388210927633941, 15.00000000000000000, -14.99680997725065978 ) ) ;
#18814 = CARTESIAN_POINT ( 'NONE',  ( 13.79529636645030344, 63.26208216824730357, 14.16423886937410614 ) ) ;
#18815 = CARTESIAN_POINT ( 'NONE',  ( 10.00000000000000000, 30.55374883491397142, -14.16423886937410082 ) ) ;
#18816 = CARTESIAN_POINT ( 'NONE',  ( 2.035157376598824452, 28.68868534415484106, 7.964842623401179544 ) ) ;
#18817 = AXIS2_PLACEMENT_3D ( 'NONE', #71124, #63109, #24641 ) ;
#18818 = CARTESIAN_POINT ( 'NONE',  ( 2.035157376598824452, 43.68868534415484106, 7.964842623401179544 ) ) ;
#18819 = FACE_OUTER_BOUND ( 'NONE', #56257, .T. ) ;
#18820 = FILL_AREA_STYLE_COLOUR ( '', #24115 ) ;
#18821 = CARTESIAN_POINT ( 'NONE',  ( 12.63842701281683034, 12.46726448433411782, 9.846743663894596210 ) ) ;
#18822 =( NAMED_UNIT ( * ) PLANE_ANGLE_UNIT ( ) SI_UNIT ( $, .RADIAN. ) );
#18823 = CARTESIAN_POINT ( 'NONE',  ( 12.63842701281683034, 27.46726448433411250, 9.846743663894596210 ) ) ;
#18824 = CARTESIAN_POINT ( 'NONE',  ( -14.88232117145532918, 14.63595249122789177, 1.875237731503045735 ) ) ;
#18825 = CARTESIAN_POINT ( 'NONE',  ( 1.472469842513823179, 26.42559781766745175, 4.923371831947296329 ) ) ;
#18826 = CARTESIAN_POINT ( 'NONE',  ( 14.92337183194729988, 54.34226448433412315, -8.527530157486177487 ) ) ;
#18827 = CARTESIAN_POINT ( 'NONE',  ( -0.8801773607110991993, 22.85535201082150181, -2.915334737309923874 ) ) ;
#18828 = PRESENTATION_LAYER_ASSIGNMENT (  '', '', ( #25273 ) ) ;
#18829 = CIRCLE ( 'NONE', #69931, 14.49999999999999822 ) ;
#18830 = CARTESIAN_POINT ( 'NONE',  ( 6.565887622018943937, 50.16530133659708213, 12.81628187352647430 ) ) ;
#18831 = CARTESIAN_POINT ( 'NONE',  ( 19.84674366389459266, 33.71726448433410894, -2.638427012816827677 ) ) ;
#18833 = CARTESIAN_POINT ( 'NONE',  ( 19.84674366389459266, 18.71726448433411960, -2.638427012816827677 ) ) ;
#18832 = CARTESIAN_POINT ( 'NONE',  ( 17.08211943468705840, 60.13708216824729647, -12.26659068614894466 ) ) ;
#18834 = DIRECTION ( 'NONE',  ( 0.000000000000000000, 0.000000000000000000, 1.000000000000000000 ) ) ;
#18835 = CARTESIAN_POINT ( 'NONE',  ( 18.52753015748617571, 63.09226448433412315, 4.923371831947298993 ) ) ;
#18836 = CARTESIAN_POINT ( 'NONE',  ( -4.164238869374098151, 11.59541550158063217, -3.795296366450310543 ) ) ;
#18837 = CARTESIAN_POINT ( 'NONE',  ( 2.917880565312948704, 32.63708216824730357, 12.26659068614894643 ) ) ;
#18838 = CARTESIAN_POINT ( 'NONE',  ( 18.52753015748617571, 33.09226448433411605, 4.923371831947298993 ) ) ;
#18839 = CARTESIAN_POINT ( 'NONE',  ( 4.221203097589939723, -3.619724449958656276, -2.500000000000000000 ) ) ;
#18840 = CARTESIAN_POINT ( 'NONE',  ( 15.44008868035555260, 24.73035201082150891, 9.422509992056143702 ) ) ;
#18841 = CARTESIAN_POINT ( 'NONE',  ( 10.00000000000000178, 54.31368534415484106, 10.88017736071110342 ) ) ;
#18842 = CARTESIAN_POINT ( 'NONE',  ( -0.8801773607111008646, 43.27201867748817676, 2.915334737309923430 ) ) ;
#18843 = ORIENTED_EDGE ( 'NONE', *, *, #58466, .F. ) ;
#18844 = CARTESIAN_POINT ( 'NONE',  ( 3.591859063236761518, 49.95696800326375353, 11.09922568453594849 ) ) ;
#18845 = CARTESIAN_POINT ( 'NONE',  ( 12.91533473730993009, 51.60535201082149825, -10.88017736071109987 ) ) ;
#18846 = ORIENTED_EDGE ( 'NONE', *, *, #1621, .F. ) ;
#18847 = EDGE_CURVE ( 'NONE', #28374, #69849, #81341, .T. ) ;
#18848 = SURFACE_SIDE_STYLE ('',( #17861 ) ) ;
#18849 = CARTESIAN_POINT ( 'NONE',  ( 2.035157376598824452, 58.68868534415482685, 7.964842623401179544 ) ) ;
#18850 = ORIENTED_EDGE ( 'NONE', *, *, #16102, .T. ) ;
#18851 = CARTESIAN_POINT ( 'NONE',  ( -0.8801773607111009756, 58.06368534415484106, 1.068504757029289695E-15 ) ) ;
#18852 = CARTESIAN_POINT ( 'NONE',  ( 12.91533473730993009, 6.605352010821504471, -10.88017736071109987 ) ) ;
#18853 = B_SPLINE_CURVE_WITH_KNOTS ( 'NONE', 3,
 ( #19465, #10979, #95466, #2529 ),
 .UNSPECIFIED., .F., .F.,
 ( 4, 4 ),
 ( 3.469446951953614189E-18, 0.002562518741975564063 ),
 .UNSPECIFIED. ) ;
#18854 = CARTESIAN_POINT ( 'NONE',  ( -5.240693273019180864, 14.95037116783537456, 13.79102773477909949 ) ) ;
#18855 = DIRECTION ( 'NONE',  ( 0.000000000000000000, 1.000000000000000000, 0.000000000000000000 ) ) ;
#18856 = CARTESIAN_POINT ( 'NONE',  ( -0.8801773607111009756, 8.063685344154837509, 1.068504757029289695E-15 ) ) ;
#18857 = CARTESIAN_POINT ( 'NONE',  ( 14.92337183194729633, 12.67559781766745353, 8.527530157486181039 ) ) ;
#18858 = CARTESIAN_POINT ( 'NONE',  ( 20.36894250292379738, 4.928748834913967869, -10.36894250292379027 ) ) ;
#18859 = CARTESIAN_POINT ( 'NONE',  ( 19.84674366389459266, 8.717264484334116048, -2.638427012816827677 ) ) ;
#18860 = CARTESIAN_POINT ( 'NONE',  ( 0.5774900079438590739, 7.647018677488171434, -5.440088680355550821 ) ) ;
#18861 = CARTESIAN_POINT ( 'NONE',  ( 7.361572987183170547, 52.05059781766745175, 9.846743663894590881 ) ) ;
#18862 = VERTEX_POINT ( 'NONE', #64091 ) ;
#18863 = CARTESIAN_POINT ( 'NONE',  ( 5.076628168052703671, 41.84226448433411605, 8.527530157486179263 ) ) ;
#18864 = ORIENTED_EDGE ( 'NONE', *, *, #65570, .F. ) ;
#18865 = CARTESIAN_POINT ( 'NONE',  ( 17.96484262340118221, 49.93868534415484106, 7.964842623401181321 ) ) ;
#18866 = CARTESIAN_POINT ( 'NONE',  ( 18.52753015748617571, 58.09226448433411605, 4.923371831947298993 ) ) ;
#18867 = EDGE_CURVE ( 'NONE', #49892, #61653, #63841, .T. ) ;
#18869 = CARTESIAN_POINT ( 'NONE',  ( -6.699646882363181177, 1.931786074955269106, -9.748952036344858740 ) ) ;
#18868 = CARTESIAN_POINT ( 'NONE',  ( -0.8801773607111008646, 8.272018677488171434, 2.915334737309923430 ) ) ;
#18870 = CARTESIAN_POINT ( 'NONE',  ( -0.8801773607111008646, 63.27201867748817676, 2.915334737309923430 ) ) ;
#18871 = CARTESIAN_POINT ( 'NONE',  ( 19.42250999205614193, 5.147018677488171434, 5.440088680355555262 ) ) ;
#18872 = ADVANCED_FACE ( 'NONE', ( #70638 ), #32621, .T. ) ;
#18873 = CARTESIAN_POINT ( 'NONE',  ( -2.816281873526473856, 44.12363466993042493, 9.499525473075851096E-16 ) ) ;
#18874 = CARTESIAN_POINT ( 'NONE',  ( 20.88017736071110164, 30.35535201082151247, 2.915334737309930979 ) ) ;
#18875 = CARTESIAN_POINT ( 'NONE',  ( -0.03447792253739070251, 10.15514106990689669, 6.401564815979740253 ) ) ;
#18876 = EDGE_LOOP ( 'NONE', ( #10127, #44241, #6183, #27664 ) ) ;
#18877 = CARTESIAN_POINT ( 'NONE',  ( -1.099225684535947600, 39.54030133659708923, 6.408140936763237150 ) ) ;
#18878 = CARTESIAN_POINT ( 'NONE',  ( 2.035157376598824452, 33.68868534415484106, 7.964842623401179544 ) ) ;
#18879 = EDGE_CURVE ( 'NONE', #47627, #59056, #63119, .T. ) ;
#18880 = VERTEX_POINT ( 'NONE', #55633 ) ;
#18881 = VECTOR ( 'NONE', #94633, 1000.000000000000000 ) ;
#18882 = CARTESIAN_POINT ( 'NONE',  ( 5.076628168052704559, 65.17559781766745175, -8.527530157486179263 ) ) ;
#18884 = CARTESIAN_POINT ( 'NONE',  ( 7.361572987183170547, 47.05059781766745175, 9.846743663894590881 ) ) ;
#18883 = CARTESIAN_POINT ( 'NONE',  ( 2.791683348922240793, 11.63393115100078568, 7.208316651077764092 ) ) ;
#18885 = CARTESIAN_POINT ( 'NONE',  ( 4.559911319644449179, 22.23035201082150536, -9.422509992056141925 ) ) ;
#18886 = DIRECTION ( 'NONE',  ( 0.000000000000000000, 0.000000000000000000, -1.000000000000000000 ) ) ;
#18887 = CARTESIAN_POINT ( 'NONE',  ( 10.00000000000000000, 34.75893115100078745, -9.846743663894594434 ) ) ;
#18888 = CARTESIAN_POINT ( 'NONE',  ( 13.82192141328812518, 4.718101003023380916E-16, -4.382292601468683380 ) ) ;
#18889 = DIRECTION ( 'NONE',  ( 0.9975640502598257520, -0.06975647374410356982, 0.000000000000000000 ) ) ;
#18892 = CARTESIAN_POINT ( 'NONE',  ( 0.8649609010932225450, -2.354751593366952970E-16, 14.60103384664012260 ) ) ;
#18891 = AXIS2_PLACEMENT_3D ( 'NONE', #10573, #17103, #94555 ) ;
#18890 = CARTESIAN_POINT ( 'NONE',  ( 1.472469842513823179, 30.59226448433411960, -4.923371831947296329 ) ) ;
#18893 = DIRECTION ( 'NONE',  ( -0.000000000000000000, 0.000000000000000000, 1.000000000000000000 ) ) ;
#18895 = ORIENTED_EDGE ( 'NONE', *, *, #13609, .F. ) ;
#18894 = CARTESIAN_POINT ( 'NONE',  ( 19.84674366389459266, 58.71726448433411605, -2.638427012816827677 ) ) ;
#18896 = AXIS2_PLACEMENT_3D ( 'NONE', #34943, #78980, #94470 ) ;
#18897 = CARTESIAN_POINT ( 'NONE',  ( -2.816281873526471635, 63.91530133659708923, -3.434112377981056508 ) ) ;
#18898 = B_SPLINE_CURVE_WITH_KNOTS ( 'NONE', 3,
 ( #69775, #1306, #78935, #16477, #62440, #71450 ),
 .UNSPECIFIED., .F., .F.,
 ( 4, 2, 4 ),
 ( 0.000000000000000000, 0.0002605067024380874896, 0.0005210134048761749792 ),
 .UNSPECIFIED. ) ;
#18899 = CARTESIAN_POINT ( 'NONE',  ( 1.274849032794306947, 7.555090184799359676, -6.499999999999997335 ) ) ;
#18900 = CARTESIAN_POINT ( 'NONE',  ( -2.816281873526473856, 24.12363466993042138, 9.499525473075851096E-16 ) ) ;
#18901 = CARTESIAN_POINT ( 'NONE',  ( 0.1532563361054082862, 46.21726448433411605, 2.638427012816831674 ) ) ;
#18902 = CARTESIAN_POINT ( 'NONE',  ( 8.235571585149870089, 6.993033628982647798, 8.235571585149868312 ) ) ;
#18903 = CARTESIAN_POINT ( 'NONE',  ( 17.08211943468705840, 65.13708216824730357, -12.26659068614894466 ) ) ;
#18904 = CARTESIAN_POINT ( 'NONE',  ( 10.00000000000000178, 17.25893115100078745, 9.846743663894594434 ) ) ;
#18905 = DIRECTION ( 'NONE',  ( 0.000000000000000000, 1.000000000000000000, 0.000000000000000000 ) ) ;
#18906 = CARTESIAN_POINT ( 'NONE',  ( -4.164238869374098151, 51.59541550158063217, -3.795296366450310543 ) ) ;
#18907 = CARTESIAN_POINT ( 'NONE',  ( 19.84674366389459266, 58.71726448433411605, -2.638427012816827677 ) ) ;
#18908 = EDGE_CURVE ( 'NONE', #60520, #82054, #97352, .T. ) ;
#18909 = CARTESIAN_POINT ( 'NONE',  ( 15.44008868035555260, 4.730352010821505360, 9.422509992056143702 ) ) ;
#18910 = CARTESIAN_POINT ( 'NONE',  ( -2.266590686148945544, 36.38708216824730357, -7.082119434687050408 ) ) ;
#18911 = CARTESIAN_POINT ( 'NONE',  ( 24.16423886937410614, 34.30374883491396787, 8.672049930838204340E-16 ) ) ;
#18912 = CARTESIAN_POINT ( 'NONE',  ( 12.60589901313225702, 14.63606915354311155, -8.129656208642060733 ) ) ;
#18914 = CARTESIAN_POINT ( 'NONE',  ( 2.791683348922237240, 60.38393115100078745, -7.208316651077763204 ) ) ;
#18913 = DIRECTION ( 'NONE',  ( -0.000000000000000000, -1.000000000000000000, -0.000000000000000000 ) ) ;
#18915 = ORIENTED_EDGE ( 'NONE', *, *, #64585, .F. ) ;
#18916 = CARTESIAN_POINT ( 'NONE',  ( 10.00000000000000178, 54.31368534415484106, 10.88017736071110342 ) ) ;
#18917 = CARTESIAN_POINT ( 'NONE',  ( 19.64275089555621179, 93.00209110515163502, -5.306638067702549755 ) ) ;
#18918 = CARTESIAN_POINT ( 'NONE',  ( 7.361572987183170547, 52.05059781766745175, 9.846743663894590881 ) ) ;
#18919 = DIRECTION ( 'NONE',  ( 0.3173046564051030805, 0.000000000000000000, -0.9483236552061955482 ) ) ;
#18920 = EDGE_CURVE ( 'NONE', #78138, #42602, #55319, .T. ) ;
#18921 = CARTESIAN_POINT ( 'NONE',  ( 14.92337183194729633, 57.67559781766745886, 8.527530157486181039 ) ) ;
#18922 = DIRECTION ( 'NONE',  ( -0.000000000000000000, 0.000000000000000000, 1.000000000000000000 ) ) ;
#18923 = ORIENTED_EDGE ( 'NONE', *, *, #62271, .T. ) ;
#18924 = CARTESIAN_POINT ( 'NONE',  ( 13.79529636645030344, 28.26208216824729647, 14.16423886937410614 ) ) ;
#18925 = CARTESIAN_POINT ( 'NONE',  ( 2.791683348922237240, 0.3839311510007847872, -7.208316651077763204 ) ) ;
#18926 = CARTESIAN_POINT ( 'NONE',  ( -4.535014064372608011, -17.52590857052054929, -2.750000000000000000 ) ) ;
#18927 = CARTESIAN_POINT ( 'NONE',  ( -0.8801773607111008646, 13.27201867748817321, 2.915334737309923430 ) ) ;
#18928 = CARTESIAN_POINT ( 'NONE',  ( 10.00000000000000000, 27.87363466993042138, -12.81628187352647608 ) ) ;
#18929 = CARTESIAN_POINT ( 'NONE',  ( -13.82192141328803991, 15.00000000000000000, -4.382292601468865456 ) ) ;
#18930 = CARTESIAN_POINT ( 'NONE',  ( 19.84674366389459266, 13.71726448433411782, -2.638427012816827677 ) ) ;
#18931 = CARTESIAN_POINT ( 'NONE',  ( -8.000000000000000000, 40.99999999999999289, 6.250000000000000000 ) ) ;
#18932 = CARTESIAN_POINT ( 'NONE',  ( 10.00000000000000178, 33.05374883491396787, 14.16423886937410082 ) ) ;
#18933 = DIRECTION ( 'NONE',  ( 1.000000000000000000, -0.000000000000000000, 0.000000000000000000 ) ) ;
#18934 = CARTESIAN_POINT ( 'NONE',  ( 19.88701968852526747, 61.79427333184084148, 6.480634945678621861 ) ) ;
#18935 = CARTESIAN_POINT ( 'NONE',  ( -0.8801773607110991993, 7.855352010821506248, -2.915334737309923874 ) ) ;
#18936 = AXIS2_PLACEMENT_3D ( 'NONE', #85335, #31828, #62324 ) ;
#18937 = DIRECTION ( 'NONE',  ( -0.9799247046208311440, 0.000000000000000000, 0.1993679344171901680 ) ) ;
#18938 = CARTESIAN_POINT ( 'NONE',  ( 20.88017736071110519, 40.56368534415484106, 2.639326808657452039E-16 ) ) ;
#18939 = CARTESIAN_POINT ( 'NONE',  ( 2.035157376598822676, 32.43868534415483396, -7.964842623401177768 ) ) ;
#18940 = CARTESIAN_POINT ( 'NONE',  ( 19.38216949554541202, 0.9986346699304200492, 9.382169495545424454 ) ) ;
#18941 = SURFACE_STYLE_USAGE ( .BOTH. , #57900 ) ;
#18942 = LINE ( 'NONE', #96926, #17962 ) ;
#18943 = CARTESIAN_POINT ( 'NONE',  ( 10.00000000000000178, 12.25893115100078568, 9.846743663894594434 ) ) ;
#18944 = EDGE_LOOP ( 'NONE', ( #39276, #54888, #58813, #95527 ) ) ;
#18945 = CARTESIAN_POINT ( 'NONE',  ( 18.50749283717773963, 49.69955587570481015, 6.500000000000079936 ) ) ;
#18946 = CARTESIAN_POINT ( 'NONE',  ( 4.559911319644449179, 48.89701867748817676, 9.422509992056141925 ) ) ;
#18947 = CARTESIAN_POINT ( 'NONE',  ( 10.00000000000000178, 0.3736346699304200492, 12.81628187352647608 ) ) ;
#18948 = CARTESIAN_POINT ( 'NONE',  ( 17.96484262340118221, 59.93868534415484106, 7.964842623401181321 ) ) ;
#18949 = CARTESIAN_POINT ( 'NONE',  ( 2.791683348922237240, 30.38393115100078390, -7.208316651077763204 ) ) ;
#18950 = CARTESIAN_POINT ( 'NONE',  ( 10.00000000000000178, 35.37363466993042493, 12.81628187352647608 ) ) ;
#18952 = CARTESIAN_POINT ( 'NONE',  ( -4.841283923550532720, 14.76930270348881002, 14.13506365971143808 ) ) ;
#18951 = CARTESIAN_POINT ( 'NONE',  ( 0.1532563361054100626, 5.800597817667452638, -2.638427012816831230 ) ) ;
#18953 = ORIENTED_EDGE ( 'NONE', *, *, #35093, .T. ) ;
#18954 = DIRECTION ( 'NONE',  ( -0.7132504491541848957, 0.000000000000000000, 0.7009092642998474565 ) ) ;
#18955 = DIRECTION ( 'NONE',  ( -0.7604059656000340395, 0.000000000000000000, 0.6494480483301798834 ) ) ;
#18956 = CARTESIAN_POINT ( 'NONE',  ( 12.91533473730992121, 4.522018677488169658, 10.88017736071110164 ) ) ;
#18957 = CARTESIAN_POINT ( 'NONE',  ( 10.00000000000000000, 57.87363466993042493, -12.81628187352647608 ) ) ;
#18958 = CARTESIAN_POINT ( 'NONE',  ( 1.472469842513823179, 31.42559781766745530, 4.923371831947296329 ) ) ;
#18959 = CARTESIAN_POINT ( 'NONE',  ( 4.559911319644449179, 13.89701867748817143, 9.422509992056141925 ) ) ;
#18960 = CARTESIAN_POINT ( 'NONE',  ( -0.8801773607111009756, 3.063685344154838397, 1.068504757029289695E-15 ) ) ;
#18961 = VERTEX_POINT ( 'NONE', #79608 ) ;
#18962 = CARTESIAN_POINT ( 'NONE',  ( -0.8801773607111008646, 18.27201867748817321, 2.915334737309923430 ) ) ;
#18963 = ADVANCED_FACE ( 'NONE', ( #47635 ), #9141, .T. ) ;
#18964 = AXIS2_PLACEMENT_3D ( 'NONE', #54616, #71616, #39647 ) ;
#18965 = CARTESIAN_POINT ( 'NONE',  ( 15.44008868035555793, 16.39701867748817321, -9.422509992056140149 ) ) ;
#18966 = DIRECTION ( 'NONE',  ( 0.000000000000000000, 0.000000000000000000, -1.000000000000000000 ) ) ;
#18967 = VERTEX_POINT ( 'NONE', #70150 ) ;
#18968 = CARTESIAN_POINT ( 'NONE',  ( 5.076628168052703671, 66.84226448433412315, 8.527530157486179263 ) ) ;
#18969 = CARTESIAN_POINT ( 'NONE',  ( 7.084665262690076126, 24.10535201082150181, 10.88017736071109987 ) ) ;
#18970 = CARTESIAN_POINT ( 'NONE',  ( 14.92337183194729988, 54.34226448433412315, -8.527530157486177487 ) ) ;
#18971 = FACE_OUTER_BOUND ( 'NONE', #35689, .T. ) ;
#18972 = CARTESIAN_POINT ( 'NONE',  ( 0.6178305044545818747, 53.49863466993041072, -9.382169495545419124 ) ) ;
#18973 = CARTESIAN_POINT ( 'NONE',  ( 12.26500600480480863, -7.132017415881208855E-16, 0.000000000000000000 ) ) ;
#18974 = CARTESIAN_POINT ( 'NONE',  ( -4.164238869374098151, 31.59541550158063927, -3.795296366450310543 ) ) ;
#18975 = CARTESIAN_POINT ( 'NONE',  ( 15.44008868035555260, 44.73035201082151247, 9.422509992056143702 ) ) ;
#18976 = CARTESIAN_POINT ( 'NONE',  ( 4.559911319644449179, 13.89701867748817321, 9.422509992056141925 ) ) ;
#18977 = CARTESIAN_POINT ( 'NONE',  ( 1.472469842513823179, 55.59226448433412315, -4.923371831947296329 ) ) ;
#18978 = CARTESIAN_POINT ( 'NONE',  ( -11.42220087045558330, -90.34422636326586087, -3.749999999999999556 ) ) ;
#18979 = CARTESIAN_POINT ( 'NONE',  ( 7.361572987183170547, 47.05059781766745175, 9.846743663894590881 ) ) ;
#18980 = CARTESIAN_POINT ( 'NONE',  ( 15.00000000000000000, 11.50000000000000000, -6.500000000000000888 ) ) ;
#18981 = CARTESIAN_POINT ( 'NONE',  ( 17.20831665107776587, 9.133931151000787452, -7.208316651077762316 ) ) ;
#18982 = CARTESIAN_POINT ( 'NONE',  ( -12.81628187352647608, -30.87636533006957507, 3.903127820947815962E-15 ) ) ;
#18983 = VERTEX_POINT ( 'NONE', #43563 ) ;
#18984 = CARTESIAN_POINT ( 'NONE',  ( 2.035157376598822676, 17.43868534415483751, -7.964842623401177768 ) ) ;
#18985 = CARTESIAN_POINT ( 'NONE',  ( 17.20831665107776587, 7.883931151000784787, 7.208316651077764980 ) ) ;
#18986 = CARTESIAN_POINT ( 'NONE',  ( -2.816281873526473856, -0.8763653300695799508, 9.499525473075851096E-16 ) ) ;
#18988 = CARTESIAN_POINT ( 'NONE',  ( 10.00000000000000178, 49.31368534415484106, 10.88017736071110342 ) ) ;
#18987 = CARTESIAN_POINT ( 'NONE',  ( 10.00000000000000000, 51.81368534415484106, -10.88017736071110342 ) ) ;
#18990 = CARTESIAN_POINT ( 'NONE',  ( 0.6178305044545818747, 38.49863466993042493, -9.382169495545419124 ) ) ;
#18989 = CARTESIAN_POINT ( 'NONE',  ( 20.88017736071110519, 20.56368534415484106, 2.639326808657452039E-16 ) ) ;
#18991 = CARTESIAN_POINT ( 'NONE',  ( 6.204703633549690345, 37.84541550158063927, 14.16423886937410082 ) ) ;
#18992 = CARTESIAN_POINT ( 'NONE',  ( 21.92686044187656336, 11.97997603579417536, 3.195792623639536423 ) ) ;
#18993 = EDGE_CURVE ( 'NONE', #51268, #9175, #58569, .T. ) ;
#18994 = CARTESIAN_POINT ( 'NONE',  ( 10.00000000000000178, 55.37363466993042493, 12.81628187352647608 ) ) ;
#18995 = ORIENTED_EDGE ( 'NONE', *, *, #22814, .T. ) ;
#18996 = CARTESIAN_POINT ( 'NONE',  ( 21.09922568453594849, 6.206968003263753531, 6.408140936763242479 ) ) ;
#18997 =( NAMED_UNIT ( * ) SI_UNIT ( $, .STERADIAN. ) SOLID_ANGLE_UNIT ( ) );
#18998 = EDGE_CURVE ( 'NONE', #24577, #40665, #96587, .T. ) ;
#18999 = CARTESIAN_POINT ( 'NONE',  ( 15.44008868035555260, 34.73035201082151247, 9.422509992056143702 ) ) ;
#19000 = CARTESIAN_POINT ( 'NONE',  ( 18.52753015748618282, 63.92559781766745886, -4.923371831947291888 ) ) ;
#19001 = ORIENTED_EDGE ( 'NONE', *, *, #36308, .F. ) ;
#19003 = CARTESIAN_POINT ( 'NONE',  ( -1.926860441876564023, 64.68830936912750929, 1.004413902775740781E-15 ) ) ;
#19002 = CARTESIAN_POINT ( 'NONE',  ( 12.63842701281683034, 7.467264484334118713, 9.846743663894596210 ) ) ;
#19004 = EDGE_CURVE ( 'NONE', #74710, #72967, #73481, .T. ) ;
#19005 = CARTESIAN_POINT ( 'NONE',  ( 18.52753015748618282, 18.92559781766745175, -4.923371831947291888 ) ) ;
#19006 = CARTESIAN_POINT ( 'NONE',  ( 0.1532563361054083140, 11.00893115100078568, 1.131784320476157264E-15 ) ) ;
#19007 = CARTESIAN_POINT ( 'NONE',  ( -4.096035146099030300, 15.00000000000000000, 13.90943910019935714 ) ) ;
#19009 = CARTESIAN_POINT ( 'NONE',  ( 0.5774900079438590739, 37.64701867748817676, -5.440088680355550821 ) ) ;
#19008 = CARTESIAN_POINT ( 'NONE',  ( 4.559911319644449179, 53.89701867748817676, 9.422509992056141925 ) ) ;
#19010 = CARTESIAN_POINT ( 'NONE',  ( 20.88017736071110519, 60.56368534415484106, 2.639326808657452039E-16 ) ) ;
#19012 = ORIENTED_EDGE ( 'NONE', *, *, #50734, .T. ) ;
#19011 = CARTESIAN_POINT ( 'NONE',  ( 1.472469842513823179, 21.42559781766745175, 4.923371831947296329 ) ) ;
#19013 = DIRECTION ( 'NONE',  ( 1.000000000000000000, 0.000000000000000000, 0.000000000000000000 ) ) ;
#19014 = CARTESIAN_POINT ( 'NONE',  ( 2.791683348922237240, 50.38393115100078035, -7.208316651077763204 ) ) ;
#19015 = ORIENTED_EDGE ( 'NONE', *, *, #16283, .F. ) ;
#19016 = ORIENTED_EDGE ( 'NONE', *, *, #27881, .F. ) ;
#19017 = CARTESIAN_POINT ( 'NONE',  ( -0.3689425029237898834, 21.17874883491396432, -10.36894250292378850 ) ) ;
#19018 = CARTESIAN_POINT ( 'NONE',  ( 2.258855624577543075, 0.04962891015807205375, 14.57926203528951881 ) ) ;
#19019 = CARTESIAN_POINT ( 'NONE',  ( 6.204703633549690345, 12.84541550158063572, 14.16423886937410082 ) ) ;
#19020 = CARTESIAN_POINT ( 'NONE',  ( 10.00000000000000000, 30.55374883491397142, -14.16423886937410082 ) ) ;
#19021 = CARTESIAN_POINT ( 'NONE',  ( -7.750000000000000000, 0.000000000000000000, -6.250000000000000000 ) ) ;
#19022 = DIRECTION ( 'NONE',  ( 0.6626200482157461602, 0.000000000000000000, -0.7489557207889945278 ) ) ;
#19023 = CARTESIAN_POINT ( 'NONE',  ( 20.88017736071110519, 30.56368534415484106, 2.639326808657452039E-16 ) ) ;
#19024 = LINE ( 'NONE', #3540, #46644 ) ;
#19025 = ORIENTED_EDGE ( 'NONE', *, *, #59229, .F. ) ;
#19026 = CARTESIAN_POINT ( 'NONE',  ( 12.63842701281683034, 22.46726448433411605, 9.846743663894596210 ) ) ;
#19028 = CARTESIAN_POINT ( 'NONE',  ( 7.361572987183169658, 9.967264484334119601, -9.846743663894592657 ) ) ;
#19027 = CARTESIAN_POINT ( 'NONE',  ( 17.96484262340118221, 59.93868534415484106, 7.964842623401181321 ) ) ;
#19029 = CARTESIAN_POINT ( 'NONE',  ( 22.81628187352648496, 41.83196800326375353, -3.434112377981050290 ) ) ;
#19030 = CARTESIAN_POINT ( 'NONE',  ( 7.361572987183169658, 34.96726448433411605, -9.846743663894592657 ) ) ;
#19031 = CIRCLE ( 'NONE', #55790, 0.1000000000000001166 ) ;
#19032 = CARTESIAN_POINT ( 'NONE',  ( 18.00000000000000000, 78.80384757729336798, 3.750000000000000000 ) ) ;
#19033 = CARTESIAN_POINT ( 'NONE',  ( 22.81628187352647785, 31.62363466993042138, 6.195893100308588602E-16 ) ) ;
#19034 = AXIS2_PLACEMENT_3D ( 'NONE', #75193, #74194, #81701 ) ;
#19035 = CARTESIAN_POINT ( 'NONE',  ( -14.16423886937410437, -38.40458449841935362, -3.795296366450299885 ) ) ;
#19036 = CARTESIAN_POINT ( 'NONE',  ( 7.361572987183169658, 29.96726448433411960, -9.846743663894592657 ) ) ;
#19037 = CARTESIAN_POINT ( 'NONE',  ( 17.08211943468705130, 13.47041550158063572, 12.26659068614894998 ) ) ;
#19038 = ORIENTED_EDGE ( 'NONE', *, *, #94988, .F. ) ;
#19039 = CARTESIAN_POINT ( 'NONE',  ( 10.00000000000000178, 44.31368534415484106, 10.88017736071110342 ) ) ;
#19040 = CARTESIAN_POINT ( 'NONE',  ( 10.00000000000000000, 51.81368534415484106, -10.88017736071110342 ) ) ;
#19041 = CARTESIAN_POINT ( 'NONE',  ( 22.26659068614895176, 44.72041550158063927, -7.082119434687042414 ) ) ;
#19042 = CARTESIAN_POINT ( 'NONE',  ( 5.076628168052703671, 56.84226448433412315, 8.527530157486179263 ) ) ;
#19043 = CARTESIAN_POINT ( 'NONE',  ( 14.92337183194729988, 14.34226448433411782, -8.527530157486177487 ) ) ;
#19045 = CARTESIAN_POINT ( 'NONE',  ( 0.000000000000000000, 14.49999999999999822, 0.000000000000000000 ) ) ;
#19044 = CARTESIAN_POINT ( 'NONE',  ( 6.565887622018943937, 65.16530133659709634, 12.81628187352647430 ) ) ;
#19046 = CARTESIAN_POINT ( 'NONE',  ( 19.42250999205614193, 40.14701867748817676, 5.440088680355555262 ) ) ;
#19047 = CARTESIAN_POINT ( 'NONE',  ( -5.078940136053648580, -28.66985681914853146, -2.500000000000000000 ) ) ;
#19048 = CARTESIAN_POINT ( 'NONE',  ( -2.816281873526473856, 29.12363466993041783, 9.499525473075851096E-16 ) ) ;
#19049 = CARTESIAN_POINT ( 'NONE',  ( 0.1532563361054100626, 50.80059781766745175, -2.638427012816831230 ) ) ;
#19050 = CARTESIAN_POINT ( 'NONE',  ( 7.964842623401177768, 21.18868534415484106, -7.964842623401181321 ) ) ;
#19051 = CARTESIAN_POINT ( 'NONE',  ( 19.42250999205614548, 65.98035201082151957, -5.440088680355545492 ) ) ;
#19052 = AXIS2_PLACEMENT_3D ( 'NONE', #75577, #37591, #1080 ) ;
#19053 = CARTESIAN_POINT ( 'NONE',  ( 4.559911319644449179, 8.897018677488171434, 9.422509992056141925 ) ) ;
#19054 = DIRECTION ( 'NONE',  ( 1.000000000000000000, 0.000000000000000000, -0.000000000000000000 ) ) ;
#19055 = CARTESIAN_POINT ( 'NONE',  ( -0.8801773607110991993, 67.85535201082151957, -2.915334737309923874 ) ) ;
#19056 = CARTESIAN_POINT ( 'NONE',  ( 0.5774900079438590739, 67.64701867748817676, -5.440088680355550821 ) ) ;
#19057 = CARTESIAN_POINT ( 'NONE',  ( 18.00000000000000000, 77.07179676972447169, -4.250000000000000000 ) ) ;
#19058 = CARTESIAN_POINT ( 'NONE',  ( 1.472469842513823179, 41.42559781766745886, 4.923371831947296329 ) ) ;
#19059 = CARTESIAN_POINT ( 'NONE',  ( 0.5774900079438590739, 17.64701867748817321, -5.440088680355550821 ) ) ;
#19060 = CARTESIAN_POINT ( 'NONE',  ( 12.63842701281683922, 59.55059781766744464, -9.846743663894590881 ) ) ;
#19062 = CARTESIAN_POINT ( 'NONE',  ( -9.065164099344372062, 14.49999999999999822, -11.95084933600779742 ) ) ;
#19061 = CARTESIAN_POINT ( 'NONE',  ( 17.96484262340118221, 36.18868534415484106, -7.964842623401177768 ) ) ;
#19063 = CARTESIAN_POINT ( 'NONE',  ( 16.40814093676323893, 40.79030133659708923, 11.09922568453595026 ) ) ;
#19064 = ORIENTED_EDGE ( 'NONE', *, *, #46893, .F. ) ;
#19065 = CARTESIAN_POINT ( 'NONE',  ( 2.035157376598822676, 47.43868534415484817, -7.964842623401177768 ) ) ;
#19066 = CARTESIAN_POINT ( 'NONE',  ( 21.09922568453595559, 27.04030133659708568, -6.408140936763230044 ) ) ;
#19067 = CARTESIAN_POINT ( 'NONE',  ( 0.5774900079438607392, 28.48035201082150891, 5.440088680355550821 ) ) ;
#19068 = CARTESIAN_POINT ( 'NONE',  ( 4.559911319644449179, 2.230352010821504916, -9.422509992056141925 ) ) ;
#19069 = CARTESIAN_POINT ( 'NONE',  ( 14.92337183194729633, 42.67559781766745886, 8.527530157486181039 ) ) ;
#19070 = AXIS2_PLACEMENT_3D ( 'NONE', #74853, #42393, #36863 ) ;
#19071 = CARTESIAN_POINT ( 'NONE',  ( 5.076628168052703671, 6.842264484334118713, 8.527530157486179263 ) ) ;
#19072 = CARTESIAN_POINT ( 'NONE',  ( -0.8801773607111008646, 58.27201867748816966, 2.915334737309923430 ) ) ;
#19073 = CARTESIAN_POINT ( 'NONE',  ( 2.962741594152983993, -0.03417435944610275333, 13.93860331045674883 ) ) ;
#19074 = CARTESIAN_POINT ( 'NONE',  ( 20.36894250292379738, 34.92874883491396076, -10.36894250292379027 ) ) ;
#19075 = AXIS2_PLACEMENT_3D ( 'NONE', #58379, #87051, #13893 ) ;
#19076 = ADVANCED_FACE ( 'NONE', ( #78441 ), #94425, .T. ) ;
#19077 = CARTESIAN_POINT ( 'NONE',  ( -9.402796353261203777, 0.5000000000000004441, 11.68706210897750708 ) ) ;
#19078 = CARTESIAN_POINT ( 'NONE',  ( -3.500000001642929792, 0.08393865083518964321, -4.000000000003232081 ) ) ;
#19079 = ORIENTED_EDGE ( 'NONE', *, *, #48113, .T. ) ;
#19080 = VERTEX_POINT ( 'NONE', #71925 ) ;
#19081 = CARTESIAN_POINT ( 'NONE',  ( -4.164238869374099927, 47.01208216824729647, 3.795296366450308767 ) ) ;
#19082 = CARTESIAN_POINT ( 'NONE',  ( 17.08211943468705840, 55.13708216824731068, -12.26659068614894466 ) ) ;
#19083 = CARTESIAN_POINT ( 'NONE',  ( 0.1532563361054100626, 10.80059781766745175, -2.638427012816831230 ) ) ;
#19084 = CARTESIAN_POINT ( 'NONE',  ( 10.00000000000000000, 17.87363466993041783, -12.81628187352647608 ) ) ;
#19085 = CARTESIAN_POINT ( 'NONE',  ( -42.94000000000001194, 92.00000000000000000, -8.999999999999998224 ) ) ;
#19087 = CARTESIAN_POINT ( 'NONE',  ( 22.81628187352647785, 36.41530133659707502, 3.434112377981063169 ) ) ;
#19086 = CARTESIAN_POINT ( 'NONE',  ( 0.5774900079438590739, 2.647018677488170990, -5.440088680355550821 ) ) ;
#19088 = CARTESIAN_POINT ( 'NONE',  ( 6.204703633549690345, 45.76208216824729647, -14.16423886937410259 ) ) ;
#19089 = FACE_BOUND ( 'NONE', #47864, .T. ) ;
#19090 = CARTESIAN_POINT ( 'NONE',  ( 20.88017736071110164, 65.35535201082150536, 2.915334737309930979 ) ) ;
#19091 = CARTESIAN_POINT ( 'NONE',  ( 8.527530157486179263, -1.907735515665878623, 4.923371831947292776 ) ) ;
#19092 = EDGE_LOOP ( 'NONE', ( #69382, #6794, #62359, #921 ) ) ;
#19093 = CARTESIAN_POINT ( 'NONE',  ( -33.19000000000001194, 92.00000000000000000, -10.09898361729590199 ) ) ;
#19094 = CARTESIAN_POINT ( 'NONE',  ( 19.84674366389459266, 13.30059781766745353, 2.638427012816836559 ) ) ;
#19095 = EDGE_LOOP ( 'NONE', ( #42235, #54972, #63922, #6426 ) ) ;
#19097 = CARTESIAN_POINT ( 'NONE',  ( 19.42250999205614193, 10.14701867748816966, 5.440088680355555262 ) ) ;
#19096 = CARTESIAN_POINT ( 'NONE',  ( -0.8801773607111009756, 13.06368534415483929, 1.068504757029289695E-15 ) ) ;
#19099 = CARTESIAN_POINT ( 'NONE',  ( 6.565887622018943937, 0.1653013365970866511, 12.81628187352647430 ) ) ;
#19098 = CARTESIAN_POINT ( 'NONE',  ( 18.52753015748618282, 53.92559781766745175, -4.923371831947291888 ) ) ;
#19100 = ADVANCED_FACE ( 'NONE', ( #17949 ), #3446, .T. ) ;
#19101 = CARTESIAN_POINT ( 'NONE',  ( 10.00000000000000000, 17.87363466993041783, -12.81628187352647608 ) ) ;
#19102 = EDGE_LOOP ( 'NONE', ( #27958, #24021, #80086, #27171 ) ) ;
#19103 = CARTESIAN_POINT ( 'NONE',  ( 10.00000000000000000, 65.55374883491396076, -14.16423886937410082 ) ) ;
#19104 = ORIENTED_EDGE ( 'NONE', *, *, #21862, .T. ) ;
#19105 = CARTESIAN_POINT ( 'NONE',  ( -4.164238869374099039, 61.80374883491397497, 8.674139862899312516E-16 ) ) ;
#19106 = ORIENTED_EDGE ( 'NONE', *, *, #16488, .F. ) ;
#19107 = CARTESIAN_POINT ( 'NONE',  ( 17.96484262340118221, 31.18868534415483751, -7.964842623401177768 ) ) ;
#19108 = CIRCLE ( 'NONE', #65421, 14.49999999999999822 ) ;
#19109 = CARTESIAN_POINT ( 'NONE',  ( 19.42250999205614548, 50.98035201082151247, -5.440088680355545492 ) ) ;
#19110 = CARTESIAN_POINT ( 'NONE',  ( 19.42250999205614548, 50.98035201082151247, -5.440088680355545492 ) ) ;
#19111 = DIRECTION ( 'NONE',  ( -0.9975640502598243087, 0.06975647374412544122, 0.000000000000000000 ) ) ;
#19112 = CARTESIAN_POINT ( 'NONE',  ( 4.559911319644449179, 38.89701867748817676, 9.422509992056141925 ) ) ;
#19113 = TOROIDAL_SURFACE ( 'NONE', #41550, 2.899999999999999467, 0.1000000000000000056 ) ;
#19114 = AXIS2_PLACEMENT_3D ( 'NONE', #96441, #58910, #20924 ) ;
#19116 = ORIENTED_EDGE ( 'NONE', *, *, #68231, .F. ) ;
#19115 = CARTESIAN_POINT ( 'NONE',  ( -8.000000000000000000, 80.99999999999994316, 0.000000000000000000 ) ) ;
#19117 = CARTESIAN_POINT ( 'NONE',  ( 10.00000000000000000, 9.758931151000785675, -9.846743663894594434 ) ) ;
#19118 = ORIENTED_EDGE ( 'NONE', *, *, #61724, .T. ) ;
#19119 = CARTESIAN_POINT ( 'NONE',  ( 9.479672251299419372, -19.63639846205726158, 4.000000000000000000 ) ) ;
#19120 = CARTESIAN_POINT ( 'NONE',  ( 0.1532563361054082862, 46.21726448433411605, 2.638427012816831674 ) ) ;
#19121 = CARTESIAN_POINT ( 'NONE',  ( 19.72487221294571569, 52.80223176428831522, -6.499999999999990230 ) ) ;
#19122 = CARTESIAN_POINT ( 'NONE',  ( 3.591859063236763294, 58.29030133659708923, -11.09922568453595026 ) ) ;
#19123 = CARTESIAN_POINT ( 'NONE',  ( -4.247994584727555534, -13.56436116443237516, 2.750000000000000000 ) ) ;
#19124 = ORIENTED_EDGE ( 'NONE', *, *, #18908, .F. ) ;
#19125 = CIRCLE ( 'NONE', #4733, 2.900000000000002576 ) ;
#19126 = EDGE_CURVE ( 'NONE', #14813, #105, #74880, .T. ) ;
#19127 = CARTESIAN_POINT ( 'NONE',  ( -4.250000000000000000, 10.25000000000000000, 3.750000000000000000 ) ) ;
#19128 = CARTESIAN_POINT ( 'NONE',  ( 18.72515096720568195, 31.07228050351032422, -6.500000000000018652 ) ) ;
#19130 = CARTESIAN_POINT ( 'NONE',  ( 14.92337183194729988, 29.34226448433411960, -8.527530157486177487 ) ) ;
#19129 = FACE_OUTER_BOUND ( 'NONE', #41124, .T. ) ;
#19131 = CARTESIAN_POINT ( 'NONE',  ( 10.00000000000000000, 60.55374883491397497, -14.16423886937410082 ) ) ;
#19132 = DIRECTION ( 'NONE',  ( 0.9961946980917462113, -0.08715574274765140739, 0.000000000000000000 ) ) ;
#19133 = ORIENTED_EDGE ( 'NONE', *, *, #34208, .F. ) ;
#19134 = B_SPLINE_CURVE_WITH_KNOTS ( 'NONE', 3,
 ( #36850, #12365, #73848, #34862, #58845, #5378 ),
 .UNSPECIFIED., .F., .F.,
 ( 4, 2, 4 ),
 ( 3.409110551494645334E-05, 0.0004400426677367917216, 0.0008459942299586370711 ),
 .UNSPECIFIED. ) ;
#19135 = CARTESIAN_POINT ( 'NONE',  ( -0.4278561937607772148, 0.000000000000000000, -5.436428395565747529 ) ) ;
#19136 = CARTESIAN_POINT ( 'NONE',  ( 18.52753015748617571, 28.09226448433411960, 4.923371831947298993 ) ) ;
#19137 = CARTESIAN_POINT ( 'NONE',  ( 21.09922568453595559, 62.04030133659709634, -6.408140936763230044 ) ) ;
#19138 = CARTESIAN_POINT ( 'NONE',  ( 22.81628187352647785, 11.62363466993042138, 6.195893100308588602E-16 ) ) ;
#19140 = EDGE_CURVE ( 'NONE', #48484, #28000, #54220, .T. ) ;
#19139 = CARTESIAN_POINT ( 'NONE',  ( 19.42250999205614548, 65.98035201082151957, -5.440088680355545492 ) ) ;
#19141 =( LENGTH_UNIT ( ) NAMED_UNIT ( * ) SI_UNIT ( .MILLI., .METRE. ) );
#19142 = CARTESIAN_POINT ( 'NONE',  ( 18.52753015748617571, 3.092264484334118269, 4.923371831947298993 ) ) ;
#19143 = CARTESIAN_POINT ( 'NONE',  ( 1.472469842513823179, 56.42559781766745886, 4.923371831947296329 ) ) ;
#19144 = CYLINDRICAL_SURFACE ( 'NONE', #20361, 11.92686044187656513 ) ;
#19145 = ORIENTED_EDGE ( 'NONE', *, *, #73553, .F. ) ;
#19146 = CARTESIAN_POINT ( 'NONE',  ( 20.36894250292379382, 58.67874883491396076, 10.36894250292379205 ) ) ;
#19147 = CARTESIAN_POINT ( 'NONE',  ( -4.164238869374099927, 12.01208216824730357, 3.795296366450308767 ) ) ;
#19148 = CARTESIAN_POINT ( 'NONE',  ( 1.472469842513823179, 16.42559781766745175, 4.923371831947296329 ) ) ;
#19149 = CARTESIAN_POINT ( 'NONE',  ( 15.44008868035555793, 36.39701867748816966, -9.422509992056140149 ) ) ;
#19151 = CARTESIAN_POINT ( 'NONE',  ( 11.25483282072091384, 12.52949842971371908, 1.007928381667628326 ) ) ;
#19150 = CARTESIAN_POINT ( 'NONE',  ( -2.816281873526473856, 24.12363466993042138, 9.499525473075851096E-16 ) ) ;
#19152 = CARTESIAN_POINT ( 'NONE',  ( 4.559911319644449179, 3.897018677488170990, 9.422509992056141925 ) ) ;
#19153 = EDGE_CURVE ( 'NONE', #13047, #24064, #28398, .T. ) ;
#19154 = FACE_OUTER_BOUND ( 'NONE', #82665, .T. ) ;
#19155 = CARTESIAN_POINT ( 'NONE',  ( 5.076628168052704559, 45.17559781766745175, -8.527530157486179263 ) ) ;
#19156 = CARTESIAN_POINT ( 'NONE',  ( 2.791683348922237240, 10.38393115100078390, -7.208316651077763204 ) ) ;
#19157 = CARTESIAN_POINT ( 'NONE',  ( -2.915334737309917656, -30.89464798917849109, 10.88017736071110164 ) ) ;
#19158 = CARTESIAN_POINT ( 'NONE',  ( 6.565887622018943937, 28.08196800326375353, -12.81628187352647608 ) ) ;
#19159 = CARTESIAN_POINT ( 'NONE',  ( -11.02864780780833520, -96.54579228622785081, -3.999999999999996891 ) ) ;
#19161 = CARTESIAN_POINT ( 'NONE',  ( 13.07907619356932827, 14.76984992095085758, -7.222187741820672358 ) ) ;
#19160 = CARTESIAN_POINT ( 'NONE',  ( 17.96484262340118221, 29.93868534415484106, 7.964842623401181321 ) ) ;
#19162 = CARTESIAN_POINT ( 'NONE',  ( 0.000000000000000000, 14.49999999999999822, 0.000000000000000000 ) ) ;
#19163 = CARTESIAN_POINT ( 'NONE',  ( 13.79529636645031943, 45.34541550158062506, -14.16423886937409904 ) ) ;
#19164 = CARTESIAN_POINT ( 'NONE',  ( 13.79529636645030344, 33.26208216824730357, 14.16423886937410614 ) ) ;
#19165 = CARTESIAN_POINT ( 'NONE',  ( 0.1532563361054100626, 40.80059781766745886, -2.638427012816831230 ) ) ;
#19166 = CARTESIAN_POINT ( 'NONE',  ( 22.81628187352647785, 31.62363466993042138, 6.195893100308588602E-16 ) ) ;
#19167 = CARTESIAN_POINT ( 'NONE',  ( 17.96484262340118221, 29.93868534415484106, 7.964842623401181321 ) ) ;
#19168 = CARTESIAN_POINT ( 'NONE',  ( 10.00000000000000178, 57.25893115100078745, 9.846743663894594434 ) ) ;
#19169 = CARTESIAN_POINT ( 'NONE',  ( 17.96484262340118221, 36.18868534415484106, -7.964842623401177768 ) ) ;
#19170 = CARTESIAN_POINT ( 'NONE',  ( 6.565887622018943937, 8.081968003263751754, -12.81628187352647608 ) ) ;
#19171 = CARTESIAN_POINT ( 'NONE',  ( 10.00000000000000000, 20.55374883491396787, -14.16423886937410082 ) ) ;
#19172 = PLANE ( 'NONE',  #74293 ) ;
#19173 = CARTESIAN_POINT ( 'NONE',  ( 17.20831665107776587, 24.13393115100078035, -7.208316651077762316 ) ) ;
#19174 = CARTESIAN_POINT ( 'NONE',  ( 22.81628187352648496, 61.83196800326376774, -3.434112377981050290 ) ) ;
#19175 = CARTESIAN_POINT ( 'NONE',  ( 7.361572987183169658, 64.96726448433412315, -9.846743663894592657 ) ) ;
#19176 = ORIENTED_EDGE ( 'NONE', *, *, #70639, .T. ) ;
#19177 = CARTESIAN_POINT ( 'NONE',  ( 0.000000000000000000, 0.5000000000000004441, 0.000000000000000000 ) ) ;
#19178 = CARTESIAN_POINT ( 'NONE',  ( 4.526800700887880780, -5.190657137169758073, 3.750000000000001776 ) ) ;
#19179 = CARTESIAN_POINT ( 'NONE',  ( -0.8801773607111008646, 13.27201867748817321, 2.915334737309923430 ) ) ;
#19180 = CARTESIAN_POINT ( 'NONE',  ( 13.79529636645030344, 8.262082168247300018, 14.16423886937410614 ) ) ;
#19181 = CARTESIAN_POINT ( 'NONE',  ( 4.559911319644449179, 68.89701867748817676, 9.422509992056141925 ) ) ;
#19182 = CARTESIAN_POINT ( 'NONE',  ( 2.791683348922240793, 51.63393115100078745, 7.208316651077764092 ) ) ;
#19183 = CARTESIAN_POINT ( 'NONE',  ( 17.96484262340118221, 31.18868534415483751, -7.964842623401177768 ) ) ;
#19184 = DIRECTION ( 'NONE',  ( -0.000000000000000000, -1.000000000000000000, -0.000000000000000000 ) ) ;
#19185 = FACE_OUTER_BOUND ( 'NONE', #29299, .T. ) ;
#19186 = VECTOR ( 'NONE', #33722, 1000.000000000000000 ) ;
#19187 = STYLED_ITEM ( 'NONE', ( #33246 ), #28482 ) ;
#19188 = ADVANCED_FACE ( 'NONE', ( #87905 ), #36895, .T. ) ;
#19189 = ORIENTED_EDGE ( 'NONE', *, *, #94387, .T. ) ;
#19190 = CYLINDRICAL_SURFACE ( 'NONE', #96214, 0.5000000000000000000 ) ;
#19191 = ORIENTED_EDGE ( 'NONE', *, *, #71070, .F. ) ;
#19192 = ORIENTED_EDGE ( 'NONE', *, *, #20344, .F. ) ;
#19193 = DIRECTION ( 'NONE',  ( 0.000000000000000000, 0.000000000000000000, 1.000000000000000000 ) ) ;
#19194 = CARTESIAN_POINT ( 'NONE',  ( -4.164238869374099039, 6.803748834913967869, 8.674139862899312516E-16 ) ) ;
#19195 = CARTESIAN_POINT ( 'NONE',  ( 17.08211943468705840, 15.13708216824730179, -12.26659068614894466 ) ) ;
#19196 = CARTESIAN_POINT ( 'NONE',  ( -0.3689425029237898834, 56.17874883491396076, -10.36894250292378850 ) ) ;
#19197 = CARTESIAN_POINT ( 'NONE',  ( 1.472469842513823179, 61.42559781766745175, 4.923371831947296329 ) ) ;
#19198 = CARTESIAN_POINT ( 'NONE',  ( 5.076628168052703671, 36.84226448433412315, 8.527530157486179263 ) ) ;
#19199 = CARTESIAN_POINT ( 'NONE',  ( 6.565887622018943937, 65.16530133659709634, 12.81628187352647430 ) ) ;
#19201 = CARTESIAN_POINT ( 'NONE',  ( 10.00000000000000178, 67.25893115100079456, 9.846743663894594434 ) ) ;
#19200 = CARTESIAN_POINT ( 'NONE',  ( 15.44008868035555793, 26.39701867748817321, -9.422509992056140149 ) ) ;
#19202 = CARTESIAN_POINT ( 'NONE',  ( 2.917880565312950480, 5.970415501580634832, -12.26659068614894821 ) ) ;
#19203 = ADVANCED_FACE ( 'NONE', ( #35398 ), #89337, .T. ) ;
#19204 = CARTESIAN_POINT ( 'NONE',  ( 17.08211943468705130, 48.47041550158063927, 12.26659068614894998 ) ) ;
#19205 = CARTESIAN_POINT ( 'NONE',  ( -4.164238869374098151, 66.59541550158060375, -3.795296366450310543 ) ) ;
#19206 = CARTESIAN_POINT ( 'NONE',  ( -0.3077640640441539621, 0.000000000000000000, 5.999999999999999112 ) ) ;
#19207 = CARTESIAN_POINT ( 'NONE',  ( -0.1503990784575328088, 3.101585745166421493, 6.262539305110068177 ) ) ;
#19208 = CARTESIAN_POINT ( 'NONE',  ( -2.816281873526473856, 44.33196800326375353, 3.434112377981055619 ) ) ;
#19209 = DIRECTION ( 'NONE',  ( 0.000000000000000000, 1.000000000000000000, 0.000000000000000000 ) ) ;
#19210 = ORIENTED_EDGE ( 'NONE', *, *, #51136, .T. ) ;
#19211 = FACE_OUTER_BOUND ( 'NONE', #93001, .T. ) ;
#19212 = ORIENTED_EDGE ( 'NONE', *, *, #15567, .T. ) ;
#19213 = CARTESIAN_POINT ( 'NONE',  ( 7.361572987183170547, 27.05059781766745175, 9.846743663894590881 ) ) ;
#19214 = ORIENTED_EDGE ( 'NONE', *, *, #16157, .T. ) ;
#19215 = CARTESIAN_POINT ( 'NONE',  ( 24.16423886937410614, 34.30374883491396787, 8.672049930838204340E-16 ) ) ;
#19216 = CARTESIAN_POINT ( 'NONE',  ( 18.52753015748618282, 33.92559781766745886, -4.923371831947291888 ) ) ;
#19217 = CARTESIAN_POINT ( 'NONE',  ( 4.559911319644449179, 58.89701867748817676, 9.422509992056141925 ) ) ;
#19218 = DIRECTION ( 'NONE',  ( -0.8320502943378437211, 0.5547001962252290364, 0.000000000000000000 ) ) ;
#19219 = CARTESIAN_POINT ( 'NONE',  ( 20.88017736071110519, 55.56368534415484817, 2.639326808657452039E-16 ) ) ;
#19220 = CARTESIAN_POINT ( 'NONE',  ( 12.63842701281683922, 44.55059781766745175, -9.846743663894590881 ) ) ;
#19221 = ADVANCED_FACE ( 'NONE', ( #57412 ), #50899, .F. ) ;
#19222 = CARTESIAN_POINT ( 'NONE',  ( 22.81628187352648496, 61.83196800326376774, -3.434112377981050290 ) ) ;
#19223 = CARTESIAN_POINT ( 'NONE',  ( -12.81628187352647963, 8.915301336597083903, -3.434112377981046293 ) ) ;
#19224 = VERTEX_POINT ( 'NONE', #58892 ) ;
#19225 = CARTESIAN_POINT ( 'NONE',  ( -0.8801773607111009756, 48.06368534415484817, 1.068504757029289695E-15 ) ) ;
#19226 = CARTESIAN_POINT ( 'NONE',  ( -2.266590686148945544, 21.38708216824730357, -7.082119434687050408 ) ) ;
#19227 = EDGE_CURVE ( 'NONE', #89066, #29532, #55877, .T. ) ;
#19228 = ORIENTED_EDGE ( 'NONE', *, *, #46768, .T. ) ;
#19229 = CARTESIAN_POINT ( 'NONE',  ( -2.816281873526473856, 29.12363466993041783, 9.499525473075851096E-16 ) ) ;
#19230 = CARTESIAN_POINT ( 'NONE',  ( 0.1532563361054083140, 21.00893115100078745, 1.131784320476157264E-15 ) ) ;
#19231 = CARTESIAN_POINT ( 'NONE',  ( 17.96484262340118221, 16.18868534415483396, -7.964842623401177768 ) ) ;
#19232 = CARTESIAN_POINT ( 'NONE',  ( 6.565887622018943937, 53.08196800326374643, -12.81628187352647608 ) ) ;
#19233 = FACE_OUTER_BOUND ( 'NONE', #2908, .T. ) ;
#19234 = CARTESIAN_POINT ( 'NONE',  ( 5.076628168052704559, 30.17559781766745175, -8.527530157486179263 ) ) ;
#19236 = AXIS2_PLACEMENT_3D ( 'NONE', #29136, #59641, #68146 ) ;
#19235 = CARTESIAN_POINT ( 'NONE',  ( 19.72487221294571569, 19.78217586085237301, 6.499999999999990230 ) ) ;
#19237 = CARTESIAN_POINT ( 'NONE',  ( 14.66196617519559808, 14.76930270348881002, -2.874856965127823294 ) ) ;
#19238 = CARTESIAN_POINT ( 'NONE',  ( -3.750000000000000000, 10.25000000000000000, -2.750000000000000000 ) ) ;
#19239 = CARTESIAN_POINT ( 'NONE',  ( 0.2751277870542914172, 23.21833443783937767, 6.499999999999992006 ) ) ;
#19240 = CARTESIAN_POINT ( 'NONE',  ( 1.796645268984721877, 14.76930270348881180, -14.83273813124059082 ) ) ;
#19241 = CARTESIAN_POINT ( 'NONE',  ( 2.791683348922240793, 6.633931151000785675, 7.208316651077764092 ) ) ;
#19242 = CARTESIAN_POINT ( 'NONE',  ( 0.6178305044545818747, 18.49863466993041428, -9.382169495545419124 ) ) ;
#19243 = LINE ( 'NONE', #12227, #67426 ) ;
#19244 = CARTESIAN_POINT ( 'NONE',  ( 12.63842701281683922, 49.55059781766744464, -9.846743663894590881 ) ) ;
#19245 = DIRECTION ( 'NONE',  ( -1.000000000000000000, 0.000000000000000000, 0.000000000000000000 ) ) ;
#19246 = CARTESIAN_POINT ( 'NONE',  ( 10.00000000000000178, 18.05374883491396787, 14.16423886937410082 ) ) ;
#19247 = CARTESIAN_POINT ( 'NONE',  ( 2.791683348922237240, 35.38393115100079456, -7.208316651077763204 ) ) ;
#19248 = CARTESIAN_POINT ( 'NONE',  ( -2.816281873526473856, 29.33196800326376064, 3.434112377981055619 ) ) ;
#19250 = CARTESIAN_POINT ( 'NONE',  ( 7.595945211628243321, 4.245086020036709294E-16, 12.35117874301647056 ) ) ;
#19249 = DIRECTION ( 'NONE',  ( 5.818595309480553908E-17, 1.000000000000000000, 0.000000000000000000 ) ) ;
#19251 = CARTESIAN_POINT ( 'NONE',  ( -0.8801773607111008646, 68.27201867748817676, 2.915334737309923430 ) ) ;
#19252 = CARTESIAN_POINT ( 'NONE',  ( 10.00000000000000000, 2.873634669930420049, -12.81628187352647608 ) ) ;
#19253 = DIRECTION ( 'NONE',  ( -0.8870108331782182720, 0.000000000000000000, -0.4617486132350404615 ) ) ;
#19254 = CARTESIAN_POINT ( 'NONE',  ( 19.84674366389459621, 38.50893115100078745, 7.409399052514197653E-17 ) ) ;
#19256 = EDGE_CURVE ( 'NONE', #35385, #63050, #70227, .T. ) ;
#19255 = CARTESIAN_POINT ( 'NONE',  ( 4.559911319644449179, 28.89701867748817321, 9.422509992056141925 ) ) ;
#19257 = CARTESIAN_POINT ( 'NONE',  ( 6.565887622018943937, 30.16530133659708568, 12.81628187352647430 ) ) ;
#19258 = CARTESIAN_POINT ( 'NONE',  ( 19.84674366389459621, 28.50893115100078745, 7.409399052514197653E-17 ) ) ;
#19259 = APPLICATION_PROTOCOL_DEFINITION ( 'draft international standard', 'automotive_design', 1998, #67892 ) ;
#19260 = CARTESIAN_POINT ( 'NONE',  ( -11.13303098458958296, 89.96146600687833939, 6.578309274437964760 ) ) ;
#19261 = CARTESIAN_POINT ( 'NONE',  ( 10.00000000000000178, 29.31368534415483751, 10.88017736071110342 ) ) ;
#19262 = ORIENTED_EDGE ( 'NONE', *, *, #69551, .F. ) ;
#19263 = CARTESIAN_POINT ( 'NONE',  ( 10.00000000000000178, 64.31368534415483396, 10.88017736071110342 ) ) ;
#19264 = CARTESIAN_POINT ( 'NONE',  ( 5.800000000000003375, 99.99999999999998579, 8.000000000000000000 ) ) ;
#19266 = CARTESIAN_POINT ( 'NONE',  ( 15.44008868035555260, 24.73035201082150891, 9.422509992056143702 ) ) ;
#19265 = CARTESIAN_POINT ( 'NONE',  ( 1.472469842513823179, 51.42559781766745886, 4.923371831947296329 ) ) ;
#19267 = CARTESIAN_POINT ( 'NONE',  ( 19.72487221294571569, 52.80223176428831522, -6.499999999999990230 ) ) ;
#19268 = CARTESIAN_POINT ( 'NONE',  ( 12.91533473730993009, 46.60535201082150536, -10.88017736071109987 ) ) ;
#19270 = CARTESIAN_POINT ( 'NONE',  ( 20.00000000000000355, 89.78870847431082325, -4.994901225422943902 ) ) ;
#19269 = CARTESIAN_POINT ( 'NONE',  ( 0.5774900079438607392, 23.48035201082150536, 5.440088680355550821 ) ) ;
#19271 = AXIS2_PLACEMENT_3D ( 'NONE', #29602, #44110, #68124 ) ;
#19272 = CARTESIAN_POINT ( 'NONE',  ( 0.1532563361054083140, 6.008931151000784787, 1.131784320476157264E-15 ) ) ;
#19273 = DIRECTION ( 'NONE',  ( 1.000000000000000000, 0.000000000000000000, 0.000000000000000000 ) ) ;
#19274 = CARTESIAN_POINT ( 'NONE',  ( 1.472469842513823179, 45.59226448433412315, -4.923371831947296329 ) ) ;
#19275 = CARTESIAN_POINT ( 'NONE',  ( 17.08211943468705130, 58.47041550158063927, 12.26659068614894998 ) ) ;
#19276 = CIRCLE ( 'NONE', #43252, 14.49999999999999822 ) ;
#19277 =( NAMED_UNIT ( * ) SI_UNIT ( $, .STERADIAN. ) SOLID_ANGLE_UNIT ( ) );
#19278 = CARTESIAN_POINT ( 'NONE',  ( 22.26659068614894466, 13.88708216824730179, 7.082119434687054849 ) ) ;
#19279 = CARTESIAN_POINT ( 'NONE',  ( -0.3689425029237898834, 36.17874883491396787, -10.36894250292378850 ) ) ;
#19280 = CARTESIAN_POINT ( 'NONE',  ( 13.43411237798105340, 5.581968003263753531, 12.81628187352647963 ) ) ;
#19282 = DIRECTION ( 'NONE',  ( 0.5948227867513318223, 0.000000000000000000, 0.8038568606172245001 ) ) ;
#19281 = VECTOR ( 'NONE', #66098, 1000.000000000000000 ) ;
#19283 = EDGE_LOOP ( 'NONE', ( #96687, #51458, #52016, #78385 ) ) ;
#19284 = CARTESIAN_POINT ( 'NONE',  ( 7.084665262690076126, 4.105352010821503583, 10.88017736071109987 ) ) ;
#19285 = CARTESIAN_POINT ( 'NONE',  ( 17.20831665107776587, 32.88393115100078745, 7.208316651077764980 ) ) ;
#19287 = LINE ( 'NONE', #42289, #29518 ) ;
#19286 = CARTESIAN_POINT ( 'NONE',  ( -6.430724159521290950, -88.51069574204372259, -3.750000000000000000 ) ) ;
#19288 = CARTESIAN_POINT ( 'NONE',  ( 20.88017736071110875, 65.77201867748817676, -2.915334737309920765 ) ) ;
#19289 = CARTESIAN_POINT ( 'NONE',  ( 20.15039907845753930, 70.00000000000000000, 6.262539305110068177 ) ) ;
#19290 = CARTESIAN_POINT ( 'NONE',  ( 20.88017736071110164, 25.35535201082150891, 2.915334737309930979 ) ) ;
#19291 = EDGE_CURVE ( 'NONE', #66685, #63139, #65891, .T. ) ;
#19292 = CARTESIAN_POINT ( 'NONE',  ( 0.6178305044545818747, 58.49863466993042493, -9.382169495545419124 ) ) ;
#19293 = CARTESIAN_POINT ( 'NONE',  ( 21.09922568453595559, 12.04030133659708746, -6.408140936763230044 ) ) ;
#19294 = CARTESIAN_POINT ( 'NONE',  ( 17.20831665107776587, 32.88393115100078745, 7.208316651077764980 ) ) ;
#19295 = ORIENTED_EDGE ( 'NONE', *, *, #43911, .T. ) ;
#19296 = FILL_AREA_STYLE_COLOUR ( '', #83623 ) ;
#19297 = CARTESIAN_POINT ( 'NONE',  ( 18.28836319691945889, 4.344927826957708739, 6.500000000000004441 ) ) ;
#19298 = CARTESIAN_POINT ( 'NONE',  ( 24.16423886937410614, 64.30374883491396076, 8.672049930838204340E-16 ) ) ;
#19299 = CARTESIAN_POINT ( 'NONE',  ( 22.26659068614895176, 24.72041550158063572, -7.082119434687042414 ) ) ;
#19300 = CARTESIAN_POINT ( 'NONE',  ( 19.42250999205614548, 35.98035201082151247, -5.440088680355545492 ) ) ;
#19301 = CARTESIAN_POINT ( 'NONE',  ( 2.035157376598822676, 47.43868534415484817, -7.964842623401177768 ) ) ;
#19302 = DIRECTION ( 'NONE',  ( 0.000000000000000000, -1.000000000000000000, 0.000000000000000000 ) ) ;
#19303 = CARTESIAN_POINT ( 'NONE',  ( 11.19532855855632292, -77.48518070178161565, -3.999999999999999112 ) ) ;
#19304 = CARTESIAN_POINT ( 'NONE',  ( 19.84674366389459621, 8.508931151000785675, 7.409399052514197653E-17 ) ) ;
#19305 = FACE_OUTER_BOUND ( 'NONE', #16743, .T. ) ;
#19306 = CARTESIAN_POINT ( 'NONE',  ( 7.361572987183170547, 22.05059781766745530, 9.846743663894590881 ) ) ;
#19307 = CARTESIAN_POINT ( 'NONE',  ( 10.00000000000000000, 54.75893115100078745, -9.846743663894594434 ) ) ;
#19308 = AXIS2_PLACEMENT_3D ( 'NONE', #76314, #7832, #38328 ) ;
#19309 = EDGE_CURVE ( 'NONE', #47024, #58376, #81394, .T. ) ;
#19310 = B_SPLINE_CURVE_WITH_KNOTS ( 'NONE', 3,
 ( #34629, #87146, #79660, #96149 ),
 .UNSPECIFIED., .F., .F.,
 ( 4, 4 ),
 ( 0.000000000000000000, 0.001036303429213300022 ),
 .UNSPECIFIED. ) ;
#19311 = CARTESIAN_POINT ( 'NONE',  ( 6.565887622018943937, 48.08196800326375353, -12.81628187352647608 ) ) ;
#19312 = FILL_AREA_STYLE ('',( #35289 ) ) ;
#19313 = CARTESIAN_POINT ( 'NONE',  ( 2.035157376598824452, 63.68868534415484106, 7.964842623401179544 ) ) ;
#19314 = CARTESIAN_POINT ( 'NONE',  ( 0.1532563361054083140, 31.00893115100078390, 1.131784320476157264E-15 ) ) ;
#19316 = CARTESIAN_POINT ( 'NONE',  ( 18.52753015748618282, 23.92559781766745530, -4.923371831947291888 ) ) ;
#19315 = CARTESIAN_POINT ( 'NONE',  ( -4.164238869374099039, 61.80374883491397497, 8.674139862899312516E-16 ) ) ;
#19318 = EDGE_CURVE ( 'NONE', #48243, #84680, #88409, .T. ) ;
#19317 = CARTESIAN_POINT ( 'NONE',  ( 0.2751277870542909176, 60.30223176428830101, 6.499999999999992006 ) ) ;
#19319 = ADVANCED_FACE ( 'NONE', ( #19909 ), #81883, .T. ) ;
#19320 = LINE ( 'NONE', #27796, #3960 ) ;
#19321 = CARTESIAN_POINT ( 'NONE',  ( 24.16423886937410614, 19.30374883491397142, 8.672049930838204340E-16 ) ) ;
#19322 = CARTESIAN_POINT ( 'NONE',  ( 24.16423886937410614, 29.51208216824729647, -3.795296366450302550 ) ) ;
#19323 = CARTESIAN_POINT ( 'NONE',  ( 10.00000000000000000, 39.75893115100078745, -9.846743663894594434 ) ) ;
#19324 = MECHANICAL_DESIGN_GEOMETRIC_PRESENTATION_REPRESENTATION (  '', ( #8123 ), #54502 ) ;
#19325 = CARTESIAN_POINT ( 'NONE',  ( 19.80427997160309417, 12.75733960839543890, -6.500000000000000888 ) ) ;
#19326 = CARTESIAN_POINT ( 'NONE',  ( 20.88017736071110519, 30.56368534415484106, 2.639326808657452039E-16 ) ) ;
#19327 = CARTESIAN_POINT ( 'NONE',  ( -0.8801773607111008646, 53.27201867748816966, 2.915334737309923430 ) ) ;
#19328 = FILL_AREA_STYLE ('',( #89302 ) ) ;
#19329 = ORIENTED_EDGE ( 'NONE', *, *, #30598, .F. ) ;
#19330 = CARTESIAN_POINT ( 'NONE',  ( 16.40814093676323893, 50.79030133659708923, 11.09922568453595026 ) ) ;
#19331 = CARTESIAN_POINT ( 'NONE',  ( -0.8801773607111008646, 58.27201867748816966, 2.915334737309923430 ) ) ;
#19332 = ORIENTED_EDGE ( 'NONE', *, *, #86156, .T. ) ;
#19333 = DIRECTION ( 'NONE',  ( 0.000000000000000000, 1.000000000000000000, 0.000000000000000000 ) ) ;
#19334 = DIRECTION ( 'NONE',  ( -1.000000000000000000, 0.000000000000000000, 0.000000000000000000 ) ) ;
#19335 = CARTESIAN_POINT ( 'NONE',  ( 10.00000000000000178, 69.31368534415484817, 10.88017736071110342 ) ) ;
#19336 = EDGE_LOOP ( 'NONE', ( #11417, #47132, #41714, #61142 ) ) ;
#19337 = CARTESIAN_POINT ( 'NONE',  ( 7.084665262690076126, 64.10535201082150536, 10.88017736071109987 ) ) ;
#19338 = CARTESIAN_POINT ( 'NONE',  ( 19.42250999205614548, 20.98035201082150891, -5.440088680355545492 ) ) ;
#19339 = CARTESIAN_POINT ( 'NONE',  ( 13.78891971893208357, 15.00000000000000000, -5.904717858191528279 ) ) ;
#19340 = DIRECTION ( 'NONE',  ( 0.000000000000000000, 0.000000000000000000, 1.000000000000000000 ) ) ;
#19341 = CARTESIAN_POINT ( 'NONE',  ( 0.5774900079438607392, 8.480352010821505360, 5.440088680355550821 ) ) ;
#19342 = CARTESIAN_POINT ( 'NONE',  ( 14.92337183194729988, 9.342264484334119601, -8.527530157486177487 ) ) ;
#19343 = CARTESIAN_POINT ( 'NONE',  ( 17.08211943468705130, 13.47041550158063572, 12.26659068614894998 ) ) ;
#19344 = CARTESIAN_POINT ( 'NONE',  ( -0.8801773607111008646, 18.27201867748817321, 2.915334737309923430 ) ) ;
#19345 = CARTESIAN_POINT ( 'NONE',  ( 1.472469842513823179, 61.42559781766745175, 4.923371831947296329 ) ) ;
#19346 = VERTEX_POINT ( 'NONE', #13395 ) ;
#19347 = EDGE_CURVE ( 'NONE', #53389, #51268, #80910, .T. ) ;
#19348 = CARTESIAN_POINT ( 'NONE',  ( 2.791683348922240793, 56.63393115100078035, 7.208316651077764092 ) ) ;
#19349 = VERTEX_POINT ( 'NONE', #96421 ) ;
#19350 = CARTESIAN_POINT ( 'NONE',  ( 20.88017736071110164, 55.35535201082149825, 2.915334737309930979 ) ) ;
#19351 = CARTESIAN_POINT ( 'NONE',  ( 5.076628168052703671, 46.84226448433412315, 8.527530157486179263 ) ) ;
#19352 = CARTESIAN_POINT ( 'NONE',  ( 21.09922568453594849, 41.20696800326375353, 6.408140936763242479 ) ) ;
#19354 = CARTESIAN_POINT ( 'NONE',  ( -13.48255862861917009, 15.00000000000000000, -5.335786055104346559 ) ) ;
#19353 = CARTESIAN_POINT ( 'NONE',  ( 4.559911319644449179, 7.230352010821504471, -9.422509992056141925 ) ) ;
#19355 = CARTESIAN_POINT ( 'NONE',  ( 20.88017736071110519, 55.56368534415484817, 2.639326808657452039E-16 ) ) ;
#19356 = CARTESIAN_POINT ( 'NONE',  ( 0.5774900079438590739, 7.647018677488171434, -5.440088680355550821 ) ) ;
#19357 = AXIS2_PLACEMENT_3D ( 'NONE', #97894, #14881, #82862 ) ;
#19358 = AXIS2_PLACEMENT_3D ( 'NONE', #53333, #38842, #83842 ) ;
#19359 = AXIS2_PLACEMENT_3D ( 'NONE', #67003, #44981, #67501 ) ;
#19360 = CARTESIAN_POINT ( 'NONE',  ( 10.00000000000000000, 42.87363466993042493, -12.81628187352647608 ) ) ;
#19361 = CARTESIAN_POINT ( 'NONE',  ( 12.91533473730993009, 36.60535201082151247, -10.88017736071109987 ) ) ;
#19362 = CARTESIAN_POINT ( 'NONE',  ( 0.2751277870542980231, 10.30223176428831522, 6.500000000000002665 ) ) ;
#19363 = B_SPLINE_CURVE_WITH_KNOTS ( 'NONE', 3,
 ( #88772, #97288, #89268, #79797, #66259, #11789 ),
 .UNSPECIFIED., .F., .F.,
 ( 4, 2, 4 ),
 ( 3.409110551495833213E-05, 0.0004400426677367820722, 0.0008459942299586057377 ),
 .UNSPECIFIED. ) ;
#19364 = EDGE_LOOP ( 'NONE', ( #85820, #84549, #87998, #63599 ) ) ;
#19365 = CARTESIAN_POINT ( 'NONE',  ( 19.38216949554541557, 47.24863466993041783, -9.382169495545420901 ) ) ;
#19366 = CARTESIAN_POINT ( 'NONE',  ( 20.88017736071110519, 40.56368534415484106, 2.639326808657452039E-16 ) ) ;
#19367 = CARTESIAN_POINT ( 'NONE',  ( 7.361572987183169658, 59.96726448433410894, -9.846743663894592657 ) ) ;
#19368 = ORIENTED_EDGE ( 'NONE', *, *, #40332, .F. ) ;
#19369 = CARTESIAN_POINT ( 'NONE',  ( 5.076628168052703671, 61.84226448433412315, 8.527530157486179263 ) ) ;
#19371 = CARTESIAN_POINT ( 'NONE',  ( 19.84674366389459266, 53.30059781766744464, 2.638427012816836559 ) ) ;
#19370 = LINE ( 'NONE', #11864, #45227 ) ;
#19372 = CARTESIAN_POINT ( 'NONE',  ( 7.084665262690076126, 24.10535201082150181, 10.88017736071109987 ) ) ;
#19373 = DIRECTION ( 'NONE',  ( -0.8320502943378437211, 0.5547001962252290364, 0.000000000000000000 ) ) ;
#19374 = CARTESIAN_POINT ( 'NONE',  ( 1.472469842513823179, 40.59226448433411605, -4.923371831947296329 ) ) ;
#19375 = DIRECTION ( 'NONE',  ( 0.000000000000000000, 0.000000000000000000, -1.000000000000000000 ) ) ;
#19376 = CARTESIAN_POINT ( 'NONE',  ( 18.17884179759845509, 58.66688879859523098, -6.500000000000054179 ) ) ;
#19377 = CARTESIAN_POINT ( 'NONE',  ( 0.1532563361054082862, 46.21726448433411605, 2.638427012816831674 ) ) ;
#19378 = FILL_AREA_STYLE ('',( #5373 ) ) ;
#19380 = VERTEX_POINT ( 'NONE', #58384 ) ;
#19379 = CARTESIAN_POINT ( 'NONE',  ( 0.1532563361054083140, 56.00893115100078745, 1.131784320476157264E-15 ) ) ;
#19381 = AXIS2_PLACEMENT_3D ( 'NONE', #53483, #29488, #45492 ) ;
#19382 = CARTESIAN_POINT ( 'NONE',  ( 13.43411237798105340, 45.58196800326374643, 12.81628187352647963 ) ) ;
#19383 = CARTESIAN_POINT ( 'NONE',  ( 2.791683348922237240, 45.38393115100079456, -7.208316651077763204 ) ) ;
#19384 = CARTESIAN_POINT ( 'NONE',  ( 2.917880565312950480, 65.97041550158063217, -12.26659068614894821 ) ) ;
#19385 = CARTESIAN_POINT ( 'NONE',  ( 18.52753015748617571, 28.09226448433411960, 4.923371831947298993 ) ) ;
#19386 = CARTESIAN_POINT ( 'NONE',  ( 8.549892366338843530, 14.76930270348882068, -12.25305656628354534 ) ) ;
#19387 = CARTESIAN_POINT ( 'NONE',  ( 22.26659068614894466, 53.88708216824731068, 7.082119434687054849 ) ) ;
#19388 = CARTESIAN_POINT ( 'NONE',  ( 2.791683348922240793, 66.63393115100079456, 7.208316651077764092 ) ) ;
#19389 = CARTESIAN_POINT ( 'NONE',  ( 2.035157376598824452, 3.688685344154837953, 7.964842623401179544 ) ) ;
#19390 = CARTESIAN_POINT ( 'NONE',  ( 10.00000000000000000, 35.55374883491396787, -14.16423886937410082 ) ) ;
#19391 = CARTESIAN_POINT ( 'NONE',  ( 2.917880565312950480, 35.97041550158063217, -12.26659068614894821 ) ) ;
#19392 = DIRECTION ( 'NONE',  ( 0.000000000000000000, 1.000000000000000000, 0.000000000000000000 ) ) ;
#19393 = VECTOR ( 'NONE', #11570, 1000.000000000000000 ) ;
#19394 = CARTESIAN_POINT ( 'NONE',  ( 10.00000000000000178, 17.25893115100078745, 9.846743663894594434 ) ) ;
#19396 = CARTESIAN_POINT ( 'NONE',  ( 10.00000000000000178, 5.373634669930420493, 12.81628187352647608 ) ) ;
#19395 = DIRECTION ( 'NONE',  ( 0.000000000000000000, 0.000000000000000000, 1.000000000000000000 ) ) ;
#19397 = CARTESIAN_POINT ( 'NONE',  ( 17.96484262340118221, 46.18868534415484106, -7.964842623401177768 ) ) ;
#19398 = EDGE_CURVE ( 'NONE', #18711, #76195, #86210, .T. ) ;
#19399 = CARTESIAN_POINT ( 'NONE',  ( 8.880000000000000782, 1.019547802438458550, 3.750000000000000000 ) ) ;
#19400 = CARTESIAN_POINT ( 'NONE',  ( 0.1532563361054100626, 50.80059781766745175, -2.638427012816831230 ) ) ;
#19401 = LINE ( 'NONE', #25924, #82555 ) ;
#19402 = CARTESIAN_POINT ( 'NONE',  ( 14.92337183194729988, 49.34226448433411605, -8.527530157486177487 ) ) ;
#19403 = CARTESIAN_POINT ( 'NONE',  ( 6.204703633549690345, 0.7620821682473009062, -14.16423886937410259 ) ) ;
#19404 = ORIENTED_EDGE ( 'NONE', *, *, #6341, .T. ) ;
#19405 = CARTESIAN_POINT ( 'NONE',  ( 6.204703633549690345, 25.76208216824730712, -14.16423886937410259 ) ) ;
#19406 = CARTESIAN_POINT ( 'NONE',  ( -14.73513795193454534, 14.95077488074854166, 0.7223639599945808065 ) ) ;
#19407 = CARTESIAN_POINT ( 'NONE',  ( 0.2751277870542967463, 70.00000000000000000, -6.500000000000000888 ) ) ;
#19408 = CARTESIAN_POINT ( 'NONE',  ( 15.44008868035555260, 24.73035201082150891, 9.422509992056143702 ) ) ;
#19409 = CARTESIAN_POINT ( 'NONE',  ( 16.40814093676323893, 25.79030133659708923, 11.09922568453595026 ) ) ;
#19410 = CYLINDRICAL_SURFACE ( 'NONE', #60818, 3.940000000000000835 ) ;
#19411 = CARTESIAN_POINT ( 'NONE',  ( 18.52753015748617571, 13.09226448433411960, 4.923371831947298993 ) ) ;
#19412 = CARTESIAN_POINT ( 'NONE',  ( 21.09922568453595559, 52.04030133659708923, -6.408140936763230044 ) ) ;
#19413 = ORIENTED_EDGE ( 'NONE', *, *, #23514, .T. ) ;
#19414 = CARTESIAN_POINT ( 'NONE',  ( 6.034747819232443078, -36.07388523689489546, -3.750000000000000000 ) ) ;
#19415 = CARTESIAN_POINT ( 'NONE',  ( 22.26659068614895176, 29.72041550158063572, -7.082119434687042414 ) ) ;
#19416 = DIRECTION ( 'NONE',  ( 0.000000000000000000, -0.000000000000000000, -1.000000000000000000 ) ) ;
#19417 = FACE_OUTER_BOUND ( 'NONE', #80323, .T. ) ;
#19418 = CARTESIAN_POINT ( 'NONE',  ( 2.035157376598824452, 13.68868534415483751, 7.964842623401179544 ) ) ;
#19419 = CARTESIAN_POINT ( 'NONE',  ( 8.629999999999995453, 41.24999999999999289, 6.250000000000000000 ) ) ;
#19420 = CARTESIAN_POINT ( 'NONE',  ( 4.391700990647163572, 0.2306972965111900586, -14.28114200970190240 ) ) ;
#19421 = CARTESIAN_POINT ( 'NONE',  ( 17.96484262340118221, 46.18868534415484106, -7.964842623401177768 ) ) ;
#19422 = CARTESIAN_POINT ( 'NONE',  ( 20.88017736071110164, 50.35535201082151247, 2.915334737309930979 ) ) ;
#19423 = CARTESIAN_POINT ( 'NONE',  ( 6.565887622018943937, 10.16530133659708746, 12.81628187352647430 ) ) ;
#19424 = CARTESIAN_POINT ( 'NONE',  ( 5.076628168052704559, 65.17559781766745175, -8.527530157486179263 ) ) ;
#19425 = CARTESIAN_POINT ( 'NONE',  ( 19.72487221294571569, 59.78217586085237656, 6.499999999999986677 ) ) ;
#19426 = CARTESIAN_POINT ( 'NONE',  ( 1.472469842513823179, 6.425597817667451750, 4.923371831947296329 ) ) ;
#19427 = EDGE_CURVE ( 'NONE', #74440, #39993, #36396, .T. ) ;
#19428 = DIRECTION ( 'NONE',  ( -1.000000000000000000, 0.000000000000000000, 0.000000000000000000 ) ) ;
#19429 = CARTESIAN_POINT ( 'NONE',  ( 19.42250999205614193, 45.14701867748817676, 5.440088680355555262 ) ) ;
#19430 = UNCERTAINTY_MEASURE_WITH_UNIT (LENGTH_MEASURE( 1.000000000000000082E-05 ), #27753, 'distance_accuracy_value', 'NONE');
#19431 = ADVANCED_FACE ( 'NONE', ( #97408 ), #12404, .F. ) ;
#19432 = AXIS2_PLACEMENT_3D ( 'NONE', #12874, #35384, #49889 ) ;
#19433 = CARTESIAN_POINT ( 'NONE',  ( 21.09922568453594849, 6.206968003263753531, 6.408140936763242479 ) ) ;
#19434 = CARTESIAN_POINT ( 'NONE',  ( 20.88017736071110875, 65.77201867748817676, -2.915334737309920765 ) ) ;
#19435 = EDGE_CURVE ( 'NONE', #38291, #3216, #405, .T. ) ;
#19436 = CARTESIAN_POINT ( 'NONE',  ( 5.076628168052703671, 31.84226448433412315, 8.527530157486179263 ) ) ;
#19437 = CARTESIAN_POINT ( 'NONE',  ( 16.40814093676323893, 50.79030133659708923, 11.09922568453595026 ) ) ;
#19439 = DIRECTION ( 'NONE',  ( 0.000000000000000000, 0.000000000000000000, -1.000000000000000000 ) ) ;
#19438 = CARTESIAN_POINT ( 'NONE',  ( 0.1532563361054083140, 1.008931151000784787, 1.131784320476157264E-15 ) ) ;
#19440 = ORIENTED_EDGE ( 'NONE', *, *, #41900, .F. ) ;
#19441 = CARTESIAN_POINT ( 'NONE',  ( 1.492507162822247491, 57.19955587570483146, -6.500000000000039080 ) ) ;
#19442 = CARTESIAN_POINT ( 'NONE',  ( -15.00000000000004974, 91.00000000000000000, -7.750000000000000000 ) ) ;
#19443 = CARTESIAN_POINT ( 'NONE',  ( 20.88017736071110875, 20.77201867748816611, -2.915334737309920765 ) ) ;
#19444 = CARTESIAN_POINT ( 'NONE',  ( 3.591859063236761518, 54.95696800326376064, 11.09922568453594849 ) ) ;
#19445 = CARTESIAN_POINT ( 'NONE',  ( 0.1532563361054082862, 36.21726448433410894, 2.638427012816831674 ) ) ;
#19446 = CARTESIAN_POINT ( 'NONE',  ( 0.5774900079438607392, 18.48035201082150536, 5.440088680355550821 ) ) ;
#19447 = CARTESIAN_POINT ( 'NONE',  ( -4.164238869374099927, 67.01208216824728936, 3.795296366450308767 ) ) ;
#19448 = ORIENTED_EDGE ( 'NONE', *, *, #44600, .F. ) ;
#19449 = CARTESIAN_POINT ( 'NONE',  ( -0.8801773607111009756, 8.063685344154837509, 1.068504757029289695E-15 ) ) ;
#19450 = CARTESIAN_POINT ( 'NONE',  ( 12.91533473730993009, 26.60535201082150536, -10.88017736071109987 ) ) ;
#19452 = CARTESIAN_POINT ( 'NONE',  ( 2.035157376598822676, 22.43868534415483396, -7.964842623401177768 ) ) ;
#19451 = CARTESIAN_POINT ( 'NONE',  ( 6.382347221874430154, 0.3640475087720987935, -13.57444820018227638 ) ) ;
#19453 = VECTOR ( 'NONE', #83520, 1000.000000000000000 ) ;
#19454 = ORIENTED_EDGE ( 'NONE', *, *, #70118, .T. ) ;
#19455 = CARTESIAN_POINT ( 'NONE',  ( 20.15039907845753575, 10.60158574516642460, -6.262539305110077059 ) ) ;
#19456 = CARTESIAN_POINT ( 'NONE',  ( 2.035157376598822676, 22.43868534415483396, -7.964842623401177768 ) ) ;
#19457 = CARTESIAN_POINT ( 'NONE',  ( 2.791683348922237240, 55.38393115100078745, -7.208316651077763204 ) ) ;
#19458 = CYLINDRICAL_SURFACE ( 'NONE', #88865, 0.5000000000000004441 ) ;
#19459 = CARTESIAN_POINT ( 'NONE',  ( 0.6178305044545818747, 63.49863466993043204, -9.382169495545419124 ) ) ;
#19460 = DIRECTION ( 'NONE',  ( -0.000000000000000000, -1.000000000000000000, -0.000000000000000000 ) ) ;
#19461 = CARTESIAN_POINT ( 'NONE',  ( 2.917880565312948704, 32.63708216824730357, 12.26659068614894643 ) ) ;
#19462 = CARTESIAN_POINT ( 'NONE',  ( 10.00000000000000178, 34.31368534415484106, 10.88017736071110342 ) ) ;
#19463 = CARTESIAN_POINT ( 'NONE',  ( -0.8801773607110991993, 22.85535201082150181, -2.915334737309923874 ) ) ;
#19464 = CARTESIAN_POINT ( 'NONE',  ( 20.15039907845753220, 42.62777174578613426, -6.262539305110077947 ) ) ;
#19465 = CARTESIAN_POINT ( 'NONE',  ( 17.39651004071842166, 32.93575266056827644, 6.499999999999998224 ) ) ;
#19466 = CARTESIAN_POINT ( 'NONE',  ( 7.361572987183169658, 44.96726448433412315, -9.846743663894592657 ) ) ;
#19467 = AXIS2_PLACEMENT_3D ( 'NONE', #91791, #68310, #77266 ) ;
#19468 = EDGE_CURVE ( 'NONE', #97173, #9609, #39889, .T. ) ;
#19469 = CARTESIAN_POINT ( 'NONE',  ( 19.84674366389459266, 23.71726448433412315, -2.638427012816827677 ) ) ;
#19470 = CARTESIAN_POINT ( 'NONE',  ( -5.204170427930421283E-15, -37.12636533006957507, -12.81628187352647608 ) ) ;
#19471 = CIRCLE ( 'NONE', #72126, 14.49999999999999822 ) ;
#19472 = CARTESIAN_POINT ( 'NONE',  ( 19.42250999205614548, 15.98035201082150714, -5.440088680355545492 ) ) ;
#19473 = CARTESIAN_POINT ( 'NONE',  ( 7.361572987183169658, 9.967264484334119601, -9.846743663894592657 ) ) ;
#19474 = CARTESIAN_POINT ( 'NONE',  ( 4.559911319644449179, 57.23035201082150536, -9.422509992056141925 ) ) ;
#19476 = CARTESIAN_POINT ( 'NONE',  ( 10.00000000000000178, 60.37363466993041783, 12.81628187352647608 ) ) ;
#19475 = CARTESIAN_POINT ( 'NONE',  ( 20.88017736071110164, 20.35535201082150891, 2.915334737309930979 ) ) ;
#19477 = CARTESIAN_POINT ( 'NONE',  ( 2.917880565312948704, 27.63708216824730357, 12.26659068614894643 ) ) ;
#19478 = ADVANCED_FACE ( 'NONE', ( #76367, #30857 ), #46360, .T. ) ;
#19479 = CARTESIAN_POINT ( 'NONE',  ( -2.816281873526471635, 58.91530133659707502, -3.434112377981056508 ) ) ;
#19480 = ORIENTED_EDGE ( 'NONE', *, *, #16628, .T. ) ;
#19481 = CARTESIAN_POINT ( 'NONE',  ( 10.00000000000000000, -2.126365330069579951, -12.81628187352647608 ) ) ;
#19482 = CARTESIAN_POINT ( 'NONE',  ( 1.274849032794324932, 32.55509018479936145, -6.500000000000021316 ) ) ;
#19483 = CARTESIAN_POINT ( 'NONE',  ( -0.8801773607110991993, 37.85535201082151247, -2.915334737309923874 ) ) ;
#19484 = CARTESIAN_POINT ( 'NONE',  ( 17.20831665107776587, 62.88393115100078745, 7.208316651077764980 ) ) ;
#19485 = ORIENTED_EDGE ( 'NONE', *, *, #4128, .F. ) ;
#19486 = CARTESIAN_POINT ( 'NONE',  ( 19.84674366389459266, 18.30059781766745175, 2.638427012816836559 ) ) ;
#19487 = CARTESIAN_POINT ( 'NONE',  ( 18.52753015748618282, 8.925597817667451750, -4.923371831947291888 ) ) ;
#19488 = CARTESIAN_POINT ( 'NONE',  ( 17.20831665107776587, 17.88393115100078745, 7.208316651077764980 ) ) ;
#19489 = CARTESIAN_POINT ( 'NONE',  ( 18.52753015748617571, 13.09226448433411960, 4.923371831947298993 ) ) ;
#19491 = DIRECTION ( 'NONE',  ( 8.673617379884028570E-16, 1.000000000000000000, 0.000000000000000000 ) ) ;
#19490 = CARTESIAN_POINT ( 'NONE',  ( 15.44008868035555260, 59.73035201082151247, 9.422509992056143702 ) ) ;
#19492 = CARTESIAN_POINT ( 'NONE',  ( 18.52753015748618282, 3.925597817667451306, -4.923371831947291888 ) ) ;
#19494 = EDGE_LOOP ( 'NONE', ( #25079, #555, #7107, #62245, #68213, #22526 ) ) ;
#19493 = CARTESIAN_POINT ( 'NONE',  ( 5.076628168052703671, 21.84226448433411960, 8.527530157486179263 ) ) ;
#19495 = AXIS2_PLACEMENT_3D ( 'NONE', #43278, #74257, #57783 ) ;
#19496 = DIRECTION ( 'NONE',  ( 0.8070303256584298035, -0.5905099943842175847, 0.000000000000000000 ) ) ;
#19497 = CARTESIAN_POINT ( 'NONE',  ( -1.099225684535947600, 3.706968003263753531, -6.408140936763238038 ) ) ;
#19498 = ORIENTED_EDGE ( 'NONE', *, *, #75080, .F. ) ;
#19499 = EDGE_LOOP ( 'NONE', ( #86516, #85166, #5674, #34565 ) ) ;
#19500 = CARTESIAN_POINT ( 'NONE',  ( 10.00000000000000178, 4.313685344154837509, 10.88017736071110342 ) ) ;
#19501 = CARTESIAN_POINT ( 'NONE',  ( 6.204703633549690345, 15.76208216824730179, -14.16423886937410259 ) ) ;
#19502 = UNCERTAINTY_MEASURE_WITH_UNIT (LENGTH_MEASURE( 1.000000000000000082E-05 ), #89351, 'distance_accuracy_value', 'NONE');
#19503 = DIRECTION ( 'NONE',  ( 0.8241261886220166977, 0.000000000000000000, 0.5664062369248314965 ) ) ;
#19504 = CARTESIAN_POINT ( 'NONE',  ( 22.26659068614895176, 19.72041550158063572, -7.082119434687042414 ) ) ;
#19505 = CARTESIAN_POINT ( 'NONE',  ( 17.08211943468705130, 28.47041550158063572, 12.26659068614894998 ) ) ;
#19506 = EDGE_CURVE ( 'NONE', #28808, #23105, #67383, .T. ) ;
#19507 = SURFACE_STYLE_FILL_AREA ( #80509 ) ;
#19508 = CARTESIAN_POINT ( 'NONE',  ( 2.917880565312950480, 0.9704155015806342766, -12.26659068614894821 ) ) ;
#19509 = CARTESIAN_POINT ( 'NONE',  ( -0.8801773607111008646, 33.27201867748817676, 2.915334737309923430 ) ) ;
#19510 = LINE ( 'NONE', #95511, #37183 ) ;
#19511 = ORIENTED_EDGE ( 'NONE', *, *, #66083, .T. ) ;
#19512 = CARTESIAN_POINT ( 'NONE',  ( 19.84674366389459266, 18.71726448433411960, -2.638427012816827677 ) ) ;
#19514 = CARTESIAN_POINT ( 'NONE',  ( 1.472469842513823179, 10.59226448433411782, -4.923371831947296329 ) ) ;
#19513 = CARTESIAN_POINT ( 'NONE',  ( 15.44008868035555793, 61.39701867748817676, -9.422509992056140149 ) ) ;
#19515 = CARTESIAN_POINT ( 'NONE',  ( 7.084665262690076126, 12.02201867748817321, -10.88017736071110164 ) ) ;
#19516 = CARTESIAN_POINT ( 'NONE',  ( 22.81628187352647785, 51.62363466993042493, 6.195893100308588602E-16 ) ) ;
#19517 = CARTESIAN_POINT ( 'NONE',  ( 10.00000000000000000, 54.75893115100078745, -9.846743663894594434 ) ) ;
#19518 = EDGE_CURVE ( 'NONE', #72221, #73524, #30155, .T. ) ;
#19519 = CARTESIAN_POINT ( 'NONE',  ( 0.4195498155886330238, 0.5000000000000023315, 9.500000000000000000 ) ) ;
#19520 = CARTESIAN_POINT ( 'NONE',  ( 0.6178305044545818747, 23.49863466993041783, -9.382169495545419124 ) ) ;
#19521 = CARTESIAN_POINT ( 'NONE',  ( 7.082119434687047743, -34.86291783175269643, -12.26659068614894821 ) ) ;
#19522 = VECTOR ( 'NONE', #55772, 1000.000000000000000 ) ;
#19523 = CARTESIAN_POINT ( 'NONE',  ( 19.84674366389459266, 43.30059781766744464, 2.638427012816836559 ) ) ;
#19524 = CARTESIAN_POINT ( 'NONE',  ( 20.36894250292379382, 8.678748834913967869, 10.36894250292379205 ) ) ;
#19525 = ORIENTED_EDGE ( 'NONE', *, *, #76871, .T. ) ;
#19526 = CARTESIAN_POINT ( 'NONE',  ( 14.99999999999997868, 80.07179676972448590, -6.250000000000000000 ) ) ;
#19527 = CARTESIAN_POINT ( 'NONE',  ( 15.44008868035555793, 46.39701867748817676, -9.422509992056140149 ) ) ;
#19528 = CARTESIAN_POINT ( 'NONE',  ( 0.5774900079438607392, 58.48035201082151247, 5.440088680355550821 ) ) ;
#19529 = CARTESIAN_POINT ( 'NONE',  ( 13.79529636645031943, 50.34541550158064638, -14.16423886937409904 ) ) ;
#19530 = CARTESIAN_POINT ( 'NONE',  ( 10.00000000000000178, 52.25893115100078745, 9.846743663894594434 ) ) ;
#19531 = STYLED_ITEM ( 'NONE', ( #48735 ), #47653 ) ;
#19532 = CARTESIAN_POINT ( 'NONE',  ( 0.6178305044545838731, 64.74863466993043914, 9.382169495545420901 ) ) ;
#19533 = CARTESIAN_POINT ( 'NONE',  ( 17.96484262340118221, 46.18868534415484106, -7.964842623401177768 ) ) ;
#19534 = CARTESIAN_POINT ( 'NONE',  ( -5.559536763064314435, -36.09058695999160449, -2.500000000000000444 ) ) ;
#19535 = CARTESIAN_POINT ( 'NONE',  ( 10.00000000000000000, 54.75893115100078745, -9.846743663894594434 ) ) ;
#19536 = CARTESIAN_POINT ( 'NONE',  ( 2.915334737309928315, 19.52201867748817676, 10.88017736071109987 ) ) ;
#19537 = AXIS2_PLACEMENT_3D ( 'NONE', #7505, #37996, #69464 ) ;
#19538 = CARTESIAN_POINT ( 'NONE',  ( 19.72487221294570858, 11.86607318730075633, 6.500000000000000888 ) ) ;
#19539 = DIRECTION ( 'NONE',  ( -0.000000000000000000, -0.000000000000000000, -1.000000000000000000 ) ) ;
#19540 = CARTESIAN_POINT ( 'NONE',  ( 17.35999999999999943, 37.99999999999997868, 10.00000000000000000 ) ) ;
#19541 = COLOUR_RGB ( '', 0.72549020, 0.75294118, 0.79215686) ;
#19542 = CARTESIAN_POINT ( 'NONE',  ( 18.52753015748617571, 3.092264484334118269, 4.923371831947298993 ) ) ;
#19543 = CARTESIAN_POINT ( 'NONE',  ( 2.035157376598822676, 67.43868534415484817, -7.964842623401177768 ) ) ;
#19544 = CARTESIAN_POINT ( 'NONE',  ( 17.99999999999999645, 78.24875198621546701, -3.965855704038845353 ) ) ;
#19545 = EDGE_CURVE ( 'NONE', #21360, #83033, #20608, .T. ) ;
#19546 = CARTESIAN_POINT ( 'NONE',  ( 1.472469842513823179, 40.59226448433411605, -4.923371831947296329 ) ) ;
#19547 = CARTESIAN_POINT ( 'NONE',  ( 15.44008868035555793, 26.39701867748817321, -9.422509992056140149 ) ) ;
#19548 = EDGE_CURVE ( 'NONE', #68154, #57109, #62383, .T. ) ;
#19549 = CARTESIAN_POINT ( 'NONE',  ( 13.43411237798105340, 5.581968003263753531, 12.81628187352647963 ) ) ;
#19551 = CARTESIAN_POINT ( 'NONE',  ( 17.39651004071841101, 37.93575266056827644, 6.500000000000005329 ) ) ;
#19550 = CARTESIAN_POINT ( 'NONE',  ( 15.44008868035555260, 29.73035201082150891, 9.422509992056143702 ) ) ;
#19552 = CARTESIAN_POINT ( 'NONE',  ( 10.00000000000000000, 32.87363466993042493, -12.81628187352647608 ) ) ;
#19553 = ORIENTED_EDGE ( 'NONE', *, *, #50727, .T. ) ;
#19554 = CARTESIAN_POINT ( 'NONE',  ( 15.44008868035555260, 49.73035201082150536, 9.422509992056143702 ) ) ;
#19556 = DIRECTION ( 'NONE',  ( 0.000000000000000000, 0.000000000000000000, 1.000000000000000000 ) ) ;
#19555 = CARTESIAN_POINT ( 'NONE',  ( 6.565887622018943937, 20.16530133659708213, 12.81628187352647430 ) ) ;
#19557 = CARTESIAN_POINT ( 'NONE',  ( 20.32896413005680003, 31.77164270246084143, 5.963430220938287007 ) ) ;
#19558 = CARTESIAN_POINT ( 'NONE',  ( 4.559911319644449179, 32.23035201082150536, -9.422509992056141925 ) ) ;
#19559 = CARTESIAN_POINT ( 'NONE',  ( -2.266590686148945544, 67.22041550158063217, 7.082119434687048631 ) ) ;
#19560 = AXIS2_PLACEMENT_3D ( 'NONE', #90433, #37964, #52451 ) ;
#19561 = CARTESIAN_POINT ( 'NONE',  ( 0.1532563361054083140, 56.00893115100078745, 1.131784320476157264E-15 ) ) ;
#19562 = CARTESIAN_POINT ( 'NONE',  ( 0.1532563361054082862, 1.217264484334117824, 2.638427012816831674 ) ) ;
#19563 = CARTESIAN_POINT ( 'NONE',  ( 20.88017736071110519, 65.56368534415483396, 2.639326808657452039E-16 ) ) ;
#19564 = CARTESIAN_POINT ( 'NONE',  ( -6.767445849361333643, 15.00000000000000000, 13.38662304974491946 ) ) ;
#19565 = CARTESIAN_POINT ( 'NONE',  ( 17.08211943468705130, 28.47041550158063572, 12.26659068614894998 ) ) ;
#19566 = DIRECTION ( 'NONE',  ( 1.000000000000000000, 0.000000000000000000, 0.000000000000000000 ) ) ;
#19567 = ORIENTED_EDGE ( 'NONE', *, *, #61050, .T. ) ;
#19568 = EDGE_LOOP ( 'NONE', ( #29354, #8551, #5699, #66300 ) ) ;
#19569 = CARTESIAN_POINT ( 'NONE',  ( 24.16423886937410614, 54.30374883491396787, 8.672049930838204340E-16 ) ) ;
#19570 = CARTESIAN_POINT ( 'NONE',  ( 20.36894250292379738, 49.92874883491396787, -10.36894250292379027 ) ) ;
#19571 = CARTESIAN_POINT ( 'NONE',  ( 14.92337183194729633, 22.67559781766745175, 8.527530157486181039 ) ) ;
#19572 = CARTESIAN_POINT ( 'NONE',  ( 21.09922568453594849, 26.20696800326375353, 6.408140936763242479 ) ) ;
#19573 = CARTESIAN_POINT ( 'NONE',  ( -13.57315748652532506, 90.98139137973063839, 7.967914335234096868 ) ) ;
#19574 = PLANE ( 'NONE',  #29080 ) ;
#19575 = CARTESIAN_POINT ( 'NONE',  ( 0.5774900079438607392, 68.48035201082150536, 5.440088680355550821 ) ) ;
#19576 = CARTESIAN_POINT ( 'NONE',  ( 22.26659068614895176, 49.72041550158063927, -7.082119434687042414 ) ) ;
#19577 = EDGE_CURVE ( 'NONE', #89199, #14221, #95768, .T. ) ;
#19578 = DIRECTION ( 'NONE',  ( -1.000000000000000000, 0.000000000000000000, -0.000000000000000000 ) ) ;
#19579 = CARTESIAN_POINT ( 'NONE',  ( 17.20831665107776587, 9.133931151000787452, -7.208316651077762316 ) ) ;
#19580 = EDGE_CURVE ( 'NONE', #14459, #88316, #19108, .T. ) ;
#19581 = CARTESIAN_POINT ( 'NONE',  ( -8.527530157486182816, 0.5922644843341234866, -4.923371831947288335 ) ) ;
#19582 = ORIENTED_EDGE ( 'NONE', *, *, #24899, .T. ) ;
#19583 = VERTEX_POINT ( 'NONE', #38374 ) ;
#19584 = CARTESIAN_POINT ( 'NONE',  ( 0.000000000000000000, 1.823139558123437975, -11.92686044187656513 ) ) ;
#19585 = EDGE_LOOP ( 'NONE', ( #17280, #98562, #40593, #62034 ) ) ;
#19587 = CARTESIAN_POINT ( 'NONE',  ( 19.42250999205614548, 20.98035201082150891, -5.440088680355545492 ) ) ;
#19586 = CARTESIAN_POINT ( 'NONE',  ( 10.00000000000000178, 24.31368534415484106, 10.88017736071110342 ) ) ;
#19589 = CARTESIAN_POINT ( 'NONE',  ( -2.816281873526473856, 19.12363466993042138, 9.499525473075851096E-16 ) ) ;
#19588 = CARTESIAN_POINT ( 'NONE',  ( 19.84674366389459621, 48.50893115100078745, 7.409399052514197653E-17 ) ) ;
#19590 = FACE_OUTER_BOUND ( 'NONE', #84488, .T. ) ;
#19591 = VECTOR ( 'NONE', #81400, 1000.000000000000000 ) ;
#19592 = CARTESIAN_POINT ( 'NONE',  ( -2.816281873526471635, 23.91530133659708568, -3.434112377981056508 ) ) ;
#19593 = ORIENTED_EDGE ( 'NONE', *, *, #62664, .T. ) ;
#19594 = AXIS2_PLACEMENT_3D ( 'NONE', #63015, #2551, #39053 ) ;
#19595 = CARTESIAN_POINT ( 'NONE',  ( 5.076628168052704559, 25.17559781766745175, -8.527530157486179263 ) ) ;
#19596 = STYLED_ITEM ( 'NONE', ( #58858 ), #49361 ) ;
#19597 = CARTESIAN_POINT ( 'NONE',  ( 2.917880565312948704, 62.63708216824730357, 12.26659068614894643 ) ) ;
#19598 = EDGE_LOOP ( 'NONE', ( #36662, #83501, #7692, #56089 ) ) ;
#19599 = VECTOR ( 'NONE', #53910, 999.9999999999998863 ) ;
#19600 = CARTESIAN_POINT ( 'NONE',  ( 2.035157376598824452, 8.688685344154839285, 7.964842623401179544 ) ) ;
#19601 = ORIENTED_EDGE ( 'NONE', *, *, #6682, .T. ) ;
#19602 = CARTESIAN_POINT ( 'NONE',  ( 19.42250999205614548, 35.98035201082151247, -5.440088680355545492 ) ) ;
#19603 = CARTESIAN_POINT ( 'NONE',  ( 12.91533473730993009, 51.60535201082149825, -10.88017736071109987 ) ) ;
#19604 = CARTESIAN_POINT ( 'NONE',  ( 19.42250999205614193, 55.14701867748817676, 5.440088680355555262 ) ) ;
#19605 = DIRECTION ( 'NONE',  ( -0.000000000000000000, 0.000000000000000000, 1.000000000000000000 ) ) ;
#19606 = CARTESIAN_POINT ( 'NONE',  ( 17.96484262340118221, 44.93868534415483396, 7.964842623401181321 ) ) ;
#19607 = CARTESIAN_POINT ( 'NONE',  ( 1.354709868695624264, 0.3640475087720588809, -14.93870011653152297 ) ) ;
#19608 = CARTESIAN_POINT ( 'NONE',  ( 6.599999999999995204, -97.00000000000000000, 4.000000000000000000 ) ) ;
#19609 = CARTESIAN_POINT ( 'NONE',  ( 5.076628168052703671, 11.84226448433411960, 8.527530157486179263 ) ) ;
#19610 = ORIENTED_EDGE ( 'NONE', *, *, #77114, .T. ) ;
#19611 = CARTESIAN_POINT ( 'NONE',  ( 10.93144397341777641, -92.98246991214814727, 4.000000000000000000 ) ) ;
#19612 = CARTESIAN_POINT ( 'NONE',  ( 18.52753015748617571, 63.09226448433412315, 4.923371831947298993 ) ) ;
#19613 = CARTESIAN_POINT ( 'NONE',  ( 0.1129803114748865051, 24.29427333184091964, -6.480634945678684922 ) ) ;
#19614 = CARTESIAN_POINT ( 'NONE',  ( -7.118731320094870973, -71.92838106472885329, 2.750000000000000000 ) ) ;
#19615 = ORIENTED_EDGE ( 'NONE', *, *, #70722, .T. ) ;
#19616 = FACE_OUTER_BOUND ( 'NONE', #34703, .T. ) ;
#19617 = CARTESIAN_POINT ( 'NONE',  ( -6.982525766850297799, -88.11956318484570261, 3.750000000000000000 ) ) ;
#19619 = CARTESIAN_POINT ( 'NONE',  ( 2.791683348922240793, 31.63393115100078745, 7.208316651077764092 ) ) ;
#19618 = CARTESIAN_POINT ( 'NONE',  ( 2.791683348922240793, 66.63393115100079456, 7.208316651077764092 ) ) ;
#19620 = CARTESIAN_POINT ( 'NONE',  ( -4.164238869374098151, 56.59541550158063927, -3.795296366450310543 ) ) ;
#19621 = CARTESIAN_POINT ( 'NONE',  ( 12.25993886608601890, 14.63606888159244512, 8.642563219313739609 ) ) ;
#19622 = ORIENTED_EDGE ( 'NONE', *, *, #66533, .F. ) ;
#19623 = CARTESIAN_POINT ( 'NONE',  ( 0.000000000000000000, 15.00000000000000000, 0.000000000000000000 ) ) ;
#19624 = CARTESIAN_POINT ( 'NONE',  ( 0.1532563361054082862, 26.21726448433411605, 2.638427012816831674 ) ) ;
#19625 = CARTESIAN_POINT ( 'NONE',  ( 6.565887622018943937, 60.16530133659707502, 12.81628187352647430 ) ) ;
#19627 = AXIS2_PLACEMENT_3D ( 'NONE', #24220, #85208, #16711 ) ;
#19626 = CARTESIAN_POINT ( 'NONE',  ( 0.6178305044545818747, 3.498634669930420049, -9.382169495545419124 ) ) ;
#19628 = CARTESIAN_POINT ( 'NONE',  ( 1.472469842513823179, 6.425597817667451750, 4.923371831947296329 ) ) ;
#19629 = EDGE_CURVE ( 'NONE', #15586, #78552, #7881, .T. ) ;
#19630 = CARTESIAN_POINT ( 'NONE',  ( -10.14667048435128294, 15.00000000000000000, -10.35833375027054082 ) ) ;
#19631 = CARTESIAN_POINT ( 'NONE',  ( 2.791683348922240793, 6.633931151000785675, 7.208316651077764092 ) ) ;
#19632 = CARTESIAN_POINT ( 'NONE',  ( 17.20831665107776587, 64.13393115100079456, -7.208316651077762316 ) ) ;
#19633 = CARTESIAN_POINT ( 'NONE',  ( 19.42250999205614193, 20.14701867748817321, 5.440088680355555262 ) ) ;
#19634 = VECTOR ( 'NONE', #94244, 1000.000000000000000 ) ;
#19635 = ORIENTED_EDGE ( 'NONE', *, *, #51144, .T. ) ;
#19636 = CARTESIAN_POINT ( 'NONE',  ( -0.8801773607110991993, 12.85535201082150358, -2.915334737309923874 ) ) ;
#19637 = CARTESIAN_POINT ( 'NONE',  ( 24.16423886937410614, 9.303748834913967869, 8.672049930838204340E-16 ) ) ;
#19638 = CARTESIAN_POINT ( 'NONE',  ( 5.076628168052703671, 16.84226448433411960, 8.527530157486179263 ) ) ;
#19639 = CARTESIAN_POINT ( 'NONE',  ( 2.035157376598822676, 42.43868534415483396, -7.964842623401177768 ) ) ;
#19641 = CARTESIAN_POINT ( 'NONE',  ( 11.27492930200523880, 12.64336083852433035, -1.672692125565626631 ) ) ;
#19640 = CARTESIAN_POINT ( 'NONE',  ( 13.43411237798105340, 30.58196800326374998, 12.81628187352647963 ) ) ;
#19642 = FILL_AREA_STYLE ('',( #27131 ) ) ;
#19643 = CARTESIAN_POINT ( 'NONE',  ( 20.15039907845753220, 17.62777174578612716, -6.262539305110077947 ) ) ;
#19644 = DIRECTION ( 'NONE',  ( 0.000000000000000000, 0.000000000000000000, 1.000000000000000000 ) ) ;
#19645 = CARTESIAN_POINT ( 'NONE',  ( 10.00000000000000178, 0.3736346699304200492, 12.81628187352647608 ) ) ;
#19646 = CARTESIAN_POINT ( 'NONE',  ( 18.52753015748618282, 58.92559781766745886, -4.923371831947291888 ) ) ;
#19647 = CARTESIAN_POINT ( 'NONE',  ( 17.20831665107776587, 9.133931151000787452, -7.208316651077762316 ) ) ;
#19648 = CARTESIAN_POINT ( 'NONE',  ( 10.88017736071110519, -19.43631465584515894, -2.602085213965210642E-15 ) ) ;
#19649 = CARTESIAN_POINT ( 'NONE',  ( 3.591859063236761518, 19.95696800326375353, 11.09922568453594849 ) ) ;
#19650 = CARTESIAN_POINT ( 'NONE',  ( 14.99847009497945116, 0.3640475087720986824, -0.2142307401080281448 ) ) ;
#19651 = CARTESIAN_POINT ( 'NONE',  ( 20.88017736071110164, 20.35535201082150891, 2.915334737309930979 ) ) ;
#19652 = CARTESIAN_POINT ( 'NONE',  ( 3.969999999999999751, 9.750000000000000000, 4.000000000000000000 ) ) ;
#19653 = CARTESIAN_POINT ( 'NONE',  ( -4.164238869374099039, 51.80374883491396787, 8.674139862899312516E-16 ) ) ;
#19654 = CARTESIAN_POINT ( 'NONE',  ( 6.829574850505127692, -88.00372650098204019, -3.749999999999998668 ) ) ;
#19655 = VECTOR ( 'NONE', #4808, 1000.000000000000000 ) ;
#19656 = CARTESIAN_POINT ( 'NONE',  ( 13.43411237798106583, 32.66530133659708213, -12.81628187352647252 ) ) ;
#19657 = CARTESIAN_POINT ( 'NONE',  ( 7.084665262690076126, 32.02201867748816966, -10.88017736071110164 ) ) ;
#19658 = CARTESIAN_POINT ( 'NONE',  ( 10.00000000000000000, 49.75893115100078745, -9.846743663894594434 ) ) ;
#19659 = EDGE_CURVE ( 'NONE', #15178, #37810, #47865, .T. ) ;
#19660 = CARTESIAN_POINT ( 'NONE',  ( 20.88017736071110875, 55.77201867748816966, -2.915334737309920765 ) ) ;
#19661 = CARTESIAN_POINT ( 'NONE',  ( 19.38216949554541202, 0.9986346699304200492, 9.382169495545424454 ) ) ;
#19662 = CARTESIAN_POINT ( 'NONE',  ( -0.3689425029237881626, 32.42874883491395366, 10.36894250292379027 ) ) ;
#19663 = DIRECTION ( 'NONE',  ( -0.000000000000000000, 1.000000000000000000, -0.000000000000000000 ) ) ;
#19664 = CIRCLE ( 'NONE', #88330, 3.699999999999999289 ) ;
#19665 = EDGE_CURVE ( 'NONE', #42611, #67453, #68383, .T. ) ;
#19666 = CARTESIAN_POINT ( 'NONE',  ( 19.84674366389459266, 18.30059781766745175, 2.638427012816836559 ) ) ;
#19667 = CARTESIAN_POINT ( 'NONE',  ( -1.099225684535947600, 64.54030133659709634, 6.408140936763237150 ) ) ;
#19668 = CARTESIAN_POINT ( 'NONE',  ( 13.43411237798105340, 0.5819680032637533085, 12.81628187352647963 ) ) ;
#19669 = VERTEX_POINT ( 'NONE', #90862 ) ;
#19670 = VECTOR ( 'NONE', #15129, 1000.000000000000000 ) ;
#19671 = CARTESIAN_POINT ( 'NONE',  ( 20.10384461210893647, 11.74302437010793554, 6.337995344473741355 ) ) ;
#19672 = CARTESIAN_POINT ( 'NONE',  ( 19.42250999205614193, 15.14701867748817143, 5.440088680355555262 ) ) ;
#19673 = CARTESIAN_POINT ( 'NONE',  ( 17.08211943468705130, 18.47041550158063572, 12.26659068614894998 ) ) ;
#19674 = CARTESIAN_POINT ( 'NONE',  ( 12.63842701281683922, 14.55059781766744997, -9.846743663894590881 ) ) ;
#19675 = CARTESIAN_POINT ( 'NONE',  ( 14.92337183194729988, 44.34226448433412315, -8.527530157486177487 ) ) ;
#19676 = CARTESIAN_POINT ( 'NONE',  ( 0.5774900079438590739, 27.64701867748817676, -5.440088680355550821 ) ) ;
#19677 = TOROIDAL_SURFACE ( 'NONE', #11686, 0.5000000000000000000, 0.2500000000000000000 ) ;
#19678 = CARTESIAN_POINT ( 'NONE',  ( 19.72487221294570858, 12.80223176428831167, -6.500000000000000888 ) ) ;
#19679 = DIRECTION ( 'NONE',  ( 0.000000000000000000, 0.000000000000000000, 1.000000000000000000 ) ) ;
#19680 = ORIENTED_EDGE ( 'NONE', *, *, #3312, .F. ) ;
#19681 = SURFACE_STYLE_USAGE ( .BOTH. , #35161 ) ;
#19682 = CARTESIAN_POINT ( 'NONE',  ( 10.00000000000000178, 52.25893115100078745, 9.846743663894594434 ) ) ;
#19683 = ORIENTED_EDGE ( 'NONE', *, *, #82536, .F. ) ;
#19684 = VERTEX_POINT ( 'NONE', #37892 ) ;
#19685 = LINE ( 'NONE', #3715, #42154 ) ;
#19686 = CARTESIAN_POINT ( 'NONE',  ( 24.16423886937410614, 14.30374883491396787, 8.672049930838204340E-16 ) ) ;
#19687 = CARTESIAN_POINT ( 'NONE',  ( -0.3689425029237898834, 6.178748834913968757, -10.36894250292378850 ) ) ;
#19688 = CARTESIAN_POINT ( 'NONE',  ( 20.88017736071110164, 40.35535201082150536, 2.915334737309930979 ) ) ;
#19689 = CARTESIAN_POINT ( 'NONE',  ( -2.266590686148945544, 61.38708216824730357, -7.082119434687050408 ) ) ;
#19690 = CARTESIAN_POINT ( 'NONE',  ( 14.92337183194729988, 54.34226448433412315, -8.527530157486177487 ) ) ;
#19691 = CARTESIAN_POINT ( 'NONE',  ( 17.20831665107776587, 32.88393115100078745, 7.208316651077764980 ) ) ;
#19692 = CARTESIAN_POINT ( 'NONE',  ( -10.77730536144846774, -98.63085534186637915, 4.000000000000001776 ) ) ;
#19694 = CARTESIAN_POINT ( 'NONE',  ( -2.816281873526473856, 4.123634669930420493, 9.499525473075851096E-16 ) ) ;
#19693 = CARTESIAN_POINT ( 'NONE',  ( 10.00000000000000178, 39.31368534415484106, 10.88017736071110342 ) ) ;
#19695 = CARTESIAN_POINT ( 'NONE',  ( 17.08211943468705840, 5.137082168247300906, -12.26659068614894466 ) ) ;
#19696 = CARTESIAN_POINT ( 'NONE',  ( 10.00000000000000178, 53.05374883491396787, 14.16423886937410082 ) ) ;
#19697 = CARTESIAN_POINT ( 'NONE',  ( 19.42250999205614193, 10.14701867748816966, 5.440088680355555262 ) ) ;
#19698 = CARTESIAN_POINT ( 'NONE',  ( -1.926860441876563801, 67.66212336850780673, 1.004413902775740978E-15 ) ) ;
#19699 = DIRECTION ( 'NONE',  ( 0.000000000000000000, -0.000000000000000000, -1.000000000000000000 ) ) ;
#19700 = CARTESIAN_POINT ( 'NONE',  ( -14.94699059465108881, 14.49999999999999112, 1.259949270174695268 ) ) ;
#19701 = ORIENTED_EDGE ( 'NONE', *, *, #58687, .F. ) ;
#19702 =( LENGTH_UNIT ( ) NAMED_UNIT ( * ) SI_UNIT ( .MILLI., .METRE. ) );
#19703 = ORIENTED_EDGE ( 'NONE', *, *, #48173, .T. ) ;
#19704 = ORIENTED_EDGE ( 'NONE', *, *, #93727, .T. ) ;
#19705 = CARTESIAN_POINT ( 'NONE',  ( 22.26659068614895176, 34.72041550158063927, -7.082119434687042414 ) ) ;
#19706 = CARTESIAN_POINT ( 'NONE',  ( 1.472469842513823179, 31.42559781766745530, 4.923371831947296329 ) ) ;
#19707 = CARTESIAN_POINT ( 'NONE',  ( 12.91533473730992121, 59.52201867748816966, 10.88017736071110164 ) ) ;
#19708 = EDGE_CURVE ( 'NONE', #88687, #21472, #94250, .T. ) ;
#19709 = FACE_OUTER_BOUND ( 'NONE', #8760, .T. ) ;
#19710 = CARTESIAN_POINT ( 'NONE',  ( 19.42250999205614193, 55.14701867748817676, 5.440088680355555262 ) ) ;
#19711 = AXIS2_PLACEMENT_3D ( 'NONE', #62394, #14966, #92415 ) ;
#19712 = CARTESIAN_POINT ( 'NONE',  ( 21.09922568453594849, 61.20696800326376064, 6.408140936763242479 ) ) ;
#19713 = CARTESIAN_POINT ( 'NONE',  ( -5.204170427930421283E-15, 7.873634669930427599, -12.81628187352647608 ) ) ;
#19714 = ORIENTED_EDGE ( 'NONE', *, *, #16542, .F. ) ;
#19715 = CARTESIAN_POINT ( 'NONE',  ( 17.08211943468705840, 15.13708216824730179, -12.26659068614894466 ) ) ;
#19716 = VERTEX_POINT ( 'NONE', #60862 ) ;
#19717 = CARTESIAN_POINT ( 'NONE',  ( -1.099225684535947600, 43.70696800326375353, -6.408140936763238038 ) ) ;
#19718 = CARTESIAN_POINT ( 'NONE',  ( 18.52753015748618282, 23.92559781766745530, -4.923371831947291888 ) ) ;
#19719 = CARTESIAN_POINT ( 'NONE',  ( 15.44008868035555793, 11.39701867748817143, -9.422509992056140149 ) ) ;
#19720 = CARTESIAN_POINT ( 'NONE',  ( 21.09922568453594849, 51.20696800326375353, 6.408140936763242479 ) ) ;
#19721 = DIRECTION ( 'NONE',  ( -0.000000000000000000, -0.000000000000000000, -1.000000000000000000 ) ) ;
#19722 = CARTESIAN_POINT ( 'NONE',  ( 10.00000000000000178, 37.25893115100078745, 9.846743663894594434 ) ) ;
#19724 = ORIENTED_EDGE ( 'NONE', *, *, #46856, .T. ) ;
#19723 = CARTESIAN_POINT ( 'NONE',  ( -12.67122524790595506, 14.95077488074853456, 7.555537761805664942 ) ) ;
#19725 = ORIENTED_EDGE ( 'NONE', *, *, #74833, .T. ) ;
#19726 = CARTESIAN_POINT ( 'NONE',  ( 14.26139399674454822, 15.00000000000000000, -2.619664342929791445 ) ) ;
#19727 = AXIS2_PLACEMENT_3D ( 'NONE', #29366, #96916, #35886 ) ;
#19728 = CARTESIAN_POINT ( 'NONE',  ( 8.629999999999995453, 40.99999999999999289, -6.500000000000000888 ) ) ;
#19729 = PLANE ( 'NONE',  #22867 ) ;
#19730 = CARTESIAN_POINT ( 'NONE',  ( -0.2418659066527639179, 44.26028685723174050, -6.114288769123057854 ) ) ;
#19731 = CARTESIAN_POINT ( 'NONE',  ( 7.361572987183170547, 22.05059781766745530, 9.846743663894590881 ) ) ;
#19732 = CARTESIAN_POINT ( 'NONE',  ( 21.09922568453595559, 22.04030133659708923, -6.408140936763230044 ) ) ;
#19734 = DIRECTION ( 'NONE',  ( 1.000000000000000000, 0.000000000000000000, 0.000000000000000000 ) ) ;
#19733 = AXIS2_PLACEMENT_3D ( 'NONE', #10467, #9980, #17973 ) ;
#19735 = CARTESIAN_POINT ( 'NONE',  ( 2.791683348922240793, 46.63393115100077324, 7.208316651077764092 ) ) ;
#19736 = CARTESIAN_POINT ( 'NONE',  ( 18.29284471827481084, 5.401890803972852595, -6.499999999999990230 ) ) ;
#19737 = CARTESIAN_POINT ( 'NONE',  ( 22.26659068614895176, 19.72041550158063572, -7.082119434687042414 ) ) ;
#19738 = CARTESIAN_POINT ( 'NONE',  ( 19.84674366389459621, 28.50893115100078745, 7.409399052514197653E-17 ) ) ;
#19739 = CARTESIAN_POINT ( 'NONE',  ( 16.40814093676324603, 27.45696800326375708, -11.09922568453594671 ) ) ;
#19741 = CARTESIAN_POINT ( 'NONE',  ( -14.17193700899791153, 15.00000000000000000, 1.489530601563921808 ) ) ;
#19740 = CARTESIAN_POINT ( 'NONE',  ( 34.56412365047463453, 26.99999999999999645, 10.00000000000000000 ) ) ;
#19742 = CARTESIAN_POINT ( 'NONE',  ( 4.559911319644449179, 57.23035201082150536, -9.422509992056141925 ) ) ;
#19743 = CARTESIAN_POINT ( 'NONE',  ( 21.09922568453594849, 6.206968003263753531, 6.408140936763242479 ) ) ;
#19744 = DIRECTION ( 'NONE',  ( 0.000000000000000000, 0.000000000000000000, 1.000000000000000000 ) ) ;
#19745 = CARTESIAN_POINT ( 'NONE',  ( 2.791683348922240793, 36.63393115100078035, 7.208316651077764092 ) ) ;
#19746 = CARTESIAN_POINT ( 'NONE',  ( 20.88017736071110519, 25.56368534415483751, 2.639326808657452039E-16 ) ) ;
#19747 = EDGE_CURVE ( 'NONE', #83096, #25751, #47933, .T. ) ;
#19748 = CARTESIAN_POINT ( 'NONE',  ( 22.81628187352648496, 31.83196800326375353, -3.434112377981050290 ) ) ;
#19749 = CARTESIAN_POINT ( 'NONE',  ( 12.63842701281683922, 34.55059781766745886, -9.846743663894590881 ) ) ;
#19750 = DIRECTION ( 'NONE',  ( 0.2920631208464244399, 0.8487660001727230785, 0.4407895307198710366 ) ) ;
#19751 = DIRECTION ( 'NONE',  ( 0.000000000000000000, 1.000000000000000000, 0.000000000000000000 ) ) ;
#19752 = CARTESIAN_POINT ( 'NONE',  ( 0.5774900079438590739, 27.64701867748817676, -5.440088680355550821 ) ) ;
#19753 = ORIENTED_EDGE ( 'NONE', *, *, #32943, .T. ) ;
#19754 = CARTESIAN_POINT ( 'NONE',  ( -3.014428414850124138, 3.963468844518203138, 11.25000000000000178 ) ) ;
#19755 =( LENGTH_UNIT ( ) NAMED_UNIT ( * ) SI_UNIT ( .MILLI., .METRE. ) );
#19757 = CARTESIAN_POINT ( 'NONE',  ( 12.91533473730993009, 31.60535201082150891, -10.88017736071109987 ) ) ;
#19756 = CARTESIAN_POINT ( 'NONE',  ( 1.472469842513823179, 56.42559781766745886, 4.923371831947296329 ) ) ;
#19758 = DIRECTION ( 'NONE',  ( 1.000000000000000000, 0.000000000000000000, 0.000000000000000000 ) ) ;
#19759 = CARTESIAN_POINT ( 'NONE',  ( 19.42250999205614548, 65.98035201082151957, -5.440088680355545492 ) ) ;
#19761 = LINE ( 'NONE', #80761, #49524 ) ;
#19760 = CARTESIAN_POINT ( 'NONE',  ( 2.035157376598822676, 27.43868534415483396, -7.964842623401177768 ) ) ;
#19762 = CARTESIAN_POINT ( 'NONE',  ( 2.791683348922240793, 6.633931151000785675, 7.208316651077764092 ) ) ;
#19763 = CARTESIAN_POINT ( 'NONE',  ( 10.00000000000000178, 52.25893115100078745, 9.846743663894594434 ) ) ;
#19765 = CARTESIAN_POINT ( 'NONE',  ( 6.829574850505126804, -88.00372650098204019, 3.750000000000001332 ) ) ;
#19764 = CARTESIAN_POINT ( 'NONE',  ( 20.36894250292379382, 58.67874883491396076, 10.36894250292379205 ) ) ;
#19766 = CARTESIAN_POINT ( 'NONE',  ( 10.00000000000000000, 15.55374883491396787, -14.16423886937410082 ) ) ;
#19767 = CARTESIAN_POINT ( 'NONE',  ( -4.164238869374099927, 42.01208216824728936, 3.795296366450308767 ) ) ;
#19768 = CARTESIAN_POINT ( 'NONE',  ( -2.816281873526473856, 4.123634669930420493, 9.499525473075851096E-16 ) ) ;
#19769 = CARTESIAN_POINT ( 'NONE',  ( -7.079957095331153916, -69.52918543726779887, 2.749999999999999112 ) ) ;
#19770 = EDGE_CURVE ( 'NONE', #30654, #83990, #52376, .T. ) ;
#19771 = CARTESIAN_POINT ( 'NONE',  ( 17.96484262340118221, 11.18868534415484106, -7.964842623401177768 ) ) ;
#19772 = CARTESIAN_POINT ( 'NONE',  ( 2.791683348922240793, 41.63393115100078745, 7.208316651077764092 ) ) ;
#19773 = CARTESIAN_POINT ( 'NONE',  ( 0.000000000000000000, 0.5000000000000004441, 0.000000000000000000 ) ) ;
#19774 = CARTESIAN_POINT ( 'NONE',  ( 19.42250999205614193, 60.14701867748817676, 5.440088680355555262 ) ) ;
#19775 = CARTESIAN_POINT ( 'NONE',  ( 11.17717139118532010, 2.266418178063696498, 2.895237119026786043 ) ) ;
#19776 = CARTESIAN_POINT ( 'NONE',  ( 22.81628187352647785, 56.41530133659708213, 3.434112377981063169 ) ) ;
#19777 = CARTESIAN_POINT ( 'NONE',  ( 21.09922568453594849, 26.20696800326375353, 6.408140936763242479 ) ) ;
#19778 = CARTESIAN_POINT ( 'NONE',  ( 14.92337183194729988, 24.34226448433411960, -8.527530157486177487 ) ) ;
#19780 = VERTEX_POINT ( 'NONE', #56327 ) ;
#19779 = EDGE_CURVE ( 'NONE', #34423, #42615, #12272, .T. ) ;
#19781 = CARTESIAN_POINT ( 'NONE',  ( 4.559911319644449179, 2.230352010821504916, -9.422509992056141925 ) ) ;
#19782 = CARTESIAN_POINT ( 'NONE',  ( -0.8801773607111008646, 18.27201867748817321, 2.915334737309923430 ) ) ;
#19783 = CARTESIAN_POINT ( 'NONE',  ( -2.266590686148945544, 47.22041550158063927, 7.082119434687048631 ) ) ;
#19784 = CARTESIAN_POINT ( 'NONE',  ( 7.084665262690076126, 34.10535201082151247, 10.88017736071109987 ) ) ;
#19785 = CARTESIAN_POINT ( 'NONE',  ( -0.8801773607110991993, 57.85535201082149825, -2.915334737309923874 ) ) ;
#19786 = CARTESIAN_POINT ( 'NONE',  ( -0.9082943533608713871, 15.00000000000000000, -14.47152380946376660 ) ) ;
#19787 = CARTESIAN_POINT ( 'NONE',  ( 10.85665724878298377, -52.68265776536580347, -4.000000000000000888 ) ) ;
#19788 = CARTESIAN_POINT ( 'NONE',  ( 17.20831665107776587, 7.883931151000784787, 7.208316651077764980 ) ) ;
#19789 = FACE_OUTER_BOUND ( 'NONE', #49113, .T. ) ;
#19790 = CARTESIAN_POINT ( 'NONE',  ( 0.1532563361054082862, 6.217264484334118713, 2.638427012816831674 ) ) ;
#19791 = CARTESIAN_POINT ( 'NONE',  ( 19.72487221294570858, 0.000000000000000000, -6.500000000000000888 ) ) ;
#19792 = CARTESIAN_POINT ( 'NONE',  ( 17.20831665107776587, 44.13393115100078745, -7.208316651077762316 ) ) ;
#19793 = CARTESIAN_POINT ( 'NONE',  ( 5.076628168052703671, 66.84226448433412315, 8.527530157486179263 ) ) ;
#19794 = CARTESIAN_POINT ( 'NONE',  ( 4.559911319644449179, 23.89701867748817321, 9.422509992056141925 ) ) ;
#19795 = ORIENTED_EDGE ( 'NONE', *, *, #35308, .T. ) ;
#19796 = CARTESIAN_POINT ( 'NONE',  ( 19.38216949554541202, 40.99863466993042493, 9.382169495545424454 ) ) ;
#19797 = LINE ( 'NONE', #4815, #41258 ) ;
#19798 = VECTOR ( 'NONE', #83144, 1000.000000000000000 ) ;
#19799 = CARTESIAN_POINT ( 'NONE',  ( 19.42250999205614548, 60.98035201082151247, -5.440088680355545492 ) ) ;
#19800 = CARTESIAN_POINT ( 'NONE',  ( 21.09922568453594849, 41.20696800326375353, 6.408140936763242479 ) ) ;
#19802 = CARTESIAN_POINT ( 'NONE',  ( 5.076628168052703671, 16.84226448433411960, 8.527530157486179263 ) ) ;
#19801 = CARTESIAN_POINT ( 'NONE',  ( 24.16423886937410614, 54.51208216824730357, -3.795296366450302550 ) ) ;
#19803 = DIRECTION ( 'NONE',  ( 1.000000000000000000, 0.000000000000000000, 0.000000000000000000 ) ) ;
#19804 = CARTESIAN_POINT ( 'NONE',  ( 0.000000000000000000, 15.00000000000000000, 0.000000000000000000 ) ) ;
#19805 = CARTESIAN_POINT ( 'NONE',  ( -4.164238869374099039, 16.80374883491396787, 8.674139862899312516E-16 ) ) ;
#19806 = CARTESIAN_POINT ( 'NONE',  ( 24.16423886937409904, 29.09541550158063572, 3.795296366450317205 ) ) ;
#19807 = CARTESIAN_POINT ( 'NONE',  ( 14.92337183194729633, 47.67559781766745175, 8.527530157486181039 ) ) ;
#19808 = CARTESIAN_POINT ( 'NONE',  ( 18.06765999051786054, 8.991275129254484355, 6.499999999999990230 ) ) ;
#19809 = CARTESIAN_POINT ( 'NONE',  ( 15.44008868035555793, 21.39701867748817321, -9.422509992056140149 ) ) ;
#19810 = AXIS2_PLACEMENT_3D ( 'NONE', #43620, #28124, #58624 ) ;
#19811 = CARTESIAN_POINT ( 'NONE',  ( 20.88017736071110164, 65.35535201082150536, 2.915334737309930979 ) ) ;
#19812 = CARTESIAN_POINT ( 'NONE',  ( 0.1532563361054083140, 56.00893115100078745, 1.131784320476157264E-15 ) ) ;
#19813 = EDGE_LOOP ( 'NONE', ( #28331, #58590, #13561, #20299 ) ) ;
#19814 = CARTESIAN_POINT ( 'NONE',  ( 22.81628187352647785, 46.41530133659708213, 3.434112377981063169 ) ) ;
#19815 = CARTESIAN_POINT ( 'NONE',  ( 15.44008868035555793, 51.39701867748816966, -9.422509992056140149 ) ) ;
#19816 = ORIENTED_EDGE ( 'NONE', *, *, #49456, .F. ) ;
#19817 = DIRECTION ( 'NONE',  ( 0.5150380749100554878, 0.000000000000000000, -0.8571673007021115565 ) ) ;
#19818 = ADVANCED_FACE ( 'NONE', ( #2360 ), #78323, .T. ) ;
#19819 = CARTESIAN_POINT ( 'NONE',  ( 49.67841921735763577, 67.89383959705537563, -8.000000000000000000 ) ) ;
#19820 = ORIENTED_EDGE ( 'NONE', *, *, #24624, .F. ) ;
#19821 = CARTESIAN_POINT ( 'NONE',  ( 10.00000000000000178, 64.31368534415483396, 10.88017736071110342 ) ) ;
#19822 = CARTESIAN_POINT ( 'NONE',  ( 10.00000000000000178, 14.31368534415483751, 10.88017736071110342 ) ) ;
#19823 = CARTESIAN_POINT ( 'NONE',  ( -5.419894505350704605, 14.63606864255126538, 13.98659156302458229 ) ) ;
#19824 = DIRECTION ( 'NONE',  ( 1.000000000000000000, 1.759564384940674839E-15, 0.000000000000000000 ) ) ;
#19825 = CARTESIAN_POINT ( 'NONE',  ( 17.96484262340118221, 9.938685344154839285, 7.964842623401181321 ) ) ;
#19826 = CARTESIAN_POINT ( 'NONE',  ( 7.361572987183169658, 24.96726448433412315, -9.846743663894592657 ) ) ;
#19827 = CARTESIAN_POINT ( 'NONE',  ( 20.36894250292379738, 19.92874883491396787, -10.36894250292379027 ) ) ;
#19828 = CARTESIAN_POINT ( 'NONE',  ( 2.035157376598824452, 18.68868534415484106, 7.964842623401179544 ) ) ;
#19829 = CARTESIAN_POINT ( 'NONE',  ( 2.791683348922237240, 65.38393115100078035, -7.208316651077763204 ) ) ;
#19830 = ORIENTED_EDGE ( 'NONE', *, *, #57231, .F. ) ;
#19831 = ADVANCED_FACE ( 'NONE', ( #63312 ), #93329, .F. ) ;
#19832 = CARTESIAN_POINT ( 'NONE',  ( 5.076628168052703671, 56.84226448433412315, 8.527530157486179263 ) ) ;
#19833 = ORIENTED_EDGE ( 'NONE', *, *, #92478, .T. ) ;
#19834 = CARTESIAN_POINT ( 'NONE',  ( 20.88017736071110519, 55.56368534415484817, 2.639326808657452039E-16 ) ) ;
#19835 = CARTESIAN_POINT ( 'NONE',  ( 0.1532563361054083140, 66.00893115100079456, 1.131784320476157264E-15 ) ) ;
#19836 = CARTESIAN_POINT ( 'NONE',  ( 10.00000000000000000, 42.87363466993042493, -12.81628187352647608 ) ) ;
#19838 = CARTESIAN_POINT ( 'NONE',  ( 10.93781366033340063, 15.00000000000000000, 10.26470809774072634 ) ) ;
#19837 = CARTESIAN_POINT ( 'NONE',  ( 7.084665262690076126, 4.105352010821503583, 10.88017736071109987 ) ) ;
#19839 = CARTESIAN_POINT ( 'NONE',  ( 2.035157376598824452, 53.68868534415484817, 7.964842623401179544 ) ) ;
#19840 = CARTESIAN_POINT ( 'NONE',  ( 20.88017736071110519, 15.56368534415483751, 2.639326808657452039E-16 ) ) ;
#19841 = SHAPE_REPRESENTATION ( '1.2 Movable Jaw', ( #27931 ), #40723 ) ;
#19842 = CARTESIAN_POINT ( 'NONE',  ( -1.099225684535947600, 44.54030133659708923, 6.408140936763237150 ) ) ;
#19843 = CARTESIAN_POINT ( 'NONE',  ( -0.8801773607111009756, 28.06368534415484106, 1.068504757029289695E-15 ) ) ;
#19844 = DIRECTION ( 'NONE',  ( 0.1822355254921578793, 0.000000000000000000, -0.9832549075639526182 ) ) ;
#19845 = CARTESIAN_POINT ( 'NONE',  ( -1.099225684535947600, 38.70696800326375353, -6.408140936763238038 ) ) ;
#19846 = CARTESIAN_POINT ( 'NONE',  ( 19.42250999205614193, 35.14701867748816966, 5.440088680355555262 ) ) ;
#19847 = CARTESIAN_POINT ( 'NONE',  ( 19.84674366389459621, 58.50893115100078745, 7.409399052514197653E-17 ) ) ;
#19848 = ORIENTED_EDGE ( 'NONE', *, *, #32622, .T. ) ;
#19849 = CARTESIAN_POINT ( 'NONE',  ( 0.000000000000000000, 15.00000000000000000, 0.000000000000000000 ) ) ;
#19850 = CARTESIAN_POINT ( 'NONE',  ( 7.361572987183169658, 59.96726448433410894, -9.846743663894592657 ) ) ;
#19852 = CARTESIAN_POINT ( 'NONE',  ( 12.63842701281683034, 52.46726448433413026, 9.846743663894596210 ) ) ;
#19851 = CARTESIAN_POINT ( 'NONE',  ( -13.80105244024794331, 90.89655890636515778, -7.750000000004162892 ) ) ;
#19853 = CARTESIAN_POINT ( 'NONE',  ( 0.5774900079438590739, 22.64701867748817321, -5.440088680355550821 ) ) ;
#19854 = DIRECTION ( 'NONE',  ( -0.000000000000000000, 0.000000000000000000, 1.000000000000000000 ) ) ;
#19855 = CARTESIAN_POINT ( 'NONE',  ( 0.1955144967549090895, 39.32703681773340776, -6.500000000002870593 ) ) ;
#19856 = CARTESIAN_POINT ( 'NONE',  ( -7.313705784284680433, 15.00000000000000000, 13.09617149020738935 ) ) ;
#19858 = CARTESIAN_POINT ( 'NONE',  ( 14.92337183194729988, 4.342264484334117824, -8.527530157486177487 ) ) ;
#19857 = CARTESIAN_POINT ( 'NONE',  ( 12.63842701281683034, 42.46726448433412315, 9.846743663894596210 ) ) ;
#19859 = CARTESIAN_POINT ( 'NONE',  ( 18.52753015748617571, 28.09226448433411960, 4.923371831947298993 ) ) ;
#19860 = ADVANCED_FACE ( 'NONE', ( #78823 ), #56803, .T. ) ;
#19862 = VERTEX_POINT ( 'NONE', #71332 ) ;
#19861 = CARTESIAN_POINT ( 'NONE',  ( 12.63842701281683922, 64.55059781766745175, -9.846743663894590881 ) ) ;
#19863 = CARTESIAN_POINT ( 'NONE',  ( 21.09922568453595559, 37.04030133659708923, -6.408140936763230044 ) ) ;
#19864 = CARTESIAN_POINT ( 'NONE',  ( 10.00000000000000000, 39.75893115100078745, -9.846743663894594434 ) ) ;
#19865 = AXIS2_PLACEMENT_3D ( 'NONE', #51471, #74959, #81960 ) ;
#19866 = CARTESIAN_POINT ( 'NONE',  ( 1.274849032794294290, 58.57228050351032778, 6.499999999999979572 ) ) ;
#19868 = ADVANCED_FACE ( 'NONE', ( #18819 ), #94305, .T. ) ;
#19867 = CARTESIAN_POINT ( 'NONE',  ( 6.204703633549690345, 57.84541550158063927, 14.16423886937410082 ) ) ;
#19869 = CARTESIAN_POINT ( 'NONE',  ( 0.1532563361054083140, 26.00893115100078745, 1.131784320476157264E-15 ) ) ;
#19870 = AXIS2_PLACEMENT_3D ( 'NONE', #1477, #84954, #1969 ) ;
#19871 = VERTEX_POINT ( 'NONE', #3319 ) ;
#19872 = VECTOR ( 'NONE', #6126, 1000.000000000000000 ) ;
#19873 = CARTESIAN_POINT ( 'NONE',  ( 22.26659068614895176, 59.72041550158063927, -7.082119434687042414 ) ) ;
#19874 = CARTESIAN_POINT ( 'NONE',  ( 12.50534872682730914, 15.00000000000000000, -7.339363270777500503 ) ) ;
#19875 = CARTESIAN_POINT ( 'NONE',  ( 20.88017736071110164, 15.35535201082150358, 2.915334737309930979 ) ) ;
#19876 = CARTESIAN_POINT ( 'NONE',  ( 24.16423886937410614, 34.51208216824731068, -3.795296366450302550 ) ) ;
#19877 = CARTESIAN_POINT ( 'NONE',  ( 22.26659068614895176, 49.72041550158063927, -7.082119434687042414 ) ) ;
#19878 = DIRECTION ( 'NONE',  ( 0.000000000000000000, 0.000000000000000000, 1.000000000000000000 ) ) ;
#19879 = AXIS2_PLACEMENT_3D ( 'NONE', #88735, #34240, #19751 ) ;
#19880 = CARTESIAN_POINT ( 'NONE',  ( 19.84674366389459621, 13.50893115100078568, 7.409399052514197653E-17 ) ) ;
#19881 = ADVANCED_FACE ( 'NONE', ( #33782, #16853 ), #64289, .F. ) ;
#19883 = CARTESIAN_POINT ( 'NONE',  ( 18.52753015748618282, 63.92559781766745886, -4.923371831947291888 ) ) ;
#19882 = CARTESIAN_POINT ( 'NONE',  ( 15.00000000000000000, 11.00000000000000000, 6.500000000000000888 ) ) ;
#19884 = ORIENTED_EDGE ( 'NONE', *, *, #77005, .F. ) ;
#19885 = CARTESIAN_POINT ( 'NONE',  ( 20.88017736071110164, 45.35535201082149115, 2.915334737309930979 ) ) ;
#19886 = CARTESIAN_POINT ( 'NONE',  ( 0.8952175423694853640, 17.60160829253886305, -5.990408912944323205 ) ) ;
#19887 = CARTESIAN_POINT ( 'NONE',  ( 10.00000000000000000, 49.75893115100078745, -9.846743663894594434 ) ) ;
#19888 = DIRECTION ( 'NONE',  ( -0.7445673648800779088, 0.6675473310227050261, 0.000000000000000000 ) ) ;
#19889 = CARTESIAN_POINT ( 'NONE',  ( 0.1532563361054082862, 56.21726448433411605, 2.638427012816831674 ) ) ;
#19890 = CARTESIAN_POINT ( 'NONE',  ( 13.79529636645030344, 3.262082168247301350, 14.16423886937410614 ) ) ;
#19891 = CIRCLE ( 'NONE', #51877, 0.5000000000000004441 ) ;
#19892 = CARTESIAN_POINT ( 'NONE',  ( -4.164238869374099927, 27.01208216824730357, 3.795296366450308767 ) ) ;
#19893 = CARTESIAN_POINT ( 'NONE',  ( 1.274849032794292736, 37.55509018479936145, -6.499999999999977796 ) ) ;
#19895 = CARTESIAN_POINT ( 'NONE',  ( -9.159723438033276821, 15.00000000000000000, 10.91613331444536250 ) ) ;
#19894 = CARTESIAN_POINT ( 'NONE',  ( -7.116252256210342964, -80.68108970088772480, -2.499999999998790745 ) ) ;
#19896 = CARTESIAN_POINT ( 'NONE',  ( 17.96484262340118221, 16.18868534415483396, -7.964842623401177768 ) ) ;
#19897 = CARTESIAN_POINT ( 'NONE',  ( -2.816281873526473856, 44.12363466993042493, 9.499525473075851096E-16 ) ) ;
#19898 =( BOUNDED_CURVE ( )  B_SPLINE_CURVE ( 2, ( #11894, #72873, #4408, #73367, #4894, #88875, #30825, #75841, #84824 ),
 .UNSPECIFIED., .F., .F. ) 
 B_SPLINE_CURVE_WITH_KNOTS ( ( 3, 2, 2, 2, 3 ),
 ( 0.04628608864975117254, 0.04761904761904761640, 0.05357142857142856845, 0.05952380952380952051, 0.06085676849310609621 ),
 .UNSPECIFIED. ) 
 CURVE ( )  GEOMETRIC_REPRESENTATION_ITEM ( )  RATIONAL_B_SPLINE_CURVE ( ( 0.9881565478350731180, 0.9923695281211489805, 1.000000000000000000, 0.9659258262890683122, 1.000000000000000000, 0.9659258262890683122, 1.000000000000000000, 0.9923695281211482033, 0.9881565478350724518 ) ) 
 REPRESENTATION_ITEM ( '' )  );
#19899 = CARTESIAN_POINT ( 'NONE',  ( -7.003840667633538963, 15.00000000000000888, -12.84073839985662779 ) ) ;
#19900 = CARTESIAN_POINT ( 'NONE',  ( 5.076628168052704559, 5.175597817667451750, -8.527530157486179263 ) ) ;
#19901 = CARTESIAN_POINT ( 'NONE',  ( -4.862001128006231632, 15.00000000000000000, -13.66056166603291189 ) ) ;
#19903 = EDGE_CURVE ( 'NONE', #75285, #59946, #69857, .T. ) ;
#19902 = VERTEX_POINT ( 'NONE', #39362 ) ;
#19904 = CARTESIAN_POINT ( 'NONE',  ( 6.910361961633475936, -84.29457034760254430, -3.750000000000000000 ) ) ;
#19905 = CARTESIAN_POINT ( 'NONE',  ( -2.266590686148945544, 31.38708216824730002, -7.082119434687050408 ) ) ;
#19906 = CARTESIAN_POINT ( 'NONE',  ( 2.917880565312948704, 2.637082168247300906, 12.26659068614894643 ) ) ;
#19907 = DIRECTION ( 'NONE',  ( 0.000000000000000000, 1.000000000000000000, 0.000000000000000000 ) ) ;
#19908 = CARTESIAN_POINT ( 'NONE',  ( 2.035157376598822676, 12.43868534415483751, -7.964842623401177768 ) ) ;
#19909 = FACE_OUTER_BOUND ( 'NONE', #62254, .T. ) ;
#19910 = CARTESIAN_POINT ( 'NONE',  ( -14.99847009497944406, 0.5000000000000004441, -0.2142307401082361173 ) ) ;
#19911 = CARTESIAN_POINT ( 'NONE',  ( 4.559911319644449179, 33.89701867748817676, 9.422509992056141925 ) ) ;
#19912 = CARTESIAN_POINT ( 'NONE',  ( 20.88017736071110875, 55.77201867748816966, -2.915334737309920765 ) ) ;
#19913 = CARTESIAN_POINT ( 'NONE',  ( 0.6178305044545838731, 19.74863466993042138, 9.382169495545420901 ) ) ;
#19914 = CARTESIAN_POINT ( 'NONE',  ( 17.20831665107776587, 62.88393115100078745, 7.208316651077764980 ) ) ;
#19915 = CARTESIAN_POINT ( 'NONE',  ( 0.000000000000000000, 15.00000000000000000, 0.000000000000000000 ) ) ;
#19916 = CARTESIAN_POINT ( 'NONE',  ( 0.1532563361054100626, 20.80059781766744464, -2.638427012816831230 ) ) ;
#19917 = SURFACE_STYLE_USAGE ( .BOTH. , #57904 ) ;
#19918 = AXIS2_PLACEMENT_3D ( 'NONE', #32718, #63216, #46265 ) ;
#19919 = CARTESIAN_POINT ( 'NONE',  ( 20.88017736071110164, 50.35535201082151247, 2.915334737309930979 ) ) ;
#19920 = CARTESIAN_POINT ( 'NONE',  ( 3.591859063236763294, 3.290301336597087012, -11.09922568453595026 ) ) ;
#19921 = CARTESIAN_POINT ( 'NONE',  ( 12.91533473730993009, 66.60535201082150536, -10.88017736071109987 ) ) ;
#19922 = CARTESIAN_POINT ( 'NONE',  ( 0.1532563361054100626, 20.80059781766744464, -2.638427012816831230 ) ) ;
#19923 = CARTESIAN_POINT ( 'NONE',  ( 10.00000000000000178, 50.37363466993042493, 12.81628187352647608 ) ) ;
#19924 = CARTESIAN_POINT ( 'NONE',  ( 14.92337183194729988, 9.342264484334119601, -8.527530157486177487 ) ) ;
#19925 = ORIENTED_EDGE ( 'NONE', *, *, #63790, .T. ) ;
#19926 = DIRECTION ( 'NONE',  ( -0.000000000000000000, -1.000000000000000000, -0.000000000000000000 ) ) ;
#19927 = CARTESIAN_POINT ( 'NONE',  ( 19.72487221294570858, 70.00000000000000000, -6.000000000000000000 ) ) ;
#19928 = CARTESIAN_POINT ( 'NONE',  ( 19.42250999205614548, 20.98035201082150891, -5.440088680355545492 ) ) ;
#19929 = CARTESIAN_POINT ( 'NONE',  ( 3.591859063236761518, 64.95696800326376774, 11.09922568453594849 ) ) ;
#19930 = CARTESIAN_POINT ( 'NONE',  ( 7.361572987183170547, 27.05059781766745175, 9.846743663894590881 ) ) ;
#19931 = CARTESIAN_POINT ( 'NONE',  ( 10.00000000000000178, 14.31368534415483751, 10.88017736071110342 ) ) ;
#19932 = CARTESIAN_POINT ( 'NONE',  ( 17.96484262340118221, 4.938685344154837509, 7.964842623401181321 ) ) ;
#19933 = VERTEX_POINT ( 'NONE', #1868 ) ;
#19934 = CARTESIAN_POINT ( 'NONE',  ( 12.91533473730993009, 11.60535201082150536, -10.88017736071109987 ) ) ;
#19935 = EDGE_CURVE ( 'NONE', #1450, #41967, #65936, .T. ) ;
#19936 = CARTESIAN_POINT ( 'NONE',  ( 2.035157376598824452, 33.68868534415484106, 7.964842623401179544 ) ) ;
#19938 = CARTESIAN_POINT ( 'NONE',  ( 15.44008868035555793, 41.39701867748817676, -9.422509992056140149 ) ) ;
#19937 = CARTESIAN_POINT ( 'NONE',  ( -13.59943737456451629, 0.04922511925147186190, -5.718514076973049143 ) ) ;
#19939 = ORIENTED_EDGE ( 'NONE', *, *, #63217, .T. ) ;
#19940 = CARTESIAN_POINT ( 'NONE',  ( 20.32896413005680358, 9.745456701841137104, 5.963430220938287007 ) ) ;
#19941 = CARTESIAN_POINT ( 'NONE',  ( 15.44008868035555260, 29.73035201082150891, 9.422509992056143702 ) ) ;
#19942 = CARTESIAN_POINT ( 'NONE',  ( 7.361572987183169658, 64.96726448433412315, -9.846743663894592657 ) ) ;
#19943 =( NAMED_UNIT ( * ) SI_UNIT ( $, .STERADIAN. ) SOLID_ANGLE_UNIT ( ) );
#19944 = CARTESIAN_POINT ( 'NONE',  ( -0.3289641300568005855, 5.104976035794174472, 5.963430220938281678 ) ) ;
#19945 = CARTESIAN_POINT ( 'NONE',  ( 2.917880565312950480, 35.97041550158063217, -12.26659068614894821 ) ) ;
#19946 = CARTESIAN_POINT ( 'NONE',  ( 0.5774900079438607392, 33.48035201082150536, 5.440088680355550821 ) ) ;
#19947 = CARTESIAN_POINT ( 'NONE',  ( 0.5774900079438607392, 33.48035201082150536, 5.440088680355550821 ) ) ;
#19948 = CARTESIAN_POINT ( 'NONE',  ( 7.361572987183169658, 64.96726448433412315, -9.846743663894592657 ) ) ;
#19949 = AXIS2_PLACEMENT_3D ( 'NONE', #60810, #84808, #92303 ) ;
#19950 = LINE ( 'NONE', #67427, #82830 ) ;
#19951 = CARTESIAN_POINT ( 'NONE',  ( 0.1532563361054083140, 46.00893115100079456, 1.131784320476157264E-15 ) ) ;
#19952 = CARTESIAN_POINT ( 'NONE',  ( 0.000000000000000000, 91.00000000000000000, 8.000000000000000000 ) ) ;
#19953 = CARTESIAN_POINT ( 'NONE',  ( 10.00000000000000000, 19.75893115100078390, -9.846743663894594434 ) ) ;
#19954 = CARTESIAN_POINT ( 'NONE',  ( -12.81628187352647608, -35.87636533006957507, 3.903127820947815962E-15 ) ) ;
#19955 = CARTESIAN_POINT ( 'NONE',  ( 10.00000000000000178, 14.31368534415483751, 10.88017736071110342 ) ) ;
#19956 = CARTESIAN_POINT ( 'NONE',  ( 17.20831665107776587, 22.88393115100078745, 7.208316651077764980 ) ) ;
#19958 = CARTESIAN_POINT ( 'NONE',  ( 12.91533473730992121, 49.52201867748817676, 10.88017736071110164 ) ) ;
#19957 = CARTESIAN_POINT ( 'NONE',  ( 10.00000000000000178, 64.31368534415483396, 10.88017736071110342 ) ) ;
#19960 = CARTESIAN_POINT ( 'NONE',  ( -2.816281873526473856, 64.12363466993042493, 9.499525473075851096E-16 ) ) ;
#19959 = CARTESIAN_POINT ( 'NONE',  ( -0.8801773607111009756, 23.06368534415484106, 1.068504757029289695E-15 ) ) ;
#19961 = CARTESIAN_POINT ( 'NONE',  ( -0.3689425029237898834, 31.17874883491396787, -10.36894250292378850 ) ) ;
#19962 = VECTOR ( 'NONE', #47199, 1000.000000000000000 ) ;
#19963 = CARTESIAN_POINT ( 'NONE',  ( 2.962741594153077251, 15.00000000000000000, -13.93860331045673107 ) ) ;
#19964 = VERTEX_POINT ( 'NONE', #55332 ) ;
#19965 = CARTESIAN_POINT ( 'NONE',  ( 21.09922568453595559, 7.040301336597086568, -6.408140936763230044 ) ) ;
#19966 = SURFACE_STYLE_FILL_AREA ( #88464 ) ;
#19967 = CARTESIAN_POINT ( 'NONE',  ( 12.91533473730993009, 31.60535201082150891, -10.88017736071109987 ) ) ;
#19968 = CARTESIAN_POINT ( 'NONE',  ( 12.63842701281683034, 62.46726448433410894, 9.846743663894596210 ) ) ;
#19969 = ORIENTED_EDGE ( 'NONE', *, *, #37042, .F. ) ;
#19970 = CARTESIAN_POINT ( 'NONE',  ( 0.1532563361054082862, 16.21726448433411960, 2.638427012816831674 ) ) ;
#19971 = CARTESIAN_POINT ( 'NONE',  ( 5.076628168052704559, 15.17559781766745175, -8.527530157486179263 ) ) ;
#19972 = CARTESIAN_POINT ( 'NONE',  ( 12.63842701281683922, 19.55059781766745175, -9.846743663894590881 ) ) ;
#19973 = ADVANCED_FACE ( 'NONE', ( #85840 ), #17353, .F. ) ;
#19974 = CARTESIAN_POINT ( 'NONE',  ( 7.361572987183170547, 17.05059781766745530, 9.846743663894590881 ) ) ;
#19975 =( LENGTH_UNIT ( ) NAMED_UNIT ( * ) SI_UNIT ( .MILLI., .METRE. ) );
#19976 = CIRCLE ( 'NONE', #88634, 0.2500000000000024980 ) ;
#19977 = DIRECTION ( 'NONE',  ( 0.000000000000000000, 0.000000000000000000, 1.000000000000000000 ) ) ;
#19979 = FACE_OUTER_BOUND ( 'NONE', #54215, .T. ) ;
#19978 = CARTESIAN_POINT ( 'NONE',  ( 2.791683348922237240, 0.3839311510007847872, -7.208316651077763204 ) ) ;
#19980 = CARTESIAN_POINT ( 'NONE',  ( 0.1532563361054083140, 1.008931151000784787, 1.131784320476157264E-15 ) ) ;
#19982 = EDGE_LOOP ( 'NONE', ( #11441, #2252, #73810, #27571 ) ) ;
#19981 = CARTESIAN_POINT ( 'NONE',  ( 1.472469842513823179, 25.59226448433412315, -4.923371831947296329 ) ) ;
#19983 = EDGE_CURVE ( 'NONE', #64886, #17335, #89413, .T. ) ;
#19984 = FACE_OUTER_BOUND ( 'NONE', #47251, .T. ) ;
#19985 = CARTESIAN_POINT ( 'NONE',  ( 16.40814093676323893, 0.7903013365970867898, 11.09922568453595026 ) ) ;
#19986 = ORIENTED_EDGE ( 'NONE', *, *, #98245, .T. ) ;
#19987 = CARTESIAN_POINT ( 'NONE',  ( 15.44008868035555260, 4.730352010821504471, 9.422509992056143702 ) ) ;
#19988 = EDGE_CURVE ( 'NONE', #18712, #44298, #64777, .T. ) ;
#19990 = EDGE_CURVE ( 'NONE', #42327, #62224, #37454, .T. ) ;
#19989 = CARTESIAN_POINT ( 'NONE',  ( 10.00000000000000000, 20.55374883491396787, -14.16423886937410082 ) ) ;
#19991 = CARTESIAN_POINT ( 'NONE',  ( 22.26659068614894466, 18.88708216824730002, 7.082119434687054849 ) ) ;
#19992 = CARTESIAN_POINT ( 'NONE',  ( 20.36894250292379382, 38.67874883491396076, 10.36894250292379205 ) ) ;
#19994 = CARTESIAN_POINT ( 'NONE',  ( 0.5774900079438607392, 68.48035201082150536, 5.440088680355550821 ) ) ;
#19993 = CARTESIAN_POINT ( 'NONE',  ( 20.36894250292379382, 18.67874883491397142, 10.36894250292379205 ) ) ;
#19995 = CARTESIAN_POINT ( 'NONE',  ( 4.559911319644449179, 28.89701867748817321, 9.422509992056141925 ) ) ;
#19996 = CARTESIAN_POINT ( 'NONE',  ( -5.419894505350674407, 0.5000000000000004441, 13.98659156302455031 ) ) ;
#19997 = PRESENTATION_LAYER_ASSIGNMENT (  '', '', ( #27985 ) ) ;
#19998 = CARTESIAN_POINT ( 'NONE',  ( 10.00000000000000178, 12.25893115100078568, 9.846743663894594434 ) ) ;
#19999 = AXIS2_PLACEMENT_3D ( 'NONE', #31771, #7818, #38313 ) ;
#20001 = CARTESIAN_POINT ( 'NONE',  ( 12.63842701281683922, 34.55059781766745886, -9.846743663894590881 ) ) ;
#20000 = CARTESIAN_POINT ( 'NONE',  ( -0.8801773607111009756, 53.06368534415484106, 1.068504757029289695E-15 ) ) ;
#20002 = ADVANCED_FACE ( 'NONE', ( #95801 ), #4802, .F. ) ;
#20003 = CARTESIAN_POINT ( 'NONE',  ( 19.42250999205614548, 15.98035201082150714, -5.440088680355545492 ) ) ;
#20004 = CARTESIAN_POINT ( 'NONE',  ( -1.099225684535947600, 39.54030133659708923, 6.408140936763237150 ) ) ;
#20005 = CARTESIAN_POINT ( 'NONE',  ( 2.791683348922240793, 56.63393115100078035, 7.208316651077764092 ) ) ;
#20006 = DIRECTION ( 'NONE',  ( -0.000000000000000000, -0.000000000000000000, -1.000000000000000000 ) ) ;
#20007 = CARTESIAN_POINT ( 'NONE',  ( 3.591859063236763294, 48.29030133659708923, -11.09922568453595026 ) ) ;
#20008 = CARTESIAN_POINT ( 'NONE',  ( -10.36894250292379205, -28.82125116508602503, -10.36894250292378672 ) ) ;
#20009 = CARTESIAN_POINT ( 'NONE',  ( 0.1532563361054082862, 41.21726448433411605, 2.638427012816831674 ) ) ;
#20010 = CARTESIAN_POINT ( 'NONE',  ( 17.08211943468705840, 25.13708216824730357, -12.26659068614894466 ) ) ;
#20011 = ORIENTED_EDGE ( 'NONE', *, *, #11527, .F. ) ;
#20012 = CARTESIAN_POINT ( 'NONE',  ( -3.843542995449753530, 0.2301500725087323451, 14.43777707752876438 ) ) ;
#20013 = COLOUR_RGB ( '', 0.09019608, 0.27058824, 0.51372549) ;
#20014 = CARTESIAN_POINT ( 'NONE',  ( 2.035157376598822676, 52.43868534415483396, -7.964842623401177768 ) ) ;
#20015 = CARTESIAN_POINT ( 'NONE',  ( 0.5774900079438607392, 53.48035201082151247, 5.440088680355550821 ) ) ;
#20016 = CARTESIAN_POINT ( 'NONE',  ( 22.26659068614894466, 48.88708216824730357, 7.082119434687054849 ) ) ;
#20017 = CARTESIAN_POINT ( 'NONE',  ( 0.1532563361054083140, 66.00893115100079456, 1.131784320476157264E-15 ) ) ;
#20018 = CARTESIAN_POINT ( 'NONE',  ( 19.38216949554541557, 62.24863466993041072, -9.382169495545420901 ) ) ;
#20019 = CARTESIAN_POINT ( 'NONE',  ( 17.96484262340118221, 39.93868534415484106, 7.964842623401181321 ) ) ;
#20020 = EDGE_CURVE ( 'NONE', #18735, #59535, #27858, .T. ) ;
#20021 = CARTESIAN_POINT ( 'NONE',  ( -7.750000000000000000, 40.74999999999999289, -4.000000000000000000 ) ) ;
#20022 = CARTESIAN_POINT ( 'NONE',  ( 22.81628187352647785, 21.62363466993041783, 6.195893100308588602E-16 ) ) ;
#20023 = CARTESIAN_POINT ( 'NONE',  ( 12.63842701281683034, 52.46726448433413026, 9.846743663894596210 ) ) ;
#20024 = CARTESIAN_POINT ( 'NONE',  ( 10.88017736071110519, 20.56368534415484106, -2.602085213965210642E-15 ) ) ;
#20025 = CARTESIAN_POINT ( 'NONE',  ( 4.559911319644449179, 63.89701867748817676, 9.422509992056141925 ) ) ;
#20026 = ORIENTED_EDGE ( 'NONE', *, *, #41296, .T. ) ;
#20028 = EDGE_CURVE ( 'NONE', #77584, #94846, #45115, .T. ) ;
#20027 = DIRECTION ( 'NONE',  ( 0.000000000000000000, 1.000000000000000000, 0.000000000000000000 ) ) ;
#20029 = CARTESIAN_POINT ( 'NONE',  ( 4.559911319644449179, 68.89701867748817676, 9.422509992056141925 ) ) ;
#20030 = CARTESIAN_POINT ( 'NONE',  ( 19.84674366389459621, 3.508931151000785231, 7.409399052514197653E-17 ) ) ;
#20031 = CARTESIAN_POINT ( 'NONE',  ( 18.00000000000000000, 77.62863618567965318, -4.012044701513177714 ) ) ;
#20032 = VECTOR ( 'NONE', #92530, 1000.000000000000114 ) ;
#20033 = CARTESIAN_POINT ( 'NONE',  ( 7.361572987183169658, 34.96726448433411605, -9.846743663894592657 ) ) ;
#20034 = CARTESIAN_POINT ( 'NONE',  ( 4.559911319644449179, 28.89701867748817321, 9.422509992056141925 ) ) ;
#20035 = CARTESIAN_POINT ( 'NONE',  ( 22.81628187352647785, 6.623634669930420493, 6.195893100308588602E-16 ) ) ;
#20037 = CARTESIAN_POINT ( 'NONE',  ( 13.99999999999999822, 11.00000000000000000, 6.000000000000000000 ) ) ;
#20036 = CARTESIAN_POINT ( 'NONE',  ( 2.035157376598822676, 32.43868534415483396, -7.964842623401177768 ) ) ;
#20038 = SURFACE_SIDE_STYLE ('',( #51028 ) ) ;
#20039 = CARTESIAN_POINT ( 'NONE',  ( 19.38216949554541202, 35.99863466993041072, 9.382169495545424454 ) ) ;
#20040 = ORIENTED_EDGE ( 'NONE', *, *, #47764, .T. ) ;
#20041 = CARTESIAN_POINT ( 'NONE',  ( 10.00000000000000178, 59.31368534415484106, 10.88017736071110342 ) ) ;
#20043 = CARTESIAN_POINT ( 'NONE',  ( 19.84674366389459621, 18.50893115100078745, 7.409399052514197653E-17 ) ) ;
#20042 = CARTESIAN_POINT ( 'NONE',  ( 22.81628187352647785, 21.62363466993041783, 6.195893100308588602E-16 ) ) ;
#20044 = SURFACE_SIDE_STYLE ('',( #88543 ) ) ;
#20045 = CARTESIAN_POINT ( 'NONE',  ( 0.5774900079438607392, 43.48035201082151247, 5.440088680355550821 ) ) ;
#20046 = CARTESIAN_POINT ( 'NONE',  ( 24.16423886937410614, 64.30374883491396076, 8.672049930838204340E-16 ) ) ;
#20047 = CARTESIAN_POINT ( 'NONE',  ( 10.00000000000000178, 57.25893115100078745, 9.846743663894594434 ) ) ;
#20048 = CARTESIAN_POINT ( 'NONE',  ( 2.791683348922237240, 10.38393115100078390, -7.208316651077763204 ) ) ;
#20049 = CARTESIAN_POINT ( 'NONE',  ( 2.035157376598822676, 62.43868534415483396, -7.964842623401177768 ) ) ;
#20050 = DIRECTION ( 'NONE',  ( 0.000000000000000000, 0.000000000000000000, 1.000000000000000000 ) ) ;
#20051 = CARTESIAN_POINT ( 'NONE',  ( 24.16423886937410614, 29.30374883491396787, 8.672049930838204340E-16 ) ) ;
#20052 = COLOUR_RGB ( '', 0.66274510, 0.83137255, 0.94901961) ;
#20053 = FACE_OUTER_BOUND ( 'NONE', #94862, .T. ) ;
#20054 = CARTESIAN_POINT ( 'NONE',  ( 19.59355871817327710, 82.60099334974556484, -5.130928526377548593 ) ) ;
#20055 = ORIENTED_EDGE ( 'NONE', *, *, #82443, .F. ) ;
#20056 = ORIENTED_EDGE ( 'NONE', *, *, #42417, .F. ) ;
#20057 = CARTESIAN_POINT ( 'NONE',  ( 13.79529636645031943, 60.34541550158063927, -14.16423886937409904 ) ) ;
#20058 = CARTESIAN_POINT ( 'NONE',  ( 17.08211943468705130, 53.47041550158063217, 12.26659068614894998 ) ) ;
#20059 = CARTESIAN_POINT ( 'NONE',  ( 19.84674366389459266, 28.30059781766745886, 2.638427012816836559 ) ) ;
#20061 = CARTESIAN_POINT ( 'NONE',  ( 0.6178305044545818747, 23.49863466993041783, -9.382169495545419124 ) ) ;
#20060 = AXIS2_PLACEMENT_3D ( 'NONE', #80779, #73757, #58249 ) ;
#20062 = LINE ( 'NONE', #34557, #55558 ) ;
#20063 = SURFACE_STYLE_USAGE ( .BOTH. , #12564 ) ;
#20064 = CARTESIAN_POINT ( 'NONE',  ( -4.164238869374099927, 47.01208216824729647, 3.795296366450308767 ) ) ;
#20065 = DIRECTION ( 'NONE',  ( 1.000000000000000000, 0.000000000000000000, 0.000000000000000000 ) ) ;
#20066 = CARTESIAN_POINT ( 'NONE',  ( 14.92337183194729988, 4.342264484334117824, -8.527530157486177487 ) ) ;
#20067 = LINE ( 'NONE', #29530, #46615 ) ;
#20068 = CARTESIAN_POINT ( 'NONE',  ( 7.208316651077764980, 7.883931151000783011, 7.208316651077762316 ) ) ;
#20069 = EDGE_CURVE ( 'NONE', #1023, #61713, #29660, .T. ) ;
#20070 = ORIENTED_EDGE ( 'NONE', *, *, #44531, .F. ) ;
#20071 = ORIENTED_EDGE ( 'NONE', *, *, #35702, .T. ) ;
#20072 = SURFACE_STYLE_USAGE ( .BOTH. , #88072 ) ;
#20073 = ORIENTED_EDGE ( 'NONE', *, *, #82402, .F. ) ;
#20075 = CARTESIAN_POINT ( 'NONE',  ( 17.96484262340118221, 26.18868534415483396, -7.964842623401177768 ) ) ;
#20074 = CARTESIAN_POINT ( 'NONE',  ( 10.00000000000000000, 21.81368534415484106, -10.88017736071110342 ) ) ;
#20077 = CARTESIAN_POINT ( 'NONE',  ( 21.09922568453594849, 16.20696800326375353, 6.408140936763242479 ) ) ;
#20076 = CARTESIAN_POINT ( 'NONE',  ( 10.00000000000000178, 52.25893115100078745, 9.846743663894594434 ) ) ;
#20078 = PRESENTATION_STYLE_ASSIGNMENT (( #95596 ) ) ;
#20079 = ADVANCED_FACE ( 'NONE', ( #22637 ), #12778, .T. ) ;
#20080 = STYLED_ITEM ( 'NONE', ( #65643 ), #35604 ) ;
#20081 = MECHANICAL_DESIGN_GEOMETRIC_PRESENTATION_REPRESENTATION (  '', ( #77599 ), #53623 ) ;
#20083 = VECTOR ( 'NONE', #36357, 999.9999999999998863 ) ;
#20082 = B_SPLINE_CURVE_WITH_KNOTS ( 'NONE', 3,
 ( #79823, #34806, #33804, #34300, #64798, #58284, #19808, #73790, #26818, #57311 ),
 .UNSPECIFIED., .F., .F.,
 ( 4, 3, 3, 4 ),
 ( 1.398578778534940505E-17, 0.0006253016069560823811, 0.001250604074564926060, 0.002501455912506542201 ),
 .UNSPECIFIED. ) ;
#20085 = CARTESIAN_POINT ( 'NONE',  ( 16.40814093676323893, 15.79030133659708746, 11.09922568453595026 ) ) ;
#20084 = CIRCLE ( 'NONE', #31214, 14.49999999999999822 ) ;
#20086 = EDGE_LOOP ( 'NONE', ( #55986, #11128, #9672, #52510 ) ) ;
#20087 = CARTESIAN_POINT ( 'NONE',  ( 10.00000000000000178, 37.25893115100078745, 9.846743663894594434 ) ) ;
#20088 = CARTESIAN_POINT ( 'NONE',  ( 13.79529636645030344, 63.26208216824730357, 14.16423886937410614 ) ) ;
#20089 = CARTESIAN_POINT ( 'NONE',  ( 12.91533473730992121, 4.522018677488170546, 10.88017736071110164 ) ) ;
#20090 = ORIENTED_EDGE ( 'NONE', *, *, #15921, .T. ) ;
#20091 = CARTESIAN_POINT ( 'NONE',  ( -0.8801773607110991993, 52.85535201082151247, -2.915334737309923874 ) ) ;
#20092 = CARTESIAN_POINT ( 'NONE',  ( 19.42250999205614193, 40.14701867748817676, 5.440088680355555262 ) ) ;
#20093 = CARTESIAN_POINT ( 'NONE',  ( 15.44008868035555260, 49.73035201082150536, 9.422509992056143702 ) ) ;
#20094 = DIRECTION ( 'NONE',  ( -0.000000000000000000, -0.000000000000000000, -1.000000000000000000 ) ) ;
#20095 = CARTESIAN_POINT ( 'NONE',  ( -0.8801773607111008646, 38.27201867748816255, 2.915334737309923430 ) ) ;
#20096 = CARTESIAN_POINT ( 'NONE',  ( 21.92686044187657401, 65.37045670184114954, -3.195792623639525765 ) ) ;
#20097 = SURFACE_STYLE_FILL_AREA ( #26609 ) ;
#20098 = EDGE_CURVE ( 'NONE', #56218, #63343, #53118, .T. ) ;
#20100 = B_SPLINE_CURVE_WITH_KNOTS ( 'NONE', 3,
 ( #39895, #48368, #85889, #17403, #48857, #94360 ),
 .UNSPECIFIED., .F., .F.,
 ( 4, 2, 4 ),
 ( 3.409110551494643301E-05, 0.0004400426677367919384, 0.0008459942299586375048 ),
 .UNSPECIFIED. ) ;
#20099 = CARTESIAN_POINT ( 'NONE',  ( 0.1532563361054082862, 31.21726448433412315, 2.638427012816831674 ) ) ;
#20101 = ORIENTED_EDGE ( 'NONE', *, *, #90664, .T. ) ;
#20102 = CARTESIAN_POINT ( 'NONE',  ( 19.84674366389459266, 53.71726448433411605, -2.638427012816827677 ) ) ;
#20104 = EDGE_CURVE ( 'NONE', #3713, #97731, #68134, .T. ) ;
#20103 = DIRECTION ( 'NONE',  ( 0.000000000000000000, 0.000000000000000000, 1.000000000000000000 ) ) ;
#20105 = DIRECTION ( 'NONE',  ( 0.000000000000000000, -0.000000000000000000, 1.000000000000000000 ) ) ;
#20106 = VERTEX_POINT ( 'NONE', #20785 ) ;
#20107 = CARTESIAN_POINT ( 'NONE',  ( -11.17418640071729818, 12.98409833943821567, 3.592726937080809257 ) ) ;
#20108 = CARTESIAN_POINT ( 'NONE',  ( 9.722841580490404922, 15.00000000000000000, 12.70211588817942960 ) ) ;
#20109 = CARTESIAN_POINT ( 'NONE',  ( -3.192513988407930547, -3.205596188883898450E-15, -14.27292421863754512 ) ) ;
#20110 = CARTESIAN_POINT ( 'NONE',  ( -4.164238869374098151, 61.59541550158063217, -3.795296366450310543 ) ) ;
#20111 = DIRECTION ( 'NONE',  ( 0.000000000000000000, 0.000000000000000000, 1.000000000000000000 ) ) ;
#20112 = EDGE_LOOP ( 'NONE', ( #95339, #27204, #77619, #28312 ) ) ;
#20113 = CARTESIAN_POINT ( 'NONE',  ( -8.124115902427742952, 75.04369783535877048, -3.000000000000000000 ) ) ;
#20114 = CARTESIAN_POINT ( 'NONE',  ( 14.92337183194729988, 29.34226448433411960, -8.527530157486177487 ) ) ;
#20115 = CARTESIAN_POINT ( 'NONE',  ( 7.595945211629608451, 15.00000000000000000, 12.35117874302463292 ) ) ;
#20116 = VECTOR ( 'NONE', #32572, 1000.000000000000227 ) ;
#20117 = CARTESIAN_POINT ( 'NONE',  ( 16.40814093676324603, 7.456968003263754419, -11.09922568453594671 ) ) ;
#20118 = CARTESIAN_POINT ( 'NONE',  ( 0.1532563361054083140, 6.008931151000784787, 1.131784320476157264E-15 ) ) ;
#20119 = CARTESIAN_POINT ( 'NONE',  ( 0.1516233060550335465, 0.2505839662184247141, 6.438133714914693329 ) ) ;
#20120 = CARTESIAN_POINT ( 'NONE',  ( 19.84674366389459266, 8.300597817667451750, 2.638427012816836559 ) ) ;
#20121 = CARTESIAN_POINT ( 'NONE',  ( 5.076628168052704559, 55.17559781766745175, -8.527530157486179263 ) ) ;
#20122 = DIRECTION ( 'NONE',  ( -0.000000000000000000, 1.000000000000000000, -0.000000000000000000 ) ) ;
#20123 = ORIENTED_EDGE ( 'NONE', *, *, #6464, .T. ) ;
#20124 = CARTESIAN_POINT ( 'NONE',  ( 19.42250999205614548, 5.980352010821504471, -5.440088680355545492 ) ) ;
#20125 = CARTESIAN_POINT ( 'NONE',  ( 6.204703633549690345, 2.845415501580634388, 14.16423886937410082 ) ) ;
#20126 = CARTESIAN_POINT ( 'NONE',  ( 0.1532563361054100626, 10.80059781766745175, -2.638427012816831230 ) ) ;
#20127 = CARTESIAN_POINT ( 'NONE',  ( 17.96484262340118221, 49.93868534415484106, 7.964842623401181321 ) ) ;
#20129 = CARTESIAN_POINT ( 'NONE',  ( -5.112373461513591621, -25.53775085953292390, -2.750000000000000444 ) ) ;
#20128 = CARTESIAN_POINT ( 'NONE',  ( 3.591859063236763294, 28.29030133659708568, -11.09922568453595026 ) ) ;
#20130 = CARTESIAN_POINT ( 'NONE',  ( 10.00000000000000000, 1.813685344154837731, -10.88017736071110342 ) ) ;
#20131 = EDGE_CURVE ( 'NONE', #94488, #98433, #80296, .T. ) ;
#20132 = DIRECTION ( 'NONE',  ( 0.000000000000000000, 0.000000000000000000, 1.000000000000000000 ) ) ;
#20133 = LINE ( 'NONE', #66118, #36019 ) ;
#20134 = CARTESIAN_POINT ( 'NONE',  ( 13.43411237798106583, 2.665301336597086568, -12.81628187352647252 ) ) ;
#20135 = CARTESIAN_POINT ( 'NONE',  ( 18.52753015748617571, 63.09226448433412315, 4.923371831947298993 ) ) ;
#20136 = CARTESIAN_POINT ( 'NONE',  ( 1.472469842513823179, 10.59226448433411782, -4.923371831947296329 ) ) ;
#20137 = CARTESIAN_POINT ( 'NONE',  ( 2.915334737309921209, -23.39464798917849464, -10.88017736071110164 ) ) ;
#20138 = CARTESIAN_POINT ( 'NONE',  ( -1.099225684535947600, 19.54030133659708568, 6.408140936763237150 ) ) ;
#20139 = CARTESIAN_POINT ( 'NONE',  ( 1.383448333479234904, 52.37718327197428891, -6.499999999999977796 ) ) ;
#20140 = CARTESIAN_POINT ( 'NONE',  ( 2.035157376598824452, 23.68868534415484461, 7.964842623401179544 ) ) ;
#20141 = DIRECTION ( 'NONE',  ( -1.000000000000000000, 6.938893903907222067E-15, 0.000000000000000000 ) ) ;
#20142 = CARTESIAN_POINT ( 'NONE',  ( 13.79529636645030344, 53.26208216824730357, 14.16423886937410614 ) ) ;
#20143 = CARTESIAN_POINT ( 'NONE',  ( 6.935110064710753974, -80.58145365566650753, -3.750000000000002665 ) ) ;
#20144 = STYLED_ITEM ( 'NONE', ( #67915 ), #36713 ) ;
#20145 = CARTESIAN_POINT ( 'NONE',  ( 15.44008868035555260, 24.73035201082150891, 9.422509992056143702 ) ) ;
#20146 = COLOUR_RGB ( '', 0.31764706, 0.68627451, 0.89019608) ;
#20147 = CARTESIAN_POINT ( 'NONE',  ( 0.1532563361054082862, 56.21726448433411605, 2.638427012816831674 ) ) ;
#20148 = CARTESIAN_POINT ( 'NONE',  ( 0.5774900079438590739, 57.64701867748817676, -5.440088680355550821 ) ) ;
#20149 = CARTESIAN_POINT ( 'NONE',  ( -2.266590686148945544, 36.38708216824730357, -7.082119434687050408 ) ) ;
#20150 = LINE ( 'NONE', #81632, #61524 ) ;
#20151 =( GEOMETRIC_REPRESENTATION_CONTEXT ( 3 ) GLOBAL_UNCERTAINTY_ASSIGNED_CONTEXT ( ( #80505 ) ) GLOBAL_UNIT_ASSIGNED_CONTEXT ( ( #8290, #23801, #74802 ) ) REPRESENTATION_CONTEXT ( 'NONE', 'WORKASPACE' ) );
#20152 = UNCERTAINTY_MEASURE_WITH_UNIT (LENGTH_MEASURE( 1.000000000000000082E-05 ), #19702, 'distance_accuracy_value', 'NONE');
#20153 = CARTESIAN_POINT ( 'NONE',  ( 14.92337183194729988, 34.34226448433411605, -8.527530157486177487 ) ) ;
#20154 = CARTESIAN_POINT ( 'NONE',  ( 3.591859063236763294, 58.29030133659708923, -11.09922568453595026 ) ) ;
#20155 = CARTESIAN_POINT ( 'NONE',  ( 14.92337183194729633, 62.67559781766745886, 8.527530157486181039 ) ) ;
#20156 = VERTEX_POINT ( 'NONE', #51276 ) ;
#20157 = CARTESIAN_POINT ( 'NONE',  ( 0.5774900079438607392, 18.48035201082150536, 5.440088680355550821 ) ) ;
#20158 = DIRECTION ( 'NONE',  ( 0.000000000000000000, 0.000000000000000000, 1.000000000000000000 ) ) ;
#20159 = DIRECTION ( 'NONE',  ( 1.000000000000000000, 0.000000000000000000, 0.000000000000000000 ) ) ;
#20160 = CARTESIAN_POINT ( 'NONE',  ( 10.00000000000000000, 11.81368534415483751, -10.88017736071110342 ) ) ;
#20161 = CARTESIAN_POINT ( 'NONE',  ( 15.44008868035555260, 64.73035201082151957, 9.422509992056143702 ) ) ;
#20162 = CARTESIAN_POINT ( 'NONE',  ( 17.08211943468705840, 25.13708216824730357, -12.26659068614894466 ) ) ;
#20163 = CARTESIAN_POINT ( 'NONE',  ( 17.20831665107776587, 14.13393115100078568, -7.208316651077762316 ) ) ;
#20164 = CARTESIAN_POINT ( 'NONE',  ( 12.63842701281683034, 57.46726448433411605, 9.846743663894596210 ) ) ;
#20165 = CARTESIAN_POINT ( 'NONE',  ( 15.44008868035555793, 31.39701867748817676, -9.422509992056140149 ) ) ;
#20166 = CARTESIAN_POINT ( 'NONE',  ( -5.361923921558584105, 0.000000000000000000, 0.9937738586171629418 ) ) ;
#20168 = VERTEX_POINT ( 'NONE', #81761 ) ;
#20167 = AXIS2_PLACEMENT_3D ( 'NONE', #53699, #68712, #60704 ) ;
#20169 = LINE ( 'NONE', #35667, #59292 ) ;
#20170 = CARTESIAN_POINT ( 'NONE',  ( 12.63842701281683922, 49.55059781766744464, -9.846743663894590881 ) ) ;
#20171 = AXIS2_PLACEMENT_3D ( 'NONE', #25424, #64367, #8918 ) ;
#20172 = VERTEX_POINT ( 'NONE', #41824 ) ;
#20173 = EDGE_LOOP ( 'NONE', ( #94577, #52042, #62448, #89610 ) ) ;
#20174 = CARTESIAN_POINT ( 'NONE',  ( 8.235571585149873641, 9.796802177851539284, 8.235571585149866536 ) ) ;
#20175 = CARTESIAN_POINT ( 'NONE',  ( 24.16423886937409904, 9.095415501580633943, 3.795296366450317205 ) ) ;
#20177 = MECHANICAL_DESIGN_GEOMETRIC_PRESENTATION_REPRESENTATION (  '', ( #13832 ), #80843 ) ;
#20176 = CARTESIAN_POINT ( 'NONE',  ( 2.917880565312948704, 12.63708216824730179, 12.26659068614894643 ) ) ;
#20178 = CARTESIAN_POINT ( 'NONE',  ( 0.5774900079438590739, 47.64701867748817676, -5.440088680355550821 ) ) ;
#20179 = CARTESIAN_POINT ( 'NONE',  ( 24.16423886937409904, 54.09541550158063217, 3.795296366450317205 ) ) ;
#20180 = CARTESIAN_POINT ( 'NONE',  ( 22.81628187352647785, 6.623634669930420493, 6.195893100308588602E-16 ) ) ;
#20181 = CARTESIAN_POINT ( 'NONE',  ( 17.20831665107776587, 39.13393115100079456, -7.208316651077762316 ) ) ;
#20182 = SURFACE_STYLE_USAGE ( .BOTH. , #88674 ) ;
#20184 = CARTESIAN_POINT ( 'NONE',  ( 21.09922568453595559, 7.040301336597086568, -6.408140936763230044 ) ) ;
#20183 = CARTESIAN_POINT ( 'NONE',  ( 12.91533473730992121, 34.52201867748817676, 10.88017736071110164 ) ) ;
#20185 = CARTESIAN_POINT ( 'NONE',  ( 10.00000000000000178, 8.053748834913967869, 14.16423886937410082 ) ) ;
#20186 = CARTESIAN_POINT ( 'NONE',  ( -4.164238869374099927, 57.01208216824731068, 3.795296366450308767 ) ) ;
#20187 = CARTESIAN_POINT ( 'NONE',  ( 19.42250999205614548, 15.98035201082150714, -5.440088680355545492 ) ) ;
#20188 = CARTESIAN_POINT ( 'NONE',  ( 17.39651004071841101, 37.93575266056827644, 6.500000000000005329 ) ) ;
#20189 = DIRECTION ( 'NONE',  ( -0.9914448613738093830, 0.000000000000000000, -0.1305261922200583180 ) ) ;
#20190 = B_SPLINE_CURVE_WITH_KNOTS ( 'NONE', 3,
 ( #46593, #69601, #25588, #94066, #79057, #1122 ),
 .UNSPECIFIED., .F., .F.,
 ( 4, 2, 4 ),
 ( 0.0002800518438701976435, 0.0006862575805781378786, 0.001092463317286078168 ),
 .UNSPECIFIED. ) ;
#20191 = DIRECTION ( 'NONE',  ( -0.000000000000000000, 1.000000000000000000, -0.000000000000000000 ) ) ;
#20192 = ORIENTED_EDGE ( 'NONE', *, *, #29887, .T. ) ;
#20193 = FACE_OUTER_BOUND ( 'NONE', #6869, .T. ) ;
#20194 = EDGE_LOOP ( 'NONE', ( #28548, #45034, #68105, #47595, #67681, #50931 ) ) ;
#20195 = ORIENTED_EDGE ( 'NONE', *, *, #65117, .T. ) ;
#20196 = CARTESIAN_POINT ( 'NONE',  ( -4.164238869374098151, 41.59541550158061796, -3.795296366450310543 ) ) ;
#20197 = CARTESIAN_POINT ( 'NONE',  ( 12.63842701281683034, 52.46726448433413026, 9.846743663894596210 ) ) ;
#20198 = CARTESIAN_POINT ( 'NONE',  ( 19.42250999205614548, 50.98035201082151247, -5.440088680355545492 ) ) ;
#20199 = EDGE_CURVE ( 'NONE', #60520, #51757, #11794, .T. ) ;
#20200 = DIRECTION ( 'NONE',  ( -0.000000000000000000, -0.000000000000000000, -1.000000000000000000 ) ) ;
#20201 = CARTESIAN_POINT ( 'NONE',  ( -0.8801773607111009756, 58.06368534415484106, 1.068504757029289695E-15 ) ) ;
#20202 = CARTESIAN_POINT ( 'NONE',  ( 6.565887622018943937, 58.08196800326376064, -12.81628187352647608 ) ) ;
#20203 = CARTESIAN_POINT ( 'NONE',  ( 6.408140936763236262, 2.456968003263761080, -11.09922568453595026 ) ) ;
#20204 = AXIS2_PLACEMENT_3D ( 'NONE', #87456, #72441, #49450 ) ;
#20205 = VERTEX_POINT ( 'NONE', #3821 ) ;
#20206 = CARTESIAN_POINT ( 'NONE',  ( 13.79529636645031943, 20.34541550158063572, -14.16423886937409904 ) ) ;
#20207 = CARTESIAN_POINT ( 'NONE',  ( 0.6178305044545818747, 23.49863466993041783, -9.382169495545419124 ) ) ;
#20208 = B_SPLINE_CURVE_WITH_KNOTS ( 'NONE', 3,
 ( #90067, #93020, #71525, #63982 ),
 .UNSPECIFIED., .F., .F.,
 ( 4, 4 ),
 ( 0.000000000000000000, 0.001036303429213355966 ),
 .UNSPECIFIED. ) ;
#20209 = ORIENTED_EDGE ( 'NONE', *, *, #97449, .F. ) ;
#20210 = CARTESIAN_POINT ( 'NONE',  ( -2.816281873526473856, 39.33196800326374643, 3.434112377981055619 ) ) ;
#20211 = CARTESIAN_POINT ( 'NONE',  ( 15.44008868035555260, 14.73035201082150536, 9.422509992056143702 ) ) ;
#20212 = CARTESIAN_POINT ( 'NONE',  ( 18.52753015748617571, 43.09226448433412315, 4.923371831947298993 ) ) ;
#20213 = CARTESIAN_POINT ( 'NONE',  ( 10.00000000000000000, 11.81368534415483751, -10.88017736071110342 ) ) ;
#20214 = CARTESIAN_POINT ( 'NONE',  ( 19.38216949554541202, 55.99863466993041072, 9.382169495545424454 ) ) ;
#20215 = CARTESIAN_POINT ( 'NONE',  ( 0.2751277870542967463, 70.00000000000000000, 6.000000000000000000 ) ) ;
#20216 = CARTESIAN_POINT ( 'NONE',  ( 1.472469842513823179, 46.42559781766745175, 4.923371831947296329 ) ) ;
#20217 = VECTOR ( 'NONE', #40317, 1000.000000000000114 ) ;
#20218 = CARTESIAN_POINT ( 'NONE',  ( 17.96484262340118221, 51.18868534415483396, -7.964842623401177768 ) ) ;
#20220 = ORIENTED_EDGE ( 'NONE', *, *, #24086, .T. ) ;
#20219 = CARTESIAN_POINT ( 'NONE',  ( 0.000000000000000000, 0.000000000000000000, 0.000000000000000000 ) ) ;
#20221 = ADVANCED_FACE ( 'NONE', ( #34785 ), #34276, .F. ) ;
#20222 = FILL_AREA_STYLE ('',( #88712 ) ) ;
#20223 = DIRECTION ( 'NONE',  ( -1.000000000000000000, 0.000000000000000000, 0.000000000000000000 ) ) ;
#20224 = TOROIDAL_SURFACE ( 'NONE', #39377, 14.49999999999999822, 0.5000000000000000000 ) ;
#20225 = CARTESIAN_POINT ( 'NONE',  ( 2.603489959281588106, 1.582109641433292690, 6.500000000000000888 ) ) ;
#20226 = CARTESIAN_POINT ( 'NONE',  ( 0.1532563361054100626, 20.80059781766744464, -2.638427012816831230 ) ) ;
#20227 = EDGE_CURVE ( 'NONE', #41669, #81607, #65273, .T. ) ;
#20228 = CARTESIAN_POINT ( 'NONE',  ( -1.099225684535947600, 23.70696800326375708, -6.408140936763238038 ) ) ;
#20229 = FACE_OUTER_BOUND ( 'NONE', #82669, .T. ) ;
#20230 = ORIENTED_EDGE ( 'NONE', *, *, #31276, .T. ) ;
#20231 = CARTESIAN_POINT ( 'NONE',  ( 19.84674366389459266, 53.71726448433411605, -2.638427012816827677 ) ) ;
#20232 = CARTESIAN_POINT ( 'NONE',  ( -11.29222593019783538, 0.2306972965111817597, 9.783848334571175087 ) ) ;
#20233 = CARTESIAN_POINT ( 'NONE',  ( -2.266590686148945544, 17.22041550158063572, 7.082119434687048631 ) ) ;
#20234 = CARTESIAN_POINT ( 'NONE',  ( 1.472469842513823179, 35.59226448433412315, -4.923371831947296329 ) ) ;
#20235 = CARTESIAN_POINT ( 'NONE',  ( 13.43411237798106583, 42.66530133659707502, -12.81628187352647252 ) ) ;
#20237 = LINE ( 'NONE', #51227, #4969 ) ;
#20236 = CARTESIAN_POINT ( 'NONE',  ( -11.81378540890925066, 0.000000000000000000, -7.968498874458281200 ) ) ;
#20238 = CARTESIAN_POINT ( 'NONE',  ( 0.5774900079438590739, 62.64701867748817676, -5.440088680355550821 ) ) ;
#20239 = CARTESIAN_POINT ( 'NONE',  ( 10.00000000000000178, 15.37363466993042138, 12.81628187352647608 ) ) ;
#20240 = AXIS2_PLACEMENT_3D ( 'NONE', #28885, #75884, #66403 ) ;
#20241 = DIRECTION ( 'NONE',  ( 0.000000000000000000, 1.000000000000000000, 0.000000000000000000 ) ) ;
#20242 = CARTESIAN_POINT ( 'NONE',  ( 12.63842701281683034, 37.46726448433411605, 9.846743663894596210 ) ) ;
#20243 = CARTESIAN_POINT ( 'NONE',  ( 19.42250999205614548, 45.98035201082150536, -5.440088680355545492 ) ) ;
#20244 = CARTESIAN_POINT ( 'NONE',  ( 3.591859063236763294, 43.29030133659708923, -11.09922568453595026 ) ) ;
#20245 = CIRCLE ( 'NONE', #29873, 6.999999999999995559 ) ;
#20246 = CARTESIAN_POINT ( 'NONE',  ( 17.20831665107776587, 32.88393115100078745, 7.208316651077764980 ) ) ;
#20247 = CIRCLE ( 'NONE', #33016, 0.2500000000000002220 ) ;
#20248 = CARTESIAN_POINT ( 'NONE',  ( -13.39911793698215270, 90.87255582226832473, 7.784798940734791728 ) ) ;
#20249 = CIRCLE ( 'NONE', #50586, 15.00000000000000000 ) ;
#20250 = CARTESIAN_POINT ( 'NONE',  ( 2.035157376598824452, 28.68868534415484106, 7.964842623401179544 ) ) ;
#20251 = ORIENTED_EDGE ( 'NONE', *, *, #17531, .F. ) ;
#20252 = CARTESIAN_POINT ( 'NONE',  ( -4.000000000000000000, 10.00000000000000000, -2.500000000000000000 ) ) ;
#20253 = CARTESIAN_POINT ( 'NONE',  ( 10.00000000000000000, 11.81368534415483751, -10.88017736071110342 ) ) ;
#20255 = CARTESIAN_POINT ( 'NONE',  ( 2.035157376598824452, 28.68868534415484106, 7.964842623401179544 ) ) ;
#20254 = CARTESIAN_POINT ( 'NONE',  ( 18.52753015748618282, 58.92559781766745886, -4.923371831947291888 ) ) ;
#20256 = CARTESIAN_POINT ( 'NONE',  ( 15.00000000000000000, 11.50000000000000000, -6.000000000000000000 ) ) ;
#20257 = CARTESIAN_POINT ( 'NONE',  ( 12.91533473730993009, 61.60535201082150536, -10.88017736071109987 ) ) ;
#20259 = CARTESIAN_POINT ( 'NONE',  ( 0.000000000000000000, 77.50050546096726123, -8.104077677183505912 ) ) ;
#20258 = CARTESIAN_POINT ( 'NONE',  ( 12.91533473730993009, 31.60535201082150891, -10.88017736071109987 ) ) ;
#20260 = LINE ( 'NONE', #73247, #2019 ) ;
#20261 = CARTESIAN_POINT ( 'NONE',  ( 0.1532563361054100626, 30.80059781766744820, -2.638427012816831230 ) ) ;
#20262 = FILL_AREA_STYLE ('',( #57263 ) ) ;
#20263 = CARTESIAN_POINT ( 'NONE',  ( 12.26659068614894821, 3.887082168247312008, 7.082119434687044190 ) ) ;
#20264 = CARTESIAN_POINT ( 'NONE',  ( 0.1532563361054100626, 50.80059781766745175, -2.638427012816831230 ) ) ;
#20266 = CARTESIAN_POINT ( 'NONE',  ( 6.575034241980325156, -50.89776066942204835, 3.750000000000000000 ) ) ;
#20265 = CARTESIAN_POINT ( 'NONE',  ( 22.26659068614894466, 53.88708216824731068, 7.082119434687054849 ) ) ;
#20267 = SURFACE_SIDE_STYLE ('',( #58237 ) ) ;
#20268 = ADVANCED_FACE ( 'NONE', ( #62084 ), #45620, .F. ) ;
#20269 = CARTESIAN_POINT ( 'NONE',  ( 6.204703633549690345, 7.845415501580634832, 14.16423886937410082 ) ) ;
#20270 = CARTESIAN_POINT ( 'NONE',  ( -4.164238869374098151, 36.59541550158063217, -3.795296366450310543 ) ) ;
#20271 = CARTESIAN_POINT ( 'NONE',  ( 21.09922568453594849, 6.206968003263753531, 6.408140936763242479 ) ) ;
#20272 = PLANE ( 'NONE',  #9022 ) ;
#20273 = ORIENTED_EDGE ( 'NONE', *, *, #80611, .F. ) ;
#20274 = CARTESIAN_POINT ( 'NONE',  ( 19.42250999205614548, 15.98035201082150714, -5.440088680355545492 ) ) ;
#20275 = CARTESIAN_POINT ( 'NONE',  ( 10.00000000000000178, 37.25893115100078745, 9.846743663894594434 ) ) ;
#20276 = CARTESIAN_POINT ( 'NONE',  ( -10.80370554825945284, 89.74834511847251406, -6.353281608588780216 ) ) ;
#20277 = DIRECTION ( 'NONE',  ( 0.000000000000000000, 1.000000000000000000, 0.000000000000000000 ) ) ;
#20278 = CARTESIAN_POINT ( 'NONE',  ( 7.361572987183170547, 2.050597817667451750, 9.846743663894590881 ) ) ;
#20279 = CARTESIAN_POINT ( 'NONE',  ( 13.43411237798105340, 25.58196800326374998, 12.81628187352647963 ) ) ;
#20280 = CARTESIAN_POINT ( 'NONE',  ( 14.92337183194729633, 22.67559781766745175, 8.527530157486181039 ) ) ;
#20281 = ORIENTED_EDGE ( 'NONE', *, *, #4005, .T. ) ;
#20282 = CARTESIAN_POINT ( 'NONE',  ( 12.63842701281683034, 12.46726448433411782, 9.846743663894596210 ) ) ;
#20283 = PLANE ( 'NONE',  #14157 ) ;
#20284 = CARTESIAN_POINT ( 'NONE',  ( -2.266590686148945544, 67.22041550158063217, 7.082119434687048631 ) ) ;
#20285 = CARTESIAN_POINT ( 'NONE',  ( 20.88017736071110519, 20.56368534415484106, 2.639326808657452039E-16 ) ) ;
#20286 = CARTESIAN_POINT ( 'NONE',  ( 13.79529636645031943, 35.34541550158063927, -14.16423886937409904 ) ) ;
#20287 = CARTESIAN_POINT ( 'NONE',  ( 7.084665262690076126, 29.10535201082150181, 10.88017736071109987 ) ) ;
#20288 = CARTESIAN_POINT ( 'NONE',  ( 10.00000000000000178, 64.31368534415483396, 10.88017736071110342 ) ) ;
#20289 = CARTESIAN_POINT ( 'NONE',  ( 0.2751277870542967463, 70.00000000000000000, 6.000000000000000000 ) ) ;
#20290 = DIRECTION ( 'NONE',  ( 0.000000000000000000, 1.000000000000000000, 0.000000000000000000 ) ) ;
#20291 = CARTESIAN_POINT ( 'NONE',  ( 14.92337183194729988, 29.34226448433411960, -8.527530157486177487 ) ) ;
#20292 = CARTESIAN_POINT ( 'NONE',  ( -9.000000000000001776, 80.99999999999994316, 0.000000000000000000 ) ) ;
#20293 = CARTESIAN_POINT ( 'NONE',  ( 0.1532563361054100626, 0.8005978176674514168, -2.638427012816831230 ) ) ;
#20294 = CARTESIAN_POINT ( 'NONE',  ( 12.80781515976310203, 15.00000000000000000, 6.246788841744411513 ) ) ;
#20295 = CARTESIAN_POINT ( 'NONE',  ( 0.1532563361054082862, 36.21726448433410894, 2.638427012816831674 ) ) ;
#20296 = CARTESIAN_POINT ( 'NONE',  ( 5.076628168052704559, 60.17559781766745175, -8.527530157486179263 ) ) ;
#20297 = CARTESIAN_POINT ( 'NONE',  ( 4.559911319644449179, 33.89701867748817676, 9.422509992056141925 ) ) ;
#20298 = UNCERTAINTY_MEASURE_WITH_UNIT (LENGTH_MEASURE( 1.000000000000000082E-05 ), #64498, 'distance_accuracy_value', 'NONE');
#20299 = ORIENTED_EDGE ( 'NONE', *, *, #58058, .F. ) ;
#20300 = CARTESIAN_POINT ( 'NONE',  ( -2.816281873526471635, 43.91530133659708923, -3.434112377981056508 ) ) ;
#20301 = DIRECTION ( 'NONE',  ( 0.000000000000000000, -1.000000000000000000, 0.000000000000000000 ) ) ;
#20302 = CARTESIAN_POINT ( 'NONE',  ( 20.88017736071110164, 60.35535201082151957, 2.915334737309930979 ) ) ;
#20303 = CARTESIAN_POINT ( 'NONE',  ( 0.6178305044545818747, 38.49863466993042493, -9.382169495545419124 ) ) ;
#20305 = CARTESIAN_POINT ( 'NONE',  ( 5.076628168052704559, 35.17559781766745175, -8.527530157486179263 ) ) ;
#20304 = CARTESIAN_POINT ( 'NONE',  ( -0.3689425029237898834, 56.17874883491396076, -10.36894250292378850 ) ) ;
#20306 = CARTESIAN_POINT ( 'NONE',  ( 4.084234479374312166, 0.000000000000000000, -3.613425430272927397 ) ) ;
#20307 = AXIS2_PLACEMENT_3D ( 'NONE', #77055, #67094, #90081 ) ;
#20308 = CARTESIAN_POINT ( 'NONE',  ( 5.076628168052703671, 61.84226448433412315, 8.527530157486179263 ) ) ;
#20309 = CARTESIAN_POINT ( 'NONE',  ( -4.164238869374099927, 17.01208216824730357, 3.795296366450308767 ) ) ;
#20310 = CARTESIAN_POINT ( 'NONE',  ( 2.917880565312950480, 35.97041550158063217, -12.26659068614894821 ) ) ;
#20311 = CARTESIAN_POINT ( 'NONE',  ( 19.84674366389459621, 43.50893115100078745, 7.409399052514197653E-17 ) ) ;
#20312 = CARTESIAN_POINT ( 'NONE',  ( -0.2538764795851958800, 70.00000000000000000, 6.092576751097361409 ) ) ;
#20313 = CARTESIAN_POINT ( 'NONE',  ( 19.42250999205614193, 35.14701867748816966, 5.440088680355555262 ) ) ;
#20314 = CARTESIAN_POINT ( 'NONE',  ( 15.44008868035555793, 56.39701867748817676, -9.422509992056140149 ) ) ;
#20315 = VECTOR ( 'NONE', #24559, 1000.000000000000000 ) ;
#20316 = CARTESIAN_POINT ( 'NONE',  ( 14.99999999999997868, 80.32179676972448590, 4.250000000000000000 ) ) ;
#20317 = EDGE_LOOP ( 'NONE', ( #90556, #65999, #49993, #92332 ) ) ;
#20318 = CARTESIAN_POINT ( 'NONE',  ( 13.43411237798106583, 42.66530133659707502, -12.81628187352647252 ) ) ;
#20319 = ORIENTED_EDGE ( 'NONE', *, *, #67059, .T. ) ;
#20320 = CARTESIAN_POINT ( 'NONE',  ( 18.52753015748617571, 3.092264484334118269, 4.923371831947298993 ) ) ;
#20321 = ORIENTED_EDGE ( 'NONE', *, *, #28594, .T. ) ;
#20322 = CARTESIAN_POINT ( 'NONE',  ( 10.00000000000000000, 0.5537488349139675359, -14.16423886937410082 ) ) ;
#20323 = CARTESIAN_POINT ( 'NONE',  ( 10.00000000000000000, 9.758931151000785675, -9.846743663894594434 ) ) ;
#20324 = EDGE_CURVE ( 'NONE', #12526, #33923, #53577, .T. ) ;
#20325 = AXIS2_PLACEMENT_3D ( 'NONE', #25419, #71405, #40416 ) ;
#20326 = CARTESIAN_POINT ( 'NONE',  ( 1.598469098248223030, 0.08731616080489693066, -6.289747708190945197 ) ) ;
#20327 = ORIENTED_EDGE ( 'NONE', *, *, #92769, .F. ) ;
#20328 = VECTOR ( 'NONE', #84015, 999.9999999999998863 ) ;
#20329 = CARTESIAN_POINT ( 'NONE',  ( 20.88017736071110875, 10.77201867748817143, -2.915334737309920765 ) ) ;
#20330 = CARTESIAN_POINT ( 'NONE',  ( -5.147851794455972296, 15.00000000000000533, 13.68970903997123401 ) ) ;
#20331 = CARTESIAN_POINT ( 'NONE',  ( 20.36894250292379382, 18.67874883491397142, 10.36894250292379205 ) ) ;
#20332 = CARTESIAN_POINT ( 'NONE',  ( 7.084665262690076126, 22.02201867748817321, -10.88017736071110164 ) ) ;
#20333 = CARTESIAN_POINT ( 'NONE',  ( 0.1532563361054100626, 65.80059781766745175, -2.638427012816831230 ) ) ;
#20334 = ORIENTED_EDGE ( 'NONE', *, *, #51018, .F. ) ;
#20335 = CARTESIAN_POINT ( 'NONE',  ( 12.63842701281683034, 57.46726448433411605, 9.846743663894596210 ) ) ;
#20336 = EDGE_LOOP ( 'NONE', ( #1928, #60541, #50574, #30774, #63581, #34978 ) ) ;
#20337 = CARTESIAN_POINT ( 'NONE',  ( 0.1532563361054100626, 0.8005978176674514168, -2.638427012816831230 ) ) ;
#20338 = CARTESIAN_POINT ( 'NONE',  ( 0.1532563361054083140, 61.00893115100078745, 1.131784320476157264E-15 ) ) ;
#20340 = PLANE ( 'NONE',  #67081 ) ;
#20339 = CARTESIAN_POINT ( 'NONE',  ( 17.96484262340118221, 11.18868534415483929, -7.964842623401177768 ) ) ;
#20341 = CARTESIAN_POINT ( 'NONE',  ( 12.91533473730993009, 66.60535201082150536, -10.88017736071109987 ) ) ;
#20342 = CARTESIAN_POINT ( 'NONE',  ( 10.00000000000000178, 19.31368534415484106, 10.88017736071110342 ) ) ;
#20343 = ORIENTED_EDGE ( 'NONE', *, *, #86509, .T. ) ;
#20344 = EDGE_CURVE ( 'NONE', #53120, #47516, #39955, .T. ) ;
#20345 = CARTESIAN_POINT ( 'NONE',  ( 13.43411237798105340, 60.58196800326376064, 12.81628187352647963 ) ) ;
#20346 = CARTESIAN_POINT ( 'NONE',  ( 2.035157376598824452, 28.68868534415484106, 7.964842623401179544 ) ) ;
#20347 = CARTESIAN_POINT ( 'NONE',  ( -46.94000000000001194, 100.5295635078804253, -8.861295791668675648 ) ) ;
#20348 = CARTESIAN_POINT ( 'NONE',  ( 10.00000000000000178, 45.37363466993041783, 12.81628187352647608 ) ) ;
#20349 = CARTESIAN_POINT ( 'NONE',  ( 10.00000000000000178, 54.31368534415484106, 10.88017736071110342 ) ) ;
#20350 = PRESENTATION_LAYER_ASSIGNMENT (  '', '', ( #65001 ) ) ;
#20351 = CARTESIAN_POINT ( 'NONE',  ( 14.92337183194729988, 54.34226448433412315, -8.527530157486177487 ) ) ;
#20352 = ORIENTED_EDGE ( 'NONE', *, *, #6684, .T. ) ;
#20353 = CARTESIAN_POINT ( 'NONE',  ( 19.84674366389459266, 18.71726448433411960, -2.638427012816827677 ) ) ;
#20354 = CARTESIAN_POINT ( 'NONE',  ( 6.565887622018943937, 5.165301336597086568, 12.81628187352647430 ) ) ;
#20356 = CARTESIAN_POINT ( 'NONE',  ( 14.92337183194729988, 54.34226448433412315, -8.527530157486177487 ) ) ;
#20355 = CARTESIAN_POINT ( 'NONE',  ( 18.17884179759847996, 3.666888798595233645, -6.499999999999976019 ) ) ;
#20357 = CARTESIAN_POINT ( 'NONE',  ( 19.42250999205614193, 25.14701867748817321, 5.440088680355555262 ) ) ;
#20358 = CARTESIAN_POINT ( 'NONE',  ( 1.472469842513823179, 51.42559781766745886, 4.923371831947296329 ) ) ;
#20359 = DIRECTION ( 'NONE',  ( -1.000000000000000000, -0.000000000000000000, -0.000000000000000000 ) ) ;
#20360 = CARTESIAN_POINT ( 'NONE',  ( 0.000000000000000000, 15.00000000000000000, 0.000000000000000000 ) ) ;
#20361 = AXIS2_PLACEMENT_3D ( 'NONE', #98118, #68103, #66613 ) ;
#20362 = CARTESIAN_POINT ( 'NONE',  ( 19.84674366389459621, 8.508931151000785675, 7.409399052514197653E-17 ) ) ;
#20363 = PLANE ( 'NONE',  #88834 ) ;
#20365 = ORIENTED_EDGE ( 'NONE', *, *, #51664, .T. ) ;
#20364 = CARTESIAN_POINT ( 'NONE',  ( 13.43411237798105340, 0.5819680032637533085, 12.81628187352647963 ) ) ;
#20366 = TOROIDAL_SURFACE ( 'NONE', #76258, 14.49999999999999822, 0.5000000000000000000 ) ;
#20367 = CARTESIAN_POINT ( 'NONE',  ( 3.591859063236761518, 64.95696800326376774, 11.09922568453594849 ) ) ;
#20368 = CARTESIAN_POINT ( 'NONE',  ( -10.93781366033333136, 0.5000000000000004441, -10.26470809774080628 ) ) ;
#20369 = CARTESIAN_POINT ( 'NONE',  ( 19.38216949554541202, 35.99863466993041072, 9.382169495545424454 ) ) ;
#20370 = CARTESIAN_POINT ( 'NONE',  ( 17.20831665107776587, 34.13393115100078745, -7.208316651077762316 ) ) ;
#20371 = LINE ( 'NONE', #81357, #72808 ) ;
#20372 = CARTESIAN_POINT ( 'NONE',  ( -2.266590686148945544, 61.38708216824730357, -7.082119434687050408 ) ) ;
#20373 = CARTESIAN_POINT ( 'NONE',  ( 12.63842701281683034, 27.46726448433411250, 9.846743663894596210 ) ) ;
#20374 = CARTESIAN_POINT ( 'NONE',  ( -0.3289641300568005855, 39.27164270246084499, -5.963430220938281678 ) ) ;
#20375 = CARTESIAN_POINT ( 'NONE',  ( 10.00000000000000000, 60.55374883491397497, -14.16423886937410082 ) ) ;
#20376 = CARTESIAN_POINT ( 'NONE',  ( 13.99999999999999822, 60.50000000000000711, -6.500000000000000888 ) ) ;
#20377 = CARTESIAN_POINT ( 'NONE',  ( 7.084665262690076126, 22.02201867748817321, -10.88017736071110164 ) ) ;
#20379 = VECTOR ( 'NONE', #41250, 1000.000000000000114 ) ;
#20378 = CARTESIAN_POINT ( 'NONE',  ( -2.266590686148945544, 32.22041550158063927, 7.082119434687048631 ) ) ;
#20381 = DIRECTION ( 'NONE',  ( -0.7604059656000340395, 0.000000000000000000, 0.6494480483301799945 ) ) ;
#20380 = CARTESIAN_POINT ( 'NONE',  ( 2.917880565312948704, 57.63708216824731068, 12.26659068614894643 ) ) ;
#20382 = CARTESIAN_POINT ( 'NONE',  ( 7.618303901329630534, 14.99999999999807798, 12.48478900416944803 ) ) ;
#20383 = ADVANCED_FACE ( 'NONE', ( #84610 ), #54584, .F. ) ;
#20384 = CARTESIAN_POINT ( 'NONE',  ( 5.076628168052703671, 6.842264484334118713, 8.527530157486179263 ) ) ;
#20385 = CARTESIAN_POINT ( 'NONE',  ( 19.84674366389459266, 63.71726448433412315, -2.638427012816827677 ) ) ;
#20386 = CARTESIAN_POINT ( 'NONE',  ( 18.39792806157249672, 14.52224192338640663, 6.500000000000000888 ) ) ;
#20387 = VERTEX_POINT ( 'NONE', #83626 ) ;
#20388 = CARTESIAN_POINT ( 'NONE',  ( 12.91533473730993009, 56.60535201082151247, -10.88017736071109987 ) ) ;
#20389 = CARTESIAN_POINT ( 'NONE',  ( 8.629999999999995453, 40.74999999999999289, -4.250000000000000000 ) ) ;
#20390 = EDGE_CURVE ( 'NONE', #52732, #22085, #30379, .T. ) ;
#20392 = DIRECTION ( 'NONE',  ( -0.000000000000000000, -1.000000000000000000, -0.000000000000000000 ) ) ;
#20391 = VECTOR ( 'NONE', #91206, 1000.000000000000000 ) ;
#20393 = CIRCLE ( 'NONE', #41109, 0.2500000000000002220 ) ;
#20394 = CARTESIAN_POINT ( 'NONE',  ( 12.30000000000000249, 99.99999999999998579, -8.525133428036873795 ) ) ;
#20395 = FACE_OUTER_BOUND ( 'NONE', #95214, .T. ) ;
#20396 = ORIENTED_EDGE ( 'NONE', *, *, #34208, .T. ) ;
#20397 = CARTESIAN_POINT ( 'NONE',  ( -4.164238869374099039, 46.80374883491397497, 8.674139862899312516E-16 ) ) ;
#20398 = SURFACE_STYLE_USAGE ( .BOTH. , #65383 ) ;
#20400 = CARTESIAN_POINT ( 'NONE',  ( -9.742785792574931492, 8.338468844518212464, 5.625000000000008882 ) ) ;
#20399 = CARTESIAN_POINT ( 'NONE',  ( -7.124975165218884854, -78.82169502743931844, -2.500000000000000000 ) ) ;
#20401 = CARTESIAN_POINT ( 'NONE',  ( 15.44008868035555260, 14.73035201082150536, 9.422509992056143702 ) ) ;
#20402 = CARTESIAN_POINT ( 'NONE',  ( 3.591859063236763294, 33.29030133659708213, -11.09922568453595026 ) ) ;
#20403 = CARTESIAN_POINT ( 'NONE',  ( -5.963430220938278126, 10.52164270246084499, 10.32896413005680358 ) ) ;
#20404 = CARTESIAN_POINT ( 'NONE',  ( -2.816281873526471635, 18.91530133659708213, -3.434112377981056508 ) ) ;
#20405 = CARTESIAN_POINT ( 'NONE',  ( 6.565887622018943937, 65.16530133659709634, 12.81628187352647430 ) ) ;
#20406 = ORIENTED_EDGE ( 'NONE', *, *, #69340, .F. ) ;
#20407 = CARTESIAN_POINT ( 'NONE',  ( 10.64017930668206446, 0.3640475087720991820, -10.57291749337215769 ) ) ;
#20408 = CARTESIAN_POINT ( 'NONE',  ( -11.37644997956084936, -81.99697149678695496, -4.000000000000000888 ) ) ;
#20409 = CARTESIAN_POINT ( 'NONE',  ( -2.266590686148945544, 26.38708216824730357, -7.082119434687050408 ) ) ;
#20410 =( NAMED_UNIT ( * ) SI_UNIT ( $, .STERADIAN. ) SOLID_ANGLE_UNIT ( ) );
#20411 = CARTESIAN_POINT ( 'NONE',  ( -3.836041483939800933, -2.701055130266049265, 4.000000000000000000 ) ) ;
#20412 = CARTESIAN_POINT ( 'NONE',  ( 10.00000000000000000, 21.81368534415484106, -10.88017736071110342 ) ) ;
#20413 = DIRECTION ( 'NONE',  ( 0.000000000000000000, 0.000000000000000000, -1.000000000000000000 ) ) ;
#20414 = CARTESIAN_POINT ( 'NONE',  ( 1.548803529118027100, 0.000000000000000000, -5.228673087012095877 ) ) ;
#20415 = CARTESIAN_POINT ( 'NONE',  ( 20.88017736071110519, 50.56368534415484106, 2.639326808657452039E-16 ) ) ;
#20416 = CARTESIAN_POINT ( 'NONE',  ( 15.44008868035555793, 46.39701867748817676, -9.422509992056140149 ) ) ;
#20417 = CARTESIAN_POINT ( 'NONE',  ( 6.565887622018943937, 15.16530133659708568, 12.81628187352647430 ) ) ;
#20418 = DIRECTION ( 'NONE',  ( 0.000000000000000000, 0.000000000000000000, 1.000000000000000000 ) ) ;
#20419 = CARTESIAN_POINT ( 'NONE',  ( -0.8801773607111009756, 3.272018677488171434, 2.915334737309923874 ) ) ;
#20420 = CARTESIAN_POINT ( 'NONE',  ( 19.84674366389459621, 18.50893115100078745, 7.409399052514197653E-17 ) ) ;
#20421 = DIRECTION ( 'NONE',  ( -1.000000000000000000, 0.000000000000000000, -0.000000000000000000 ) ) ;
#20422 = CARTESIAN_POINT ( 'NONE',  ( 0.5774900079438607392, 43.48035201082151247, 5.440088680355550821 ) ) ;
#20423 = CARTESIAN_POINT ( 'NONE',  ( 0.6178305044545838731, 4.748634669930420493, 9.382169495545420901 ) ) ;
#20424 = CARTESIAN_POINT ( 'NONE',  ( 12.63842701281683034, 27.46726448433411250, 9.846743663894596210 ) ) ;
#20425 = CARTESIAN_POINT ( 'NONE',  ( 0.6178305044545818747, 53.49863466993041072, -9.382169495545419124 ) ) ;
#20426 = CARTESIAN_POINT ( 'NONE',  ( 4.559911319644449179, 68.89701867748817676, 9.422509992056141925 ) ) ;
#20427 = ORIENTED_EDGE ( 'NONE', *, *, #36389, .F. ) ;
#20428 = DIRECTION ( 'NONE',  ( -0.000000000000000000, 0.000000000000000000, 1.000000000000000000 ) ) ;
#20429 = CARTESIAN_POINT ( 'NONE',  ( 1.472469842513823179, 36.42559781766745175, 4.923371831947296329 ) ) ;
#20430 = CARTESIAN_POINT ( 'NONE',  ( 17.96484262340118221, 16.18868534415483396, -7.964842623401177768 ) ) ;
#20432 = CARTESIAN_POINT ( 'NONE',  ( 20.36894250292379738, 29.92874883491396432, -10.36894250292379027 ) ) ;
#20431 = CARTESIAN_POINT ( 'NONE',  ( 11.81378540890930751, 0.000000000000000000, 7.968498874458199488 ) ) ;
#20433 = CARTESIAN_POINT ( 'NONE',  ( 0.1532563361054082862, 31.21726448433412315, 2.638427012816831674 ) ) ;
#20434 = CARTESIAN_POINT ( 'NONE',  ( 10.00000000000000000, 16.81368534415483751, -10.88017736071110342 ) ) ;
#20435 = CARTESIAN_POINT ( 'NONE',  ( -4.164238869374099039, 66.80374883491396076, 8.674139862899312516E-16 ) ) ;
#20436 = ORIENTED_EDGE ( 'NONE', *, *, #84695, .F. ) ;
#20437 = CARTESIAN_POINT ( 'NONE',  ( 7.084665262690076126, 32.02201867748816966, -10.88017736071110164 ) ) ;
#20438 = EDGE_CURVE ( 'NONE', #23897, #74408, #50042, .T. ) ;
#20439 = CARTESIAN_POINT ( 'NONE',  ( 17.96484262340118221, 29.93868534415484106, 7.964842623401181321 ) ) ;
#20441 = CARTESIAN_POINT ( 'NONE',  ( 0.5774900079438607392, 43.48035201082151247, 5.440088680355550821 ) ) ;
#20440 = CARTESIAN_POINT ( 'NONE',  ( -5.419894505350399072, 14.63595249122790598, -13.98659156302466222 ) ) ;
#20442 = ORIENTED_EDGE ( 'NONE', *, *, #67066, .T. ) ;
#20443 = CARTESIAN_POINT ( 'NONE',  ( 17.20831665107776587, 62.88393115100078745, 7.208316651077764980 ) ) ;
#20444 = CARTESIAN_POINT ( 'NONE',  ( 7.084665262690076126, 32.02201867748816966, -10.88017736071110164 ) ) ;
#20445 = CARTESIAN_POINT ( 'NONE',  ( 2.062412797813223616E-17, 1.639999999999999014, 0.000000000000000000 ) ) ;
#20446 = CARTESIAN_POINT ( 'NONE',  ( -1.099225684535947600, 63.70696800326376774, -6.408140936763238038 ) ) ;
#20447 = DIRECTION ( 'NONE',  ( -0.000000000000000000, 1.000000000000000000, 0.000000000000000000 ) ) ;
#20448 = CARTESIAN_POINT ( 'NONE',  ( 6.204703633549690345, 32.84541550158063927, 14.16423886937410082 ) ) ;
#20449 = CARTESIAN_POINT ( 'NONE',  ( 17.96484262340118221, 54.93868534415484106, 7.964842623401181321 ) ) ;
#20450 = ADVANCED_FACE ( 'NONE', ( #16608 ), #63074, .F. ) ;
#20451 = CARTESIAN_POINT ( 'NONE',  ( 19.80427997160309417, 42.75733960839543357, -6.499999999999988454 ) ) ;
#20452 = DIRECTION ( 'NONE',  ( 0.000000000000000000, 0.000000000000000000, 1.000000000000000000 ) ) ;
#20453 = CARTESIAN_POINT ( 'NONE',  ( 1.472469842513823179, 45.59226448433412315, -4.923371831947296329 ) ) ;
#20454 = VERTEX_POINT ( 'NONE', #78086 ) ;
#20455 = CARTESIAN_POINT ( 'NONE',  ( 14.92337183194729988, 24.34226448433411960, -8.527530157486177487 ) ) ;
#20456 = CARTESIAN_POINT ( 'NONE',  ( 12.81628187352647608, -13.58469866340290899, 3.434112377981052511 ) ) ;
#20457 = CIRCLE ( 'NONE', #90747, 0.1000000000000001166 ) ;
#20458 = CARTESIAN_POINT ( 'NONE',  ( 0.5774900079438607392, 8.480352010821505360, 5.440088680355550821 ) ) ;
#20459 = CARTESIAN_POINT ( 'NONE',  ( 10.00000000000000000, 24.75893115100078745, -9.846743663894594434 ) ) ;
#20460 = CARTESIAN_POINT ( 'NONE',  ( 21.09922568453595559, 7.040301336597086568, -6.408140936763230044 ) ) ;
#20462 = CARTESIAN_POINT ( 'NONE',  ( 4.559911319644449179, 52.23035201082151247, -9.422509992056141925 ) ) ;
#20461 = CARTESIAN_POINT ( 'NONE',  ( 19.42250999205614548, 55.98035201082150536, -5.440088680355545492 ) ) ;
#20464 = CARTESIAN_POINT ( 'NONE',  ( 10.00000000000000178, 55.37363466993042493, 12.81628187352647608 ) ) ;
#20463 = CARTESIAN_POINT ( 'NONE',  ( 20.88017736071110519, 35.56368534415484106, 2.639326808657452039E-16 ) ) ;
#20465 = CARTESIAN_POINT ( 'NONE',  ( 22.26659068614895176, 49.72041550158063927, -7.082119434687042414 ) ) ;
#20466 = CIRCLE ( 'NONE', #30015, 1.249999999999987121 ) ;
#20467 = EDGE_CURVE ( 'NONE', #1194, #35951, #49498, .T. ) ;
#20468 = CARTESIAN_POINT ( 'NONE',  ( -12.98685442714204008, 4.660809545892429844E-16, 6.449155920600864178 ) ) ;
#20469 = ORIENTED_EDGE ( 'NONE', *, *, #56988, .T. ) ;
#20470 = CARTESIAN_POINT ( 'NONE',  ( 10.00000000000000178, 67.25893115100079456, 9.846743663894594434 ) ) ;
#20471 = CARTESIAN_POINT ( 'NONE',  ( 7.084665262690076126, 2.022018677488170990, -10.88017736071110164 ) ) ;
#20472 = CARTESIAN_POINT ( 'NONE',  ( 15.44008868035555260, 44.73035201082151247, 9.422509992056143702 ) ) ;
#20474 = EDGE_CURVE ( 'NONE', #42599, #40639, #32012, .T. ) ;
#20473 = CARTESIAN_POINT ( 'NONE',  ( 2.791683348922240793, 61.63393115100079456, 7.208316651077764092 ) ) ;
#20475 = ORIENTED_EDGE ( 'NONE', *, *, #4415, .T. ) ;
#20476 = CARTESIAN_POINT ( 'NONE',  ( 14.92337183194729988, 14.34226448433411782, -8.527530157486177487 ) ) ;
#20477 = CARTESIAN_POINT ( 'NONE',  ( -5.204170427930421283E-15, 8.438309369127518167, -11.92686044187656513 ) ) ;
#20478 = CARTESIAN_POINT ( 'NONE',  ( 17.20831665107776587, 12.88393115100078390, 7.208316651077764980 ) ) ;
#20479 = CARTESIAN_POINT ( 'NONE',  ( 10.00000000000000178, 22.25893115100078745, 9.846743663894594434 ) ) ;
#20480 = CARTESIAN_POINT ( 'NONE',  ( 19.84674366389459266, 13.30059781766745353, 2.638427012816836559 ) ) ;
#20481 = CARTESIAN_POINT ( 'NONE',  ( -6.874974626955391521, -78.82095024088569346, 2.500000000000000000 ) ) ;
#20483 = DIRECTION ( 'NONE',  ( 0.4924235601034648302, 0.000000000000000000, 0.8703556959399010307 ) ) ;
#20482 = CARTESIAN_POINT ( 'NONE',  ( 7.361572987183170547, 7.050597817667451750, 9.846743663894590881 ) ) ;
#20484 = CARTESIAN_POINT ( 'NONE',  ( 17.20831665107776587, 2.883931151000785231, 7.208316651077764980 ) ) ;
#20486 = ORIENTED_EDGE ( 'NONE', *, *, #13094, .F. ) ;
#20485 = CARTESIAN_POINT ( 'NONE',  ( 18.52753015748617571, 18.09226448433411960, 4.923371831947298993 ) ) ;
#20487 = DIRECTION ( 'NONE',  ( 0.000000000000000000, 1.000000000000000000, 0.000000000000000000 ) ) ;
#20488 = CARTESIAN_POINT ( 'NONE',  ( 14.92337183194729988, 64.34226448433412315, -8.527530157486177487 ) ) ;
#20489 = VERTEX_POINT ( 'NONE', #7646 ) ;
#20490 = DIRECTION ( 'NONE',  ( 0.000000000000000000, 1.000000000000000000, 0.000000000000000000 ) ) ;
#20491 = CARTESIAN_POINT ( 'NONE',  ( -4.164238869374099927, 17.01208216824730357, 3.795296366450308767 ) ) ;
#20492 = UNCERTAINTY_MEASURE_WITH_UNIT (LENGTH_MEASURE( 1.000000000000000082E-05 ), #9055, 'distance_accuracy_value', 'NONE');
#20493 = CARTESIAN_POINT ( 'NONE',  ( -2.266590686148945544, 22.22041550158063572, 7.082119434687048631 ) ) ;
#20494 = CARTESIAN_POINT ( 'NONE',  ( -4.164238869374099039, 46.80374883491397497, 8.674139862899312516E-16 ) ) ;
#20495 =( NAMED_UNIT ( * ) SI_UNIT ( $, .STERADIAN. ) SOLID_ANGLE_UNIT ( ) );
#20497 = CARTESIAN_POINT ( 'NONE',  ( 4.559911319644449179, 67.23035201082150536, -9.422509992056141925 ) ) ;
#20496 = CARTESIAN_POINT ( 'NONE',  ( 6.204703633549690345, 12.84541550158063572, 14.16423886937410082 ) ) ;
#20498 = CARTESIAN_POINT ( 'NONE',  ( 7.084665262690076126, 34.10535201082151247, 10.88017736071109987 ) ) ;
#20499 = CARTESIAN_POINT ( 'NONE',  ( -11.62719953690072217, 14.63595249122789177, 9.476720473301721626 ) ) ;
#20500 = AXIS2_PLACEMENT_3D ( 'NONE', #27276, #65767, #26790 ) ;
#20501 = VERTEX_POINT ( 'NONE', #40093 ) ;
#20502 = CARTESIAN_POINT ( 'NONE',  ( 0.1532563361054083140, 11.00893115100078568, 1.131784320476157264E-15 ) ) ;
#20504 = CARTESIAN_POINT ( 'NONE',  ( 14.92337183194729988, 29.34226448433411960, -8.527530157486177487 ) ) ;
#20503 = CARTESIAN_POINT ( 'NONE',  ( 19.42250999205614193, 50.14701867748817676, 5.440088680355555262 ) ) ;
#20505 = CARTESIAN_POINT ( 'NONE',  ( 12.91533473730992121, 9.522018677488171434, 10.88017736071110164 ) ) ;
#20506 = CARTESIAN_POINT ( 'NONE',  ( -2.816281873526471635, 63.91530133659708923, -3.434112377981056508 ) ) ;
#20507 = CARTESIAN_POINT ( 'NONE',  ( 14.92337183194729988, 44.34226448433412315, -8.527530157486177487 ) ) ;
#20508 = CARTESIAN_POINT ( 'NONE',  ( 0.000000000000000000, 14.49999999999999822, 0.000000000000000000 ) ) ;
#20509 = ADVANCED_FACE ( 'NONE', ( #9590 ), #70593, .T. ) ;
#20510 = CARTESIAN_POINT ( 'NONE',  ( 6.565887622018943937, 40.16530133659708923, 12.81628187352647430 ) ) ;
#20511 = CARTESIAN_POINT ( 'NONE',  ( -12.26659068614895354, -23.61291783175269643, -7.082119434687038861 ) ) ;
#20512 = CARTESIAN_POINT ( 'NONE',  ( 2.035157376598822676, 47.43868534415484817, -7.964842623401177768 ) ) ;
#20513 = CARTESIAN_POINT ( 'NONE',  ( 2.791683348922240793, 36.63393115100078035, 7.208316651077764092 ) ) ;
#20514 = CARTESIAN_POINT ( 'NONE',  ( 13.79529636645030344, 33.26208216824730357, 14.16423886937410614 ) ) ;
#20515 = VERTEX_POINT ( 'NONE', #38137 ) ;
#20516 = DIRECTION ( 'NONE',  ( -1.000000000000000000, 0.000000000000000000, 0.000000000000000000 ) ) ;
#20517 = CARTESIAN_POINT ( 'NONE',  ( 15.44008868035555793, 51.39701867748816966, -9.422509992056140149 ) ) ;
#20518 = CARTESIAN_POINT ( 'NONE',  ( 15.44008868035555793, 66.39701867748817676, -9.422509992056140149 ) ) ;
#20519 = CARTESIAN_POINT ( 'NONE',  ( 17.08211943468705840, 45.13708216824730357, -12.26659068614894466 ) ) ;
#20520 = CARTESIAN_POINT ( 'NONE',  ( 3.591859063236763294, -1.709698663402913210, -11.09922568453595026 ) ) ;
#20521 = CARTESIAN_POINT ( 'NONE',  ( 14.36343418943210892, 14.95077488074853456, 3.367173657400750031 ) ) ;
#20522 = CARTESIAN_POINT ( 'NONE',  ( 12.91533473730993009, 41.60535201082149825, -10.88017736071109987 ) ) ;
#20523 = CARTESIAN_POINT ( 'NONE',  ( -6.874984555098657246, -78.81798443069058635, -2.499999999999999112 ) ) ;
#20524 = STYLED_ITEM ( 'NONE', ( #54422 ), #13803 ) ;
#20525 = CARTESIAN_POINT ( 'NONE',  ( 13.43411237798106583, 22.66530133659708923, -12.81628187352647252 ) ) ;
#20526 = CARTESIAN_POINT ( 'NONE',  ( 19.84674366389459266, 48.71726448433413026, -2.638427012816827677 ) ) ;
#20527 = CARTESIAN_POINT ( 'NONE',  ( 9.422509992056141925, 15.98035201082151424, -5.440088680355554374 ) ) ;
#20528 =( NAMED_UNIT ( * ) SI_UNIT ( $, .STERADIAN. ) SOLID_ANGLE_UNIT ( ) );
#20529 = CARTESIAN_POINT ( 'NONE',  ( 7.084665262690076126, 17.02201867748817676, -10.88017736071110164 ) ) ;
#20530 = DIRECTION ( 'NONE',  ( 0.5948227867513480316, 0.000000000000000000, -0.8038568606172125097 ) ) ;
#20531 = EDGE_LOOP ( 'NONE', ( #44330, #10130, #35029, #69999 ) ) ;
#20532 = VECTOR ( 'NONE', #7779, 1000.000000000000000 ) ;
#20533 = CARTESIAN_POINT ( 'NONE',  ( 15.44008868035555260, 4.730352010821504471, 9.422509992056143702 ) ) ;
#20534 = PRESENTATION_STYLE_ASSIGNMENT (( #43031 ) ) ;
#20535 = COLOUR_RGB ( '', 0.31764706, 0.68627451, 0.89019608) ;
#20536 = CARTESIAN_POINT ( 'NONE',  ( 7.361572987183170547, 2.050597817667451750, 9.846743663894590881 ) ) ;
#20537 = CARTESIAN_POINT ( 'NONE',  ( 19.84674366389459266, 3.300597817667451750, 2.638427012816836559 ) ) ;
#20538 = CARTESIAN_POINT ( 'NONE',  ( 19.84674366389459266, 33.30059781766744464, 2.638427012816836559 ) ) ;
#20539 = CARTESIAN_POINT ( 'NONE',  ( 15.44008868035555260, 24.73035201082150891, 9.422509992056143702 ) ) ;
#20540 = CARTESIAN_POINT ( 'NONE',  ( -2.816281873526471635, 3.915301336597087456, -3.434112377981056508 ) ) ;
#20542 = CARTESIAN_POINT ( 'NONE',  ( -1.780824192092587577, 14.49999999999999112, 14.89391369643518637 ) ) ;
#20541 = CARTESIAN_POINT ( 'NONE',  ( 20.88017736071110875, 40.77201867748818387, -2.915334737309920765 ) ) ;
#20543 = LINE ( 'NONE', #88038, #3410 ) ;
#20544 = CARTESIAN_POINT ( 'NONE',  ( 10.00000000000000178, 40.37363466993042493, 12.81628187352647608 ) ) ;
#20545 = ORIENTED_EDGE ( 'NONE', *, *, #18000, .F. ) ;
#20546 = CARTESIAN_POINT ( 'NONE',  ( 19.42250999205614193, 60.14701867748817676, 5.440088680355555262 ) ) ;
#20548 = CARTESIAN_POINT ( 'NONE',  ( 17.08211943468705130, 3.470415501580634388, 12.26659068614894998 ) ) ;
#20547 = CARTESIAN_POINT ( 'NONE',  ( 3.591859063236761518, 14.95696800326375531, 11.09922568453594849 ) ) ;
#20549 = CARTESIAN_POINT ( 'NONE',  ( 7.361572987183169658, -0.03273551566588185635, -9.846743663894592657 ) ) ;
#20550 = CARTESIAN_POINT ( 'NONE',  ( 2.035157376598822676, 37.43868534415484106, -7.964842623401177768 ) ) ;
#20551 = CARTESIAN_POINT ( 'NONE',  ( -15.67879934938584263, -0.03417435944610275333, 3.170591017105712339 ) ) ;
#20552 = CARTESIAN_POINT ( 'NONE',  ( 10.00000000000000178, 68.05374883491397497, 14.16423886937410082 ) ) ;
#20553 = CARTESIAN_POINT ( 'NONE',  ( 0.1532563361054100626, 50.80059781766745175, -2.638427012816831230 ) ) ;
#20554 = CARTESIAN_POINT ( 'NONE',  ( 7.361572987183169658, -0.03273551566588185635, -9.846743663894592657 ) ) ;
#20555 = CARTESIAN_POINT ( 'NONE',  ( 0.5774900079438607392, 63.48035201082149825, 5.440088680355550821 ) ) ;
#20556 = DIRECTION ( 'NONE',  ( 0.000000000000000000, 0.000000000000000000, -1.000000000000000000 ) ) ;
#20557 = CARTESIAN_POINT ( 'NONE',  ( -2.266590686148945544, 27.22041550158063572, 7.082119434687048631 ) ) ;
#20558 = CARTESIAN_POINT ( 'NONE',  ( 9.209947446681445271, -9.314274491706216352, -3.750000000000000444 ) ) ;
#20559 = CARTESIAN_POINT ( 'NONE',  ( 19.50000000000000355, 79.40087001978915282, -5.000000000000000000 ) ) ;
#20560 = VERTEX_POINT ( 'NONE', #8122 ) ;
#20561 = ORIENTED_EDGE ( 'NONE', *, *, #25638, .F. ) ;
#20562 = CARTESIAN_POINT ( 'NONE',  ( 13.79529636645030344, 63.26208216824730357, 14.16423886937410614 ) ) ;
#20563 = CARTESIAN_POINT ( 'NONE',  ( 17.08211943468705840, 50.13708216824730357, -12.26659068614894466 ) ) ;
#20564 = CARTESIAN_POINT ( 'NONE',  ( 0.1532563361054083140, 26.00893115100078745, 1.131784320476157264E-15 ) ) ;
#20565 = B_SPLINE_CURVE_WITH_KNOTS ( 'NONE', 3,
 ( #78679, #33159, #86673, #47178 ),
 .UNSPECIFIED., .F., .F.,
 ( 4, 4 ),
 ( 1.084202172485504434E-19, 0.002657014572711316382 ),
 .UNSPECIFIED. ) ;
#20566 = CARTESIAN_POINT ( 'NONE',  ( 10.00000000000000000, 27.87363466993042138, -12.81628187352647608 ) ) ;
#20567 = CARTESIAN_POINT ( 'NONE',  ( -12.00809552683946357, 14.49999999999999822, -8.989195838243713155 ) ) ;
#20568 = CARTESIAN_POINT ( 'NONE',  ( -12.60589901313233874, 14.49999999999999112, 8.129656208641975468 ) ) ;
#20569 = CARTESIAN_POINT ( 'NONE',  ( 0.5774900079438590739, 7.647018677488171434, -5.440088680355550821 ) ) ;
#20570 = CARTESIAN_POINT ( 'NONE',  ( 24.16423886937410614, 54.30374883491396787, 8.672049930838204340E-16 ) ) ;
#20571 = ADVANCED_FACE ( 'NONE', ( #68624 ), #75066, .T. ) ;
#20572 = ADVANCED_FACE ( 'NONE', ( #30603 ), #65528, .T. ) ;
#20573 = CARTESIAN_POINT ( 'NONE',  ( 5.076628168052703671, 26.84226448433411960, 8.527530157486179263 ) ) ;
#20574 = CARTESIAN_POINT ( 'NONE',  ( -14.71525861348295017, 0.3639310978437778066, 2.908807992686501809 ) ) ;
#20575 = CARTESIAN_POINT ( 'NONE',  ( 12.63842701281683034, 7.467264484334118713, 9.846743663894596210 ) ) ;
#20576 = CARTESIAN_POINT ( 'NONE',  ( 20.15039907845754286, 14.72266099184918531, 6.262539305110064625 ) ) ;
#20577 = CARTESIAN_POINT ( 'NONE',  ( 2.638427012816829897, 4.550597817667449974, -9.846743663894592657 ) ) ;
#20578 = ORIENTED_EDGE ( 'NONE', *, *, #2813, .T. ) ;
#20579 = ORIENTED_EDGE ( 'NONE', *, *, #55220, .T. ) ;
#20580 = ORIENTED_EDGE ( 'NONE', *, *, #43120, .F. ) ;
#20581 = CARTESIAN_POINT ( 'NONE',  ( 24.16423886937409904, 14.09541550158063217, 3.795296366450317205 ) ) ;
#20583 = CARTESIAN_POINT ( 'NONE',  ( 20.88017736071110519, 25.56368534415483751, 2.639326808657452039E-16 ) ) ;
#20582 = CARTESIAN_POINT ( 'NONE',  ( 7.084665262690076126, 22.02201867748817321, -10.88017736071110164 ) ) ;
#20585 = CARTESIAN_POINT ( 'NONE',  ( 21.09922568453595559, 12.04030133659708746, -6.408140936763230044 ) ) ;
#20584 = CARTESIAN_POINT ( 'NONE',  ( 19.84674366389459266, 48.71726448433413026, -2.638427012816827677 ) ) ;
#20586 = CARTESIAN_POINT ( 'NONE',  ( 10.00000000000000178, 3.053748834913967425, 14.16423886937410082 ) ) ;
#20587 = CARTESIAN_POINT ( 'NONE',  ( 16.40814093676323893, 25.79030133659708923, 11.09922568453595026 ) ) ;
#20589 = ORIENTED_EDGE ( 'NONE', *, *, #43226, .T. ) ;
#20588 =( NAMED_UNIT ( * ) SI_UNIT ( $, .STERADIAN. ) SOLID_ANGLE_UNIT ( ) );
#20590 = CARTESIAN_POINT ( 'NONE',  ( 19.84674366389459266, 28.30059781766745886, 2.638427012816836559 ) ) ;
#20591 = CARTESIAN_POINT ( 'NONE',  ( 10.00000000000000000, 55.55374883491396787, -14.16423886937410082 ) ) ;
#20592 = ORIENTED_EDGE ( 'NONE', *, *, #17668, .F. ) ;
#20593 = EDGE_CURVE ( 'NONE', #91503, #21162, #97711, .T. ) ;
#20594 = CARTESIAN_POINT ( 'NONE',  ( 6.204703633549690345, 67.84541550158060375, 14.16423886937410082 ) ) ;
#20595 = ORIENTED_EDGE ( 'NONE', *, *, #98732, .F. ) ;
#20596 = CARTESIAN_POINT ( 'NONE',  ( 20.88017736071110519, 45.56368534415484106, 2.639326808657452039E-16 ) ) ;
#20597 = CARTESIAN_POINT ( 'NONE',  ( 0.5774900079438607392, 48.48035201082150536, 5.440088680355550821 ) ) ;
#20598 =( GEOMETRIC_REPRESENTATION_CONTEXT ( 3 ) GLOBAL_UNCERTAINTY_ASSIGNED_CONTEXT ( ( #24234 ) ) GLOBAL_UNIT_ASSIGNED_CONTEXT ( ( #60767, #53269, #67795 ) ) REPRESENTATION_CONTEXT ( 'NONE', 'WORKASPACE' ) );
#20599 = CARTESIAN_POINT ( 'NONE',  ( 17.96484262340118221, 54.93868534415484106, 7.964842623401181321 ) ) ;
#20600 = CARTESIAN_POINT ( 'NONE',  ( 4.559911319644449179, 37.23035201082150536, -9.422509992056141925 ) ) ;
#20601 = VECTOR ( 'NONE', #71125, 1000.000000000000114 ) ;
#20602 = AXIS2_PLACEMENT_3D ( 'NONE', #6928, #82919, #96966 ) ;
#20604 = VERTEX_POINT ( 'NONE', #87551 ) ;
#20603 = DIRECTION ( 'NONE',  ( -0.3007057995042635712, 0.000000000000000000, -0.9537169507482300412 ) ) ;
#20605 = CARTESIAN_POINT ( 'NONE',  ( 5.076628168052703671, 26.84226448433411960, 8.527530157486179263 ) ) ;
#20606 = VERTEX_POINT ( 'NONE', #33551 ) ;
#20607 = CARTESIAN_POINT ( 'NONE',  ( 12.63842701281683034, 52.46726448433413026, 9.846743663894596210 ) ) ;
#20608 = B_SPLINE_CURVE_WITH_KNOTS ( 'NONE', 3,
 ( #45877, #15875, #91863, #7393, #23381, #54340 ),
 .UNSPECIFIED., .F., .F.,
 ( 4, 2, 4 ),
 ( 3.409110551494648722E-05, 0.0004400426677367932937, 0.0008459942299586401069 ),
 .UNSPECIFIED. ) ;
#20609 = CARTESIAN_POINT ( 'NONE',  ( -0.03743638938522729498, 24.25197528031018734, -6.399506433553966644 ) ) ;
#20610 = CARTESIAN_POINT ( 'NONE',  ( 13.79529636645031943, 10.34541550158063394, -14.16423886937409904 ) ) ;
#20611 = ORIENTED_EDGE ( 'NONE', *, *, #71835, .F. ) ;
#20612 = CARTESIAN_POINT ( 'NONE',  ( -42.94000000000001194, 92.00000000000000000, -10.09898361729590199 ) ) ;
#20613 = CARTESIAN_POINT ( 'NONE',  ( -4.431036607602702126, 14.49999999999999112, 14.33059365769913462 ) ) ;
#20614 = CARTESIAN_POINT ( 'NONE',  ( -46.94000000000001194, 103.0000000000000000, -5.997726559847240679 ) ) ;
#20615 = CARTESIAN_POINT ( 'NONE',  ( -0.3689425029237898834, 56.17874883491396076, -10.36894250292378850 ) ) ;
#20616 = LINE ( 'NONE', #13602, #22755 ) ;
#20617 = DIRECTION ( 'NONE',  ( 0.000000000000000000, 1.000000000000000000, -0.000000000000000000 ) ) ;
#20618 = CARTESIAN_POINT ( 'NONE',  ( 0.1532563361054082862, 51.21726448433412315, 2.638427012816831674 ) ) ;
#20619 = FACE_OUTER_BOUND ( 'NONE', #40624, .T. ) ;
#20620 = CARTESIAN_POINT ( 'NONE',  ( -2.816281873526473856, -0.8763653300695799508, 9.499525473075851096E-16 ) ) ;
#20621 = CARTESIAN_POINT ( 'NONE',  ( 18.52753015748618282, 13.92559781766745175, -4.923371831947291888 ) ) ;
#20622 = VECTOR ( 'NONE', #40881, 1000.000000000000000 ) ;
#20623 = CARTESIAN_POINT ( 'NONE',  ( 0.000000000000000000, 0.5000000000000004441, 0.000000000000000000 ) ) ;
#20624 = CARTESIAN_POINT ( 'NONE',  ( 1.472469842513823179, 11.42559781766745175, 4.923371831947296329 ) ) ;
#20625 = CARTESIAN_POINT ( 'NONE',  ( 13.43411237798106583, 7.665301336597086568, -12.81628187352647252 ) ) ;
#20626 = LINE ( 'NONE', #4650, #88788 ) ;
#20627 = EDGE_LOOP ( 'NONE', ( #6672, #58045, #44001, #65827, #51565, #71090 ) ) ;
#20628 = CARTESIAN_POINT ( 'NONE',  ( 17.96484262340118221, 14.93868534415484106, 7.964842623401181321 ) ) ;
#20629 = CARTESIAN_POINT ( 'NONE',  ( -4.164238869374099927, 7.012082168247302683, 3.795296366450308767 ) ) ;
#20630 = CARTESIAN_POINT ( 'NONE',  ( 14.92337183194729633, 27.67559781766745530, 8.527530157486181039 ) ) ;
#20631 = CARTESIAN_POINT ( 'NONE',  ( 0.5774900079438590739, 57.64701867748817676, -5.440088680355550821 ) ) ;
#20633 = DIRECTION ( 'NONE',  ( 0.9426414910921736556, 0.000000000000000000, 0.3338068592337842255 ) ) ;
#20632 = CARTESIAN_POINT ( 'NONE',  ( 22.81628187352647785, 31.62363466993042138, 6.195893100308588602E-16 ) ) ;
#20634 = CARTESIAN_POINT ( 'NONE',  ( 12.91533473730993009, 6.605352010821504471, -10.88017736071109987 ) ) ;
#20635 = DIRECTION ( 'NONE',  ( 0.000000000000000000, -0.000000000000000000, -1.000000000000000000 ) ) ;
#20636 = DIRECTION ( 'NONE',  ( 1.000000000000000000, 0.000000000000000000, 0.000000000000000000 ) ) ;
#20637 = CARTESIAN_POINT ( 'NONE',  ( 19.38216949554541202, 0.9986346699304200492, 9.382169495545424454 ) ) ;
#20638 = CARTESIAN_POINT ( 'NONE',  ( 17.20831665107776587, 64.13393115100079456, -7.208316651077762316 ) ) ;
#20639 = CARTESIAN_POINT ( 'NONE',  ( 19.84674366389459621, 18.50893115100078745, 7.409399052514197653E-17 ) ) ;
#20640 = CARTESIAN_POINT ( 'NONE',  ( -9.422509992056145478, -27.35298132251182324, -5.440088680355541939 ) ) ;
#20641 = CARTESIAN_POINT ( 'NONE',  ( 22.81628187352647785, 26.62363466993042138, 6.195893100308588602E-16 ) ) ;
#20642 = CARTESIAN_POINT ( 'NONE',  ( -10.95083791927332051, -94.44918831363982292, -4.000000000000000000 ) ) ;
#20644 = FACE_OUTER_BOUND ( 'NONE', #84092, .T. ) ;
#20643 = CARTESIAN_POINT ( 'NONE',  ( 10.00000000000000178, 44.31368534415484106, 10.88017736071110342 ) ) ;
#20645 = DIRECTION ( 'NONE',  ( -1.000000000000000000, 0.000000000000000000, 0.000000000000000000 ) ) ;
#20646 = EDGE_CURVE ( 'NONE', #95164, #88686, #54810, .T. ) ;
#20647 = CARTESIAN_POINT ( 'NONE',  ( 14.99999999999997691, 80.32179676972448590, 4.000000000000000000 ) ) ;
#20648 = CARTESIAN_POINT ( 'NONE',  ( 20.88017736071110164, 30.35535201082151247, 2.915334737309930979 ) ) ;
#20649 = CARTESIAN_POINT ( 'NONE',  ( 19.84674366389459621, 48.50893115100078745, 7.409399052514197653E-17 ) ) ;
#20650 = CARTESIAN_POINT ( 'NONE',  ( 12.91533473730992121, 54.52201867748816255, 10.88017736071110164 ) ) ;
#20651 = CARTESIAN_POINT ( 'NONE',  ( 24.16423886937409904, 34.09541550158064638, 3.795296366450317205 ) ) ;
#20652 = CARTESIAN_POINT ( 'NONE',  ( 18.06765999051784988, 33.99127512925449679, 6.500000000000019540 ) ) ;
#20653 = CARTESIAN_POINT ( 'NONE',  ( 18.52753015748618282, 43.92559781766745175, -4.923371831947291888 ) ) ;
#20654 =( NAMED_UNIT ( * ) SI_UNIT ( $, .STERADIAN. ) SOLID_ANGLE_UNIT ( ) );
#20655 = CARTESIAN_POINT ( 'NONE',  ( 1.472469842513823179, 65.59226448433412315, -4.923371831947296329 ) ) ;
#20656 = VERTEX_POINT ( 'NONE', #11553 ) ;
#20657 = CARTESIAN_POINT ( 'NONE',  ( -0.8801773607111009756, 28.06368534415484106, 1.068504757029289695E-15 ) ) ;
#20658 = CARTESIAN_POINT ( 'NONE',  ( 20.88017736071110875, 5.772018677488170546, -2.915334737309920765 ) ) ;
#20659 = CARTESIAN_POINT ( 'NONE',  ( 0.5774900079438590739, 17.64701867748817321, -5.440088680355550821 ) ) ;
#20660 = CARTESIAN_POINT ( 'NONE',  ( 5.076628168052704559, 5.175597817667451750, -8.527530157486179263 ) ) ;
#20661 = CARTESIAN_POINT ( 'NONE',  ( 20.36894250292379382, 23.67874883491397142, 10.36894250292379205 ) ) ;
#20662 = CARTESIAN_POINT ( 'NONE',  ( 10.00000000000000000, 19.75893115100078390, -9.846743663894594434 ) ) ;
#20663 = CARTESIAN_POINT ( 'NONE',  ( 2.791683348922240793, 61.63393115100079456, 7.208316651077764092 ) ) ;
#20664 = CARTESIAN_POINT ( 'NONE',  ( 10.00000000000000000, 31.81368534415483751, -10.88017736071110342 ) ) ;
#20665 = CARTESIAN_POINT ( 'NONE',  ( 0.1129803114748866161, 34.29427333184091964, -6.480634945678686698 ) ) ;
#20666 = CARTESIAN_POINT ( 'NONE',  ( 19.42250999205614548, 25.98035201082150891, -5.440088680355545492 ) ) ;
#20667 = EDGE_CURVE ( 'NONE', #93500, #71973, #98957, .T. ) ;
#20668 = ORIENTED_EDGE ( 'NONE', *, *, #10297, .T. ) ;
#20669 = FACE_OUTER_BOUND ( 'NONE', #82579, .T. ) ;
#20670 = CARTESIAN_POINT ( 'NONE',  ( 5.076628168052703671, 41.84226448433411605, 8.527530157486179263 ) ) ;
#20671 =( BOUNDED_CURVE ( )  B_SPLINE_CURVE ( 2, ( #41942, #63913, #86926, #17946, #4433, #18438, #56915, #65395, #48921 ),
 .UNSPECIFIED., .F., .T. ) 
 B_SPLINE_CURVE_WITH_KNOTS ( ( 3, 2, 2, 2, 3 ),
 ( 0.2953713073319822469, 0.2976190476190476164, 0.3035714285714285476, 0.3095238095238095344, 0.3117715498108742378 ),
 .UNSPECIFIED. ) 
 CURVE ( )  GEOMETRIC_REPRESENTATION_ITEM ( )  RATIONAL_B_SPLINE_CURVE ( ( 0.9839835555609424134, 0.9871328979762477029, 1.000000000000000000, 0.9659258262890683122, 1.000000000000000000, 0.9659258262890683122, 1.000000000000000000, 0.9871328979762515887, 0.9839835555609444118 ) ) 
 REPRESENTATION_ITEM ( '' )  );
#20673 = EDGE_LOOP ( 'NONE', ( #88088, #66176, #84875, #89987 ) ) ;
#20672 = EDGE_CURVE ( 'NONE', #75793, #27193, #13023, .T. ) ;
#20674 = ORIENTED_EDGE ( 'NONE', *, *, #13689, .T. ) ;
#20675 = FACE_OUTER_BOUND ( 'NONE', #42187, .T. ) ;
#20676 = CARTESIAN_POINT ( 'NONE',  ( 2.917880565312950480, 15.97041550158063217, -12.26659068614894821 ) ) ;
#20677 = CARTESIAN_POINT ( 'NONE',  ( 6.204703633549690345, 15.76208216824730179, -14.16423886937410259 ) ) ;
#20678 = CARTESIAN_POINT ( 'NONE',  ( 4.559911319644449179, 57.23035201082150536, -9.422509992056141925 ) ) ;
#20679 = CARTESIAN_POINT ( 'NONE',  ( -4.164238869374099927, 57.01208216824731068, 3.795296366450308767 ) ) ;
#20680 = CARTESIAN_POINT ( 'NONE',  ( 1.472469842513823179, 65.59226448433412315, -4.923371831947296329 ) ) ;
#20681 = CARTESIAN_POINT ( 'NONE',  ( 5.076628168052703671, 31.84226448433412315, 8.527530157486179263 ) ) ;
#20682 = FACE_OUTER_BOUND ( 'NONE', #36712, .T. ) ;
#20684 = CARTESIAN_POINT ( 'NONE',  ( -1.099225684535947600, -0.4596986634029132657, 6.408140936763237150 ) ) ;
#20683 = CARTESIAN_POINT ( 'NONE',  ( 4.559911319644449179, 33.89701867748817676, 9.422509992056141925 ) ) ;
#20685 = CARTESIAN_POINT ( 'NONE',  ( -0.3689425029237898834, 21.17874883491396432, -10.36894250292378850 ) ) ;
#20686 = CARTESIAN_POINT ( 'NONE',  ( 22.26659068614894466, 48.88708216824730357, 7.082119434687054849 ) ) ;
#20687 = EDGE_CURVE ( 'NONE', #49977, #1901, #41539, .T. ) ;
#20688 = CARTESIAN_POINT ( 'NONE',  ( 15.44008868035555260, 24.73035201082150891, 9.422509992056143702 ) ) ;
#20689 = CARTESIAN_POINT ( 'NONE',  ( -0.1503990784575328643, 0.07447313448805115144, 6.262539305110068177 ) ) ;
#20690 = LINE ( 'NONE', #83655, #33149 ) ;
#20691 = CARTESIAN_POINT ( 'NONE',  ( 4.559911319644449179, 37.23035201082150536, -9.422509992056141925 ) ) ;
#20692 = CIRCLE ( 'NONE', #38470, 9.999999999999994671 ) ;
#20693 = CARTESIAN_POINT ( 'NONE',  ( 4.923371831947301658, -37.32440218233254114, 8.527530157486175710 ) ) ;
#20694 = VERTEX_POINT ( 'NONE', #65025 ) ;
#20695 = CARTESIAN_POINT ( 'NONE',  ( 0.2851878892742318872, 14.76937129508116264, -14.93850447011040927 ) ) ;
#20696 = ORIENTED_EDGE ( 'NONE', *, *, #24985, .F. ) ;
#20697 = ORIENTED_EDGE ( 'NONE', *, *, #35991, .F. ) ;
#20698 = CARTESIAN_POINT ( 'NONE',  ( 2.917880565312948704, 42.63708216824729647, 12.26659068614894643 ) ) ;
#20699 = CARTESIAN_POINT ( 'NONE',  ( 7.361572987183170547, 42.05059781766745886, 9.846743663894590881 ) ) ;
#20700 = CARTESIAN_POINT ( 'NONE',  ( 0.5774900079438590739, 52.64701867748817676, -5.440088680355550821 ) ) ;
#20701 = STYLED_ITEM ( 'NONE', ( #70484 ), #27325 ) ;
#20702 = DIRECTION ( 'NONE',  ( 0.000000000000000000, 1.000000000000000000, 0.000000000000000000 ) ) ;
#20703 = CARTESIAN_POINT ( 'NONE',  ( 7.084665262690076126, 54.10535201082151247, 10.88017736071109987 ) ) ;
#20704 = CARTESIAN_POINT ( 'NONE',  ( 3.591859063236763294, 58.29030133659708923, -11.09922568453595026 ) ) ;
#20705 = CARTESIAN_POINT ( 'NONE',  ( 11.09922568453595026, 11.20696800326376241, 6.408140936763232709 ) ) ;
#20706 = EDGE_LOOP ( 'NONE', ( #53087, #26994, #61274, #83480, #296, #68808 ) ) ;
#20707 = CARTESIAN_POINT ( 'NONE',  ( 13.79529636645031943, 25.34541550158063572, -14.16423886937409904 ) ) ;
#20708 = ORIENTED_EDGE ( 'NONE', *, *, #30256, .T. ) ;
#20709 = EDGE_CURVE ( 'NONE', #89907, #69690, #91120, .T. ) ;
#20710 = CARTESIAN_POINT ( 'NONE',  ( 3.591859063236761518, 19.95696800326375353, 11.09922568453594849 ) ) ;
#20711 = ORIENTED_EDGE ( 'NONE', *, *, #67409, .T. ) ;
#20712 = CARTESIAN_POINT ( 'NONE',  ( 3.591859063236761518, 39.95696800326375353, 11.09922568453594849 ) ) ;
#20713 =( GEOMETRIC_REPRESENTATION_CONTEXT ( 3 ) GLOBAL_UNCERTAINTY_ASSIGNED_CONTEXT ( ( #71206 ) ) GLOBAL_UNIT_ASSIGNED_CONTEXT ( ( #33757, #93792, #49275 ) ) REPRESENTATION_CONTEXT ( 'NONE', 'WORKASPACE' ) );
#20714 = CARTESIAN_POINT ( 'NONE',  ( 10.00000000000000178, 14.31368534415483929, 10.88017736071110342 ) ) ;
#20715 = CARTESIAN_POINT ( 'NONE',  ( 2.791683348922240793, 36.63393115100078035, 7.208316651077764092 ) ) ;
#20716 = CARTESIAN_POINT ( 'NONE',  ( 10.00000000000000178, 14.31368534415483751, 10.88017736071110342 ) ) ;
#20717 = CARTESIAN_POINT ( 'NONE',  ( 22.81628187352648496, 56.83196800326374643, -3.434112377981050290 ) ) ;
#20718 = FACE_OUTER_BOUND ( 'NONE', #18944, .T. ) ;
#20719 = CARTESIAN_POINT ( 'NONE',  ( 0.1532563361054083140, 41.00893115100078745, 1.131784320476157264E-15 ) ) ;
#20721 = ORIENTED_EDGE ( 'NONE', *, *, #33440, .T. ) ;
#20720 = CARTESIAN_POINT ( 'NONE',  ( 0.5774900079438607392, 68.48035201082150536, 5.440088680355550821 ) ) ;
#20722 = CIRCLE ( 'NONE', #76602, 0.2500000000000002220 ) ;
#20723 = CARTESIAN_POINT ( 'NONE',  ( 66.76470751278411342, 44.49999999999998579, -10.00000000000000000 ) ) ;
#20724 = DIRECTION ( 'NONE',  ( 0.000000000000000000, 1.000000000000000000, 0.000000000000000000 ) ) ;
#20725 = DIRECTION ( 'NONE',  ( 0.9238795325112876267, 0.000000000000000000, 0.3826834323650877279 ) ) ;
#20726 =( NAMED_UNIT ( * ) PLANE_ANGLE_UNIT ( ) SI_UNIT ( $, .RADIAN. ) );
#20727 = CARTESIAN_POINT ( 'NONE',  ( 18.52753015748617571, 13.09226448433411960, 4.923371831947298993 ) ) ;
#20728 = CARTESIAN_POINT ( 'NONE',  ( 0.6178305044545818747, 23.49863466993041783, -9.382169495545419124 ) ) ;
#20729 = VERTEX_POINT ( 'NONE', #57540 ) ;
#20730 = CARTESIAN_POINT ( 'NONE',  ( 19.84674366389459266, 58.71726448433411605, -2.638427012816827677 ) ) ;
#20731 = CARTESIAN_POINT ( 'NONE',  ( -14.62232599144297929, 6.894848190650002788E-16, 0.3548652576987693097 ) ) ;
#20732 = CARTESIAN_POINT ( 'NONE',  ( 24.16423886937410614, 19.30374883491397142, 8.672049930838204340E-16 ) ) ;
#20733 = CARTESIAN_POINT ( 'NONE',  ( 10.00000000000000178, 42.25893115100078745, 9.846743663894594434 ) ) ;
#20734 = CARTESIAN_POINT ( 'NONE',  ( 0.6178305044545818747, 48.49863466993042493, -9.382169495545419124 ) ) ;
#20735 = CARTESIAN_POINT ( 'NONE',  ( 20.24186590665277308, 37.61633188102327807, -6.114288769123051637 ) ) ;
#20736 = CARTESIAN_POINT ( 'NONE',  ( 17.96484262340118221, 56.18868534415484817, -7.964842623401177768 ) ) ;
#20737 = CARTESIAN_POINT ( 'NONE',  ( 6.689969769698871360, -0.03417435944610275333, 12.58200319823975022 ) ) ;
#20738 = CARTESIAN_POINT ( 'NONE',  ( 0.1532563361054100626, 30.80059781766744820, -2.638427012816831230 ) ) ;
#20739 = CARTESIAN_POINT ( 'NONE',  ( 0.5774900079438590739, 42.64701867748816966, -5.440088680355550821 ) ) ;
#20740 = CARTESIAN_POINT ( 'NONE',  ( 19.38216949554541202, 45.99863466993041072, 9.382169495545424454 ) ) ;
#20741 = CARTESIAN_POINT ( 'NONE',  ( 12.63842701281683034, 32.46726448433412315, 9.846743663894596210 ) ) ;
#20742 = PRESENTATION_STYLE_ASSIGNMENT (( #78285 ) ) ;
#20743 = CARTESIAN_POINT ( 'NONE',  ( -13.45431060380794541, 90.84076481352336430, 7.653071044410319601 ) ) ;
#20744 = CARTESIAN_POINT ( 'NONE',  ( 17.96484262340118221, 51.18868534415483396, -7.964842623401177768 ) ) ;
#20745 = EDGE_LOOP ( 'NONE', ( #76134, #73033, #91440, #47676 ) ) ;
#20746 = DIRECTION ( 'NONE',  ( 0.000000000000000000, -0.000000000000000000, 1.000000000000000000 ) ) ;
#20747 = CARTESIAN_POINT ( 'NONE',  ( -0.8801773607111009756, 13.06368534415483929, 1.068504757029289695E-15 ) ) ;
#20749 = CARTESIAN_POINT ( 'NONE',  ( -0.8801773607110991993, 42.85535201082150536, -2.915334737309923874 ) ) ;
#20748 = CARTESIAN_POINT ( 'NONE',  ( 14.92337183194729633, 62.67559781766745886, 8.527530157486181039 ) ) ;
#20750 = CARTESIAN_POINT ( 'NONE',  ( 14.24131928502211331, 0.000000000000000000, 0.4973178280106892446 ) ) ;
#20751 = CARTESIAN_POINT ( 'NONE',  ( 2.035157376598824452, 63.68868534415484106, 7.964842623401179544 ) ) ;
#20752 = VECTOR ( 'NONE', #50088, 1000.000000000000114 ) ;
#20754 = CARTESIAN_POINT ( 'NONE',  ( 9.629649721936188023E-32, 78.62578230273079782, -9.232066091999506341 ) ) ;
#20753 = CARTESIAN_POINT ( 'NONE',  ( 0.5774900079438590739, 32.64701867748816966, -5.440088680355550821 ) ) ;
#20755 = CARTESIAN_POINT ( 'NONE',  ( 7.361572987183169658, 4.967264484334119601, -9.846743663894592657 ) ) ;
#20756 = CARTESIAN_POINT ( 'NONE',  ( 10.00000000000000000, 24.75893115100078745, -9.846743663894594434 ) ) ;
#20757 = DIRECTION ( 'NONE',  ( -0.000000000000000000, -0.000000000000000000, 1.000000000000000000 ) ) ;
#20758 = CARTESIAN_POINT ( 'NONE',  ( -12.26659068614895354, 1.387082168247309788, -7.082119434687038861 ) ) ;
#20759 = CARTESIAN_POINT ( 'NONE',  ( 19.84674366389459621, 48.50893115100078745, 7.409399052514197653E-17 ) ) ;
#20761 = CARTESIAN_POINT ( 'NONE',  ( 4.656498301622464808, -8.256471156977859494, 3.749999999999998668 ) ) ;
#20760 = CARTESIAN_POINT ( 'NONE',  ( 17.08211943468705840, 55.13708216824731068, -12.26659068614894466 ) ) ;
#20762 = CARTESIAN_POINT ( 'NONE',  ( 1.711636803080574420, 61.84492782695771496, -6.500000000000073719 ) ) ;
#20763 = EDGE_CURVE ( 'NONE', #16885, #62857, #11779, .T. ) ;
#20764 = CIRCLE ( 'NONE', #30309, 2.896551724137931494 ) ;
#20765 = CARTESIAN_POINT ( 'NONE',  ( -4.164238869374099927, 12.01208216824730357, 3.795296366450308767 ) ) ;
#20766 = CARTESIAN_POINT ( 'NONE',  ( 10.00000000000000178, 43.05374883491397497, 14.16423886937410082 ) ) ;
#20767 = CARTESIAN_POINT ( 'NONE',  ( -2.816281873526471635, 3.915301336597087456, -3.434112377981056508 ) ) ;
#20768 = EDGE_LOOP ( 'NONE', ( #3128, #66247, #61347, #45636 ) ) ;
#20769 = CARTESIAN_POINT ( 'NONE',  ( 12.91533473730993009, 11.60535201082150714, -10.88017736071109987 ) ) ;
#20770 = CARTESIAN_POINT ( 'NONE',  ( 7.361572987183170547, 47.05059781766745175, 9.846743663894590881 ) ) ;
#20772 = CARTESIAN_POINT ( 'NONE',  ( -12.24686443627858878, 90.44926614966340139, -7.163467944141197918 ) ) ;
#20771 = CARTESIAN_POINT ( 'NONE',  ( -4.000000000000000000, 37.00000000000000000, 3.750000000000000000 ) ) ;
#20773 = FILL_AREA_STYLE ('',( #4789 ) ) ;
#20774 = CARTESIAN_POINT ( 'NONE',  ( 5.076628168052704559, 0.1755978176674514724, -8.527530157486179263 ) ) ;
#20775 = CARTESIAN_POINT ( 'NONE',  ( -2.816281873526471635, 18.91530133659708213, -3.434112377981056508 ) ) ;
#20776 = CARTESIAN_POINT ( 'NONE',  ( 18.52753015748617571, 23.09226448433411960, 4.923371831947298993 ) ) ;
#20777 = EDGE_LOOP ( 'NONE', ( #75543, #64569, #49543, #17412 ) ) ;
#20778 = CARTESIAN_POINT ( 'NONE',  ( 18.52753015748618282, 3.925597817667451306, -4.923371831947291888 ) ) ;
#20779 = DIRECTION ( 'NONE',  ( -2.107602052970794797E-16, 1.000000000000000000, 0.000000000000000000 ) ) ;
#20780 = CARTESIAN_POINT ( 'NONE',  ( 4.838527690343521925, 0.5000000000000004441, 14.19819177887730177 ) ) ;
#20781 = CARTESIAN_POINT ( 'NONE',  ( 20.88017736071110875, 15.77201867748817143, -2.915334737309920765 ) ) ;
#20782 = CARTESIAN_POINT ( 'NONE',  ( 13.79529636645030344, 38.26208216824729647, 14.16423886937410614 ) ) ;
#20783 = CARTESIAN_POINT ( 'NONE',  ( 0.5774900079438590739, 47.64701867748817676, -5.440088680355550821 ) ) ;
#20784 = CARTESIAN_POINT ( 'NONE',  ( 7.084665262690076126, 67.02201867748817676, -10.88017736071110164 ) ) ;
#20785 = CARTESIAN_POINT ( 'NONE',  ( 38.04706783004212411, 44.99999999999998579, -7.000000000000000000 ) ) ;
#20786 = VECTOR ( 'NONE', #52721, 1000.000000000000000 ) ;
#20787 = SURFACE_SIDE_STYLE ('',( #49301 ) ) ;
#20788 = CARTESIAN_POINT ( 'NONE',  ( 19.84674366389459266, 23.71726448433412315, -2.638427012816827677 ) ) ;
#20789 = CARTESIAN_POINT ( 'NONE',  ( 70.19910379943081580, 41.67447916666664298, 9.500000000000000000 ) ) ;
#20790 = CARTESIAN_POINT ( 'NONE',  ( 1.472469842513823179, 5.592264484334118713, -4.923371831947296329 ) ) ;
#20791 = CARTESIAN_POINT ( 'NONE',  ( -46.82017113615791004, 100.6079546444643427, 9.324761308090124601 ) ) ;
#20792 = CARTESIAN_POINT ( 'NONE',  ( 5.076628168052704559, 35.17559781766745175, -8.527530157486179263 ) ) ;
#20793 = CARTESIAN_POINT ( 'NONE',  ( 10.00000000000000178, 62.25893115100078745, 9.846743663894594434 ) ) ;
#20794 = CARTESIAN_POINT ( 'NONE',  ( 12.91533473730992121, 39.52201867748817676, 10.88017736071110164 ) ) ;
#20795 = B_SPLINE_CURVE_WITH_KNOTS ( 'NONE', 3,
 ( #58103, #49617, #48644, #88119, #26154, #18656 ),
 .UNSPECIFIED., .F., .F.,
 ( 4, 2, 4 ),
 ( 1.170549273921106170E-18, 0.0002626113303185924623, 0.0005252226606371837320 ),
 .UNSPECIFIED. ) ;
#20796 = ADVANCED_FACE ( 'NONE', ( #41087 ), #70374, .T. ) ;
#20797 = ORIENTED_EDGE ( 'NONE', *, *, #98370, .T. ) ;
#20798 = CARTESIAN_POINT ( 'NONE',  ( 10.00000000000000000, 62.87363466993042493, -12.81628187352647608 ) ) ;
#20799 = CARTESIAN_POINT ( 'NONE',  ( 12.25993886608605443, 0.5000000000000004441, -8.642563219313617040 ) ) ;
#20800 = CARTESIAN_POINT ( 'NONE',  ( 22.81628187352647785, 41.41530133659708923, 3.434112377981063169 ) ) ;
#20802 = CARTESIAN_POINT ( 'NONE',  ( 12.63842701281683034, 32.46726448433412315, 9.846743663894596210 ) ) ;
#20801 = CARTESIAN_POINT ( 'NONE',  ( 13.79529636645031943, 65.34541550158063217, -14.16423886937409904 ) ) ;
#20803 = CARTESIAN_POINT ( 'NONE',  ( -0.1503990784575328643, 60.12777174578613426, 6.262539305110068177 ) ) ;
#20804 = CARTESIAN_POINT ( 'NONE',  ( 2.791683348922240793, 1.633931151000784565, 7.208316651077764092 ) ) ;
#20805 = CARTESIAN_POINT ( 'NONE',  ( -2.266590686148945544, 21.38708216824730357, -7.082119434687050408 ) ) ;
#20806 = EDGE_CURVE ( 'NONE', #87437, #11855, #16050, .T. ) ;
#20807 = CARTESIAN_POINT ( 'NONE',  ( 17.08211943468705840, 50.13708216824730357, -12.26659068614894466 ) ) ;
#20808 = CARTESIAN_POINT ( 'NONE',  ( 0.1532563361054082862, 41.21726448433411605, 2.638427012816831674 ) ) ;
#20809 = CARTESIAN_POINT ( 'NONE',  ( -14.56195259121199115, 6.572975670693368659E-16, 1.374002722866616066 ) ) ;
#20810 = CARTESIAN_POINT ( 'NONE',  ( 20.88017736071110164, 40.35535201082150536, 2.915334737309930979 ) ) ;
#20811 = CARTESIAN_POINT ( 'NONE',  ( 17.96484262340118221, 54.93868534415484106, 7.964842623401181321 ) ) ;
#20812 = EDGE_LOOP ( 'NONE', ( #50589, #57978, #50752, #81554, #29729, #35968 ) ) ;
#20813 = CARTESIAN_POINT ( 'NONE',  ( -2.816281873526473856, 49.12363466993042493, 9.499525473075851096E-16 ) ) ;
#20814 = CARTESIAN_POINT ( 'NONE',  ( 0.1532563361054100626, 0.8005978176674514168, -2.638427012816831230 ) ) ;
#20815 = ORIENTED_EDGE ( 'NONE', *, *, #79843, .F. ) ;
#20816 = CARTESIAN_POINT ( 'NONE',  ( -0.3689425029237898834, 1.178748834913967869, -10.36894250292378850 ) ) ;
#20817 = CARTESIAN_POINT ( 'NONE',  ( 0.1532563361054083140, 6.008931151000784787, 1.131784320476157264E-15 ) ) ;
#20818 = DIRECTION ( 'NONE',  ( 5.506706202140776441E-14, 0.000000000000000000, 1.000000000000000000 ) ) ;
#20819 = VERTEX_POINT ( 'NONE', #71584 ) ;
#20820 = AXIS2_PLACEMENT_3D ( 'NONE', #6642, #82140, #81645 ) ;
#20821 = CARTESIAN_POINT ( 'NONE',  ( 12.91533473730992121, 19.52201867748816611, 10.88017736071110164 ) ) ;
#20822 = DIRECTION ( 'NONE',  ( -0.000000000000000000, -0.000000000000000000, -1.000000000000000000 ) ) ;
#20823 = CARTESIAN_POINT ( 'NONE',  ( 13.79529636645031943, 20.34541550158063572, -14.16423886937409904 ) ) ;
#20824 = ORIENTED_EDGE ( 'NONE', *, *, #26557, .F. ) ;
#20825 = CARTESIAN_POINT ( 'NONE',  ( -0.8801773607111009756, 28.06368534415484106, 1.068504757029289695E-15 ) ) ;
#20826 = AXIS2_PLACEMENT_3D ( 'NONE', #58385, #63915, #18937 ) ;
#20827 = CARTESIAN_POINT ( 'NONE',  ( 18.52753015748617571, 63.09226448433412315, 4.923371831947298993 ) ) ;
#20828 = ORIENTED_EDGE ( 'NONE', *, *, #28948, .F. ) ;
#20829 = CARTESIAN_POINT ( 'NONE',  ( 19.84674366389459266, 63.71726448433412315, -2.638427012816827677 ) ) ;
#20830 = EDGE_LOOP ( 'NONE', ( #13331, #75595, #90781, #3664 ) ) ;
#20831 = CARTESIAN_POINT ( 'NONE',  ( 2.035157376598822676, 67.43868534415484817, -7.964842623401177768 ) ) ;
#20832 = CARTESIAN_POINT ( 'NONE',  ( 2.393480905993173646, 14.63606894034135308, -14.80781041047755053 ) ) ;
#20833 = CARTESIAN_POINT ( 'NONE',  ( 22.81628187352648496, 36.83196800326376064, -3.434112377981050290 ) ) ;
#20835 = DIRECTION ( 'NONE',  ( -1.000000000000000000, 0.000000000000000000, 0.000000000000000000 ) ) ;
#20834 = CARTESIAN_POINT ( 'NONE',  ( -0.8801773607111009756, 13.06368534415483929, 1.068504757029289695E-15 ) ) ;
#20836 = CARTESIAN_POINT ( 'NONE',  ( -0.8801773607110991993, 67.85535201082151957, -2.915334737309923874 ) ) ;
#20837 = CONICAL_SURFACE ( 'NONE', #30383, 1.249999999999987121, 1.029744258676654312 ) ;
#20838 = CARTESIAN_POINT ( 'NONE',  ( 10.00000000000000178, 24.31368534415484106, 10.88017736071110342 ) ) ;
#20839 = VERTEX_POINT ( 'NONE', #20542 ) ;
#20840 = CARTESIAN_POINT ( 'NONE',  ( 0.6178305044545818747, 53.49863466993041072, -9.382169495545419124 ) ) ;
#20841 = CARTESIAN_POINT ( 'NONE',  ( -0.8801773607110991993, 42.85535201082150536, -2.915334737309923874 ) ) ;
#20842 = DIRECTION ( 'NONE',  ( 1.000000000000000000, 3.945256819650108695E-12, 0.000000000000000000 ) ) ;
#20843 = CARTESIAN_POINT ( 'NONE',  ( -2.816281873526473856, 44.12363466993042493, 9.499525473075851096E-16 ) ) ;
#20844 = CARTESIAN_POINT ( 'NONE',  ( 17.96484262340118221, 46.18868534415484106, -7.964842623401177768 ) ) ;
#20845 = CARTESIAN_POINT ( 'NONE',  ( 18.52753015748617571, 58.09226448433411605, 4.923371831947298993 ) ) ;
#20846 = LINE ( 'NONE', #43337, #1661 ) ;
#20847 = CIRCLE ( 'NONE', #46403, 20.00000000000000000 ) ;
#20848 = CARTESIAN_POINT ( 'NONE',  ( 10.00000000000000178, 12.25893115100078568, 9.846743663894594434 ) ) ;
#20849 = CARTESIAN_POINT ( 'NONE',  ( -1.099225684535947600, 9.540301336597087456, 6.408140936763237150 ) ) ;
#20851 = CARTESIAN_POINT ( 'NONE',  ( 19.84674366389459621, 58.50893115100078745, 7.409399052514197653E-17 ) ) ;
#20850 = DIRECTION ( 'NONE',  ( 0.000000000000000000, 0.000000000000000000, -1.000000000000000000 ) ) ;
#20852 = CARTESIAN_POINT ( 'NONE',  ( 2.035157376598822676, 22.43868534415483396, -7.964842623401177768 ) ) ;
#20853 = CARTESIAN_POINT ( 'NONE',  ( 1.472469842513823179, 55.59226448433412315, -4.923371831947296329 ) ) ;
#20854 = DIRECTION ( 'NONE',  ( 0.000000000000000000, -1.000000000000000000, 0.000000000000000000 ) ) ;
#20855 = AXIS2_PLACEMENT_3D ( 'NONE', #89122, #81614, #81124 ) ;
#20856 = CARTESIAN_POINT ( 'NONE',  ( 1.829604203029677523, -0.03417435944610275333, -15.89119079541585755 ) ) ;
#20857 = CARTESIAN_POINT ( 'NONE',  ( 2.791683348922240793, 11.63393115100078568, 7.208316651077764092 ) ) ;
#20858 = CARTESIAN_POINT ( 'NONE',  ( 0.1532563361054083140, 1.008931151000784787, 1.131784320476157264E-15 ) ) ;
#20860 = ORIENTED_EDGE ( 'NONE', *, *, #553, .T. ) ;
#20859 = CARTESIAN_POINT ( 'NONE',  ( 10.00000000000000178, 67.25893115100079456, 9.846743663894594434 ) ) ;
#20861 = DIRECTION ( 'NONE',  ( 0.000000000000000000, 0.000000000000000000, 1.000000000000000000 ) ) ;
#20862 = CARTESIAN_POINT ( 'NONE',  ( 0.6178305044545838731, 39.74863466993041072, 9.382169495545420901 ) ) ;
#20863 = CARTESIAN_POINT ( 'NONE',  ( 19.84674366389459621, 28.50893115100078745, 7.409399052514197653E-17 ) ) ;
#20864 = CARTESIAN_POINT ( 'NONE',  ( 0.5774900079438590739, 57.64701867748817676, -5.440088680355550821 ) ) ;
#20865 = CARTESIAN_POINT ( 'NONE',  ( -4.164238869374099039, 56.80374883491397497, 8.674139862899312516E-16 ) ) ;
#20866 = CARTESIAN_POINT ( 'NONE',  ( 17.20831665107776587, 27.88393115100078390, 7.208316651077764980 ) ) ;
#20867 = EDGE_LOOP ( 'NONE', ( #86946, #42407, #9158, #64251 ) ) ;
#20868 = CARTESIAN_POINT ( 'NONE',  ( -0.2418659066527710233, 50.11633188102328518, 6.114288769123046308 ) ) ;
#20869 = CARTESIAN_POINT ( 'NONE',  ( 2.035157376598824452, 8.688685344154839285, 7.964842623401179544 ) ) ;
#20870 = CARTESIAN_POINT ( 'NONE',  ( -8.118176716543590743, 86.25458391402875691, -4.292297935673068388 ) ) ;
#20871 = CARTESIAN_POINT ( 'NONE',  ( -0.8801773607111009756, 18.06368534415484106, 1.068504757029289695E-15 ) ) ;
#20872 = CARTESIAN_POINT ( 'NONE',  ( -4.164238869374099039, 46.80374883491397497, 8.674139862899312516E-16 ) ) ;
#20874 = DIRECTION ( 'NONE',  ( 0.000000000000000000, 0.000000000000000000, -1.000000000000000000 ) ) ;
#20873 = CARTESIAN_POINT ( 'NONE',  ( 10.00000000000000178, 53.05374883491396787, 14.16423886937410082 ) ) ;
#20875 = LINE ( 'NONE', #42394, #6902 ) ;
#20876 = CARTESIAN_POINT ( 'NONE',  ( 0.1532563361054100626, 15.80059781766745353, -2.638427012816831230 ) ) ;
#20877 = CARTESIAN_POINT ( 'NONE',  ( 22.81628187352647785, 1.415301336597087012, 3.434112377981063169 ) ) ;
#20878 = VERTEX_POINT ( 'NONE', #20037 ) ;
#20879 = CARTESIAN_POINT ( 'NONE',  ( -0.8801773607110991993, 52.85535201082151247, -2.915334737309923874 ) ) ;
#20880 = SURFACE_SIDE_STYLE ('',( #74858 ) ) ;
#20881 = EDGE_CURVE ( 'NONE', #95321, #77887, #75507, .T. ) ;
#20882 = CARTESIAN_POINT ( 'NONE',  ( 0.1532563361054100626, 55.80059781766745175, -2.638427012816831230 ) ) ;
#20883 = CARTESIAN_POINT ( 'NONE',  ( -8.099999999999999645, 83.99999999999994316, -2.900000000000000799 ) ) ;
#20884 = CARTESIAN_POINT ( 'NONE',  ( 14.92337183194729988, 64.34226448433412315, -8.527530157486177487 ) ) ;
#20885 = CARTESIAN_POINT ( 'NONE',  ( -0.2076750170234879511, 0.04922511925147027984, 14.75137184266417201 ) ) ;
#20886 = AXIS2_PLACEMENT_3D ( 'NONE', #94063, #3575, #70584 ) ;
#20887 = EDGE_LOOP ( 'NONE', ( #15083, #42582, #23074, #67684, #63891, #98798 ) ) ;
#20888 = CARTESIAN_POINT ( 'NONE',  ( 0.1532563361054082862, 26.21726448433411605, 2.638427012816831674 ) ) ;
#20889 = LINE ( 'NONE', #49043, #89518 ) ;
#20890 = CARTESIAN_POINT ( 'NONE',  ( 6.204703633549690345, 37.84541550158063927, 14.16423886937410082 ) ) ;
#20891 = DIRECTION ( 'NONE',  ( 1.000000000000000000, 0.000000000000000000, 0.000000000000000000 ) ) ;
#20893 = DIRECTION ( 'NONE',  ( 0.000000000000000000, 0.000000000000000000, 1.000000000000000000 ) ) ;
#20892 = CARTESIAN_POINT ( 'NONE',  ( -6.982525766850296023, -88.11956318484570261, -2.500000000000000888 ) ) ;
#20894 = CARTESIAN_POINT ( 'NONE',  ( 15.44008868035555793, 26.39701867748817321, -9.422509992056140149 ) ) ;
#20895 = CARTESIAN_POINT ( 'NONE',  ( -2.816281873526473856, 34.12363466993042493, 9.499525473075851096E-16 ) ) ;
#20896 = CARTESIAN_POINT ( 'NONE',  ( 20.88017736071110519, 10.56368534415483751, 2.639326808657452039E-16 ) ) ;
#20897 = AXIS2_PLACEMENT_3D ( 'NONE', #406, #77337, #54341 ) ;
#20898 = CARTESIAN_POINT ( 'NONE',  ( 21.09922568453594849, 41.20696800326375353, 6.408140936763242479 ) ) ;
#20899 = CARTESIAN_POINT ( 'NONE',  ( 21.09922568453594849, 56.20696800326375353, 6.408140936763242479 ) ) ;
#20900 = ORIENTED_EDGE ( 'NONE', *, *, #58413, .F. ) ;
#20901 = CYLINDRICAL_SURFACE ( 'NONE', #19727, 0.2500000000000002220 ) ;
#20902 = CARTESIAN_POINT ( 'NONE',  ( -10.91025143199674829, -52.91559880499846003, -4.000000000000000888 ) ) ;
#20903 = CARTESIAN_POINT ( 'NONE',  ( -4.164238869374099927, 32.01208216824730357, 3.795296366450308767 ) ) ;
#20904 = CARTESIAN_POINT ( 'NONE',  ( 17.08211943468705130, 3.470415501580634388, 12.26659068614894998 ) ) ;
#20905 = CARTESIAN_POINT ( 'NONE',  ( -0.8801773607110991993, 7.855352010821504471, -2.915334737309923874 ) ) ;
#20906 = CARTESIAN_POINT ( 'NONE',  ( 15.44008868035555793, 21.39701867748817321, -9.422509992056140149 ) ) ;
#20907 = DIRECTION ( 'NONE',  ( 0.000000000000000000, 1.000000000000000000, 3.035766082959409260E-14 ) ) ;
#20908 = FACE_OUTER_BOUND ( 'NONE', #1546, .T. ) ;
#20909 = CARTESIAN_POINT ( 'NONE',  ( 12.91533473730992121, 49.52201867748817676, 10.88017736071110164 ) ) ;
#20910 = CARTESIAN_POINT ( 'NONE',  ( 20.88017736071110875, 45.77201867748816966, -2.915334737309920765 ) ) ;
#20911 = CARTESIAN_POINT ( 'NONE',  ( -2.816281873526471635, 13.91530133659708746, -3.434112377981056508 ) ) ;
#20912 = CARTESIAN_POINT ( 'NONE',  ( -2.888814634336892784, -3.129363223631011419E-15, 14.33747749179066666 ) ) ;
#20913 = LINE ( 'NONE', #3939, #3621 ) ;
#20914 = CARTESIAN_POINT ( 'NONE',  ( 17.20831665107776587, 19.13393115100078035, -7.208316651077762316 ) ) ;
#20915 = CARTESIAN_POINT ( 'NONE',  ( 19.42250999205614193, 40.14701867748817676, 5.440088680355555262 ) ) ;
#20916 = EDGE_CURVE ( 'NONE', #31163, #31031, #71495, .T. ) ;
#20917 = CARTESIAN_POINT ( 'NONE',  ( 22.81628187352647785, 1.623634669930420271, 6.195893100308588602E-16 ) ) ;
#20918 = CARTESIAN_POINT ( 'NONE',  ( 1.274849032794231007, 43.57228050351031357, 6.499999999999895195 ) ) ;
#20919 = CARTESIAN_POINT ( 'NONE',  ( 18.52753015748618282, 18.92559781766745175, -4.923371831947291888 ) ) ;
#20920 = CARTESIAN_POINT ( 'NONE',  ( 0.6178305044545818747, 43.49863466993042493, -9.382169495545419124 ) ) ;
#20921 = CARTESIAN_POINT ( 'NONE',  ( 0.1532563361054083140, 21.00893115100078745, 1.131784320476157264E-15 ) ) ;
#20922 = ORIENTED_EDGE ( 'NONE', *, *, #13337, .T. ) ;
#20923 = CARTESIAN_POINT ( 'NONE',  ( 24.16423886937410614, 4.303748834913967869, 8.672049930838204340E-16 ) ) ;
#20924 = DIRECTION ( 'NONE',  ( 0.000000000000000000, 0.000000000000000000, 1.000000000000000000 ) ) ;
#20925 = CARTESIAN_POINT ( 'NONE',  ( 15.44008868035555793, 21.39701867748817321, -9.422509992056140149 ) ) ;
#20926 = CARTESIAN_POINT ( 'NONE',  ( 2.035157376598824452, 3.688685344154837953, 7.964842623401179544 ) ) ;
#20927 = CARTESIAN_POINT ( 'NONE',  ( 10.00000000000000000, 34.75893115100078745, -9.846743663894594434 ) ) ;
#20928 = CARTESIAN_POINT ( 'NONE',  ( 7.084665262690076126, 14.10535201082150358, 10.88017736071109987 ) ) ;
#20929 = CARTESIAN_POINT ( 'NONE',  ( 10.00000000000000000, 21.81368534415484106, -10.88017736071110342 ) ) ;
#20930 = ORIENTED_EDGE ( 'NONE', *, *, #75923, .T. ) ;
#20931 = TOROIDAL_SURFACE ( 'NONE', #9724, 2.500000000000000888, 0.5000000000000000000 ) ;
#20932 = CARTESIAN_POINT ( 'NONE',  ( 20.88017736071110875, 20.77201867748816611, -2.915334737309920765 ) ) ;
#20933 = CARTESIAN_POINT ( 'NONE',  ( 13.43411237798106583, 52.66530133659708213, -12.81628187352647252 ) ) ;
#20934 = CARTESIAN_POINT ( 'NONE',  ( 4.559911319644449179, 28.89701867748817321, 9.422509992056141925 ) ) ;
#20936 = CARTESIAN_POINT ( 'NONE',  ( 12.91533473730992121, 44.52201867748816966, 10.88017736071110164 ) ) ;
#20935 = CARTESIAN_POINT ( 'NONE',  ( -13.50249619331269102, 7.318364664277152957E-16, -5.623250243473677301 ) ) ;
#20937 = VERTEX_POINT ( 'NONE', #74018 ) ;
#20938 = CARTESIAN_POINT ( 'NONE',  ( 19.84674366389459266, 53.30059781766744464, 2.638427012816836559 ) ) ;
#20939 = CARTESIAN_POINT ( 'NONE',  ( 19.42250999205614548, 40.98035201082150536, -5.440088680355545492 ) ) ;
#20940 = CARTESIAN_POINT ( 'NONE',  ( 14.92337183194729988, 64.34226448433412315, -8.527530157486177487 ) ) ;
#20941 = MECHANICAL_DESIGN_GEOMETRIC_PRESENTATION_REPRESENTATION (  '', ( #8169 ), #38569 ) ;
#20942 =( LENGTH_UNIT ( ) NAMED_UNIT ( * ) SI_UNIT ( .MILLI., .METRE. ) );
#20943 = CARTESIAN_POINT ( 'NONE',  ( 3.591859063236763294, 58.29030133659708923, -11.09922568453595026 ) ) ;
#20944 = CARTESIAN_POINT ( 'NONE',  ( -8.000000000000000000, 79.82179676972448590, -4.250000000000000000 ) ) ;
#20945 = CARTESIAN_POINT ( 'NONE',  ( -4.164238869374099039, 51.80374883491396787, 8.674139862899312516E-16 ) ) ;
#20946 = CARTESIAN_POINT ( 'NONE',  ( 19.42250999205614548, 50.98035201082151247, -5.440088680355545492 ) ) ;
#20947 = FACE_OUTER_BOUND ( 'NONE', #10478, .T. ) ;
#20948 = PLANE ( 'NONE',  #98860 ) ;
#20949 = CARTESIAN_POINT ( 'NONE',  ( 19.84674366389459621, 48.50893115100078745, 7.409399052514197653E-17 ) ) ;
#20950 = CARTESIAN_POINT ( 'NONE',  ( 12.63842701281683922, 4.550597817667451750, -9.846743663894590881 ) ) ;
#20951 = CARTESIAN_POINT ( 'NONE',  ( 0.1532563361054082862, 21.21726448433412315, 2.638427012816831674 ) ) ;
#20952 = ORIENTED_EDGE ( 'NONE', *, *, #43747, .F. ) ;
#20953 = CARTESIAN_POINT ( 'NONE',  ( 14.92337183194729633, 22.67559781766745175, 8.527530157486181039 ) ) ;
#20954 = CARTESIAN_POINT ( 'NONE',  ( 9.382169495545415572, -12.75136533006957507, -9.382169495545422677 ) ) ;
#20955 = EDGE_CURVE ( 'NONE', #43301, #63180, #52025, .T. ) ;
#20956 =( BOUNDED_SURFACE ( )  B_SPLINE_SURFACE ( 1, 2, ( 
 ( #3518, #12476, #80491, #49983, #27475, #48998, #42980, #72479, #64967, #4504, #71528, #41026, #42014, #34969, #4012, #94986, #96492, #95493, #50473, #4988, #3038, #88972, #64479, #41525, #73460, #35469, #57484, #33488, #65466, #26492, #63987, #94497, #33976, #95993, #26016, #56511, #18508, #79507, #60435, #66458, #74446, #13466, #20980, #45434, #74949, #21969, #67951, #6956, #14463, #29434, #51463, #36962, #98971, #43459, #60926, #82449, #90928, #67457, #44447, #58966, #59938, #97978, #13972, #6452, #81953, #37464, #98475, #43947, #90429, #73961, #29930, #30425, #44938, #22457, #5490, #75444, #89462, #52448, #59447, #82948, #5972, #36466, #14964, #66961, #97479, #52932, #83443, #89948, #75936, #28945, #91432, #7460, #37959, #22959, #68450, #35961, #81461, #21466, #12965, #96992, #28469, #51964, #93397, #76918, #53928, #15934, #9411, #77399, #16921, #15460, #62393, #945, #63387, #85908, #47397, #38442, #46906, #54896, #77899, #31895, #32888, #24922, #93891, #70416, #46424, #17422, #24432, #92901, #32393, #91925, #47890, #16429, #8912, #39913, #45941, #53424, #23937, #85411, #39429, #38935, #40415, #69922, #78392, #9914, #76431, #2431, #8428, #69424, #70911, #83931, #1443, #7946, #31406, #61907, #68939, #469, #92413, #30917, #54406, #61417, #23451, #84918, #4385, #10398, #48871, #86882, #63864, #50348, #18887, #64846, #11868, #42374, #87856, #72355, #94378, #79870, #42863, #86401, #4872, #26372, #34850, #11374, #87372, #35350, #27355, #17903, #95365, #25897, #79383, #65345, #95874, #94870, #49368, #10889, #55903, #3888, #19374, #48386, #34355, #78888, #26864, #3390, #80859, #73345, #57849, #41413, #12356, #40903, #71404, #2920, #52330, #21347, #59818, #58333, #6333, #43829, #7341, #98358, #90313, #81347, #89830, #97858, #21849, #74828, #75820, #67840, #37842, #14344, #89343, #29816, #67332, #29321, #44815, #35847, #60325, #59327, #51838, #82823, #88850, #96372, #66836, #75322, #82325, #81829, #83325, #13845, #6835, #90815, #20358, #45322, #51344, #28346, #37349, #22344, #44327, #14851, #74325, #13345, #52817, #27845, #96870, #50854, #97358, #12843, #43343, #66334, #73840, #5368, #20853, #58836, #5851, #36342, #28827, #8801, #54782, #92787, #1333, #16313, #7834, #23828, #85791, #30307, #47780, #69313, #77783, #54291, #31294, #78279, #70305, #60809, #39316, #45828, #46797, #84804, #834, #61794, #38331, #24317, #85298, #68824, #77290, #91309, #16806, #17305, #31785, #47281, #22837, #62281, #76316, #92302, #46315, #69811, #356, #23335, #1818, #9295, #39803, #32275, #53815, #30805, #68333, #38821, #93281, #62782, #8317 ),
 ( #24805, #84326, #55282, #9792, #98853, #53312, #83820, #15346, #15826, #61303, #91814, #76801, #33739, #57731, #86777, #94260, #72729, #65226, #40786, #64241, #10776, #80742, #40291, #78780, #19252, #25301, #33263, #71285, #10287, #4263, #94759, #11257, #26748, #64729, #72245, #87251, #2808, #56756, #88234, #2316, #19743, #41292, #49736, #18776, #3276, #50227, #42259, #32770, #41774, #17792, #49259, #3779, #71766, #34232, #63754, #95239, #57242, #25786, #87740, #63266, #80244, #70800, #11751, #34734, #93775, #95752, #48267, #27236, #18278, #55788, #56281, #48759, #86284, #79266, #73227, #88728, #58211, #35227, #65725, #4756, #50743, #96251, #27730, #12237, #20239, #42746, #8898, #53916, #62885, #55393, #84905, #76420, #16910, #30906, #7934, #38430, #62380, #31393, #69910, #68438, #16417, #84425, #17409, #9397, #1430, #91419, #932, #39415, #31883, #85893, #61402, #68928, #24418, #54883, #61893, #24909, #15922, #91913, #39898, #32380, #458, #92400, #76903, #47876, #7449, #45929, #85397, #22945, #23437, #46413, #8416, #70404, #23923, #46894, #92886, #47383, #77884, #54394, #38923, #77385, #37946, #98958, #30414, #69409, #1922, #93382, #60914, #53412, #83920, #15450, #84186, #21715, #61648, #14211, #96111, #55362, #1401, #10359, #40858, #69881, #85866, #92372, #71363, #41371, #2880, #33330, #23898, #63824, #39387, #17379, #9367, #78352, #24387, #85367, #94338, #54854, #77857, #25855, #56352, #39870, #9873, #1895, #31367, #40372, #18353, #61867, #70873, #54366, #32842, #62858, #48830, #84876, #2389, #16384, #46869, #26823, #3847, #34305, #58289, #27308, #65797, #64316, #12315, #49814, #13301, #5325, #96331, #87327, #95827, #4830, #27806, #80815, #81786, #73795, #43788, #20318, #95322, #35806, #73307, #42822, #50814, #41849, #66293, #65301, #57807, #88807, #94828, #3347, #72802, #35305, #88315, #87809, #89304, #19814, #81307, #96827, #26331, #28304, #56830, #12802, #79827, #50303, #43302, #34812, #58796, #72315, #20813, #51303, #64803, #33810, #18844, #49324, #11332, #57316, #19330, #80321, #11822, #42328, #4341, #52289, #37308, #82283, #29285, #7792, #44287, #13801, #15301, #91270, #82787, #67797, #36802, #53770, #98316, #7298, #15786, #29770, #66798, #75777, #21807, #30757, #23293, #52777, #74791, #83778, #97823, #6300, #67296, #30266, #60280, #37798, #36302, #83284, #14308, #84286, #76277, #68295, #59291, #90777, #98815, #60769, #14810, #74281, #45785, #5810, #22794, #59782, #38288, #45281, #53271, #68782, #90273, #314, #22304, #61263, #91771, #97318, #28791, #44778, #89789, #21306, #75283, #51798, #6795, #25265, #40739 ) ),
 .UNSPECIFIED., .F., .F., .T. ) 
 B_SPLINE_SURFACE_WITH_KNOTS ( ( 2, 2 ),
 ( 3, 2, 2, 2, 2, 2, 2, 2, 2, 2, 2, 2, 2, 2, 2, 2, 2, 2, 2, 2, 2, 2, 2, 2, 2, 2, 2, 2, 2, 2, 2, 2, 2, 2, 2, 2, 2, 2, 2, 2, 2, 2, 2, 2, 2, 2, 2, 2, 2, 2, 2, 2, 2, 2, 2, 2, 2, 2, 2, 2, 2, 2, 2, 2, 2, 2, 2, 2, 2, 2, 2, 2, 2, 2, 2, 2, 2, 2, 2, 2, 2, 2, 2, 2, 2, 2, 2, 2, 2, 2, 2, 2, 2, 2, 2, 2, 2, 2, 2, 2, 2, 2, 2, 2, 2, 2, 2, 2, 2, 2, 2, 2, 2, 2, 2, 2, 2, 2, 2, 2, 2, 2, 2, 2, 2, 2, 2, 2, 2, 2, 2, 2, 2, 2, 2, 2, 2, 2, 2, 2, 2, 2, 2, 2, 2, 2, 2, 2, 2, 2, 2, 2, 2, 2, 2, 2, 2, 2, 2, 2, 2, 2, 3 ),
 ( 0.000000000000000000, 1.000000000000000000 ),
 ( 0.000000000000000000, 0.005952380952380952051, 0.01190476190476190410, 0.01785714285714285615, 0.02380952380952380820, 0.02976190476190476025, 0.03571428571428571230, 0.04166666666666666435, 0.04761904761904761640, 0.05357142857142856845, 0.05952380952380952051, 0.06547619047619047949, 0.07142857142857142461, 0.07738095238095238360, 0.08333333333333332871, 0.08928571428571428770, 0.09523809523809523281, 0.1011904761904761918, 0.1071428571428571369, 0.1130952380952380959, 0.1190476190476190410, 0.1250000000000000000, 0.1309523809523809590, 0.1369047619047619180, 0.1428571428571428492, 0.1488095238095238082, 0.1547619047619047672, 0.1607142857142857262, 0.1666666666666666574, 0.1726190476190476164, 0.1785714285714285754, 0.1845238095238095344, 0.1904761904761904656, 0.1964285714285714246, 0.2023809523809523836, 0.2083333333333333426, 0.2142857142857142738, 0.2202380952380952328, 0.2261904761904761918, 0.2321428571428571508, 0.2380952380952380820, 0.2440476190476190410, 0.2500000000000000000, 0.2559523809523809312, 0.2619047619047619180, 0.2678571428571428492, 0.2738095238095238360, 0.2797619047619047672, 0.2857142857142856984, 0.2916666666666666852, 0.2976190476190476164, 0.3035714285714285476, 0.3095238095238095344, 0.3154761904761904656, 0.3214285714285714524, 0.3273809523809523836, 0.3333333333333333148, 0.3392857142857143016, 0.3452380952380952328, 0.3511904761904761640, 0.3571428571428571508, 0.3630952380952380820, 0.3690476190476190688, 0.3750000000000000000, 0.3809523809523809312, 0.3869047619047619180, 0.3928571428571428492, 0.3988095238095238360, 0.4047619047619047672, 0.4107142857142856984, 0.4166666666666666852, 0.4226190476190476164, 0.4285714285714285476, 0.4345238095238095344, 0.4404761904761904656, 0.4464285714285714524, 0.4523809523809523836, 0.4583333333333333148, 0.4642857142857143016, 0.4702380952380952328, 0.4761904761904761640, 0.4821428571428571508, 0.4880952380952380820, 0.4940476190476190688, 0.5000000000000000000, 0.5059523809523809312, 0.5119047619047618625, 0.5178571428571429047, 0.5238095238095238360, 0.5297619047619047672, 0.5357142857142856984, 0.5416666666666666297, 0.5476190476190476719, 0.5535714285714286031, 0.5595238095238095344, 0.5654761904761904656, 0.5714285714285713969, 0.5773809523809523281, 0.5833333333333333703, 0.5892857142857143016, 0.5952380952380952328, 0.6011904761904761640, 0.6071428571428570953, 0.6130952380952381375, 0.6190476190476190688, 0.6250000000000000000, 0.6309523809523809312, 0.6369047619047618625, 0.6428571428571429047, 0.6488095238095238360, 0.6547619047619047672, 0.6607142857142856984, 0.6666666666666666297, 0.6726190476190476719, 0.6785714285714286031, 0.6845238095238095344, 0.6904761904761904656, 0.6964285714285713969, 0.7023809523809523281, 0.7083333333333333703, 0.7142857142857143016, 0.7202380952380952328, 0.7261904761904761640, 0.7321428571428570953, 0.7380952380952381375, 0.7440476190476190688, 0.7500000000000000000, 0.7559523809523809312, 0.7619047619047618625, 0.7678571428571429047, 0.7738095238095238360, 0.7797619047619047672, 0.7857142857142856984, 0.7916666666666666297, 0.7976190476190476719, 0.8035714285714286031, 0.8095238095238095344, 0.8154761904761904656, 0.8214285714285713969, 0.8273809523809523281, 0.8333333333333333703, 0.8392857142857143016, 0.8452380952380952328, 0.8511904761904761640, 0.8571428571428570953, 0.8630952380952381375, 0.8690476190476190688, 0.8750000000000000000, 0.8809523809523809312, 0.8869047619047618625, 0.8928571428571429047, 0.8988095238095238360, 0.9047619047619047672, 0.9107142857142856984, 0.9166666666666666297, 0.9226190476190476719, 0.9285714285714286031, 0.9345238095238095344, 0.9404761904761904656, 0.9464285714285713969, 0.9523809523809523281, 0.9583333333333333703, 0.9642857142857143016 ),
 .UNSPECIFIED. ) 
 GEOMETRIC_REPRESENTATION_ITEM ( )  RATIONAL_B_SPLINE_SURFACE ( (
 ( 1.000000000000000000, 0.9659258262890683122, 1.000000000000000000, 0.9659258262890683122, 1.000000000000000000, 0.9659258262890683122, 1.000000000000000000, 0.9659258262890683122, 1.000000000000000000, 0.9659258262890683122, 1.000000000000000000, 0.9659258262890683122, 1.000000000000000000, 0.9659258262890683122, 1.000000000000000000, 0.9659258262890683122, 1.000000000000000000, 0.9659258262890683122, 1.000000000000000000, 0.9659258262890683122, 1.000000000000000000, 0.9659258262890683122, 1.000000000000000000, 0.9659258262890683122, 1.000000000000000000, 0.9659258262890683122, 1.000000000000000000, 0.9659258262890683122, 1.000000000000000000, 0.9659258262890683122, 1.000000000000000000, 0.9659258262890683122, 1.000000000000000000, 0.9659258262890683122, 1.000000000000000000, 0.9659258262890683122, 1.000000000000000000, 0.9659258262890683122, 1.000000000000000000, 0.9659258262890683122, 1.000000000000000000, 0.9659258262890683122, 1.000000000000000000, 0.9659258262890683122, 1.000000000000000000, 0.9659258262890683122, 1.000000000000000000, 0.9659258262890683122, 1.000000000000000000, 0.9659258262890683122, 1.000000000000000000, 0.9659258262890683122, 1.000000000000000000, 0.9659258262890683122, 1.000000000000000000, 0.9659258262890683122, 1.000000000000000000, 0.9659258262890683122, 1.000000000000000000, 0.9659258262890683122, 1.000000000000000000, 0.9659258262890683122, 1.000000000000000000, 0.9659258262890683122, 1.000000000000000000, 0.9659258262890683122, 1.000000000000000000, 0.9659258262890683122, 1.000000000000000000, 0.9659258262890683122, 1.000000000000000000, 0.9659258262890683122, 1.000000000000000000, 0.9659258262890683122, 1.000000000000000000, 0.9659258262890683122, 1.000000000000000000, 0.9659258262890683122, 1.000000000000000000, 0.9659258262890683122, 1.000000000000000000, 0.9659258262890683122, 1.000000000000000000, 0.9659258262890683122, 1.000000000000000000, 0.9659258262890683122, 1.000000000000000000, 0.9659258262890683122, 1.000000000000000000, 0.9659258262890683122, 1.000000000000000000, 0.9659258262890683122, 1.000000000000000000, 0.9659258262890683122, 1.000000000000000000, 0.9659258262890683122, 1.000000000000000000, 0.9659258262890683122, 1.000000000000000000, 0.9659258262890683122, 1.000000000000000000, 0.9659258262890683122, 1.000000000000000000, 0.9659258262890683122, 1.000000000000000000, 0.9659258262890683122, 1.000000000000000000, 0.9659258262890683122, 1.000000000000000000, 0.9659258262890683122, 1.000000000000000000, 0.9659258262890683122, 1.000000000000000000, 0.9659258262890683122, 1.000000000000000000, 0.9659258262890683122, 1.000000000000000000, 0.9659258262890683122, 1.000000000000000000, 0.9659258262890683122, 1.000000000000000000, 0.9659258262890683122, 1.000000000000000000, 0.9659258262890683122, 1.000000000000000000, 0.9659258262890683122, 1.000000000000000000, 0.9659258262890683122, 1.000000000000000000, 0.9659258262890683122, 1.000000000000000000, 0.9659258262890683122, 1.000000000000000000, 0.9659258262890683122, 1.000000000000000000, 0.9659258262890683122, 1.000000000000000000, 0.9659258262890683122, 1.000000000000000000, 0.9659258262890683122, 1.000000000000000000, 0.9659258262890683122, 1.000000000000000000, 0.9659258262890683122, 1.000000000000000000, 0.9659258262890683122, 1.000000000000000000, 0.9659258262890683122, 1.000000000000000000, 0.9659258262890683122, 1.000000000000000000, 0.9659258262890683122, 1.000000000000000000, 0.9659258262890683122, 1.000000000000000000, 0.9659258262890683122, 1.000000000000000000, 0.9659258262890683122, 1.000000000000000000, 0.9659258262890683122, 1.000000000000000000, 0.9659258262890683122, 1.000000000000000000, 0.9659258262890683122, 1.000000000000000000, 0.9659258262890683122, 1.000000000000000000, 0.9659258262890683122, 1.000000000000000000, 0.9659258262890683122, 1.000000000000000000, 0.9659258262890683122, 1.000000000000000000, 0.9659258262890683122, 1.000000000000000000, 0.9659258262890683122, 1.000000000000000000, 0.9659258262890683122, 1.000000000000000000, 0.9659258262890683122, 1.000000000000000000, 0.9659258262890683122, 1.000000000000000000, 0.9659258262890683122, 1.000000000000000000, 0.9659258262890683122, 1.000000000000000000, 0.9659258262890683122, 1.000000000000000000, 0.9659258262890683122, 1.000000000000000000, 0.9659258262890683122, 1.000000000000000000, 0.9659258262890683122, 1.000000000000000000, 0.9659258262890683122, 1.000000000000000000, 0.9659258262890683122, 1.000000000000000000, 0.9659258262890683122, 1.000000000000000000, 0.9659258262890683122, 1.000000000000000000, 0.9659258262890683122, 1.000000000000000000, 0.9659258262890683122, 1.000000000000000000, 0.9659258262890683122, 1.000000000000000000, 0.9659258262890683122, 1.000000000000000000, 0.9659258262890683122, 1.000000000000000000, 0.9659258262890683122, 1.000000000000000000, 0.9659258262890683122, 1.000000000000000000, 0.9659258262890683122, 1.000000000000000000, 0.9659258262890683122, 1.000000000000000000, 0.9659258262890683122, 1.000000000000000000, 0.9659258262890683122, 1.000000000000000000, 0.9659258262890683122, 1.000000000000000000, 0.9659258262890683122, 1.000000000000000000, 0.9659258262890683122, 1.000000000000000000, 0.9659258262890683122, 1.000000000000000000, 0.9659258262890683122, 1.000000000000000000, 0.9659258262890683122, 1.000000000000000000, 0.9659258262890683122, 1.000000000000000000, 0.9659258262890683122, 1.000000000000000000, 0.9659258262890683122, 1.000000000000000000, 0.9659258262890683122, 1.000000000000000000, 0.9659258262890683122, 1.000000000000000000, 0.9659258262890683122, 1.000000000000000000, 0.9659258262890683122, 1.000000000000000000, 0.9659258262890683122, 1.000000000000000000, 0.9659258262890683122, 1.000000000000000000, 0.9659258262890683122, 1.000000000000000000, 0.9659258262890683122, 1.000000000000000000, 0.9659258262890683122, 1.000000000000000000, 0.9659258262890683122, 1.000000000000000000, 0.9659258262890683122, 1.000000000000000000, 0.9659258262890683122, 1.000000000000000000, 0.9659258262890683122, 1.000000000000000000, 0.9659258262890683122, 1.000000000000000000, 0.9659258262890683122, 1.000000000000000000, 0.9659258262890683122, 1.000000000000000000, 0.9659258262890683122, 1.000000000000000000, 0.9659258262890683122, 1.000000000000000000, 0.9659258262890683122, 1.000000000000000000, 0.9659258262890683122, 1.000000000000000000, 0.9659258262890683122, 1.000000000000000000, 0.9659258262890683122, 1.000000000000000000, 0.9659258262890683122, 1.000000000000000000, 0.9659258262890683122, 1.000000000000000000, 0.9659258262890683122, 1.000000000000000000, 0.9659258262890683122, 1.000000000000000000, 0.9659258262890683122, 1.000000000000000000, 0.9659258262890683122, 1.000000000000000000, 0.9659258262890683122, 1.000000000000000000, 0.9659258262890683122, 1.000000000000000000, 0.9659258262890683122, 1.000000000000000000, 0.9659258262890683122, 1.000000000000000000, 0.9659258262890683122, 1.000000000000000000, 0.9659258262890683122, 1.000000000000000000, 0.9659258262890683122, 1.000000000000000000, 0.9659258262890683122, 1.000000000000000000, 0.9659258262890683122, 1.000000000000000000, 0.9659258262890683122, 1.000000000000000000, 0.9659258262890683122, 1.000000000000000000, 0.9659258262890683122, 1.000000000000000000, 0.9659258262890683122, 1.000000000000000000),
 ( 1.000000000000000000, 0.9659258262890683122, 1.000000000000000000, 0.9659258262890683122, 1.000000000000000000, 0.9659258262890683122, 1.000000000000000000, 0.9659258262890683122, 1.000000000000000000, 0.9659258262890683122, 1.000000000000000000, 0.9659258262890683122, 1.000000000000000000, 0.9659258262890683122, 1.000000000000000000, 0.9659258262890683122, 1.000000000000000000, 0.9659258262890683122, 1.000000000000000000, 0.9659258262890683122, 1.000000000000000000, 0.9659258262890683122, 1.000000000000000000, 0.9659258262890683122, 1.000000000000000000, 0.9659258262890683122, 1.000000000000000000, 0.9659258262890683122, 1.000000000000000000, 0.9659258262890683122, 1.000000000000000000, 0.9659258262890683122, 1.000000000000000000, 0.9659258262890683122, 1.000000000000000000, 0.9659258262890683122, 1.000000000000000000, 0.9659258262890683122, 1.000000000000000000, 0.9659258262890683122, 1.000000000000000000, 0.9659258262890683122, 1.000000000000000000, 0.9659258262890683122, 1.000000000000000000, 0.9659258262890683122, 1.000000000000000000, 0.9659258262890683122, 1.000000000000000000, 0.9659258262890683122, 1.000000000000000000, 0.9659258262890683122, 1.000000000000000000, 0.9659258262890683122, 1.000000000000000000, 0.9659258262890683122, 1.000000000000000000, 0.9659258262890683122, 1.000000000000000000, 0.9659258262890683122, 1.000000000000000000, 0.9659258262890683122, 1.000000000000000000, 0.9659258262890683122, 1.000000000000000000, 0.9659258262890683122, 1.000000000000000000, 0.9659258262890683122, 1.000000000000000000, 0.9659258262890683122, 1.000000000000000000, 0.9659258262890683122, 1.000000000000000000, 0.9659258262890683122, 1.000000000000000000, 0.9659258262890683122, 1.000000000000000000, 0.9659258262890683122, 1.000000000000000000, 0.9659258262890683122, 1.000000000000000000, 0.9659258262890683122, 1.000000000000000000, 0.9659258262890683122, 1.000000000000000000, 0.9659258262890683122, 1.000000000000000000, 0.9659258262890683122, 1.000000000000000000, 0.9659258262890683122, 1.000000000000000000, 0.9659258262890683122, 1.000000000000000000, 0.9659258262890683122, 1.000000000000000000, 0.9659258262890683122, 1.000000000000000000, 0.9659258262890683122, 1.000000000000000000, 0.9659258262890683122, 1.000000000000000000, 0.9659258262890683122, 1.000000000000000000, 0.9659258262890683122, 1.000000000000000000, 0.9659258262890683122, 1.000000000000000000, 0.9659258262890683122, 1.000000000000000000, 0.9659258262890683122, 1.000000000000000000, 0.9659258262890683122, 1.000000000000000000, 0.9659258262890683122, 1.000000000000000000, 0.9659258262890683122, 1.000000000000000000, 0.9659258262890683122, 1.000000000000000000, 0.9659258262890683122, 1.000000000000000000, 0.9659258262890683122, 1.000000000000000000, 0.9659258262890683122, 1.000000000000000000, 0.9659258262890683122, 1.000000000000000000, 0.9659258262890683122, 1.000000000000000000, 0.9659258262890683122, 1.000000000000000000, 0.9659258262890683122, 1.000000000000000000, 0.9659258262890683122, 1.000000000000000000, 0.9659258262890683122, 1.000000000000000000, 0.9659258262890683122, 1.000000000000000000, 0.9659258262890683122, 1.000000000000000000, 0.9659258262890683122, 1.000000000000000000, 0.9659258262890683122, 1.000000000000000000, 0.9659258262890683122, 1.000000000000000000, 0.9659258262890683122, 1.000000000000000000, 0.9659258262890683122, 1.000000000000000000, 0.9659258262890683122, 1.000000000000000000, 0.9659258262890683122, 1.000000000000000000, 0.9659258262890683122, 1.000000000000000000, 0.9659258262890683122, 1.000000000000000000, 0.9659258262890683122, 1.000000000000000000, 0.9659258262890683122, 1.000000000000000000, 0.9659258262890683122, 1.000000000000000000, 0.9659258262890683122, 1.000000000000000000, 0.9659258262890683122, 1.000000000000000000, 0.9659258262890683122, 1.000000000000000000, 0.9659258262890683122, 1.000000000000000000, 0.9659258262890683122, 1.000000000000000000, 0.9659258262890683122, 1.000000000000000000, 0.9659258262890683122, 1.000000000000000000, 0.9659258262890683122, 1.000000000000000000, 0.9659258262890683122, 1.000000000000000000, 0.9659258262890683122, 1.000000000000000000, 0.9659258262890683122, 1.000000000000000000, 0.9659258262890683122, 1.000000000000000000, 0.9659258262890683122, 1.000000000000000000, 0.9659258262890683122, 1.000000000000000000, 0.9659258262890683122, 1.000000000000000000, 0.9659258262890683122, 1.000000000000000000, 0.9659258262890683122, 1.000000000000000000, 0.9659258262890683122, 1.000000000000000000, 0.9659258262890683122, 1.000000000000000000, 0.9659258262890683122, 1.000000000000000000, 0.9659258262890683122, 1.000000000000000000, 0.9659258262890683122, 1.000000000000000000, 0.9659258262890683122, 1.000000000000000000, 0.9659258262890683122, 1.000000000000000000, 0.9659258262890683122, 1.000000000000000000, 0.9659258262890683122, 1.000000000000000000, 0.9659258262890683122, 1.000000000000000000, 0.9659258262890683122, 1.000000000000000000, 0.9659258262890683122, 1.000000000000000000, 0.9659258262890683122, 1.000000000000000000, 0.9659258262890683122, 1.000000000000000000, 0.9659258262890683122, 1.000000000000000000, 0.9659258262890683122, 1.000000000000000000, 0.9659258262890683122, 1.000000000000000000, 0.9659258262890683122, 1.000000000000000000, 0.9659258262890683122, 1.000000000000000000, 0.9659258262890683122, 1.000000000000000000, 0.9659258262890683122, 1.000000000000000000, 0.9659258262890683122, 1.000000000000000000, 0.9659258262890683122, 1.000000000000000000, 0.9659258262890683122, 1.000000000000000000, 0.9659258262890683122, 1.000000000000000000, 0.9659258262890683122, 1.000000000000000000, 0.9659258262890683122, 1.000000000000000000, 0.9659258262890683122, 1.000000000000000000, 0.9659258262890683122, 1.000000000000000000, 0.9659258262890683122, 1.000000000000000000, 0.9659258262890683122, 1.000000000000000000, 0.9659258262890683122, 1.000000000000000000, 0.9659258262890683122, 1.000000000000000000, 0.9659258262890683122, 1.000000000000000000, 0.9659258262890683122, 1.000000000000000000, 0.9659258262890683122, 1.000000000000000000, 0.9659258262890683122, 1.000000000000000000, 0.9659258262890683122, 1.000000000000000000, 0.9659258262890683122, 1.000000000000000000, 0.9659258262890683122, 1.000000000000000000, 0.9659258262890683122, 1.000000000000000000, 0.9659258262890683122, 1.000000000000000000, 0.9659258262890683122, 1.000000000000000000, 0.9659258262890683122, 1.000000000000000000, 0.9659258262890683122, 1.000000000000000000, 0.9659258262890683122, 1.000000000000000000, 0.9659258262890683122, 1.000000000000000000, 0.9659258262890683122, 1.000000000000000000, 0.9659258262890683122, 1.000000000000000000, 0.9659258262890683122, 1.000000000000000000, 0.9659258262890683122, 1.000000000000000000, 0.9659258262890683122, 1.000000000000000000, 0.9659258262890683122, 1.000000000000000000, 0.9659258262890683122, 1.000000000000000000, 0.9659258262890683122, 1.000000000000000000, 0.9659258262890683122, 1.000000000000000000, 0.9659258262890683122, 1.000000000000000000, 0.9659258262890683122, 1.000000000000000000, 0.9659258262890683122, 1.000000000000000000, 0.9659258262890683122, 1.000000000000000000, 0.9659258262890683122, 1.000000000000000000, 0.9659258262890683122, 1.000000000000000000, 0.9659258262890683122, 1.000000000000000000) ) ) 
 REPRESENTATION_ITEM ( '' )  SURFACE ( )  );
#20957 = CARTESIAN_POINT ( 'NONE',  ( 0.5774900079438590739, 27.64701867748817676, -5.440088680355550821 ) ) ;
#20958 = CARTESIAN_POINT ( 'NONE',  ( 5.076628168052704559, 25.17559781766745175, -8.527530157486179263 ) ) ;
#20959 = CARTESIAN_POINT ( 'NONE',  ( -2.816281873526473856, 9.331968003263753531, 3.434112377981055619 ) ) ;
#20960 = CARTESIAN_POINT ( 'NONE',  ( 7.084665262690076126, 64.10535201082150536, 10.88017736071109987 ) ) ;
#20962 = CARTESIAN_POINT ( 'NONE',  ( -1.099225684535947600, 54.54030133659708923, 6.408140936763237150 ) ) ;
#20961 = CARTESIAN_POINT ( 'NONE',  ( 20.88017736071110875, 30.77201867748816966, -2.915334737309920765 ) ) ;
#20963 = CARTESIAN_POINT ( 'NONE',  ( 22.26659068614895176, 44.72041550158063927, -7.082119434687042414 ) ) ;
#20964 = ADVANCED_FACE ( 'NONE', ( #90011 ), #74516, .F. ) ;
#20965 =( BOUNDED_SURFACE ( )  B_SPLINE_SURFACE ( 3, 2, ( 
 ( #60834, #83841, #38353 ),
 ( #15366, #30828, #61327 ),
 ( #91838, #53837, #69333 ),
 ( #28850, #54800, #33280 ) ),
 .UNSPECIFIED., .F., .F., .F. ) 
 B_SPLINE_SURFACE_WITH_KNOTS ( ( 4, 4 ),
 ( 3, 3 ),
 ( 0.000000000000000000, 0.0004252381714231216660 ),
 ( 0.000000000000000000, 1.000000000000000000 ),
 .UNSPECIFIED. ) 
 GEOMETRIC_REPRESENTATION_ITEM ( )  RATIONAL_B_SPLINE_SURFACE ( (
 ( 1.000000000000000000, 0.7411386215561424073, 1.000000000000000000),
 ( 1.000000000000000000, 0.7847835171315882263, 1.000000000000000000),
 ( 1.000000000000000000, 0.8182188757360080444, 1.000000000000000000),
 ( 1.000000000000000000, 0.8414823709351041403, 1.000000000000000000) ) ) 
 REPRESENTATION_ITEM ( '' )  SURFACE ( )  );
#20966 = AXIS2_PLACEMENT_3D ( 'NONE', #84491, #61476, #75502 ) ;
#20967 = CARTESIAN_POINT ( 'NONE',  ( -42.50123216575902063, 107.2490263651838802, 4.999999999999999112 ) ) ;
#20968 = EDGE_LOOP ( 'NONE', ( #55828, #52059, #67309, #28237, #602, #29738 ) ) ;
#20969 = CARTESIAN_POINT ( 'NONE',  ( 0.6178305044545818747, 3.498634669930420049, -9.382169495545419124 ) ) ;
#20970 = CARTESIAN_POINT ( 'NONE',  ( 10.00000000000000000, 11.81368534415483751, -10.88017736071110342 ) ) ;
#20971 = CARTESIAN_POINT ( 'NONE',  ( 0.5774900079438590739, 42.64701867748816966, -5.440088680355550821 ) ) ;
#20972 = MECHANICAL_DESIGN_GEOMETRIC_PRESENTATION_REPRESENTATION (  '', ( #56087 ), #81682 ) ;
#20973 = CARTESIAN_POINT ( 'NONE',  ( 17.39651004071842522, 24.08210964143329491, -6.499999999999992895 ) ) ;
#20974 = ORIENTED_EDGE ( 'NONE', *, *, #45429, .T. ) ;
#20976 = CARTESIAN_POINT ( 'NONE',  ( 1.274849032794305170, 17.55509018479936145, -6.499999999999995559 ) ) ;
#20975 = CARTESIAN_POINT ( 'NONE',  ( 0.1532563361054100626, 20.80059781766744464, -2.638427012816831230 ) ) ;
#20977 = CARTESIAN_POINT ( 'NONE',  ( 7.084665262690076126, 64.10535201082150536, 10.88017736071109987 ) ) ;
#20978 = CARTESIAN_POINT ( 'NONE',  ( 0.1532563361054083140, 36.00893115100078745, 1.131784320476157264E-15 ) ) ;
#20979 = CARTESIAN_POINT ( 'NONE',  ( 2.791683348922240793, 26.63393115100078745, 7.208316651077764092 ) ) ;
#20980 = CARTESIAN_POINT ( 'NONE',  ( 19.84674366389459621, 8.508931151000785675, 7.409399052514197653E-17 ) ) ;
#20981 = CARTESIAN_POINT ( 'NONE',  ( -5.809210876199123241, -36.07757871006187855, 2.750000000000000444 ) ) ;
#20982 = CARTESIAN_POINT ( 'NONE',  ( 4.559911319644449179, 68.89701867748817676, 9.422509992056141925 ) ) ;
#20984 = VERTEX_POINT ( 'NONE', #52507 ) ;
#20983 = CARTESIAN_POINT ( 'NONE',  ( 7.361572987183170547, 37.05059781766744464, 9.846743663894590881 ) ) ;
#20985 = CARTESIAN_POINT ( 'NONE',  ( 10.00000000000000000, 52.87363466993041783, -12.81628187352647608 ) ) ;
#20986 = CARTESIAN_POINT ( 'NONE',  ( 7.155629327958949126, -69.45263185074755086, 3.999999999999999112 ) ) ;
#20987 = CARTESIAN_POINT ( 'NONE',  ( 5.076628168052704559, 65.17559781766745175, -8.527530157486179263 ) ) ;
#20988 = CARTESIAN_POINT ( 'NONE',  ( 0.5774900079438590739, 2.647018677488170990, -5.440088680355550821 ) ) ;
#20989 = CARTESIAN_POINT ( 'NONE',  ( 22.26659068614894466, 23.88708216824730357, 7.082119434687054849 ) ) ;
#20990 = CARTESIAN_POINT ( 'NONE',  ( -14.88232117145535405, 0.3639310251205940538, 1.875237731503057281 ) ) ;
#20991 = CARTESIAN_POINT ( 'NONE',  ( 2.917880565312948704, 22.63708216824730002, 12.26659068614894643 ) ) ;
#20992 = CARTESIAN_POINT ( 'NONE',  ( 2.917880565312948704, 52.63708216824730357, 12.26659068614894643 ) ) ;
#20994 = CARTESIAN_POINT ( 'NONE',  ( 17.96484262340118221, 66.18868534415483396, -7.964842623401177768 ) ) ;
#20993 = CARTESIAN_POINT ( 'NONE',  ( 10.00000000000000178, 8.053748834913967869, 14.16423886937410082 ) ) ;
#20995 = CARTESIAN_POINT ( 'NONE',  ( 19.42250999205614548, 50.98035201082151247, -5.440088680355545492 ) ) ;
#20996 = CARTESIAN_POINT ( 'NONE',  ( 6.732888861736110009, -58.30752899003807954, -2.750000000000000000 ) ) ;
#20997 = CARTESIAN_POINT ( 'NONE',  ( 17.20831665107776587, 24.13393115100078035, -7.208316651077762316 ) ) ;
#20999 = CARTESIAN_POINT ( 'NONE',  ( 5.076628168052704559, 30.17559781766745175, -8.527530157486179263 ) ) ;
#20998 = CARTESIAN_POINT ( 'NONE',  ( 5.377205135395962010, 0.2306972965111855067, -13.94000429068781877 ) ) ;
#21000 = CARTESIAN_POINT ( 'NONE',  ( 0.5774900079438607392, 13.48035201082150358, 5.440088680355550821 ) ) ;
#21001 = CARTESIAN_POINT ( 'NONE',  ( 3.591859063236763294, 53.29030133659708923, -11.09922568453595026 ) ) ;
#21002 = CARTESIAN_POINT ( 'NONE',  ( 19.84674366389459266, 48.30059781766745175, 2.638427012816836559 ) ) ;
#21003 = FACE_OUTER_BOUND ( 'NONE', #64322, .T. ) ;
#21004 = EDGE_CURVE ( 'NONE', #72511, #57827, #4916, .T. ) ;
#21005 = CARTESIAN_POINT ( 'NONE',  ( 7.361572987183170547, 32.05059781766745175, 9.846743663894590881 ) ) ;
#21006 = CARTESIAN_POINT ( 'NONE',  ( -2.816281873526473856, 39.33196800326374643, 3.434112377981055619 ) ) ;
#21007 = CARTESIAN_POINT ( 'NONE',  ( -5.204170427930421283E-15, -24.44625116508603213, -14.16423886937410082 ) ) ;
#21008 = CARTESIAN_POINT ( 'NONE',  ( 17.96484262340118221, 46.18868534415484106, -7.964842623401177768 ) ) ;
#21009 = CARTESIAN_POINT ( 'NONE',  ( 17.20831665107776587, 39.13393115100079456, -7.208316651077762316 ) ) ;
#21010 = CARTESIAN_POINT ( 'NONE',  ( 10.00000000000000178, 23.05374883491397142, 14.16423886937410082 ) ) ;
#21011 = ORIENTED_EDGE ( 'NONE', *, *, #15294, .F. ) ;
#21012 = CARTESIAN_POINT ( 'NONE',  ( -27.43587634952537968, 22.49999999999998934, -10.00000000000000000 ) ) ;
#21013 = CARTESIAN_POINT ( 'NONE',  ( 17.96484262340118221, 49.93868534415484106, 7.964842623401181321 ) ) ;
#21014 = CARTESIAN_POINT ( 'NONE',  ( -0.8801773607110991993, 67.85535201082151957, -2.915334737309923874 ) ) ;
#21015 = CARTESIAN_POINT ( 'NONE',  ( 22.26659068614895176, 49.72041550158063927, -7.082119434687042414 ) ) ;
#21016 = CARTESIAN_POINT ( 'NONE',  ( 10.00000000000000000, 2.873634669930420049, -12.81628187352647608 ) ) ;
#21017 = CARTESIAN_POINT ( 'NONE',  ( 15.96747533562963639, 15.00000000000000000, -0.9576679184940652956 ) ) ;
#21018 = CARTESIAN_POINT ( 'NONE',  ( 10.00000000000000178, 49.31368534415484106, 10.88017736071110342 ) ) ;
#21019 = DIRECTION ( 'NONE',  ( -1.000000000000000000, 0.000000000000000000, 0.000000000000000000 ) ) ;
#21020 = CARTESIAN_POINT ( 'NONE',  ( -2.816281873526471635, 28.91530133659708213, -3.434112377981056508 ) ) ;
#21021 = CARTESIAN_POINT ( 'NONE',  ( 6.565887622018943937, 3.081968003263753531, -12.81628187352647608 ) ) ;
#21022 = CARTESIAN_POINT ( 'NONE',  ( 3.469446951953614189E-15, 34.31368534415485527, 10.88017736071110342 ) ) ;
#21023 = CARTESIAN_POINT ( 'NONE',  ( 10.00000000000000178, 19.31368534415484106, 10.88017736071110342 ) ) ;
#21024 = CARTESIAN_POINT ( 'NONE',  ( 0.5774900079438607392, 13.48035201082150358, 5.440088680355550821 ) ) ;
#21025 = CARTESIAN_POINT ( 'NONE',  ( 12.63842701281683922, 44.55059781766745175, -9.846743663894590881 ) ) ;
#21026 = CARTESIAN_POINT ( 'NONE',  ( -14.56332774647475858, 0.04922511925147020351, 2.357028871694085481 ) ) ;
#21027 = ORIENTED_EDGE ( 'NONE', *, *, #36345, .T. ) ;
#21028 = FILL_AREA_STYLE ('',( #87543 ) ) ;
#21029 = CARTESIAN_POINT ( 'NONE',  ( 17.20831665107776587, 9.133931151000787452, -7.208316651077762316 ) ) ;
#21030 =( GEOMETRIC_REPRESENTATION_CONTEXT ( 3 ) GLOBAL_UNCERTAINTY_ASSIGNED_CONTEXT ( ( #14289 ) ) GLOBAL_UNIT_ASSIGNED_CONTEXT ( ( #40489, #26443, #78472 ) ) REPRESENTATION_CONTEXT ( 'NONE', 'WORKASPACE' ) );
#21031 = EDGE_CURVE ( 'NONE', #20454, #95449, #58524, .T. ) ;
#21032 = CARTESIAN_POINT ( 'NONE',  ( 5.076628168052703671, 36.84226448433412315, 8.527530157486179263 ) ) ;
#21033 = CARTESIAN_POINT ( 'NONE',  ( 12.91533473730993009, 31.60535201082150891, -10.88017736071109987 ) ) ;
#21034 = CARTESIAN_POINT ( 'NONE',  ( 21.09922568453594849, 6.206968003263753531, 6.408140936763242479 ) ) ;
#21036 = CARTESIAN_POINT ( 'NONE',  ( 13.86102707272219980, 15.00000000000000711, 4.666951904077296653 ) ) ;
#21035 = CARTESIAN_POINT ( 'NONE',  ( 12.91533473730992121, 39.52201867748817676, 10.88017736071110164 ) ) ;
#21037 = CARTESIAN_POINT ( 'NONE',  ( 0.000000000000000000, 0.000000000000000000, 0.000000000000000000 ) ) ;
#21038 = CARTESIAN_POINT ( 'NONE',  ( -2.816281873526473856, 49.33196800326374643, 3.434112377981055619 ) ) ;
#21039 = ORIENTED_EDGE ( 'NONE', *, *, #8530, .F. ) ;
#21040 = CARTESIAN_POINT ( 'NONE',  ( 20.88017736071110875, 60.77201867748817676, -2.915334737309920765 ) ) ;
#21041 = EDGE_CURVE ( 'NONE', #64665, #24788, #68799, .T. ) ;
#21043 = CARTESIAN_POINT ( 'NONE',  ( 2.917880565312948704, 2.637082168247300906, 12.26659068614894643 ) ) ;
#21042 = CARTESIAN_POINT ( 'NONE',  ( 6.565887622018943937, 35.16530133659708923, 12.81628187352647430 ) ) ;
#21044 =( LENGTH_UNIT ( ) NAMED_UNIT ( * ) SI_UNIT ( .MILLI., .METRE. ) );
#21045 = CARTESIAN_POINT ( 'NONE',  ( 0.5774900079438590739, 42.64701867748816966, -5.440088680355550821 ) ) ;
#21046 = CARTESIAN_POINT ( 'NONE',  ( 12.63842701281683922, 64.55059781766745175, -9.846743663894590881 ) ) ;
#21047 = CARTESIAN_POINT ( 'NONE',  ( 2.791683348922240793, 56.63393115100078035, 7.208316651077764092 ) ) ;
#21048 = CARTESIAN_POINT ( 'NONE',  ( 2.791683348922237240, 20.38393115100078745, -7.208316651077763204 ) ) ;
#21049 = CARTESIAN_POINT ( 'NONE',  ( 17.96484262340118221, 61.18868534415482685, -7.964842623401177768 ) ) ;
#21050 = CARTESIAN_POINT ( 'NONE',  ( -0.1503990784575328643, 5.127771745786130708, 6.262539305110068177 ) ) ;
#21051 = CARTESIAN_POINT ( 'NONE',  ( -0.3689425029237898834, 26.17874883491396432, -10.36894250292378850 ) ) ;
#21052 = VECTOR ( 'NONE', #77538, 1000.000000000000114 ) ;
#21053 = DIRECTION ( 'NONE',  ( 0.000000000000000000, -1.000000000000000000, 0.000000000000000000 ) ) ;
#21054 = CARTESIAN_POINT ( 'NONE',  ( 11.33948230079944253, -87.84096554735758389, -3.749999999999999556 ) ) ;
#21055 = VERTEX_POINT ( 'NONE', #27535 ) ;
#21056 = CARTESIAN_POINT ( 'NONE',  ( -2.266590686148945544, 57.22041550158063217, 7.082119434687048631 ) ) ;
#21057 = CARTESIAN_POINT ( 'NONE',  ( 17.08211943468705130, 58.47041550158063927, 12.26659068614894998 ) ) ;
#21058 = CARTESIAN_POINT ( 'NONE',  ( 10.00000000000000000, 34.75893115100078745, -9.846743663894594434 ) ) ;
#21059 = CARTESIAN_POINT ( 'NONE',  ( 21.09922568453595559, 22.04030133659708923, -6.408140936763230044 ) ) ;
#21060 = DIRECTION ( 'NONE',  ( 0.000000000000000000, 0.000000000000000000, 1.000000000000000000 ) ) ;
#21061 = CARTESIAN_POINT ( 'NONE',  ( 12.91533473730992121, 14.52201867748817143, 10.88017736071110164 ) ) ;
#21062 = CARTESIAN_POINT ( 'NONE',  ( 10.00000000000000000, 55.55374883491396787, -14.16423886937410082 ) ) ;
#21063 = CARTESIAN_POINT ( 'NONE',  ( 7.361572987183170547, 27.05059781766745175, 9.846743663894590881 ) ) ;
#21064 = CARTESIAN_POINT ( 'NONE',  ( 10.84451454130500636, 4.196149184706192213E-16, 9.625305416630906663 ) ) ;
#21065 = CARTESIAN_POINT ( 'NONE',  ( 17.20831665107776587, 14.13393115100078568, -7.208316651077762316 ) ) ;
#21066 = CARTESIAN_POINT ( 'NONE',  ( 17.39651004071841811, 4.082109641433293135, -6.499999999999999112 ) ) ;
#21067 = CARTESIAN_POINT ( 'NONE',  ( -9.846743663894596210, 10.80059781766745530, -2.638427012816824124 ) ) ;
#21068 = EDGE_LOOP ( 'NONE', ( #5179, #13547, #39389, #10641, #14163, #93641 ) ) ;
#21069 = EDGE_LOOP ( 'NONE', ( #74533, #5260, #60734, #39903 ) ) ;
#21070 = DIRECTION ( 'NONE',  ( 0.5547001962252290364, 0.8320502943378437211, 0.000000000000000000 ) ) ;
#21071 = ORIENTED_EDGE ( 'NONE', *, *, #27915, .T. ) ;
#21072 = CARTESIAN_POINT ( 'NONE',  ( -2.266590686148945544, 16.38708216824730357, -7.082119434687050408 ) ) ;
#21074 = CARTESIAN_POINT ( 'NONE',  ( 4.559911319644449179, 27.23035201082150536, -9.422509992056141925 ) ) ;
#21073 = CARTESIAN_POINT ( 'NONE',  ( -0.8801773607111009756, 18.06368534415484106, 1.068504757029289695E-15 ) ) ;
#21076 = CARTESIAN_POINT ( 'NONE',  ( -1.099225684535947600, 13.70696800326375353, -6.408140936763238038 ) ) ;
#21075 = CARTESIAN_POINT ( 'NONE',  ( 10.00000000000000000, 59.75893115100078745, -9.846743663894594434 ) ) ;
#21077 = CARTESIAN_POINT ( 'NONE',  ( 24.16423886937410614, 4.303748834913967869, 8.672049930838204340E-16 ) ) ;
#21078 = EDGE_CURVE ( 'NONE', #59804, #76742, #6036, .T. ) ;
#21079 = AXIS2_PLACEMENT_3D ( 'NONE', #49688, #87691, #96201 ) ;
#21080 = CARTESIAN_POINT ( 'NONE',  ( 16.40814093676323893, 30.79030133659708923, 11.09922568453595026 ) ) ;
#21081 = VERTEX_POINT ( 'NONE', #58028 ) ;
#21082 = CARTESIAN_POINT ( 'NONE',  ( 19.84674366389459621, 28.50893115100078745, 7.409399052514197653E-17 ) ) ;
#21083 = CARTESIAN_POINT ( 'NONE',  ( 19.42250999205614548, 5.980352010821504471, -5.440088680355545492 ) ) ;
#21084 = ORIENTED_EDGE ( 'NONE', *, *, #24016, .F. ) ;
#21085 = CARTESIAN_POINT ( 'NONE',  ( 20.36894250292379738, 64.92874883491397497, -10.36894250292379027 ) ) ;
#21086 = ORIENTED_EDGE ( 'NONE', *, *, #38357, .F. ) ;
#21087 = CARTESIAN_POINT ( 'NONE',  ( 7.084665262690076126, 42.02201867748816966, -10.88017736071110164 ) ) ;
#21088 = CARTESIAN_POINT ( 'NONE',  ( 2.035157376598824452, 63.68868534415484106, 7.964842623401179544 ) ) ;
#21089 = CARTESIAN_POINT ( 'NONE',  ( 20.88017736071110875, 45.77201867748816966, -2.915334737309920765 ) ) ;
#21090 =( LENGTH_UNIT ( ) NAMED_UNIT ( * ) SI_UNIT ( .MILLI., .METRE. ) );
#21091 = CARTESIAN_POINT ( 'NONE',  ( -0.8801773607111008646, 58.27201867748816966, 2.915334737309923430 ) ) ;
#21092 = CYLINDRICAL_SURFACE ( 'NONE', #41098, 15.00000000000000000 ) ;
#21095 = ORIENTED_EDGE ( 'NONE', *, *, #42772, .F. ) ;
#21094 = AXIS2_PLACEMENT_3D ( 'NONE', #50726, #35715, #30175 ) ;
#21093 = SURFACE_SIDE_STYLE ('',( #91565 ) ) ;
#21096 = CARTESIAN_POINT ( 'NONE',  ( 10.00000000000000178, 27.25893115100078390, 9.846743663894594434 ) ) ;
#21097 = VERTEX_POINT ( 'NONE', #97545 ) ;
#21098 = CARTESIAN_POINT ( 'NONE',  ( 0.1532563361054082862, 56.21726448433411605, 2.638427012816831674 ) ) ;
#21099 = LINE ( 'NONE', #81585, #50074 ) ;
#21100 = CIRCLE ( 'NONE', #76984, 1.000000000000000888 ) ;
#21101 = AXIS2_PLACEMENT_3D ( 'NONE', #53516, #75036, #563 ) ;
#21102 = CARTESIAN_POINT ( 'NONE',  ( -4.164238869374099927, 12.01208216824730357, 3.795296366450308767 ) ) ;
#21103 = ORIENTED_EDGE ( 'NONE', *, *, #55564, .F. ) ;
#21104 = CARTESIAN_POINT ( 'NONE',  ( 17.99999999999999645, 91.28723161455539525, -8.000000000000000000 ) ) ;
#21105 = CARTESIAN_POINT ( 'NONE',  ( -7.121361074407936975, -73.24646532379340158, 3.749999999999999556 ) ) ;
#21106 = DIRECTION ( 'NONE',  ( -0.000000000000000000, -1.000000000000000000, -0.000000000000000000 ) ) ;
#21107 = CARTESIAN_POINT ( 'NONE',  ( 2.035157376598824452, 3.688685344154837953, 7.964842623401179544 ) ) ;
#21108 = FACE_OUTER_BOUND ( 'NONE', #22315, .T. ) ;
#21109 = VERTEX_POINT ( 'NONE', #81033 ) ;
#21111 = VECTOR ( 'NONE', #84837, 1000.000000000000000 ) ;
#21110 = CARTESIAN_POINT ( 'NONE',  ( 9.383795276901770066, 14.76930270348882601, -11.62679839395692305 ) ) ;
#21112 = CARTESIAN_POINT ( 'NONE',  ( 19.84674366389459266, 43.71726448433410894, -2.638427012816827677 ) ) ;
#21113 = CARTESIAN_POINT ( 'NONE',  ( 16.40814093676324603, 12.45696800326375353, -11.09922568453594671 ) ) ;
#21114 = CARTESIAN_POINT ( 'NONE',  ( 2.791683348922237240, 10.38393115100078390, -7.208316651077763204 ) ) ;
#21115 = FACE_OUTER_BOUND ( 'NONE', #87748, .T. ) ;
#21116 = EDGE_CURVE ( 'NONE', #55876, #57707, #25043, .T. ) ;
#21117 = CARTESIAN_POINT ( 'NONE',  ( 0.1532563361054100626, 10.80059781766745175, -2.638427012816831230 ) ) ;
#21118 = CARTESIAN_POINT ( 'NONE',  ( 6.565887622018943937, -1.918031996736246692, -12.81628187352647608 ) ) ;
#21119 = VECTOR ( 'NONE', #43755, 1000.000000000000000 ) ;
#21120 = CARTESIAN_POINT ( 'NONE',  ( 1.472469842513823179, 26.42559781766745175, 4.923371831947296329 ) ) ;
#21121 = EDGE_CURVE ( 'NONE', #83598, #26486, #73521, .T. ) ;
#21122 = EDGE_CURVE ( 'NONE', #18240, #72111, #89558, .T. ) ;
#21123 = ORIENTED_EDGE ( 'NONE', *, *, #57955, .F. ) ;
#21124 = CARTESIAN_POINT ( 'NONE',  ( 10.00000000000000000, 11.81368534415483751, -10.88017736071110342 ) ) ;
#21125 = CARTESIAN_POINT ( 'NONE',  ( 13.79529636645031943, 10.34541550158063394, -14.16423886937409904 ) ) ;
#21126 = CARTESIAN_POINT ( 'NONE',  ( 2.791683348922240793, 31.63393115100078745, 7.208316651077764092 ) ) ;
#21127 = CARTESIAN_POINT ( 'NONE',  ( 20.88017736071110519, 60.56368534415484106, 2.639326808657452039E-16 ) ) ;
#21129 = FILL_AREA_STYLE_COLOUR ( '', #22600 ) ;
#21128 = CARTESIAN_POINT ( 'NONE',  ( 16.40814093676324603, 22.45696800326375353, -11.09922568453594671 ) ) ;
#21130 = CARTESIAN_POINT ( 'NONE',  ( 20.88017736071110519, 10.56368534415483751, 2.639326808657452039E-16 ) ) ;
#21131 = DIRECTION ( 'NONE',  ( 0.5547001962252290364, 0.8320502943378437211, 0.000000000000000000 ) ) ;
#21132 = CARTESIAN_POINT ( 'NONE',  ( 15.00000000000000000, 77.07179676972447169, -6.500000000000000888 ) ) ;
#21133 = CARTESIAN_POINT ( 'NONE',  ( 1.472469842513823179, 61.42559781766745175, 4.923371831947296329 ) ) ;
#21134 = CARTESIAN_POINT ( 'NONE',  ( 17.20831665107776587, 34.13393115100078745, -7.208316651077762316 ) ) ;
#21135 = CARTESIAN_POINT ( 'NONE',  ( -9.422509992056136596, -11.51964798917848931, 5.440088680355559703 ) ) ;
#21136 = CARTESIAN_POINT ( 'NONE',  ( 3.591859063236761518, 39.95696800326375353, 11.09922568453594849 ) ) ;
#21138 = CARTESIAN_POINT ( 'NONE',  ( 20.15039907845753575, 6.748846992468889638, 6.262539305110063736 ) ) ;
#21137 = CARTESIAN_POINT ( 'NONE',  ( 4.559911319644449179, 33.89701867748817676, 9.422509992056141925 ) ) ;
#21139 = FACE_OUTER_BOUND ( 'NONE', #59243, .T. ) ;
#21140 = CARTESIAN_POINT ( 'NONE',  ( 17.96484262340118221, 26.18868534415483396, -7.964842623401177768 ) ) ;
#21142 = CARTESIAN_POINT ( 'NONE',  ( 19.42250999205614193, 30.14701867748817321, 5.440088680355555262 ) ) ;
#21141 = AXIS2_PLACEMENT_3D ( 'NONE', #24910, #48862, #1923 ) ;
#21143 = CARTESIAN_POINT ( 'NONE',  ( 17.20831665107776587, 52.88393115100078035, 7.208316651077764980 ) ) ;
#21144 = EDGE_CURVE ( 'NONE', #65098, #58411, #10742, .T. ) ;
#21145 = CARTESIAN_POINT ( 'NONE',  ( -0.8801773607111009756, 48.06368534415484817, 1.068504757029289695E-15 ) ) ;
#21146 = CARTESIAN_POINT ( 'NONE',  ( -4.164238869374099039, 31.80374883491396432, 8.674139862899312516E-16 ) ) ;
#21147 = UNCERTAINTY_MEASURE_WITH_UNIT (LENGTH_MEASURE( 1.000000000000000082E-05 ), #21090, 'distance_accuracy_value', 'NONE');
#21148 = CARTESIAN_POINT ( 'NONE',  ( 5.076628168052703671, 31.84226448433412315, 8.527530157486179263 ) ) ;
#21149 = CARTESIAN_POINT ( 'NONE',  ( -2.816281873526473856, -0.8763653300695799508, 9.499525473075851096E-16 ) ) ;
#21150 = ORIENTED_EDGE ( 'NONE', *, *, #29943, .F. ) ;
#21151 = CARTESIAN_POINT ( 'NONE',  ( 4.559911319644449179, 22.23035201082150536, -9.422509992056141925 ) ) ;
#21152 = EDGE_CURVE ( 'NONE', #44437, #54112, #22473, .T. ) ;
#21153 = DIRECTION ( 'NONE',  ( -0.000000000000000000, -1.000000000000000000, -0.000000000000000000 ) ) ;
#21154 = CARTESIAN_POINT ( 'NONE',  ( 4.559911319644449179, 18.89701867748817321, 9.422509992056141925 ) ) ;
#21155 = CARTESIAN_POINT ( 'NONE',  ( 7.084665262690076126, 64.10535201082150536, 10.88017736071109987 ) ) ;
#21156 = CARTESIAN_POINT ( 'NONE',  ( -2.266590686148945544, 21.38708216824730357, -7.082119434687050408 ) ) ;
#21157 = CARTESIAN_POINT ( 'NONE',  ( 1.472469842513823179, 15.59226448433411960, -4.923371831947296329 ) ) ;
#21158 = CARTESIAN_POINT ( 'NONE',  ( 18.52753015748618282, 58.92559781766745886, -4.923371831947291888 ) ) ;
#21159 = CARTESIAN_POINT ( 'NONE',  ( 2.035157376598824452, 43.68868534415484106, 7.964842623401179544 ) ) ;
#21160 = CARTESIAN_POINT ( 'NONE',  ( -0.04758788293964817673, 0.000000000000000000, -5.453031268574420665 ) ) ;
#21161 = CARTESIAN_POINT ( 'NONE',  ( -45.35355022568786154, 104.5915939144275342, -5.642319926932224838 ) ) ;
#21162 = VERTEX_POINT ( 'NONE', #91987 ) ;
#21163 = VECTOR ( 'NONE', #89603, 1000.000000000000000 ) ;
#21164 = DIRECTION ( 'NONE',  ( -0.000000000000000000, -1.000000000000000000, -0.000000000000000000 ) ) ;
#21165 = CARTESIAN_POINT ( 'NONE',  ( 5.076628168052704559, 40.17559781766745175, -8.527530157486179263 ) ) ;
#21166 = VERTEX_POINT ( 'NONE', #1511 ) ;
#21167 = ORIENTED_EDGE ( 'NONE', *, *, #26397, .T. ) ;
#21168 = CARTESIAN_POINT ( 'NONE',  ( 13.79529636645030344, 18.26208216824730002, 14.16423886937410614 ) ) ;
#21169 = CARTESIAN_POINT ( 'NONE',  ( 6.204703633549690345, 20.76208216824730357, -14.16423886937410259 ) ) ;
#21170 = CARTESIAN_POINT ( 'NONE',  ( 20.88017736071110519, 55.56368534415484817, 2.639326808657452039E-16 ) ) ;
#21171 = CARTESIAN_POINT ( 'NONE',  ( 20.36894250292379382, 48.67874883491396076, 10.36894250292379205 ) ) ;
#21172 = CARTESIAN_POINT ( 'NONE',  ( 12.63842701281683922, 64.55059781766745175, -9.846743663894590881 ) ) ;
#21173 = CARTESIAN_POINT ( 'NONE',  ( 1.472469842513823179, 46.42559781766745175, 4.923371831947296329 ) ) ;
#21174 = CARTESIAN_POINT ( 'NONE',  ( -11.26393249273843011, -93.42496533368144185, 3.750000000000000000 ) ) ;
#21176 = CARTESIAN_POINT ( 'NONE',  ( 10.00000000000000178, 5.373634669930420493, 12.81628187352647608 ) ) ;
#21175 = CARTESIAN_POINT ( 'NONE',  ( 19.42250999205614548, 50.98035201082151247, -5.440088680355545492 ) ) ;
#21177 = CARTESIAN_POINT ( 'NONE',  ( 6.204703633549690345, 22.84541550158062861, 14.16423886937410082 ) ) ;
#21178 = CARTESIAN_POINT ( 'NONE',  ( -4.164238869374098151, 46.59541550158063927, -3.795296366450310543 ) ) ;
#21179 = PRESENTATION_LAYER_ASSIGNMENT (  '', '', ( #94609 ) ) ;
#21180 = CARTESIAN_POINT ( 'NONE',  ( 19.42250999205614193, 25.14701867748817321, 5.440088680355555262 ) ) ;
#21181 = AXIS2_PLACEMENT_3D ( 'NONE', #67356, #80879, #87876 ) ;
#21182 = CARTESIAN_POINT ( 'NONE',  ( -1.926860441876564023, 2.870456701841137992, 3.195792623639529761 ) ) ;
#21183 = CARTESIAN_POINT ( 'NONE',  ( -0.8801773607111009756, 38.06368534415484106, 1.068504757029289695E-15 ) ) ;
#21184 = AXIS2_PLACEMENT_3D ( 'NONE', #52358, #37375, #82859 ) ;
#21185 = CARTESIAN_POINT ( 'NONE',  ( 4.923371831947301658, -27.32440218233254114, 8.527530157486175710 ) ) ;
#21186 = ORIENTED_EDGE ( 'NONE', *, *, #61966, .T. ) ;
#21187 = DIRECTION ( 'NONE',  ( -0.000000000000000000, -0.000000000000000000, 1.000000000000000000 ) ) ;
#21188 = STYLED_ITEM ( 'NONE', ( #96284 ), #76770 ) ;
#21189 = ORIENTED_EDGE ( 'NONE', *, *, #8524, .F. ) ;
#21190 = VERTEX_POINT ( 'NONE', #39496 ) ;
#21191 = CARTESIAN_POINT ( 'NONE',  ( 22.26659068614895176, 44.72041550158063927, -7.082119434687042414 ) ) ;
#21192 = CARTESIAN_POINT ( 'NONE',  ( 19.84674366389459621, 48.50893115100078745, 7.409399052514197653E-17 ) ) ;
#21193 = CARTESIAN_POINT ( 'NONE',  ( 7.084665262690076126, 69.10535201082151957, 10.88017736071109987 ) ) ;
#21194 = CARTESIAN_POINT ( 'NONE',  ( -10.00000000000000000, 82.00000000000000000, 5.000000000000000000 ) ) ;
#21195 = EDGE_CURVE ( 'NONE', #39466, #69849, #91500, .T. ) ;
#21196 = COLOUR_RGB ( '', 0.09019608, 0.27058824, 0.51372549) ;
#21197 = CARTESIAN_POINT ( 'NONE',  ( -0.8801773607111008646, 58.27201867748816966, 2.915334737309923430 ) ) ;
#21198 = B_SPLINE_CURVE_WITH_KNOTS ( 'NONE', 3,
 ( #46877, #8879, #25385, #85376, #47856, #48840, #86367, #94346, #40870, #48351 ),
 .UNSPECIFIED., .F., .F.,
 ( 4, 3, 3, 4 ),
 ( 2.388396739587122319E-17, 0.0006253016069560766348, 0.001250604074564918254, 0.002501455912506555211 ),
 .UNSPECIFIED. ) ;
#21199 = CARTESIAN_POINT ( 'NONE',  ( 0.6178305044545818747, 58.49863466993042493, -9.382169495545419124 ) ) ;
#21200 = CARTESIAN_POINT ( 'NONE',  ( -6.408140936763232709, 4.956968003263756195, 11.09922568453595026 ) ) ;
#21201 = ORIENTED_EDGE ( 'NONE', *, *, #7939, .F. ) ;
#21202 = CARTESIAN_POINT ( 'NONE',  ( 13.79529636645030344, 38.26208216824729647, 14.16423886937410614 ) ) ;
#21203 = CARTESIAN_POINT ( 'NONE',  ( 19.38216949554541202, 25.99863466993042138, 9.382169495545424454 ) ) ;
#21204 = ORIENTED_EDGE ( 'NONE', *, *, #98705, .F. ) ;
#21205 = CIRCLE ( 'NONE', #62647, 3.000000000000002665 ) ;
#21206 = CARTESIAN_POINT ( 'NONE',  ( 19.38216949554541557, 42.24863466993041783, -9.382169495545420901 ) ) ;
#21207 = CARTESIAN_POINT ( 'NONE',  ( 19.84674366389459266, 38.71726448433412315, -2.638427012816827677 ) ) ;
#21208 = CARTESIAN_POINT ( 'NONE',  ( 20.88017736071110519, 15.56368534415483751, 2.639326808657452039E-16 ) ) ;
#21209 = FACE_OUTER_BOUND ( 'NONE', #55987, .T. ) ;
#21210 = CARTESIAN_POINT ( 'NONE',  ( 19.84674366389459266, 38.30059781766745175, 2.638427012816836559 ) ) ;
#21211 = DIRECTION ( 'NONE',  ( -0.9975640502598243087, 0.06975647374412452528, -0.000000000000000000 ) ) ;
#21212 = CIRCLE ( 'NONE', #61174, 13.74999999999999467 ) ;
#21213 = DIRECTION ( 'NONE',  ( -0.000000000000000000, -0.000000000000000000, 1.000000000000000000 ) ) ;
#21214 = DIRECTION ( 'NONE',  ( -7.105427357601001859E-15, 0.000000000000000000, 1.000000000000000000 ) ) ;
#21215 = CARTESIAN_POINT ( 'NONE',  ( 0.3329122712635265713, 0.000000000000000000, 5.443067521379392204 ) ) ;
#21216 = DIRECTION ( 'NONE',  ( 0.9970872288863216193, 0.07626964003977222684, -0.000000000000000000 ) ) ;
#21217 = CARTESIAN_POINT ( 'NONE',  ( 14.92337183194729633, 12.67559781766745353, 8.527530157486181039 ) ) ;
#21218 = CARTESIAN_POINT ( 'NONE',  ( 21.09922568453594849, 26.20696800326375353, 6.408140936763242479 ) ) ;
#21219 = DIRECTION ( 'NONE',  ( 0.000000000000000000, -1.000000000000000000, 0.000000000000000000 ) ) ;
#21220 = ORIENTED_EDGE ( 'NONE', *, *, #1410, .T. ) ;
#21221 = CARTESIAN_POINT ( 'NONE',  ( 19.84674366389459621, 58.50893115100078745, 7.409399052514197653E-17 ) ) ;
#21222 = CARTESIAN_POINT ( 'NONE',  ( 4.629999999999994564, 43.00000000000000711, 4.000000000000000000 ) ) ;
#21223 = CARTESIAN_POINT ( 'NONE',  ( -2.266590686148945544, 26.38708216824730357, -7.082119434687050408 ) ) ;
#21224 = CARTESIAN_POINT ( 'NONE',  ( 19.84674366389459266, 48.71726448433413026, -2.638427012816827677 ) ) ;
#21225 = CARTESIAN_POINT ( 'NONE',  ( 22.81628187352648496, 41.83196800326375353, -3.434112377981050290 ) ) ;
#21227 = DIRECTION ( 'NONE',  ( -0.4461978131098131573, 0.000000000000000000, 0.8949343616020228875 ) ) ;
#21226 = CARTESIAN_POINT ( 'NONE',  ( -4.265913727725424209, 14.95037113646024096, 14.12300574719970392 ) ) ;
#21228 = CARTESIAN_POINT ( 'NONE',  ( 0.1532563361054082862, 11.21726448433411605, 2.638427012816831674 ) ) ;
#21229 = ADVANCED_FACE ( 'NONE', ( #38018 ), #76982, .F. ) ;
#21230 = CARTESIAN_POINT ( 'NONE',  ( -0.1049300847420626126, 67.21697413083880690, -6.336235997365760042 ) ) ;
#21231 = CARTESIAN_POINT ( 'NONE',  ( 18.52753015748617571, 53.09226448433412315, 4.923371831947298993 ) ) ;
#21232 = CARTESIAN_POINT ( 'NONE',  ( 17.96484262340118221, 44.93868534415483396, 7.964842623401181321 ) ) ;
#21233 = AXIS2_PLACEMENT_3D ( 'NONE', #47828, #46366, #23387 ) ;
#21234 = APPLICATION_PROTOCOL_DEFINITION ( 'draft international standard', 'automotive_design', 1998, #47424 ) ;
#21235 = DIRECTION ( 'NONE',  ( 0.000000000000000000, 0.000000000000000000, 1.000000000000000000 ) ) ;
#21236 = ADVANCED_FACE ( 'NONE', ( #53989 ), #30983, .T. ) ;
#21237 = CARTESIAN_POINT ( 'NONE',  ( 7.084665262690076126, 44.10535201082151247, 10.88017736071109987 ) ) ;
#21238 = EDGE_CURVE ( 'NONE', #82102, #2502, #54473, .T. ) ;
#21239 = VECTOR ( 'NONE', #29199, 1000.000000000000000 ) ;
#21240 = VERTEX_POINT ( 'NONE', #23519 ) ;
#21241 = MECHANICAL_DESIGN_GEOMETRIC_PRESENTATION_REPRESENTATION (  '', ( #89897 ), #46785 ) ;
#21242 = CARTESIAN_POINT ( 'NONE',  ( 0.5774900079438590739, 17.64701867748817321, -5.440088680355550821 ) ) ;
#21244 = CARTESIAN_POINT ( 'NONE',  ( 2.035157376598822676, 37.43868534415484106, -7.964842623401177768 ) ) ;
#21243 = CARTESIAN_POINT ( 'NONE',  ( 1.472469842513823179, 50.59226448433411605, -4.923371831947296329 ) ) ;
#21245 = FACE_OUTER_BOUND ( 'NONE', #66359, .T. ) ;
#21246 = CARTESIAN_POINT ( 'NONE',  ( 19.42250999205614548, 55.98035201082150536, -5.440088680355545492 ) ) ;
#21248 = CARTESIAN_POINT ( 'NONE',  ( 20.00000000000000355, 81.00009212066629516, -4.499999999999997335 ) ) ;
#21247 = CARTESIAN_POINT ( 'NONE',  ( 12.91533473730992121, 24.52201867748816966, 10.88017736071110164 ) ) ;
#21249 = CARTESIAN_POINT ( 'NONE',  ( 5.076628168052704559, 5.175597817667451750, -8.527530157486179263 ) ) ;
#21250 = CARTESIAN_POINT ( 'NONE',  ( 17.20831665107776587, 27.88393115100078390, 7.208316651077764980 ) ) ;
#21251 = CIRCLE ( 'NONE', #26039, 15.00000000000000000 ) ;
#21252 = CARTESIAN_POINT ( 'NONE',  ( -14.16423886937410437, 11.59541550158063750, -3.795296366450299885 ) ) ;
#21253 = CARTESIAN_POINT ( 'NONE',  ( 7.361572987183170547, 57.05059781766744464, 9.846743663894590881 ) ) ;
#21254 = CARTESIAN_POINT ( 'NONE',  ( 22.26659068614895176, 64.72041550158064638, -7.082119434687042414 ) ) ;
#21255 = EDGE_CURVE ( 'NONE', #74674, #89788, #31958, .T. ) ;
#21256 = CARTESIAN_POINT ( 'NONE',  ( 2.377183314879995013, 60.78593319516821936, -6.500000000000057732 ) ) ;
#21257 = CARTESIAN_POINT ( 'NONE',  ( 17.08211943468705130, 3.470415501580634388, 12.26659068614894998 ) ) ;
#21258 = CARTESIAN_POINT ( 'NONE',  ( 10.00000000000000000, 55.55374883491396787, -14.16423886937410082 ) ) ;
#21259 = CARTESIAN_POINT ( 'NONE',  ( -2.816281873526471635, 8.915301336597083903, -3.434112377981056508 ) ) ;
#21260 = ORIENTED_EDGE ( 'NONE', *, *, #22376, .T. ) ;
#21261 = CARTESIAN_POINT ( 'NONE',  ( 7.084665262690076126, 14.10535201082150358, 10.88017736071109987 ) ) ;
#21262 = CARTESIAN_POINT ( 'NONE',  ( 14.92337183194729633, 47.67559781766745175, 8.527530157486181039 ) ) ;
#21264 = LINE ( 'NONE', #95787, #35876 ) ;
#21263 = CARTESIAN_POINT ( 'NONE',  ( -2.266590686148945544, 1.387082168247301128, -7.082119434687050408 ) ) ;
#21265 =( NAMED_UNIT ( * ) SI_UNIT ( $, .STERADIAN. ) SOLID_ANGLE_UNIT ( ) );
#21266 =( LENGTH_UNIT ( ) NAMED_UNIT ( * ) SI_UNIT ( .MILLI., .METRE. ) );
#21267 = CARTESIAN_POINT ( 'NONE',  ( 22.81628187352647785, 26.41530133659708923, 3.434112377981063169 ) ) ;
#21268 = CARTESIAN_POINT ( 'NONE',  ( 19.84674366389459266, 28.71726448433411960, -2.638427012816827677 ) ) ;
#21269 = ORIENTED_EDGE ( 'NONE', *, *, #86840, .T. ) ;
#21270 = CARTESIAN_POINT ( 'NONE',  ( 17.20831665107776587, 2.883931151000785231, 7.208316651077764980 ) ) ;
#21271 = EDGE_CURVE ( 'NONE', #52968, #76742, #33643, .T. ) ;
#21272 = CARTESIAN_POINT ( 'NONE',  ( 11.44533173448679619, -77.48526441101047624, -4.000000000000000000 ) ) ;
#21273 = CARTESIAN_POINT ( 'NONE',  ( 17.35999999999999943, 37.99999999999997868, 10.00000000000000000 ) ) ;
#21274 = CARTESIAN_POINT ( 'NONE',  ( 15.44008868035555260, 14.73035201082150536, 9.422509992056143702 ) ) ;
#21275 = CARTESIAN_POINT ( 'NONE',  ( 24.16423886937410614, 34.30374883491396787, 8.672049930838204340E-16 ) ) ;
#21276 = CARTESIAN_POINT ( 'NONE',  ( 2.035157376598824452, 43.68868534415484106, 7.964842623401179544 ) ) ;
#21277 = CARTESIAN_POINT ( 'NONE',  ( 2.035157376598822676, 67.43868534415484817, -7.964842623401177768 ) ) ;
#21278 = CARTESIAN_POINT ( 'NONE',  ( 20.15039907845753220, 52.62777174578612716, -6.262539305110077947 ) ) ;
#21279 = CARTESIAN_POINT ( 'NONE',  ( 18.52753015748618282, 23.92559781766745530, -4.923371831947291888 ) ) ;
#21280 = DIRECTION ( 'NONE',  ( 0.000000000000000000, 1.000000000000000000, 0.000000000000000000 ) ) ;
#21281 = CARTESIAN_POINT ( 'NONE',  ( 7.361572987183170547, 2.050597817667451750, 9.846743663894590881 ) ) ;
#21282 = CARTESIAN_POINT ( 'NONE',  ( 4.862001128006773421, 4.807100664002271835E-16, -13.66056166602460031 ) ) ;
#21283 = CARTESIAN_POINT ( 'NONE',  ( 18.52753015748617571, 33.09226448433411605, 4.923371831947298993 ) ) ;
#21284 = AXIS2_PLACEMENT_3D ( 'NONE', #69966, #45987, #91970 ) ;
#21285 = CARTESIAN_POINT ( 'NONE',  ( 12.91533473730992121, 34.52201867748817676, 10.88017736071110164 ) ) ;
#21286 = EDGE_CURVE ( 'NONE', #97713, #80329, #28613, .T. ) ;
#21287 = AXIS2_PLACEMENT_3D ( 'NONE', #24434, #70418, #24925 ) ;
#21288 = ORIENTED_EDGE ( 'NONE', *, *, #75730, .F. ) ;
#21289 = CARTESIAN_POINT ( 'NONE',  ( 6.565887622018943937, 60.16530133659707502, 12.81628187352647430 ) ) ;
#21290 = CARTESIAN_POINT ( 'NONE',  ( 0.000000000000000000, 0.5000000000000004441, 0.000000000000000000 ) ) ;
#21291 = CARTESIAN_POINT ( 'NONE',  ( 14.92337183194729633, 7.675597817667451750, 8.527530157486181039 ) ) ;
#21292 = CARTESIAN_POINT ( 'NONE',  ( -1.099225684535947600, 48.70696800326375353, -6.408140936763238038 ) ) ;
#21294 = CARTESIAN_POINT ( 'NONE',  ( 0.1532563361054083140, 41.00893115100078745, 1.131784320476157264E-15 ) ) ;
#21293 = CARTESIAN_POINT ( 'NONE',  ( -0.3689425029237881626, 67.42874883491396076, 10.36894250292379027 ) ) ;
#21295 = DIRECTION ( 'NONE',  ( 0.000000000000000000, 0.000000000000000000, -1.000000000000000000 ) ) ;
#21296 = CARTESIAN_POINT ( 'NONE',  ( 12.63842701281683034, 2.467264484334118269, 9.846743663894596210 ) ) ;
#21297 = CARTESIAN_POINT ( 'NONE',  ( -0.3689425029237881626, 22.42874883491397142, 10.36894250292379027 ) ) ;
#21298 = CARTESIAN_POINT ( 'NONE',  ( 22.26659068614895176, 39.72041550158063217, -7.082119434687042414 ) ) ;
#21299 = CARTESIAN_POINT ( 'NONE',  ( 14.92337183194729633, 37.67559781766745175, 8.527530157486181039 ) ) ;
#21300 = SURFACE_STYLE_FILL_AREA ( #5804 ) ;
#21301 = CARTESIAN_POINT ( 'NONE',  ( 10.00000000000000178, 44.31368534415484106, 10.88017736071110342 ) ) ;
#21302 = CARTESIAN_POINT ( 'NONE',  ( 10.00000000000000000, 4.758931151000784787, -9.846743663894594434 ) ) ;
#21303 = DIRECTION ( 'NONE',  ( 0.000000000000000000, 0.000000000000000000, -1.000000000000000000 ) ) ;
#21304 = PRODUCT_DEFINITION_SHAPE ( 'NONE', 'NONE',  #70937 ) ;
#21305 = ORIENTED_EDGE ( 'NONE', *, *, #14272, .F. ) ;
#21306 = CARTESIAN_POINT ( 'NONE',  ( -2.816281873526473856, 64.33196800326376774, 3.434112377981055619 ) ) ;
#21307 = ORIENTED_EDGE ( 'NONE', *, *, #77475, .T. ) ;
#21308 = CARTESIAN_POINT ( 'NONE',  ( 20.88017736071110164, 65.35535201082150536, 2.915334737309930979 ) ) ;
#21309 = ORIENTED_EDGE ( 'NONE', *, *, #29943, .T. ) ;
#21310 = CARTESIAN_POINT ( 'NONE',  ( 10.00000000000000000, 5.553748834913967869, -14.16423886937410082 ) ) ;
#21311 = CARTESIAN_POINT ( 'NONE',  ( 12.63842701281683034, 7.467264484334118713, 9.846743663894596210 ) ) ;
#21312 = PLANE ( 'NONE',  #45635 ) ;
#21313 = VERTEX_POINT ( 'NONE', #15525 ) ;
#21314 = CARTESIAN_POINT ( 'NONE',  ( 19.42250999205614193, 20.14701867748817321, 5.440088680355555262 ) ) ;
#21315 = STYLED_ITEM ( 'NONE', ( #62941 ), #96216 ) ;
#21316 = VECTOR ( 'NONE', #61180, 1000.000000000000000 ) ;
#21317 = ORIENTED_EDGE ( 'NONE', *, *, #59388, .T. ) ;
#21318 = CARTESIAN_POINT ( 'NONE',  ( 19.42250999205614193, 40.14701867748817676, 5.440088680355555262 ) ) ;
#21319 = CARTESIAN_POINT ( 'NONE',  ( 2.791683348922240793, 56.63393115100078035, 7.208316651077764092 ) ) ;
#21320 = EDGE_LOOP ( 'NONE', ( #72284, #83297, #2052, #69275, #2765, #95909, #34381 ) ) ;
#21321 = AXIS2_PLACEMENT_3D ( 'NONE', #86474, #78466, #46488 ) ;
#21322 = CARTESIAN_POINT ( 'NONE',  ( 0.1532563361054083140, 61.00893115100078745, 1.131784320476157264E-15 ) ) ;
#21323 = ORIENTED_EDGE ( 'NONE', *, *, #36603, .F. ) ;
#21324 = EDGE_CURVE ( 'NONE', #90354, #79846, #92474, .T. ) ;
#21325 = MECHANICAL_DESIGN_GEOMETRIC_PRESENTATION_REPRESENTATION (  '', ( #29301 ), #595 ) ;
#21326 = CARTESIAN_POINT ( 'NONE',  ( 0.5774900079438590739, 62.64701867748817676, -5.440088680355550821 ) ) ;
#21327 = CARTESIAN_POINT ( 'NONE',  ( 14.92337183194729988, 64.34226448433412315, -8.527530157486177487 ) ) ;
#21328 = CARTESIAN_POINT ( 'NONE',  ( 0.6178305044545818747, 33.49863466993042493, -9.382169495545419124 ) ) ;
#21330 = CARTESIAN_POINT ( 'NONE',  ( 0.1089645850229091079, 58.16234555792573246, 6.479102184480836080 ) ) ;
#21329 = CARTESIAN_POINT ( 'NONE',  ( 7.084665262690076126, 27.02201867748817676, -10.88017736071110164 ) ) ;
#21331 = CARTESIAN_POINT ( 'NONE',  ( 7.361572987183170547, 7.050597817667451750, 9.846743663894590881 ) ) ;
#21332 = CARTESIAN_POINT ( 'NONE',  ( 19.42250999205614193, 15.14701867748817143, 5.440088680355555262 ) ) ;
#21333 = ADVANCED_FACE ( 'NONE', ( #47468 ), #29996, .T. ) ;
#21334 = VERTEX_POINT ( 'NONE', #23021 ) ;
#21335 = CARTESIAN_POINT ( 'NONE',  ( 22.81628187352647785, 51.41530133659708923, 3.434112377981063169 ) ) ;
#21336 = CARTESIAN_POINT ( 'NONE',  ( 20.88017736071110519, 40.56368534415484106, 2.639326808657452039E-16 ) ) ;
#21337 = CARTESIAN_POINT ( 'NONE',  ( -46.94000000000001194, 103.0000000000000000, -5.997726559847240679 ) ) ;
#21338 = CARTESIAN_POINT ( 'NONE',  ( 6.565887622018943937, 60.16530133659707502, 12.81628187352647430 ) ) ;
#21339 = CARTESIAN_POINT ( 'NONE',  ( 17.96484262340118221, 51.18868534415483396, -7.964842623401177768 ) ) ;
#21340 = CARTESIAN_POINT ( 'NONE',  ( 19.84674366389459266, 53.71726448433411605, -2.638427012816827677 ) ) ;
#21341 = DIRECTION ( 'NONE',  ( -0.000000000000000000, -0.000000000000000000, -1.000000000000000000 ) ) ;
#21342 = CARTESIAN_POINT ( 'NONE',  ( 19.84674366389459621, 23.50893115100078390, 7.409399052514197653E-17 ) ) ;
#21343 = CARTESIAN_POINT ( 'NONE',  ( 13.43411237798106583, 2.665301336597086568, -12.81628187352647252 ) ) ;
#21345 = CARTESIAN_POINT ( 'NONE',  ( 2.791683348922240793, 61.63393115100079456, 7.208316651077764092 ) ) ;
#21344 = CYLINDRICAL_SURFACE ( 'NONE', #42036, 11.92686044187656513 ) ;
#21346 = CARTESIAN_POINT ( 'NONE',  ( 15.44008868035555793, 36.39701867748816966, -9.422509992056140149 ) ) ;
#21347 = CARTESIAN_POINT ( 'NONE',  ( 19.84674366389459266, 43.71726448433410894, -2.638427012816827677 ) ) ;
#21348 = SURFACE_STYLE_FILL_AREA ( #74326 ) ;
#21349 = CARTESIAN_POINT ( 'NONE',  ( 13.14228782657334804, 15.00000000000000000, 7.230509711182329546 ) ) ;
#21351 = VERTEX_POINT ( 'NONE', #61975 ) ;
#21350 = CARTESIAN_POINT ( 'NONE',  ( 3.591859063236763294, 8.290301336597087456, -11.09922568453595026 ) ) ;
#21352 = CARTESIAN_POINT ( 'NONE',  ( 0.6081133539230525464, 63.33703382326400089, 6.499999999999970690 ) ) ;
#21353 = CARTESIAN_POINT ( 'NONE',  ( -5.817157072110618721, 0.5000000000000004441, -13.82608706751094552 ) ) ;
#21354 = EDGE_CURVE ( 'NONE', #62017, #89406, #56023, .T. ) ;
#21355 = CARTESIAN_POINT ( 'NONE',  ( 13.43411237798105340, 35.58196800326375353, 12.81628187352647963 ) ) ;
#21356 = CARTESIAN_POINT ( 'NONE',  ( 5.076628168052704559, 35.17559781766745175, -8.527530157486179263 ) ) ;
#21357 = CARTESIAN_POINT ( 'NONE',  ( 17.96484262340118221, 9.938685344154839285, 7.964842623401181321 ) ) ;
#21358 = CARTESIAN_POINT ( 'NONE',  ( 1.472469842513823179, 30.59226448433411960, -4.923371831947296329 ) ) ;
#21359 = EDGE_CURVE ( 'NONE', #15746, #2183, #60503, .T. ) ;
#21360 = VERTEX_POINT ( 'NONE', #53490 ) ;
#21361 = LINE ( 'NONE', #82341, #32853 ) ;
#21362 = CARTESIAN_POINT ( 'NONE',  ( 20.88017736071110875, 5.772018677488170546, -2.915334737309920765 ) ) ;
#21363 = CARTESIAN_POINT ( 'NONE',  ( 0.000000000000000000, 0.5000000000000004441, 0.000000000000000000 ) ) ;
#21364 = CARTESIAN_POINT ( 'NONE',  ( 12.91533473730992121, 19.52201867748816611, 10.88017736071110164 ) ) ;
#21365 = CARTESIAN_POINT ( 'NONE',  ( -4.164238869374098151, 46.59541550158063927, -3.795296366450310543 ) ) ;
#21367 = CARTESIAN_POINT ( 'NONE',  ( 0.000000000000000000, 0.000000000000000000, 0.000000000000000000 ) ) ;
#21366 = CARTESIAN_POINT ( 'NONE',  ( 17.08211943468705130, 48.47041550158063927, 12.26659068614894998 ) ) ;
#21368 = CARTESIAN_POINT ( 'NONE',  ( 0.09770025222076675342, 69.67742753483354079, 6.500000000000000000 ) ) ;
#21369 = CARTESIAN_POINT ( 'NONE',  ( 5.076628168052704559, 15.17559781766745175, -8.527530157486179263 ) ) ;
#21370 = CARTESIAN_POINT ( 'NONE',  ( 0.1532563361054082862, 66.21726448433413736, 2.638427012816831674 ) ) ;
#21371 = ORIENTED_EDGE ( 'NONE', *, *, #6894, .F. ) ;
#21372 =( NAMED_UNIT ( * ) SI_UNIT ( $, .STERADIAN. ) SOLID_ANGLE_UNIT ( ) );
#21373 = CARTESIAN_POINT ( 'NONE',  ( 7.361572987183169658, 59.96726448433410894, -9.846743663894592657 ) ) ;
#21374 = CYLINDRICAL_SURFACE ( 'NONE', #26804, 15.00000000000000000 ) ;
#21375 = DIRECTION ( 'NONE',  ( -1.000000000000000000, 0.000000000000000000, 0.000000000000000000 ) ) ;
#21376 = CARTESIAN_POINT ( 'NONE',  ( 1.472469842513823179, 21.42559781766745175, 4.923371831947296329 ) ) ;
#21377 = CARTESIAN_POINT ( 'NONE',  ( 2.618367889266248100E-15, 44.99999999999999289, -7.000000000000000000 ) ) ;
#21378 = ORIENTED_EDGE ( 'NONE', *, *, #41239, .T. ) ;
#21379 = TOROIDAL_SURFACE ( 'NONE', #7047, 14.49999999999999822, 0.5000000000000000000 ) ;
#21380 = EDGE_CURVE ( 'NONE', #96219, #29181, #12170, .T. ) ;
#21381 = CARTESIAN_POINT ( 'NONE',  ( 6.204703633549690345, 42.84541550158063217, 14.16423886937410082 ) ) ;
#21382 = CARTESIAN_POINT ( 'NONE',  ( 0.1532563361054100626, 10.80059781766745175, -2.638427012816831230 ) ) ;
#21384 = PRESENTATION_STYLE_ASSIGNMENT (( #34889 ) ) ;
#21383 = CARTESIAN_POINT ( 'NONE',  ( 0.1089645850229080254, 63.16234555792569694, 6.479102184480831639 ) ) ;
#21385 = CARTESIAN_POINT ( 'NONE',  ( 0.5774900079438607392, 33.48035201082150536, 5.440088680355550821 ) ) ;
#21386 = CARTESIAN_POINT ( 'NONE',  ( 21.09922568453595559, 32.04030133659708923, -6.408140936763230044 ) ) ;
#21387 = CARTESIAN_POINT ( 'NONE',  ( 19.42250999205614193, 5.147018677488171434, 5.440088680355555262 ) ) ;
#21388 = CARTESIAN_POINT ( 'NONE',  ( -2.816281873526471635, 33.91530133659708213, -3.434112377981056508 ) ) ;
#21389 = CARTESIAN_POINT ( 'NONE',  ( -2.816281873526473856, 64.12363466993042493, 9.499525473075851096E-16 ) ) ;
#21390 = ORIENTED_EDGE ( 'NONE', *, *, #90819, .F. ) ;
#21391 = CIRCLE ( 'NONE', #80483, 3.500000000000003109 ) ;
#21392 = SURFACE_STYLE_FILL_AREA ( #90355 ) ;
#21393 = EDGE_CURVE ( 'NONE', #35759, #59916, #75130, .T. ) ;
#21394 = CARTESIAN_POINT ( 'NONE',  ( -5.803070148808410877, 15.00000000000000000, 13.28812917035381780 ) ) ;
#21395 = CARTESIAN_POINT ( 'NONE',  ( -2.266590686148945544, 47.22041550158063927, 7.082119434687048631 ) ) ;
#21396 =( LENGTH_UNIT ( ) NAMED_UNIT ( * ) SI_UNIT ( .MILLI., .METRE. ) );
#21397 = CARTESIAN_POINT ( 'NONE',  ( 19.42250999205614193, 5.147018677488171434, 5.440088680355555262 ) ) ;
#21398 = CARTESIAN_POINT ( 'NONE',  ( -0.8801773607111009756, 18.06368534415484106, 1.068504757029289695E-15 ) ) ;
#21399 = DIRECTION ( 'NONE',  ( -3.730349362740525976E-14, 0.000000000000000000, 1.000000000000000000 ) ) ;
#21400 = DIRECTION ( 'NONE',  ( -0.000000000000000000, 1.000000000000000000, -0.000000000000000000 ) ) ;
#21401 = CARTESIAN_POINT ( 'NONE',  ( 7.084665262690076126, 47.02201867748818387, -10.88017736071110164 ) ) ;
#21402 = CARTESIAN_POINT ( 'NONE',  ( 15.44008868035555793, 56.39701867748817676, -9.422509992056140149 ) ) ;
#21403 = CARTESIAN_POINT ( 'NONE',  ( 22.81628187352647785, 16.62363466993042138, 6.195893100308588602E-16 ) ) ;
#21404 = DIRECTION ( 'NONE',  ( 0.000000000000000000, 0.000000000000000000, 1.000000000000000000 ) ) ;
#21405 = CARTESIAN_POINT ( 'NONE',  ( 18.52753015748618282, 23.92559781766745530, -4.923371831947291888 ) ) ;
#21406 = CARTESIAN_POINT ( 'NONE',  ( 19.42250999205614548, 50.98035201082151247, -5.440088680355545492 ) ) ;
#21407 = B_SPLINE_CURVE_WITH_KNOTS ( 'NONE', 3,
 ( #32440, #989, #93441, #92939, #69468, #9451 ),
 .UNSPECIFIED., .F., .F.,
 ( 4, 2, 4 ),
 ( -1.099704249473512899E-05, 0.0008751816947074439641, 0.001761360431909623093 ),
 .UNSPECIFIED. ) ;
#21408 = CARTESIAN_POINT ( 'NONE',  ( 3.591859063236763294, 18.29030133659708568, -11.09922568453595026 ) ) ;
#21409 = DIRECTION ( 'NONE',  ( 0.9969173337331278528, 0.000000000000000000, 0.07845909572784537378 ) ) ;
#21410 = CARTESIAN_POINT ( 'NONE',  ( 2.035157376598822676, 7.438685344154837509, -7.964842623401177768 ) ) ;
#21411 = CARTESIAN_POINT ( 'NONE',  ( 7.361572987183169658, 44.96726448433412315, -9.846743663894592657 ) ) ;
#21412 = CARTESIAN_POINT ( 'NONE',  ( 6.565887622018943937, 45.16530133659708923, 12.81628187352647430 ) ) ;
#21413 = CARTESIAN_POINT ( 'NONE',  ( 2.791683348922237240, 25.38393115100078390, -7.208316651077763204 ) ) ;
#21414 = CARTESIAN_POINT ( 'NONE',  ( 24.16423886937409904, 4.095415501580634832, 3.795296366450317205 ) ) ;
#21415 = CARTESIAN_POINT ( 'NONE',  ( 17.39651004071842166, 27.93575266056828355, 6.499999999999998224 ) ) ;
#21416 = CARTESIAN_POINT ( 'NONE',  ( 15.44008868035555793, 26.39701867748817321, -9.422509992056140149 ) ) ;
#21418 = CARTESIAN_POINT ( 'NONE',  ( 10.00000000000000178, 33.05374883491396787, 14.16423886937410082 ) ) ;
#21417 = CARTESIAN_POINT ( 'NONE',  ( 0.2751277870542967463, 0.000000000000000000, 6.500000000000000888 ) ) ;
#21419 = CARTESIAN_POINT ( 'NONE',  ( 10.00000000000000000, 49.75893115100078745, -9.846743663894594434 ) ) ;
#21420 = CARTESIAN_POINT ( 'NONE',  ( 0.5774900079438607392, 28.48035201082150891, 5.440088680355550821 ) ) ;
#21421 = CARTESIAN_POINT ( 'NONE',  ( 19.42250999205614193, 20.14701867748817321, 5.440088680355555262 ) ) ;
#21422 = ORIENTED_EDGE ( 'NONE', *, *, #91077, .F. ) ;
#21423 = CARTESIAN_POINT ( 'NONE',  ( 17.96484262340118221, 24.93868534415484461, 7.964842623401181321 ) ) ;
#21424 = CARTESIAN_POINT ( 'NONE',  ( 10.00000000000000178, 50.37363466993042493, 12.81628187352647608 ) ) ;
#21425 = CARTESIAN_POINT ( 'NONE',  ( 20.88017736071110164, 40.35535201082150536, 2.915334737309930979 ) ) ;
#21426 = CARTESIAN_POINT ( 'NONE',  ( 19.42250999205614193, 40.14701867748817676, 5.440088680355555262 ) ) ;
#21427 = VERTEX_POINT ( 'NONE', #72423 ) ;
#21428 = CARTESIAN_POINT ( 'NONE',  ( 0.1532563361054082862, 56.21726448433411605, 2.638427012816831674 ) ) ;
#21429 = CARTESIAN_POINT ( 'NONE',  ( 15.44008868035555793, 31.39701867748817676, -9.422509992056140149 ) ) ;
#21430 = CARTESIAN_POINT ( 'NONE',  ( 4.645844135293939914, -0.8374644621422210333, 4.000000000000000000 ) ) ;
#21431 = CARTESIAN_POINT ( 'NONE',  ( 0.000000000000000000, 0.000000000000000000, 8.000000000000000000 ) ) ;
#21432 = CARTESIAN_POINT ( 'NONE',  ( 22.81628187352647785, 61.62363466993041783, 6.195893100308588602E-16 ) ) ;
#21433 = DIRECTION ( 'NONE',  ( 1.000000000000000000, 0.000000000000000000, 0.000000000000000000 ) ) ;
#21434 = CARTESIAN_POINT ( 'NONE',  ( 13.79529636645030344, 53.26208216824730357, 14.16423886937410614 ) ) ;
#21435 = CARTESIAN_POINT ( 'NONE',  ( 2.035157376598824452, 48.68868534415483396, 7.964842623401179544 ) ) ;
#21436 = CARTESIAN_POINT ( 'NONE',  ( -14.03351048042393856, -0.03417435944610275333, -2.474486531753901541 ) ) ;
#21437 = FACE_OUTER_BOUND ( 'NONE', #2090, .T. ) ;
#21438 = CARTESIAN_POINT ( 'NONE',  ( 1.472469842513823179, 65.59226448433412315, -4.923371831947296329 ) ) ;
#21439 = CARTESIAN_POINT ( 'NONE',  ( 19.84674366389459266, 3.300597817667451750, 2.638427012816836559 ) ) ;
#21440 = CARTESIAN_POINT ( 'NONE',  ( 5.076628168052704559, 25.17559781766745175, -8.527530157486179263 ) ) ;
#21441 = ORIENTED_EDGE ( 'NONE', *, *, #74292, .F. ) ;
#21442 = CARTESIAN_POINT ( 'NONE',  ( 7.361572987183170547, 27.05059781766745175, 9.846743663894590881 ) ) ;
#21443 = CARTESIAN_POINT ( 'NONE',  ( 3.434112377981060948, -19.41803199673624647, 12.81628187352647430 ) ) ;
#21444 = CARTESIAN_POINT ( 'NONE',  ( -0.8801773607111009756, 33.06368534415484106, 1.068504757029289695E-15 ) ) ;
#21445 = CARTESIAN_POINT ( 'NONE',  ( 12.63842701281683922, 24.55059781766745175, -9.846743663894590881 ) ) ;
#21446 = SURFACE_STYLE_FILL_AREA ( #8292 ) ;
#21447 = CARTESIAN_POINT ( 'NONE',  ( -1.099225684535947600, 13.70696800326375353, -6.408140936763238038 ) ) ;
#21449 = CARTESIAN_POINT ( 'NONE',  ( 4.559911319644449179, 53.89701867748817676, 9.422509992056141925 ) ) ;
#21448 = CARTESIAN_POINT ( 'NONE',  ( 17.96484262340118221, 66.18868534415483396, -7.964842623401177768 ) ) ;
#21451 = CARTESIAN_POINT ( 'NONE',  ( 19.38216949554541557, 52.24863466993041072, -9.382169495545420901 ) ) ;
#21450 = CARTESIAN_POINT ( 'NONE',  ( 17.96484262340118221, 31.18868534415483751, -7.964842623401177768 ) ) ;
#21452 = CARTESIAN_POINT ( 'NONE',  ( -4.164238869374099927, 42.01208216824728936, 3.795296366450308767 ) ) ;
#21453 = EDGE_CURVE ( 'NONE', #14221, #23745, #96462, .T. ) ;
#21454 = VECTOR ( 'NONE', #48016, 1000.000000000000000 ) ;
#21455 = CARTESIAN_POINT ( 'NONE',  ( -14.71525861348292175, 14.63595249122790598, 2.908807992686487154 ) ) ;
#21456 = ORIENTED_EDGE ( 'NONE', *, *, #29507, .T. ) ;
#21457 = CARTESIAN_POINT ( 'NONE',  ( 22.81628187352647785, 11.41530133659708390, 3.434112377981063169 ) ) ;
#21458 = CARTESIAN_POINT ( 'NONE',  ( 7.084665262690076126, 7.022018677488169658, -10.88017736071110164 ) ) ;
#21459 = CARTESIAN_POINT ( 'NONE',  ( 12.91533473730993009, 51.60535201082149825, -10.88017736071109987 ) ) ;
#21460 = CARTESIAN_POINT ( 'NONE',  ( 18.72515096720568195, 26.07228050351032778, -6.500000000000018652 ) ) ;
#21461 = AXIS2_PLACEMENT_3D ( 'NONE', #38979, #32443, #70457 ) ;
#21462 = ORIENTED_EDGE ( 'NONE', *, *, #64553, .F. ) ;
#21463 = CARTESIAN_POINT ( 'NONE',  ( 10.00000000000000178, 64.31368534415483396, 10.88017736071110342 ) ) ;
#21464 = CARTESIAN_POINT ( 'NONE',  ( 19.84674366389459266, 33.71726448433410894, -2.638427012816827677 ) ) ;
#21465 = CARTESIAN_POINT ( 'NONE',  ( 17.20831665107776587, 24.13393115100078035, -7.208316651077762316 ) ) ;
#21466 = CARTESIAN_POINT ( 'NONE',  ( 7.361572987183169658, 19.96726448433411960, -9.846743663894592657 ) ) ;
#21467 = DIRECTION ( 'NONE',  ( 0.000000000000000000, 0.000000000000000000, 1.000000000000000000 ) ) ;
#21469 = CARTESIAN_POINT ( 'NONE',  ( -0.03932841506543475335, 23.12161441960502373, 6.397827110478943702 ) ) ;
#21468 = CARTESIAN_POINT ( 'NONE',  ( 7.361572987183170547, 2.050597817667451750, 9.846743663894590881 ) ) ;
#21470 = CARTESIAN_POINT ( 'NONE',  ( 9.209315896035914051, -9.300848983899108191, 3.750000000000000000 ) ) ;
#21472 = VERTEX_POINT ( 'NONE', #86471 ) ;
#21471 = CARTESIAN_POINT ( 'NONE',  ( 10.00000000000000178, 37.25893115100078745, 9.846743663894594434 ) ) ;
#21473 = CARTESIAN_POINT ( 'NONE',  ( 13.43411237798106583, 57.66530133659708923, -12.81628187352647252 ) ) ;
#21474 = CARTESIAN_POINT ( 'NONE',  ( -6.689969769699040114, -0.03417435944610275333, 12.58200319823965785 ) ) ;
#21475 = EDGE_CURVE ( 'NONE', #17879, #39344, #51094, .T. ) ;
#21476 = CARTESIAN_POINT ( 'NONE',  ( 21.09922568453594849, 1.206968003263753531, 6.408140936763242479 ) ) ;
#21477 = CARTESIAN_POINT ( 'NONE',  ( 20.88017736071110164, 10.35535201082150714, 2.915334737309930979 ) ) ;
#21478 = CARTESIAN_POINT ( 'NONE',  ( -0.3689425029237881626, 32.42874883491395366, 10.36894250292379027 ) ) ;
#21479 = ADVANCED_FACE ( 'NONE', ( #26931 ), #62960, .T. ) ;
#21480 = UNCERTAINTY_MEASURE_WITH_UNIT (LENGTH_MEASURE( 1.000000000000000082E-05 ), #65012, 'distance_accuracy_value', 'NONE');
#21481 = LINE ( 'NONE', #36483, #16888 ) ;
#21482 = CARTESIAN_POINT ( 'NONE',  ( 2.917880565312950480, 25.97041550158063572, -12.26659068614894821 ) ) ;
#21483 = CARTESIAN_POINT ( 'NONE',  ( -2.266590686148945544, 42.22041550158063217, 7.082119434687048631 ) ) ;
#21484 = CARTESIAN_POINT ( 'NONE',  ( 24.16423886937409904, 4.095415501580634832, 3.795296366450317205 ) ) ;
#21486 = CARTESIAN_POINT ( 'NONE',  ( -13.76191411541410048, 90.94479608829072959, -7.905863191225801501 ) ) ;
#21485 = CARTESIAN_POINT ( 'NONE',  ( -0.3689425029237881626, 17.42874883491397142, 10.36894250292379027 ) ) ;
#21487 = CARTESIAN_POINT ( 'NONE',  ( -0.8801773607110991993, 47.85535201082150536, -2.915334737309923874 ) ) ;
#21488 = CARTESIAN_POINT ( 'NONE',  ( 0.000000000000000000, 14.49999999999999822, 0.000000000000000000 ) ) ;
#21489 = ORIENTED_EDGE ( 'NONE', *, *, #77434, .T. ) ;
#21490 = CARTESIAN_POINT ( 'NONE',  ( 17.20831665107776587, 29.13393115100078390, -7.208316651077762316 ) ) ;
#21492 = CARTESIAN_POINT ( 'NONE',  ( 18.52753015748617571, 28.09226448433411960, 4.923371831947298993 ) ) ;
#21491 = DIRECTION ( 'NONE',  ( -1.000000000000000000, 0.000000000000000000, 0.000000000000000000 ) ) ;
#21493 = CARTESIAN_POINT ( 'NONE',  ( 19.42250999205614193, 10.14701867748816966, 5.440088680355555262 ) ) ;
#21494 = CARTESIAN_POINT ( 'NONE',  ( -1.099225684535947600, 59.54030133659708923, 6.408140936763237150 ) ) ;
#21495 = CARTESIAN_POINT ( 'NONE',  ( 1.472469842513823179, 46.42559781766745175, 4.923371831947296329 ) ) ;
#21496 = VECTOR ( 'NONE', #57797, 1000.000000000000114 ) ;
#21497 = CARTESIAN_POINT ( 'NONE',  ( 0.000000000000000000, 14.49999999999999822, 0.000000000000000000 ) ) ;
#21498 = CARTESIAN_POINT ( 'NONE',  ( 13.43411237798106583, 37.66530133659708923, -12.81628187352647252 ) ) ;
#21499 = CARTESIAN_POINT ( 'NONE',  ( 10.36894250292378850, -25.07125116508602858, -10.36894250292379027 ) ) ;
#21500 = CARTESIAN_POINT ( 'NONE',  ( 4.559911319644449179, 37.23035201082150536, -9.422509992056141925 ) ) ;
#21501 = CARTESIAN_POINT ( 'NONE',  ( 2.791683348922237240, 45.38393115100079456, -7.208316651077763204 ) ) ;
#21502 = CARTESIAN_POINT ( 'NONE',  ( 22.26659068614895176, 29.72041550158063572, -7.082119434687042414 ) ) ;
#21503 = VERTEX_POINT ( 'NONE', #25486 ) ;
#21504 = CARTESIAN_POINT ( 'NONE',  ( 6.204703633549690345, 2.845415501580634388, 14.16423886937410082 ) ) ;
#21505 = CARTESIAN_POINT ( 'NONE',  ( 19.42250999205614193, 65.14701867748817676, 5.440088680355555262 ) ) ;
#21506 = CARTESIAN_POINT ( 'NONE',  ( 19.42250999205614548, 65.98035201082151957, -5.440088680355545492 ) ) ;
#21507 = CARTESIAN_POINT ( 'NONE',  ( 2.917880565312950480, 60.97041550158063927, -12.26659068614894821 ) ) ;
#21508 = CARTESIAN_POINT ( 'NONE',  ( 22.81628187352647785, 1.623634669930420271, 6.195893100308588602E-16 ) ) ;
#21509 = DIRECTION ( 'NONE',  ( -0.000000000000000000, 1.000000000000000000, -0.000000000000000000 ) ) ;
#21510 = CARTESIAN_POINT ( 'NONE',  ( 12.91533473730992121, 59.52201867748816966, 10.88017736071110164 ) ) ;
#21511 = DIRECTION ( 'NONE',  ( 0.000000000000000000, 1.000000000000000000, -0.000000000000000000 ) ) ;
#21512 = CARTESIAN_POINT ( 'NONE',  ( 0.6178305044545838731, 34.74863466993042493, 9.382169495545420901 ) ) ;
#21513 = CARTESIAN_POINT ( 'NONE',  ( 7.964842623401177768, 26.18868534415484106, -7.964842623401181321 ) ) ;
#21514 = CARTESIAN_POINT ( 'NONE',  ( 15.44008868035555793, 11.39701867748817143, -9.422509992056140149 ) ) ;
#21515 = CARTESIAN_POINT ( 'NONE',  ( 12.91533473730992121, 14.52201867748817143, 10.88017736071110164 ) ) ;
#21516 = CIRCLE ( 'NONE', #16740, 14.49999999999999822 ) ;
#21517 = CARTESIAN_POINT ( 'NONE',  ( 5.076628168052704559, 40.17559781766745175, -8.527530157486179263 ) ) ;
#21518 = CARTESIAN_POINT ( 'NONE',  ( 3.591859063236761518, 49.95696800326375353, 11.09922568453594849 ) ) ;
#21519 = CARTESIAN_POINT ( 'NONE',  ( 20.00000000000000711, 105.0000000000000000, 4.500000000000000888 ) ) ;
#21520 = VERTEX_POINT ( 'NONE', #10464 ) ;
#21521 = B_SPLINE_CURVE_WITH_KNOTS ( 'NONE', 3,
 ( #53309, #15343, #76313, #38818 ),
 .UNSPECIFIED., .F., .F.,
 ( 4, 4 ),
 ( 0.000000000000000000, 0.0006109242138661632711 ),
 .UNSPECIFIED. ) ;
#21522 = EDGE_CURVE ( 'NONE', #20172, #18488, #97497, .T. ) ;
#21523 = CARTESIAN_POINT ( 'NONE',  ( 19.42250999205614193, 15.14701867748817143, 5.440088680355555262 ) ) ;
#21524 = CARTESIAN_POINT ( 'NONE',  ( 21.09922568453594849, 1.206968003263753531, 6.408140936763242479 ) ) ;
#21525 = FACE_OUTER_BOUND ( 'NONE', #74586, .T. ) ;
#21526 = CARTESIAN_POINT ( 'NONE',  ( 0.1532563361054082862, 16.21726448433411960, 2.638427012816831674 ) ) ;
#21527 = CARTESIAN_POINT ( 'NONE',  ( 17.20831665107776587, 52.88393115100078035, 7.208316651077764980 ) ) ;
#21528 = CARTESIAN_POINT ( 'NONE',  ( 7.084665262690076126, 32.02201867748816966, -10.88017736071110164 ) ) ;
#21529 = COLOUR_RGB ( '', 0.40784314, 0.44705882, 0.49803922) ;
#21530 = CARTESIAN_POINT ( 'NONE',  ( -2.816281873526473856, 9.331968003263753531, 3.434112377981055619 ) ) ;
#21532 = CARTESIAN_POINT ( 'NONE',  ( 17.88828545106793655, 91.03678680451055527, 8.000000000000001776 ) ) ;
#21531 = CARTESIAN_POINT ( 'NONE',  ( 20.88017736071110519, 50.56368534415484106, 2.639326808657452039E-16 ) ) ;
#21533 = CARTESIAN_POINT ( 'NONE',  ( 16.40814093676324603, 52.45696800326375353, -11.09922568453594671 ) ) ;
#21534 = ORIENTED_EDGE ( 'NONE', *, *, #53716, .T. ) ;
#21535 = CARTESIAN_POINT ( 'NONE',  ( 17.96484262340118221, 64.93868534415483396, 7.964842623401181321 ) ) ;
#21536 = AXIS2_PLACEMENT_3D ( 'NONE', #40338, #86816, #79309 ) ;
#21538 = CARTESIAN_POINT ( 'NONE',  ( 10.00000000000000178, 3.053748834913967425, 14.16423886937410082 ) ) ;
#21537 = CARTESIAN_POINT ( 'NONE',  ( 22.81628187352647785, 31.41530133659709279, 3.434112377981063169 ) ) ;
#21539 = DIRECTION ( 'NONE',  ( 1.257568779154408793E-17, 1.000000000000000000, -0.000000000000000000 ) ) ;
#21540 = CARTESIAN_POINT ( 'NONE',  ( 19.42250999205614193, 40.14701867748817676, 5.440088680355555262 ) ) ;
#21541 = CARTESIAN_POINT ( 'NONE',  ( 19.84674366389459621, 63.50893115100078745, 7.409399052514197653E-17 ) ) ;
#21542 = CARTESIAN_POINT ( 'NONE',  ( 12.63842701281683922, 49.55059781766744464, -9.846743663894590881 ) ) ;
#21543 = CARTESIAN_POINT ( 'NONE',  ( 7.361572987183170547, 22.05059781766745530, 9.846743663894590881 ) ) ;
#21544 = CARTESIAN_POINT ( 'NONE',  ( 2.791683348922240793, 11.63393115100078568, 7.208316651077764092 ) ) ;
#21545 =( LENGTH_UNIT ( ) NAMED_UNIT ( * ) SI_UNIT ( .MILLI., .METRE. ) );
#21546 = CARTESIAN_POINT ( 'NONE',  ( 22.26659068614894466, 48.88708216824730357, 7.082119434687054849 ) ) ;
#21547 =( BOUNDED_CURVE ( )  B_SPLINE_CURVE ( 2, ( #56991, #87494, #19009, #49485, #79992, #42016, #47529, #78031, #9533 ),
 .UNSPECIFIED., .F., .T. ) 
 B_SPLINE_CURVE_WITH_KNOTS ( ( 3, 2, 2, 2, 3 ),
 ( 0.5105718029354654464, 0.5119047619047618625, 0.5178571428571429047, 0.5238095238095238360, 0.5251424827788202521 ),
 .UNSPECIFIED. ) 
 CURVE ( )  GEOMETRIC_REPRESENTATION_ITEM ( )  RATIONAL_B_SPLINE_CURVE ( ( 0.9881565478350733400, 0.9923695281211490915, 1.000000000000000000, 0.9659258262890683122, 1.000000000000000000, 0.9659258262890683122, 1.000000000000000000, 0.9923695281211490915, 0.9881565478350733400 ) ) 
 REPRESENTATION_ITEM ( '' )  );
#21548 = CARTESIAN_POINT ( 'NONE',  ( 20.32896413005680714, 25.57879003517447458, -5.963430220938276349 ) ) ;
#21549 =( LENGTH_UNIT ( ) NAMED_UNIT ( * ) SI_UNIT ( .MILLI., .METRE. ) );
#21550 = CARTESIAN_POINT ( 'NONE',  ( 0.1916775849787289987, 7.258688159020694641, -6.500000000000003553 ) ) ;
#21551 =( BOUNDED_CURVE ( )  B_SPLINE_CURVE ( 2, ( #40239, #61735, #55739, #16753, #47228, #70747, #39266, #9243, #2263 ),
 .UNSPECIFIED., .F., .F. ) 
 B_SPLINE_CURVE_WITH_KNOTS ( ( 3, 2, 2, 2, 3 ),
 ( 0.4401409369402313199, 0.4404761904761904656, 0.4464285714285713969, 0.4523809523809524391, 0.4527162059169115849 ),
 .UNSPECIFIED. ) 
 CURVE ( )  GEOMETRIC_REPRESENTATION_ITEM ( )  RATIONAL_B_SPLINE_CURVE ( ( 0.9963778908391760503, 0.9980808541467920403, 1.000000000000000000, 0.9659258262890683122, 1.000000000000000000, 0.9659258262890683122, 1.000000000000000000, 0.9980808541467920403, 0.9963778908391759392 ) ) 
 REPRESENTATION_ITEM ( '' )  );
#21552 = ORIENTED_EDGE ( 'NONE', *, *, #37731, .F. ) ;
#21553 = ORIENTED_EDGE ( 'NONE', *, *, #88511, .T. ) ;
#21554 = CARTESIAN_POINT ( 'NONE',  ( 13.79529636645031943, 65.34541550158063217, -14.16423886937409904 ) ) ;
#21555 = CARTESIAN_POINT ( 'NONE',  ( 10.00000000000000000, 1.813685344154838175, -10.88017736071110342 ) ) ;
#21556 = CARTESIAN_POINT ( 'NONE',  ( 10.00000000000000000, 29.75893115100078745, -9.846743663894594434 ) ) ;
#21557 = VECTOR ( 'NONE', #39348, 1000.000000000000000 ) ;
#21558 = CARTESIAN_POINT ( 'NONE',  ( 16.40814093676324603, 22.45696800326375353, -11.09922568453594671 ) ) ;
#21559 = DIRECTION ( 'NONE',  ( 0.000000000000000000, 0.000000000000000000, 1.000000000000000000 ) ) ;
#21561 = CARTESIAN_POINT ( 'NONE',  ( 17.08211943468705130, 13.47041550158063572, 12.26659068614894998 ) ) ;
#21560 = CARTESIAN_POINT ( 'NONE',  ( -12.79762580179198039, 90.64749249312866652, -7.346077433012456304 ) ) ;
#21562 = CARTESIAN_POINT ( 'NONE',  ( 10.00000000000000178, 19.31368534415484106, 10.88017736071110342 ) ) ;
#21563 = CARTESIAN_POINT ( 'NONE',  ( -2.266590686148945544, 61.38708216824730357, -7.082119434687050408 ) ) ;
#21564 = CARTESIAN_POINT ( 'NONE',  ( 7.361572987183170547, 32.05059781766745175, 9.846743663894590881 ) ) ;
#21565 = CARTESIAN_POINT ( 'NONE',  ( 13.40508947812163143, 15.00000000000000000, 5.527528931046191474 ) ) ;
#21566 = CARTESIAN_POINT ( 'NONE',  ( 19.84674366389459621, 28.50893115100078745, 7.409399052514197653E-17 ) ) ;
#21567 = CARTESIAN_POINT ( 'NONE',  ( 0.000000000000000000, 15.00000000000000000, 0.000000000000000000 ) ) ;
#21568 = CARTESIAN_POINT ( 'NONE',  ( 4.923371831947295441, 14.34226448433412138, -8.527530157486179263 ) ) ;
#21569 = ORIENTED_EDGE ( 'NONE', *, *, #18758, .T. ) ;
#21570 = ORIENTED_EDGE ( 'NONE', *, *, #25455, .T. ) ;
#21571 = LINE ( 'NONE', #37065, #60565 ) ;
#21572 = ORIENTED_EDGE ( 'NONE', *, *, #16159, .T. ) ;
#21573 = CARTESIAN_POINT ( 'NONE',  ( 10.00000000000000178, 47.25893115100078745, 9.846743663894594434 ) ) ;
#21574 = CARTESIAN_POINT ( 'NONE',  ( 24.16423886937409904, 19.09541550158063927, 3.795296366450317205 ) ) ;
#21576 = CARTESIAN_POINT ( 'NONE',  ( 10.00000000000000178, 34.31368534415484106, 10.88017736071110342 ) ) ;
#21575 = CARTESIAN_POINT ( 'NONE',  ( 2.035157376598822676, 17.43868534415483751, -7.964842623401177768 ) ) ;
#21578 = CARTESIAN_POINT ( 'NONE',  ( 0.6178305044545838731, 14.74863466993041783, 9.382169495545420901 ) ) ;
#21577 = CARTESIAN_POINT ( 'NONE',  ( 0.1532563361054083140, 66.00893115100079456, 1.131784320476157264E-15 ) ) ;
#21579 = CARTESIAN_POINT ( 'NONE',  ( -2.266590686148945544, 7.220415501580634832, 7.082119434687048631 ) ) ;
#21581 = EDGE_CURVE ( 'NONE', #60237, #16271, #57429, .T. ) ;
#21580 = CARTESIAN_POINT ( 'NONE',  ( 2.035157376598824452, 68.68868534415484817, 7.964842623401179544 ) ) ;
#21582 = CARTESIAN_POINT ( 'NONE',  ( -1.099225684535947600, 28.70696800326375353, -6.408140936763238038 ) ) ;
#21583 = VERTEX_POINT ( 'NONE', #55971 ) ;
#21584 = CARTESIAN_POINT ( 'NONE',  ( 5.076628168052703671, 26.84226448433411960, 8.527530157486179263 ) ) ;
#21585 = CARTESIAN_POINT ( 'NONE',  ( 6.204703633549690345, 67.84541550158060375, 14.16423886937410082 ) ) ;
#21586 = EDGE_LOOP ( 'NONE', ( #80199, #75059, #38152, #46431, #66467, #48696 ) ) ;
#21587 = CARTESIAN_POINT ( 'NONE',  ( 20.88017736071110875, 5.772018677488170546, -2.915334737309920765 ) ) ;
#21588 = ORIENTED_EDGE ( 'NONE', *, *, #45490, .F. ) ;
#21589 = CARTESIAN_POINT ( 'NONE',  ( 19.42250999205614193, 50.14701867748817676, 5.440088680355555262 ) ) ;
#21590 = CARTESIAN_POINT ( 'NONE',  ( 17.96484262340118221, 64.93868534415483396, 7.964842623401181321 ) ) ;
#21591 = CARTESIAN_POINT ( 'NONE',  ( 2.035157376598822676, 62.43868534415483396, -7.964842623401177768 ) ) ;
#21592 = VECTOR ( 'NONE', #32260, 1000.000000000000000 ) ;
#21593 = CARTESIAN_POINT ( 'NONE',  ( 17.96484262340118221, 59.93868534415484106, 7.964842623401181321 ) ) ;
#21594 = CARTESIAN_POINT ( 'NONE',  ( -3.999999999999999112, 78.07179676972445748, -4.250000000000000000 ) ) ;
#21595 = DIRECTION ( 'NONE',  ( 0.5372996083468306594, 0.000000000000000000, -0.8433914458128813907 ) ) ;
#21596 = EDGE_CURVE ( 'NONE', #61713, #98693, #54362, .T. ) ;
#21597 = PRODUCT_DEFINITION_FORMATION_WITH_SPECIFIED_SOURCE ( 'ANY', '', #7560, .NOT_KNOWN. ) ;
#21598 = CARTESIAN_POINT ( 'NONE',  ( 17.20831665107776587, 34.13393115100078745, -7.208316651077762316 ) ) ;
#21599 = ORIENTED_EDGE ( 'NONE', *, *, #87049, .T. ) ;
#21600 = CARTESIAN_POINT ( 'NONE',  ( 5.076628168052703671, 56.84226448433412315, 8.527530157486179263 ) ) ;
#21601 = VECTOR ( 'NONE', #10777, 1000.000000000000227 ) ;
#21602 = DIRECTION ( 'NONE',  ( -2.131628207280300558E-14, 0.000000000000000000, 1.000000000000000000 ) ) ;
#21603 = EDGE_CURVE ( 'NONE', #16203, #95857, #48942, .T. ) ;
#21604 = CARTESIAN_POINT ( 'NONE',  ( 2.917880565312948704, 2.637082168247300906, 12.26659068614894643 ) ) ;
#21605 = VERTEX_POINT ( 'NONE', #41475 ) ;
#21606 = CARTESIAN_POINT ( 'NONE',  ( -10.02032951099770841, 12.52870482769689708, -5.208770347913566745 ) ) ;
#21607 = FACE_OUTER_BOUND ( 'NONE', #68656, .T. ) ;
#21609 = CARTESIAN_POINT ( 'NONE',  ( 7.361572987183169658, 39.96726448433411605, -9.846743663894592657 ) ) ;
#21608 = CARTESIAN_POINT ( 'NONE',  ( 13.14228782657346528, 14.49999999999999112, -7.230509711182246058 ) ) ;
#21610 = CARTESIAN_POINT ( 'NONE',  ( 10.00000000000000000, 6.813685344154838397, -10.88017736071110342 ) ) ;
#21611 = CARTESIAN_POINT ( 'NONE',  ( 7.684764310694878198, 15.00000000000000000, -12.88194075009934991 ) ) ;
#21612 = ORIENTED_EDGE ( 'NONE', *, *, #83216, .F. ) ;
#21613 = CARTESIAN_POINT ( 'NONE',  ( 3.469446951953614189E-15, 5.938309369127516391, 11.92686044187656513 ) ) ;
#21614 = CARTESIAN_POINT ( 'NONE',  ( 18.52753015748618282, 43.92559781766745175, -4.923371831947291888 ) ) ;
#21615 = CARTESIAN_POINT ( 'NONE',  ( 13.21236992757673789, -0.03417435944610275333, -5.338143956176714333 ) ) ;
#21616 = CARTESIAN_POINT ( 'NONE',  ( -1.099225684535947600, 13.70696800326375353, -6.408140936763238038 ) ) ;
#21617 = CARTESIAN_POINT ( 'NONE',  ( 7.361572987183169658, 9.967264484334119601, -9.846743663894592657 ) ) ;
#21618 = FACE_OUTER_BOUND ( 'NONE', #83419, .T. ) ;
#21619 = CARTESIAN_POINT ( 'NONE',  ( 19.38216949554541557, 7.248634669930421381, -9.382169495545420901 ) ) ;
#21620 =( LENGTH_UNIT ( ) NAMED_UNIT ( * ) SI_UNIT ( .MILLI., .METRE. ) );
#21621 = VECTOR ( 'NONE', #35472, 1000.000000000000000 ) ;
#21622 = ORIENTED_EDGE ( 'NONE', *, *, #68762, .F. ) ;
#21623 = B_SPLINE_CURVE_WITH_KNOTS ( 'NONE', 3,
 ( #45202, #75701, #7212, #30187, #68215, #64117 ),
 .UNSPECIFIED., .F., .F.,
 ( 4, 2, 4 ),
 ( 0.000000000000000000, 0.0002701661927229328424, 0.0005403323854458656848 ),
 .UNSPECIFIED. ) ;
#21624 = EDGE_LOOP ( 'NONE', ( #91274, #41951, #55494, #74518 ) ) ;
#21625 = CARTESIAN_POINT ( 'NONE',  ( 19.42250999205614548, 15.98035201082150714, -5.440088680355545492 ) ) ;
#21626 = CARTESIAN_POINT ( 'NONE',  ( -0.3689425029237898834, 16.17874883491396076, -10.36894250292378850 ) ) ;
#21627 = CARTESIAN_POINT ( 'NONE',  ( 18.52753015748618282, 28.92559781766745175, -4.923371831947291888 ) ) ;
#21628 = CARTESIAN_POINT ( 'NONE',  ( 20.88017736071110875, 55.77201867748816966, -2.915334737309920765 ) ) ;
#21629 = CARTESIAN_POINT ( 'NONE',  ( 21.09922568453594849, 36.20696800326375353, 6.408140936763242479 ) ) ;
#21630 = CARTESIAN_POINT ( 'NONE',  ( 17.96484262340118221, 21.18868534415483396, -7.964842623401177768 ) ) ;
#21631 = DIRECTION ( 'NONE',  ( -0.5905099943842175847, -0.8070303256584298035, 0.000000000000000000 ) ) ;
#21632 = CARTESIAN_POINT ( 'NONE',  ( 13.99999999999999822, 61.00000000000000711, 6.000000000000000000 ) ) ;
#21633 = CARTESIAN_POINT ( 'NONE',  ( 18.52753015748617571, 58.09226448433411605, 4.923371831947298993 ) ) ;
#21634 = CARTESIAN_POINT ( 'NONE',  ( 0.1532563361054082862, 26.21726448433411605, 2.638427012816831674 ) ) ;
#21635 = CARTESIAN_POINT ( 'NONE',  ( -7.964842623401172439, -16.31131465584515539, 7.964842623401183097 ) ) ;
#21636 = CARTESIAN_POINT ( 'NONE',  ( -2.816281873526473856, 34.33196800326376064, 3.434112377981055619 ) ) ;
#21637 = CARTESIAN_POINT ( 'NONE',  ( 0.2751277870542967463, 70.00000000000000000, -6.500000000000000888 ) ) ;
#21639 = LINE ( 'NONE', #6623, #73505 ) ;
#21638 = CARTESIAN_POINT ( 'NONE',  ( -0.8801773607111009756, 38.06368534415484106, 1.068504757029289695E-15 ) ) ;
#21640 = STYLED_ITEM ( 'NONE', ( #86298 ), #53296 ) ;
#21641 = EDGE_CURVE ( 'NONE', #38304, #23275, #24122, .T. ) ;
#21642 = CARTESIAN_POINT ( 'NONE',  ( 14.09397099617992311, 14.95037102751076752, -4.360881834954174252 ) ) ;
#21643 = CARTESIAN_POINT ( 'NONE',  ( 19.42250999205614548, 60.98035201082151247, -5.440088680355545492 ) ) ;
#21644 = CARTESIAN_POINT ( 'NONE',  ( 15.44008868035555793, 46.39701867748817676, -9.422509992056140149 ) ) ;
#21645 = CARTESIAN_POINT ( 'NONE',  ( 17.96484262340118221, 39.93868534415484106, 7.964842623401181321 ) ) ;
#21646 = CARTESIAN_POINT ( 'NONE',  ( 8.979999999999991545, 0.000000000000000000, 3.000000000000000000 ) ) ;
#21647 = CARTESIAN_POINT ( 'NONE',  ( 2.035157376598822676, 52.43868534415483396, -7.964842623401177768 ) ) ;
#21648 = AXIS2_PLACEMENT_3D ( 'NONE', #73267, #35265, #65762 ) ;
#21649 = CARTESIAN_POINT ( 'NONE',  ( 7.361572987183170547, 42.05059781766745886, 9.846743663894590881 ) ) ;
#21650 = CARTESIAN_POINT ( 'NONE',  ( 20.88017736071110519, 10.56368534415483751, 2.639326808657452039E-16 ) ) ;
#21651 = CARTESIAN_POINT ( 'NONE',  ( 16.40814093676324603, 17.45696800326375353, -11.09922568453594671 ) ) ;
#21652 = ORIENTED_EDGE ( 'NONE', *, *, #4531, .F. ) ;
#21653 = CARTESIAN_POINT ( 'NONE',  ( 15.44008868035555793, 26.39701867748817321, -9.422509992056140149 ) ) ;
#21654 = EDGE_CURVE ( 'NONE', #11855, #60629, #64912, .T. ) ;
#21655 = CARTESIAN_POINT ( 'NONE',  ( 0.6081133539230539897, 23.33703382326399733, 6.499999999999968914 ) ) ;
#21656 = CARTESIAN_POINT ( 'NONE',  ( -0.8801773607110991993, 27.85535201082150181, -2.915334737309923874 ) ) ;
#21657 = CARTESIAN_POINT ( 'NONE',  ( 12.91533473730992121, 64.52201867748817676, 10.88017736071110164 ) ) ;
#21658 = CARTESIAN_POINT ( 'NONE',  ( 24.16423886937410614, 29.30374883491396787, 8.672049930838204340E-16 ) ) ;
#21659 = CARTESIAN_POINT ( 'NONE',  ( 7.361572987183169658, 9.967264484334119601, -9.846743663894592657 ) ) ;
#21660 = CARTESIAN_POINT ( 'NONE',  ( 10.00000000000000000, 46.81368534415484106, -10.88017736071110342 ) ) ;
#21661 = CARTESIAN_POINT ( 'NONE',  ( 9.065164099344563908, 14.63606892172321139, -11.95084933600769439 ) ) ;
#21662 = CARTESIAN_POINT ( 'NONE',  ( 10.00000000000000000, 0.5537488349139675359, -14.16423886937410082 ) ) ;
#21663 = ORIENTED_EDGE ( 'NONE', *, *, #38673, .F. ) ;
#21664 = AXIS2_PLACEMENT_3D ( 'NONE', #81051, #11571, #65044 ) ;
#21665 = DIRECTION ( 'NONE',  ( 0.000000000000000000, 0.000000000000000000, 1.000000000000000000 ) ) ;
#21666 = CARTESIAN_POINT ( 'NONE',  ( 10.00000000000000178, 42.25893115100078745, 9.846743663894594434 ) ) ;
#21667 = ORIENTED_EDGE ( 'NONE', *, *, #37571, .T. ) ;
#21668 = ORIENTED_EDGE ( 'NONE', *, *, #93405, .F. ) ;
#21669 =( NAMED_UNIT ( * ) PLANE_ANGLE_UNIT ( ) SI_UNIT ( $, .RADIAN. ) );
#21670 = CARTESIAN_POINT ( 'NONE',  ( -0.3689425029237898834, 21.17874883491396432, -10.36894250292378850 ) ) ;
#21671 = CARTESIAN_POINT ( 'NONE',  ( 2.917880565312948704, 22.63708216824730002, 12.26659068614894643 ) ) ;
#21672 = CARTESIAN_POINT ( 'NONE',  ( 2.035157376598824452, 53.68868534415484817, 7.964842623401179544 ) ) ;
#21673 = CARTESIAN_POINT ( 'NONE',  ( 6.204703633549690345, 67.84541550158060375, 14.16423886937410082 ) ) ;
#21674 = CARTESIAN_POINT ( 'NONE',  ( 13.43411237798105340, 0.5819680032637533085, 12.81628187352647963 ) ) ;
#21675 = CARTESIAN_POINT ( 'NONE',  ( 7.361572987183169658, 54.96726448433413026, -9.846743663894592657 ) ) ;
#21676 =( NAMED_UNIT ( * ) PLANE_ANGLE_UNIT ( ) SI_UNIT ( $, .RADIAN. ) );
#21678 = CARTESIAN_POINT ( 'NONE',  ( 16.40814093676323893, 10.79030133659708923, 11.09922568453595026 ) ) ;
#21677 = CARTESIAN_POINT ( 'NONE',  ( 12.91533473730993009, 41.60535201082149825, -10.88017736071109987 ) ) ;
#21679 = CARTESIAN_POINT ( 'NONE',  ( -2.266590686148945544, 11.38708216824730179, -7.082119434687050408 ) ) ;
#21680 = CIRCLE ( 'NONE', #52002, 0.2499999999999980294 ) ;
#21681 = CARTESIAN_POINT ( 'NONE',  ( 15.44008868035555260, 14.73035201082150536, 9.422509992056143702 ) ) ;
#21682 = CARTESIAN_POINT ( 'NONE',  ( -0.2418659066527486246, 3.090145880403572409, 6.114288769123083611 ) ) ;
#21683 = CARTESIAN_POINT ( 'NONE',  ( 20.88017736071110519, 45.56368534415484106, 2.639326808657452039E-16 ) ) ;
#21684 = CARTESIAN_POINT ( 'NONE',  ( 0.6178305044545838731, 44.74863466993042493, 9.382169495545420901 ) ) ;
#21685 = CARTESIAN_POINT ( 'NONE',  ( 2.638427012816829897, -25.44940218233254825, -9.846743663894592657 ) ) ;
#21686 = ORIENTED_EDGE ( 'NONE', *, *, #78131, .F. ) ;
#21687 = CARTESIAN_POINT ( 'NONE',  ( -13.69000000000001549, 92.00000000000000000, 9.500000000000000000 ) ) ;
#21688 = VERTEX_POINT ( 'NONE', #24992 ) ;
#21689 = ORIENTED_EDGE ( 'NONE', *, *, #17049, .T. ) ;
#21690 = CARTESIAN_POINT ( 'NONE',  ( -0.7375392941519317569, 0.5000000000000004441, 14.98185688723470044 ) ) ;
#21692 = CARTESIAN_POINT ( 'NONE',  ( -0.8801773607111008646, 8.272018677488171434, 2.915334737309923430 ) ) ;
#21691 = CARTESIAN_POINT ( 'NONE',  ( 20.36894250292379382, 48.67874883491396076, 10.36894250292379205 ) ) ;
#21694 = CARTESIAN_POINT ( 'NONE',  ( 1.472469842513823179, 45.59226448433412315, -4.923371831947296329 ) ) ;
#21693 = CARTESIAN_POINT ( 'NONE',  ( 18.52753015748617571, 23.09226448433411960, 4.923371831947298993 ) ) ;
#21695 = CARTESIAN_POINT ( 'NONE',  ( 10.00000000000000178, 69.31368534415484817, 10.88017736071110342 ) ) ;
#21696 = ADVANCED_FACE ( 'NONE', ( #55475 ), #8387, .T. ) ;
#21697 = CARTESIAN_POINT ( 'NONE',  ( 20.88017736071110875, 65.77201867748817676, -2.915334737309920765 ) ) ;
#21698 = AXIS2_PLACEMENT_3D ( 'NONE', #43621, #65623, #49633 ) ;
#21699 = EDGE_CURVE ( 'NONE', #81069, #38526, #84779, .T. ) ;
#21700 = CARTESIAN_POINT ( 'NONE',  ( -3.434112377981067610, 28.08196800326376774, -12.81628187352647252 ) ) ;
#21701 = EDGE_LOOP ( 'NONE', ( #24655, #72686, #91285, #51016 ) ) ;
#21702 = CARTESIAN_POINT ( 'NONE',  ( 2.917880565312948704, 27.63708216824730357, 12.26659068614894643 ) ) ;
#21703 = CARTESIAN_POINT ( 'NONE',  ( -2.816281873526473856, 19.33196800326375708, 3.434112377981055619 ) ) ;
#21704 = ORIENTED_EDGE ( 'NONE', *, *, #41262, .F. ) ;
#21705 = CARTESIAN_POINT ( 'NONE',  ( -1.099225684535947600, 39.54030133659708923, 6.408140936763237150 ) ) ;
#21706 = CARTESIAN_POINT ( 'NONE',  ( 4.559911319644449179, 17.23035201082150536, -9.422509992056141925 ) ) ;
#21707 = CARTESIAN_POINT ( 'NONE',  ( 7.361572987183169658, 34.96726448433411605, -9.846743663894592657 ) ) ;
#21708 = CARTESIAN_POINT ( 'NONE',  ( 15.44008868035555793, 26.39701867748817321, -9.422509992056140149 ) ) ;
#21709 = LINE ( 'NONE', #52682, #81849 ) ;
#21710 = EDGE_CURVE ( 'NONE', #82533, #70499, #57636, .T. ) ;
#21711 = CARTESIAN_POINT ( 'NONE',  ( -4.000000000000000000, 37.00000000000000000, 2.750000000000000000 ) ) ;
#21712 = CARTESIAN_POINT ( 'NONE',  ( 10.00000000000000178, 42.25893115100078745, 9.846743663894594434 ) ) ;
#21713 = CARTESIAN_POINT ( 'NONE',  ( 2.791683348922240793, 51.63393115100078745, 7.208316651077764092 ) ) ;
#21714 = VECTOR ( 'NONE', #81243, 1000.000000000000000 ) ;
#21715 = CARTESIAN_POINT ( 'NONE',  ( -2.816281873526473856, 29.33196800326376064, 3.434112377981055619 ) ) ;
#21716 = DIRECTION ( 'NONE',  ( -0.000000000000000000, -1.000000000000000000, -0.000000000000000000 ) ) ;
#21717 = EDGE_CURVE ( 'NONE', #44781, #46487, #11328, .T. ) ;
#21718 = CYLINDRICAL_SURFACE ( 'NONE', #97227, 15.00000000000000000 ) ;
#21719 = CARTESIAN_POINT ( 'NONE',  ( -0.1503990784575328643, 10.12777174578612716, 6.262539305110068177 ) ) ;
#21720 =( NAMED_UNIT ( * ) PLANE_ANGLE_UNIT ( ) SI_UNIT ( $, .RADIAN. ) );
#21721 =( NAMED_UNIT ( * ) SI_UNIT ( $, .STERADIAN. ) SOLID_ANGLE_UNIT ( ) );
#21722 = CARTESIAN_POINT ( 'NONE',  ( 1.472469842513823179, 20.59226448433411960, -4.923371831947296329 ) ) ;
#21723 = CARTESIAN_POINT ( 'NONE',  ( 21.09922568453594849, 31.20696800326375353, 6.408140936763242479 ) ) ;
#21724 = ADVANCED_FACE ( 'NONE', ( #32870 ), #19113, .T. ) ;
#21725 = DIRECTION ( 'NONE',  ( -1.000000000000000000, 0.000000000000000000, 0.000000000000000000 ) ) ;
#21726 = ORIENTED_EDGE ( 'NONE', *, *, #57443, .F. ) ;
#21727 = CARTESIAN_POINT ( 'NONE',  ( 12.63842701281683034, 57.46726448433411605, 9.846743663894596210 ) ) ;
#21728 = DIRECTION ( 'NONE',  ( -0.000000000000000000, -0.000000000000000000, -1.000000000000000000 ) ) ;
#21729 = CARTESIAN_POINT ( 'NONE',  ( 17.20831665107776587, 37.88393115100078745, 7.208316651077764980 ) ) ;
#21730 = CARTESIAN_POINT ( 'NONE',  ( 13.79529636645031943, 40.34541550158063217, -14.16423886937409904 ) ) ;
#21731 = CARTESIAN_POINT ( 'NONE',  ( 1.472469842513823179, 46.42559781766745175, 4.923371831947296329 ) ) ;
#21732 = CARTESIAN_POINT ( 'NONE',  ( 21.09922568453595559, 52.04030133659708923, -6.408140936763230044 ) ) ;
#21734 = FACE_OUTER_BOUND ( 'NONE', #32198, .T. ) ;
#21733 = CARTESIAN_POINT ( 'NONE',  ( -14.97653319723434073, -0.03417435944610275333, -5.619684139539446122 ) ) ;
#21735 = CARTESIAN_POINT ( 'NONE',  ( 18.52753015748618282, 8.925597817667451750, -4.923371831947291888 ) ) ;
#21736 = PLANE ( 'NONE',  #45570 ) ;
#21737 = CARTESIAN_POINT ( 'NONE',  ( 18.52753015748618282, 53.92559781766745175, -4.923371831947291888 ) ) ;
#21738 = CARTESIAN_POINT ( 'NONE',  ( 7.084665262690076126, 47.02201867748818387, -10.88017736071110164 ) ) ;
#21739 = AXIS2_PLACEMENT_3D ( 'NONE', #35362, #59338, #28359 ) ;
#21740 = CONTEXT_DEPENDENT_SHAPE_REPRESENTATION ( #16783, #81949 ) ;
#21741 = CARTESIAN_POINT ( 'NONE',  ( -2.933660812630105141, -0.03417435944610275333, 15.72485391577587954 ) ) ;
#21742 = AXIS2_PLACEMENT_3D ( 'NONE', #38173, #44670, #83165 ) ;
#21743 = CARTESIAN_POINT ( 'NONE',  ( 0.5774900079438590739, 47.64701867748817676, -5.440088680355550821 ) ) ;
#21744 = AXIS2_PLACEMENT_3D ( 'NONE', #705, #22703, #67705 ) ;
#21745 = VERTEX_POINT ( 'NONE', #92881 ) ;
#21746 = CARTESIAN_POINT ( 'NONE',  ( -3.881785064875084235, 2.270048298641524909E-16, -14.10213074188660443 ) ) ;
#21747 = CARTESIAN_POINT ( 'NONE',  ( 19.42250999205614548, 15.98035201082150714, -5.440088680355545492 ) ) ;
#21749 = CARTESIAN_POINT ( 'NONE',  ( 4.559911319644449179, 47.23035201082150536, -9.422509992056141925 ) ) ;
#21748 = CARTESIAN_POINT ( 'NONE',  ( 17.20831665107776587, 64.13393115100079456, -7.208316651077762316 ) ) ;
#21750 = FACE_OUTER_BOUND ( 'NONE', #51258, .T. ) ;
#21751 = CARTESIAN_POINT ( 'NONE',  ( 20.88017736071110875, 55.77201867748816966, -2.915334737309920765 ) ) ;
#21752 = CARTESIAN_POINT ( 'NONE',  ( 66.76470751278411342, 40.99999999999997868, 10.00000000000000000 ) ) ;
#21754 = CARTESIAN_POINT ( 'NONE',  ( 4.630000000000003446, 1.019547802438464545, 4.000000000000000000 ) ) ;
#21753 = CARTESIAN_POINT ( 'NONE',  ( 19.42250999205614193, 40.14701867748817676, 5.440088680355555262 ) ) ;
#21755 = CARTESIAN_POINT ( 'NONE',  ( 12.63842701281683034, 7.467264484334118713, 9.846743663894596210 ) ) ;
#21756 = CARTESIAN_POINT ( 'NONE',  ( 2.791683348922237240, 20.38393115100078745, -7.208316651077763204 ) ) ;
#21757 = CARTESIAN_POINT ( 'NONE',  ( 1.881370533971186143, 2.354751593366954943E-16, 14.50512983964829772 ) ) ;
#21758 = CARTESIAN_POINT ( 'NONE',  ( -10.36894250292379205, 16.17874883491396432, -10.36894250292378672 ) ) ;
#21759 = CARTESIAN_POINT ( 'NONE',  ( 0.1532563361054100626, 65.80059781766745175, -2.638427012816831230 ) ) ;
#21761 = CARTESIAN_POINT ( 'NONE',  ( 2.603489959281115151, 16.58210964143323807, 6.499999999999462652 ) ) ;
#21760 = CARTESIAN_POINT ( 'NONE',  ( 19.42250999205614548, 5.980352010821504471, -5.440088680355545492 ) ) ;
#21762 = PRESENTATION_STYLE_ASSIGNMENT (( #59735 ) ) ;
#21763 = CARTESIAN_POINT ( 'NONE',  ( 24.16423886937410614, 29.30374883491396787, 8.672049930838204340E-16 ) ) ;
#21764 = EDGE_CURVE ( 'NONE', #71998, #47390, #24414, .T. ) ;
#21765 = CARTESIAN_POINT ( 'NONE',  ( 20.36894250292379382, 53.67874883491397497, 10.36894250292379205 ) ) ;
#21766 = CARTESIAN_POINT ( 'NONE',  ( 17.96484262340118221, 4.938685344154837509, 7.964842623401181321 ) ) ;
#21767 = ORIENTED_EDGE ( 'NONE', *, *, #8526, .T. ) ;
#21768 = CARTESIAN_POINT ( 'NONE',  ( 5.076628168052703671, 21.84226448433411960, 8.527530157486179263 ) ) ;
#21769 = CARTESIAN_POINT ( 'NONE',  ( 15.44008868035555793, 11.39701867748817143, -9.422509992056140149 ) ) ;
#21770 = CARTESIAN_POINT ( 'NONE',  ( 17.20831665107776587, 49.13393115100078745, -7.208316651077762316 ) ) ;
#21772 = SURFACE_STYLE_USAGE ( .BOTH. , #7757 ) ;
#21771 = DIRECTION ( 'NONE',  ( 0.000000000000000000, 0.000000000000000000, 1.000000000000000000 ) ) ;
#21773 = CARTESIAN_POINT ( 'NONE',  ( 1.460619146402132233E-15, 13.17686044187655270, -11.92686044187656513 ) ) ;
#21774 = CARTESIAN_POINT ( 'NONE',  ( 22.81628187352647785, 31.62363466993042138, 6.195893100308588602E-16 ) ) ;
#21775 = CARTESIAN_POINT ( 'NONE',  ( 0.1532563361054083140, 41.00893115100078745, 1.131784320476157264E-15 ) ) ;
#21776 = ORIENTED_EDGE ( 'NONE', *, *, #55835, .F. ) ;
#21777 = CARTESIAN_POINT ( 'NONE',  ( 5.076628168052704559, 5.175597817667451750, -8.527530157486179263 ) ) ;
#21778 = CARTESIAN_POINT ( 'NONE',  ( 10.88670032936942711, -94.01435490392699990, -4.000000000000000000 ) ) ;
#21779 = DIRECTION ( 'NONE',  ( -0.000000000000000000, -0.000000000000000000, -1.000000000000000000 ) ) ;
#21780 = CARTESIAN_POINT ( 'NONE',  ( 2.035157376598824452, 8.688685344154839285, 7.964842623401179544 ) ) ;
#21781 = CARTESIAN_POINT ( 'NONE',  ( 2.917880565312948704, 42.63708216824729647, 12.26659068614894643 ) ) ;
#21782 = CARTESIAN_POINT ( 'NONE',  ( 19.42250999205614193, 45.14701867748817676, 5.440088680355555262 ) ) ;
#21783 = CARTESIAN_POINT ( 'NONE',  ( 15.44008868035555260, 64.73035201082151957, 9.422509992056143702 ) ) ;
#21784 = CARTESIAN_POINT ( 'NONE',  ( 19.84674366389459266, 23.30059781766745530, 2.638427012816836559 ) ) ;
#21785 = CARTESIAN_POINT ( 'NONE',  ( 15.44008868035555260, 4.730352010821504471, 9.422509992056143702 ) ) ;
#21786 = CARTESIAN_POINT ( 'NONE',  ( 19.84674366389459621, 8.508931151000785675, 7.409399052514197653E-17 ) ) ;
#21787 = CARTESIAN_POINT ( 'NONE',  ( -46.70105855243338766, 101.0494761711182718, 8.834315900847478531 ) ) ;
#21788 = CARTESIAN_POINT ( 'NONE',  ( 19.84674366389459266, 43.30059781766744464, 2.638427012816836559 ) ) ;
#21789 = AXIS2_PLACEMENT_3D ( 'NONE', #4062, #58519, #87546 ) ;
#21790 = CARTESIAN_POINT ( 'NONE',  ( 10.00000000000000178, 39.31368534415484106, 10.88017736071110342 ) ) ;
#21791 = ORIENTED_EDGE ( 'NONE', *, *, #94605, .F. ) ;
#21792 = CARTESIAN_POINT ( 'NONE',  ( 22.81628187352648496, 61.83196800326376774, -3.434112377981050290 ) ) ;
#21793 = CARTESIAN_POINT ( 'NONE',  ( -8.000000000000000000, 79.82179676972448590, 4.250000000000000000 ) ) ;
#21794 = CARTESIAN_POINT ( 'NONE',  ( 14.92337183194729633, 2.675597817667451750, 8.527530157486181039 ) ) ;
#21795 = CARTESIAN_POINT ( 'NONE',  ( 13.43411237798106583, 42.66530133659707502, -12.81628187352647252 ) ) ;
#21797 = CARTESIAN_POINT ( 'NONE',  ( 10.00000000000000178, 42.25893115100078745, 9.846743663894594434 ) ) ;
#21796 = CARTESIAN_POINT ( 'NONE',  ( 2.035157376598822676, 12.43868534415483751, -7.964842623401177768 ) ) ;
#21798 = SURFACE_STYLE_FILL_AREA ( #13789 ) ;
#21799 = CARTESIAN_POINT ( 'NONE',  ( -4.164238869374099927, 32.01208216824730357, 3.795296366450308767 ) ) ;
#21800 = PRESENTATION_LAYER_ASSIGNMENT (  '', '', ( #25018 ) ) ;
#21801 = CARTESIAN_POINT ( 'NONE',  ( 10.00000000000000000, 50.55374883491396787, -14.16423886937410082 ) ) ;
#21802 = CARTESIAN_POINT ( 'NONE',  ( 19.84674366389459266, 63.71726448433412315, -2.638427012816827677 ) ) ;
#21803 = DIRECTION ( 'NONE',  ( 0.000000000000000000, -0.000000000000000000, -1.000000000000000000 ) ) ;
#21804 = CARTESIAN_POINT ( 'NONE',  ( 4.559911319644449179, 37.23035201082150536, -9.422509992056141925 ) ) ;
#21805 = CARTESIAN_POINT ( 'NONE',  ( 17.20831665107776587, 2.883931151000785231, 7.208316651077764980 ) ) ;
#21806 = ORIENTED_EDGE ( 'NONE', *, *, #54731, .F. ) ;
#21807 = CARTESIAN_POINT ( 'NONE',  ( 16.40814093676323893, 55.79030133659708923, 11.09922568453595026 ) ) ;
#21808 = CARTESIAN_POINT ( 'NONE',  ( 0.5774900079438590739, 62.64701867748817676, -5.440088680355550821 ) ) ;
#21809 = EDGE_LOOP ( 'NONE', ( #96877, #26854, #12450, #58338 ) ) ;
#21810 = CARTESIAN_POINT ( 'NONE',  ( 13.79529636645031943, 5.345415501580634832, -14.16423886937409904 ) ) ;
#21811 = CARTESIAN_POINT ( 'NONE',  ( 17.20831665107776587, 12.88393115100078390, 7.208316651077764980 ) ) ;
#21812 = CARTESIAN_POINT ( 'NONE',  ( 20.88017736071110519, 30.56368534415484106, 2.639326808657452039E-16 ) ) ;
#21813 = LINE ( 'NONE', #42827, #80824 ) ;
#21814 = VECTOR ( 'NONE', #42766, 1000.000000000000114 ) ;
#21815 = ORIENTED_EDGE ( 'NONE', *, *, #80132, .F. ) ;
#21816 = EDGE_CURVE ( 'NONE', #47923, #79627, #20100, .T. ) ;
#21817 = CARTESIAN_POINT ( 'NONE',  ( 4.559911319644449179, 33.89701867748817676, 9.422509992056141925 ) ) ;
#21818 = EDGE_CURVE ( 'NONE', #18712, #33937, #7016, .T. ) ;
#21819 = CIRCLE ( 'NONE', #82463, 1.249999999999987121 ) ;
#21820 = ADVANCED_FACE ( 'NONE', ( #86382 ), #78873, .T. ) ;
#21821 = ORIENTED_EDGE ( 'NONE', *, *, #94151, .T. ) ;
#21822 = CARTESIAN_POINT ( 'NONE',  ( 7.084665262690076126, 32.02201867748816966, -10.88017736071110164 ) ) ;
#21823 = ORIENTED_EDGE ( 'NONE', *, *, #53278, .F. ) ;
#21824 = EDGE_LOOP ( 'NONE', ( #77873, #7603, #22098, #60568 ) ) ;
#21825 = CARTESIAN_POINT ( 'NONE',  ( 0.5774900079438607392, 63.48035201082149825, 5.440088680355550821 ) ) ;
#21827 = CARTESIAN_POINT ( 'NONE',  ( 7.361572987183169658, 64.96726448433412315, -9.846743663894592657 ) ) ;
#21826 = B_SPLINE_CURVE_WITH_KNOTS ( 'NONE', 3,
 ( #28010, #4546, #27518, #58009, #49045, #50521 ),
 .UNSPECIFIED., .F., .F.,
 ( 4, 2, 4 ),
 ( 0.0002800011564896255026, 0.0006862063972211533995, 0.001092411637952681296 ),
 .UNSPECIFIED. ) ;
#21829 = CARTESIAN_POINT ( 'NONE',  ( 19.72487221294570858, 6.866073187300758107, 6.500000000000000888 ) ) ;
#21828 = CARTESIAN_POINT ( 'NONE',  ( 17.96484262340118221, 24.93868534415484461, 7.964842623401181321 ) ) ;
#21830 = CARTESIAN_POINT ( 'NONE',  ( 18.52753015748617571, 3.092264484334118269, 4.923371831947298993 ) ) ;
#21831 = CARTESIAN_POINT ( 'NONE',  ( 19.42250999205614548, 20.98035201082150891, -5.440088680355545492 ) ) ;
#21832 = CIRCLE ( 'NONE', #55370, 0.2499999999999997224 ) ;
#21833 = ORIENTED_EDGE ( 'NONE', *, *, #64637, .T. ) ;
#21834 = AXIS2_PLACEMENT_3D ( 'NONE', #32544, #31064, #61563 ) ;
#21835 = CARTESIAN_POINT ( 'NONE',  ( 7.084665262690076126, 39.10535201082150536, 10.88017736071109987 ) ) ;
#21836 = DIRECTION ( 'NONE',  ( -0.000000000000000000, -0.000000000000000000, -1.000000000000000000 ) ) ;
#21837 = CARTESIAN_POINT ( 'NONE',  ( 3.591859063236763294, 58.29030133659708923, -11.09922568453595026 ) ) ;
#21838 = CARTESIAN_POINT ( 'NONE',  ( 19.42250999205614548, 45.98035201082150536, -5.440088680355545492 ) ) ;
#21839 = CARTESIAN_POINT ( 'NONE',  ( 0.6178305044545818747, 3.498634669930420049, -9.382169495545419124 ) ) ;
#21840 = EDGE_CURVE ( 'NONE', #45159, #17988, #83004, .T. ) ;
#21841 = DIRECTION ( 'NONE',  ( -0.8320502943378437211, 0.5547001962252290364, 0.000000000000000000 ) ) ;
#21842 = EDGE_LOOP ( 'NONE', ( #86581, #52208, #56156, #92476 ) ) ;
#21843 = CARTESIAN_POINT ( 'NONE',  ( 7.361572987183169658, 14.96726448433411960, -9.846743663894592657 ) ) ;
#21844 = CARTESIAN_POINT ( 'NONE',  ( 0.000000000000000000, 0.000000000000000000, 0.000000000000000000 ) ) ;
#21845 = CARTESIAN_POINT ( 'NONE',  ( 16.40814093676324603, 7.456968003263754419, -11.09922568453594671 ) ) ;
#21847 = CARTESIAN_POINT ( 'NONE',  ( 2.791683348922240793, 66.63393115100079456, 7.208316651077764092 ) ) ;
#21846 = FILL_AREA_STYLE ('',( #14340 ) ) ;
#21848 = CARTESIAN_POINT ( 'NONE',  ( 2.035157376598822676, 37.43868534415484106, -7.964842623401177768 ) ) ;
#21849 = CARTESIAN_POINT ( 'NONE',  ( 0.1532563361054083140, 46.00893115100079456, 1.131784320476157264E-15 ) ) ;
#21850 = VECTOR ( 'NONE', #93133, 1000.000000000000114 ) ;
#21851 = CARTESIAN_POINT ( 'NONE',  ( 0.2751277870542967463, 70.00000000000000000, 6.000000000000000000 ) ) ;
#21852 = CARTESIAN_POINT ( 'NONE',  ( 12.63842701281683034, 17.46726448433411250, 9.846743663894596210 ) ) ;
#21853 = CARTESIAN_POINT ( 'NONE',  ( 14.92337183194729988, 4.342264484334117824, -8.527530157486177487 ) ) ;
#21855 = ORIENTED_EDGE ( 'NONE', *, *, #15190, .F. ) ;
#21854 = CARTESIAN_POINT ( 'NONE',  ( -1.099225684535947600, -0.4596986634029132657, 6.408140936763237150 ) ) ;
#21856 = EDGE_CURVE ( 'NONE', #13218, #9024, #64184, .T. ) ;
#21857 = FILL_AREA_STYLE_COLOUR ( '', #51848 ) ;
#21858 = CARTESIAN_POINT ( 'NONE',  ( 0.1532563361054082862, 61.21726448433412315, 2.638427012816831674 ) ) ;
#21859 = CARTESIAN_POINT ( 'NONE',  ( 18.52753015748618282, 33.92559781766745886, -4.923371831947291888 ) ) ;
#21860 = CARTESIAN_POINT ( 'NONE',  ( 6.829574850505124139, -88.00372650098202598, -2.500000000000001776 ) ) ;
#21861 = CARTESIAN_POINT ( 'NONE',  ( 10.00000000000000000, 1.813685344154838175, -10.88017736071110342 ) ) ;
#21862 = EDGE_CURVE ( 'NONE', #49345, #23295, #50327, .T. ) ;
#21863 = CARTESIAN_POINT ( 'NONE',  ( 19.84674366389459621, 43.50893115100078745, 7.409399052514197653E-17 ) ) ;
#21864 = CIRCLE ( 'NONE', #69756, 15.00000000000000000 ) ;
#21865 = CARTESIAN_POINT ( 'NONE',  ( 17.39651004071841456, 64.08210964143329136, -6.500000000000001776 ) ) ;
#21866 = CARTESIAN_POINT ( 'NONE',  ( 24.16423886937410614, 64.51208216824728936, -3.795296366450302550 ) ) ;
#21867 = FACE_OUTER_BOUND ( 'NONE', #73480, .T. ) ;
#21868 = CARTESIAN_POINT ( 'NONE',  ( 4.559911319644449179, 22.23035201082150536, -9.422509992056141925 ) ) ;
#21869 = CARTESIAN_POINT ( 'NONE',  ( 22.26659068614894466, 53.88708216824731068, 7.082119434687054849 ) ) ;
#21871 = LINE ( 'NONE', #45340, #47823 ) ;
#21870 = CARTESIAN_POINT ( 'NONE',  ( 17.08211943468705840, 50.13708216824730357, -12.26659068614894466 ) ) ;
#21872 = CARTESIAN_POINT ( 'NONE',  ( 18.52753015748617571, 3.092264484334118269, 4.923371831947298993 ) ) ;
#21873 = CARTESIAN_POINT ( 'NONE',  ( 12.63842701281683922, 29.55059781766745175, -9.846743663894590881 ) ) ;
#21874 = CARTESIAN_POINT ( 'NONE',  ( 10.00000000000000000, 12.87363466993042138, -12.81628187352647608 ) ) ;
#21875 = ORIENTED_EDGE ( 'NONE', *, *, #43513, .F. ) ;
#21876 = CARTESIAN_POINT ( 'NONE',  ( -3.250000000000000444, 1.019547802438465656, 2.500000000000000000 ) ) ;
#21877 = CARTESIAN_POINT ( 'NONE',  ( 11.92686044187656336, 2.188309369127512838, -2.602085213965210642E-15 ) ) ;
#21878 = CARTESIAN_POINT ( 'NONE',  ( 7.361572987183170547, 67.05059781766746596, 9.846743663894590881 ) ) ;
#21879 = CARTESIAN_POINT ( 'NONE',  ( 10.00000000000000000, 5.553748834913967869, -14.16423886937410082 ) ) ;
#21880 = CARTESIAN_POINT ( 'NONE',  ( 1.472469842513823179, 20.59226448433411960, -4.923371831947296329 ) ) ;
#21881 = EDGE_LOOP ( 'NONE', ( #10896, #41179, #79115, #85768, #19567, #37324 ) ) ;
#21882 = CARTESIAN_POINT ( 'NONE',  ( 20.36894250292379738, 39.92874883491396787, -10.36894250292379027 ) ) ;
#21883 = AXIS2_PLACEMENT_3D ( 'NONE', #53197, #76197, #91692 ) ;
#21884 = CARTESIAN_POINT ( 'NONE',  ( 1.472469842513823179, 10.59226448433411782, -4.923371831947296329 ) ) ;
#21886 = LINE ( 'NONE', #19895, #85420 ) ;
#21885 = CARTESIAN_POINT ( 'NONE',  ( -7.121341127240343738, -73.24353698637879972, -2.500000000000000000 ) ) ;
#21887 = CARTESIAN_POINT ( 'NONE',  ( 2.035157376598824452, 28.68868534415484106, 7.964842623401179544 ) ) ;
#21888 = CARTESIAN_POINT ( 'NONE',  ( -1.099225684535947600, 39.54030133659708923, 6.408140936763237150 ) ) ;
#21889 = CARTESIAN_POINT ( 'NONE',  ( 4.559911319644449179, 7.230352010821504471, -9.422509992056141925 ) ) ;
#21890 = CARTESIAN_POINT ( 'NONE',  ( -2.816281873526473856, 39.33196800326374643, 3.434112377981055619 ) ) ;
#21891 = CARTESIAN_POINT ( 'NONE',  ( 22.81628187352647785, 56.62363466993042493, 6.195893100308588602E-16 ) ) ;
#21892 = ORIENTED_EDGE ( 'NONE', *, *, #56016, .F. ) ;
#21893 = CARTESIAN_POINT ( 'NONE',  ( 1.821708436314931179, 11.66792564121895381, -6.499999999999995559 ) ) ;
#21894 = LINE ( 'NONE', #55327, #82950 ) ;
#21895 = CARTESIAN_POINT ( 'NONE',  ( 20.36894250292379738, 44.92874883491396787, -10.36894250292379027 ) ) ;
#21896 = CARTESIAN_POINT ( 'NONE',  ( 13.79529636645031943, 5.345415501580634832, -14.16423886937409904 ) ) ;
#21897 = CARTESIAN_POINT ( 'NONE',  ( 4.559911319644449179, 2.230352010821504471, -9.422509992056141925 ) ) ;
#21898 = CARTESIAN_POINT ( 'NONE',  ( 4.559911319644449179, 27.23035201082150536, -9.422509992056141925 ) ) ;
#21899 = CARTESIAN_POINT ( 'NONE',  ( 9.997910040112596874, 15.00000000000000000, -10.50199004140715253 ) ) ;
#21900 = DIRECTION ( 'NONE',  ( -0.000000000000000000, -1.000000000000000000, -0.000000000000000000 ) ) ;
#21901 = CARTESIAN_POINT ( 'NONE',  ( 20.88017736071110164, 55.35535201082149825, 2.915334737309930979 ) ) ;
#21902 = CARTESIAN_POINT ( 'NONE',  ( 12.91533473730992121, 64.52201867748817676, 10.88017736071110164 ) ) ;
#21903 = CARTESIAN_POINT ( 'NONE',  ( 21.09922568453595559, 22.04030133659708923, -6.408140936763230044 ) ) ;
#21904 = CARTESIAN_POINT ( 'NONE',  ( -0.1503990784575294781, 48.10158574516642460, 6.262539305110072618 ) ) ;
#21905 = APPLICATION_CONTEXT ( 'automotive_design' ) ;
#21906 = CARTESIAN_POINT ( 'NONE',  ( -9.509319644403765537, 13.17686044187662020, 7.198808227794258663 ) ) ;
#21907 = CARTESIAN_POINT ( 'NONE',  ( 18.52753015748618282, 18.92559781766745175, -4.923371831947291888 ) ) ;
#21908 = TOROIDAL_SURFACE ( 'NONE', #44352, 14.49999999999999822, 0.5000000000000000000 ) ;
#21909 = ADVANCED_FACE ( 'NONE', ( #11847 ), #41395, .T. ) ;
#21910 = CARTESIAN_POINT ( 'NONE',  ( 20.88017736071110164, 60.35535201082151957, 2.915334737309930979 ) ) ;
#21911 = TOROIDAL_SURFACE ( 'NONE', #64969, 0.5000000000000000000, 0.2500000000000000000 ) ;
#21912 = AXIS2_PLACEMENT_3D ( 'NONE', #3594, #57552, #56099 ) ;
#21913 = CARTESIAN_POINT ( 'NONE',  ( -1.099225684535947600, 23.70696800326375708, -6.408140936763238038 ) ) ;
#21914 = CARTESIAN_POINT ( 'NONE',  ( -0.8801773607111009756, 3.063685344154837509, 1.068504757029289695E-15 ) ) ;
#21915 = CARTESIAN_POINT ( 'NONE',  ( 12.63842701281683922, 34.55059781766745886, -9.846743663894590881 ) ) ;
#21916 = CARTESIAN_POINT ( 'NONE',  ( 4.873787042390789637, 15.00000000000000000, -13.39061984619918988 ) ) ;
#21917 = CARTESIAN_POINT ( 'NONE',  ( 19.84674366389459266, 18.30059781766745175, 2.638427012816836559 ) ) ;
#21918 = CARTESIAN_POINT ( 'NONE',  ( 20.88017736071110875, 30.77201867748816966, -2.915334737309920321 ) ) ;
#21919 = CARTESIAN_POINT ( 'NONE',  ( 15.44008868035555260, 39.73035201082150536, 9.422509992056143702 ) ) ;
#21920 = CARTESIAN_POINT ( 'NONE',  ( 17.08211943468705840, 35.13708216824730357, -12.26659068614894466 ) ) ;
#21921 = CARTESIAN_POINT ( 'NONE',  ( 17.20831665107776587, 39.13393115100079456, -7.208316651077762316 ) ) ;
#21922 = CARTESIAN_POINT ( 'NONE',  ( 12.91533473730993009, 31.60535201082150891, -10.88017736071109987 ) ) ;
#21923 = CARTESIAN_POINT ( 'NONE',  ( 10.00000000000000000, 11.81368534415483751, -10.88017736071110342 ) ) ;
#21924 = ORIENTED_EDGE ( 'NONE', *, *, #3766, .F. ) ;
#21925 = EDGE_CURVE ( 'NONE', #81593, #7375, #89417, .T. ) ;
#21926 = CARTESIAN_POINT ( 'NONE',  ( -0.8801773607111008646, 23.27201867748817676, 2.915334737309923430 ) ) ;
#21927 = CARTESIAN_POINT ( 'NONE',  ( 0.6178305044545818747, 43.49863466993042493, -9.382169495545419124 ) ) ;
#21928 = CARTESIAN_POINT ( 'NONE',  ( 0.5774900079438590739, 47.64701867748817676, -5.440088680355550821 ) ) ;
#21929 = FACE_OUTER_BOUND ( 'NONE', #98439, .T. ) ;
#21930 = ORIENTED_EDGE ( 'NONE', *, *, #45398, .T. ) ;
#21931 = CARTESIAN_POINT ( 'NONE',  ( 12.63842701281683922, 54.55059781766745175, -9.846743663894590881 ) ) ;
#21933 = ADVANCED_FACE ( 'NONE', ( #41874 ), #79852, .T. ) ;
#21932 = CARTESIAN_POINT ( 'NONE',  ( 12.91533473730993009, 41.60535201082149825, -10.88017736071109987 ) ) ;
#21934 =( NAMED_UNIT ( * ) PLANE_ANGLE_UNIT ( ) SI_UNIT ( $, .RADIAN. ) );
#21935 = DIRECTION ( 'NONE',  ( 0.000000000000000000, 0.000000000000000000, -1.000000000000000000 ) ) ;
#21936 = CARTESIAN_POINT ( 'NONE',  ( 0.1129803114748714477, 9.294273331840907204, -6.480634945678661829 ) ) ;
#21937 = CARTESIAN_POINT ( 'NONE',  ( 17.08211943468705130, 43.47041550158063927, 12.26659068614894998 ) ) ;
#21938 = CARTESIAN_POINT ( 'NONE',  ( 10.00000000000000178, 59.31368534415484106, 10.88017736071110342 ) ) ;
#21939 = SURFACE_STYLE_USAGE ( .BOTH. , #90904 ) ;
#21940 = EDGE_CURVE ( 'NONE', #25854, #50813, #42844, .T. ) ;
#21941 = STYLED_ITEM ( 'NONE', ( #85845 ), #30196 ) ;
#21942 = LINE ( 'NONE', #52420, #54065 ) ;
#21943 = CARTESIAN_POINT ( 'NONE',  ( 10.00000000000000178, 67.25893115100079456, 9.846743663894594434 ) ) ;
#21944 = CARTESIAN_POINT ( 'NONE',  ( -0.8801773607110991993, 2.855352010821504471, -2.915334737309923874 ) ) ;
#21945 = CARTESIAN_POINT ( 'NONE',  ( 14.92337183194729988, 34.34226448433411605, -8.527530157486177487 ) ) ;
#21946 = ORIENTED_EDGE ( 'NONE', *, *, #72467, .F. ) ;
#21947 = CARTESIAN_POINT ( 'NONE',  ( 1.472469842513823179, 41.42559781766745886, 4.923371831947296329 ) ) ;
#21948 = CARTESIAN_POINT ( 'NONE',  ( 6.408140936763243367, -19.20969866340291077, 11.09922568453594494 ) ) ;
#21949 = CARTESIAN_POINT ( 'NONE',  ( 15.44008868035555793, 26.39701867748817321, -9.422509992056140149 ) ) ;
#21950 = CARTESIAN_POINT ( 'NONE',  ( 14.92337183194729633, 22.67559781766745175, 8.527530157486181039 ) ) ;
#21951 = CARTESIAN_POINT ( 'NONE',  ( 16.40814093676324603, 22.45696800326375353, -11.09922568453594671 ) ) ;
#21953 = CARTESIAN_POINT ( 'NONE',  ( 4.559911319644449179, 58.89701867748817676, 9.422509992056141925 ) ) ;
#21952 = CARTESIAN_POINT ( 'NONE',  ( 12.91533473730993009, 66.60535201082150536, -10.88017736071109987 ) ) ;
#21955 = FACE_OUTER_BOUND ( 'NONE', #85115, .T. ) ;
#21954 = CARTESIAN_POINT ( 'NONE',  ( 4.559911319644449179, 38.89701867748817676, 9.422509992056141925 ) ) ;
#21956 = CARTESIAN_POINT ( 'NONE',  ( 10.00000000000000178, 48.05374883491396787, 14.16423886937410082 ) ) ;
#21957 = CARTESIAN_POINT ( 'NONE',  ( -14.49120296996859558, 14.95077488074853456, 2.766068805437424949 ) ) ;
#21958 = EDGE_LOOP ( 'NONE', ( #84269, #20930, #71362, #71221 ) ) ;
#21959 = CARTESIAN_POINT ( 'NONE',  ( 22.81628187352648496, 16.83196800326374998, -3.434112377981050290 ) ) ;
#21960 = CARTESIAN_POINT ( 'NONE',  ( 15.44008868035555260, 9.730352010821505360, 9.422509992056143702 ) ) ;
#21961 = CARTESIAN_POINT ( 'NONE',  ( -0.8801773607111009756, 53.06368534415484106, 1.068504757029289695E-15 ) ) ;
#21962 = CARTESIAN_POINT ( 'NONE',  ( 10.00000000000000178, 70.00000000000000000, 0.000000000000000000 ) ) ;
#21964 = ORIENTED_EDGE ( 'NONE', *, *, #61050, .F. ) ;
#21963 = EDGE_CURVE ( 'NONE', #10040, #2203, #57831, .T. ) ;
#21965 = VECTOR ( 'NONE', #71242, 1000.000000000000000 ) ;
#21966 = CARTESIAN_POINT ( 'NONE',  ( 20.88017736071110519, 55.56368534415484817, 2.639326808657452039E-16 ) ) ;
#21967 = CARTESIAN_POINT ( 'NONE',  ( 10.00000000000000178, 32.25893115100078745, 9.846743663894594434 ) ) ;
#21968 = CARTESIAN_POINT ( 'NONE',  ( 2.791683348922237240, 25.38393115100078390, -7.208316651077763204 ) ) ;
#21969 = CARTESIAN_POINT ( 'NONE',  ( 17.20831665107776587, 9.133931151000787452, -7.208316651077762316 ) ) ;
#21971 = CARTESIAN_POINT ( 'NONE',  ( 10.00000000000000178, 35.37363466993042493, 12.81628187352647608 ) ) ;
#21970 = CARTESIAN_POINT ( 'NONE',  ( 1.042145700049404766, 49.74216108172002038, -6.499999999999937828 ) ) ;
#21974 = CARTESIAN_POINT ( 'NONE',  ( 3.897244926436223444, 15.00000000000000000, -13.96644127841327787 ) ) ;
#21973 = CIRCLE ( 'NONE', #37900, 15.00000000000000000 ) ;
#21972 = CARTESIAN_POINT ( 'NONE',  ( 0.1532563361054100626, 5.800597817667452638, -2.638427012816831230 ) ) ;
#21975 = CARTESIAN_POINT ( 'NONE',  ( 7.154372922009559765, 15.00000000000000000, -14.30707323420376831 ) ) ;
#21977 = EDGE_LOOP ( 'NONE', ( #87211, #66920, #6096, #41851 ) ) ;
#21976 = CARTESIAN_POINT ( 'NONE',  ( 14.92337183194729633, 32.67559781766745175, 8.527530157486181039 ) ) ;
#21978 = EDGE_CURVE ( 'NONE', #70649, #88318, #71296, .T. ) ;
#21979 = MECHANICAL_DESIGN_GEOMETRIC_PRESENTATION_REPRESENTATION (  '', ( #65045 ), #77841 ) ;
#21980 = CARTESIAN_POINT ( 'NONE',  ( 6.565887622018943937, 50.16530133659708213, 12.81628187352647430 ) ) ;
#21981 = CYLINDRICAL_SURFACE ( 'NONE', #27854, 15.00000000000000000 ) ;
#21982 = CARTESIAN_POINT ( 'NONE',  ( 3.591859063236761518, 14.95696800326375531, 11.09922568453594849 ) ) ;
#21983 = CARTESIAN_POINT ( 'NONE',  ( 20.88017736071110519, 50.56368534415484106, 2.639326808657452039E-16 ) ) ;
#21984 = CARTESIAN_POINT ( 'NONE',  ( -0.3689425029237881626, 27.42874883491397142, 10.36894250292379027 ) ) ;
#21985 = CARTESIAN_POINT ( 'NONE',  ( -8.223478179881292149, 85.80780507572754345, 3.936430718245549354 ) ) ;
#21986 = CARTESIAN_POINT ( 'NONE',  ( 22.26659068614895176, 29.72041550158063572, -7.082119434687042414 ) ) ;
#21987 = CARTESIAN_POINT ( 'NONE',  ( 22.26659068614894466, 48.88708216824730357, 7.082119434687054849 ) ) ;
#21988 = CARTESIAN_POINT ( 'NONE',  ( 24.16423886937410614, 4.512082168247300906, -3.795296366450302550 ) ) ;
#21989 = CARTESIAN_POINT ( 'NONE',  ( 2.917880565312948704, 12.63708216824730179, 12.26659068614894643 ) ) ;
#21990 = CARTESIAN_POINT ( 'NONE',  ( 4.559911319644449179, 43.89701867748816966, 9.422509992056141925 ) ) ;
#21991 = CARTESIAN_POINT ( 'NONE',  ( -4.000000000000000000, 10.25000000000000000, -3.750000000000000000 ) ) ;
#21992 = CARTESIAN_POINT ( 'NONE',  ( 7.361572987183170547, 27.05059781766745175, 9.846743663894590881 ) ) ;
#21994 = CARTESIAN_POINT ( 'NONE',  ( 0.1532563361054083140, 31.00893115100078390, 1.131784320476157264E-15 ) ) ;
#21993 = CARTESIAN_POINT ( 'NONE',  ( -45.94000000000000483, 92.00000000000000000, -8.999999999999998224 ) ) ;
#21995 = CARTESIAN_POINT ( 'NONE',  ( 0.5774900079438607392, 28.48035201082150891, 5.440088680355550821 ) ) ;
#21996 = CARTESIAN_POINT ( 'NONE',  ( 3.591859063236763294, 58.29030133659708923, -11.09922568453595026 ) ) ;
#21997 = LINE ( 'NONE', #61935, #63347 ) ;
#21998 = FACE_OUTER_BOUND ( 'NONE', #53286, .T. ) ;
#21999 = CARTESIAN_POINT ( 'NONE',  ( 19.84674366389459266, 23.30059781766745530, 2.638427012816836559 ) ) ;
#22000 = CARTESIAN_POINT ( 'NONE',  ( -1.099225684535947600, 38.70696800326375353, -6.408140936763238038 ) ) ;
#22001 = CARTESIAN_POINT ( 'NONE',  ( 12.26659068614894821, -21.11291783175269643, 7.082119434687044190 ) ) ;
#22002 = CARTESIAN_POINT ( 'NONE',  ( 15.44008868035555793, 41.39701867748817676, -9.422509992056140149 ) ) ;
#22003 = CARTESIAN_POINT ( 'NONE',  ( 5.076628168052703671, 56.84226448433412315, 8.527530157486179263 ) ) ;
#22004 = CARTESIAN_POINT ( 'NONE',  ( 20.36894250292379382, 23.67874883491397142, 10.36894250292379205 ) ) ;
#22005 = ORIENTED_EDGE ( 'NONE', *, *, #45495, .F. ) ;
#22006 = SURFACE_STYLE_FILL_AREA ( #98517 ) ;
#22007 = CARTESIAN_POINT ( 'NONE',  ( 0.5774900079438607392, 63.48035201082149825, 5.440088680355550821 ) ) ;
#22008 = CARTESIAN_POINT ( 'NONE',  ( 4.559911319644449179, 63.89701867748817676, 9.422509992056141925 ) ) ;
#22009 = CARTESIAN_POINT ( 'NONE',  ( -2.266590686148945544, 61.38708216824730357, -7.082119434687050408 ) ) ;
#22010 = CARTESIAN_POINT ( 'NONE',  ( 10.00000000000000000, -2.126365330069579951, -12.81628187352647608 ) ) ;
#22011 = CARTESIAN_POINT ( 'NONE',  ( 2.913501739333663743, 15.00000000000000000, 14.20427779279537184 ) ) ;
#22012 = CARTESIAN_POINT ( 'NONE',  ( 4.559911319644449179, 58.89701867748817676, 9.422509992056141925 ) ) ;
#22013 = CARTESIAN_POINT ( 'NONE',  ( -0.2418659066527792945, 28.09014588040356841, 6.114288769123030320 ) ) ;
#22014 = CIRCLE ( 'NONE', #77875, 0.2500000000000002220 ) ;
#22015 = CARTESIAN_POINT ( 'NONE',  ( 10.00000000000000000, 32.87363466993042493, -12.81628187352647608 ) ) ;
#22016 = CARTESIAN_POINT ( 'NONE',  ( 13.79529636645030344, 43.26208216824730357, 14.16423886937410614 ) ) ;
#22017 = CARTESIAN_POINT ( 'NONE',  ( 10.88017736071110519, 25.56368534415484461, -2.602085213965210642E-15 ) ) ;
#22018 = CARTESIAN_POINT ( 'NONE',  ( 7.084665262690076126, 9.105352010821503583, 10.88017736071109987 ) ) ;
#22019 = CARTESIAN_POINT ( 'NONE',  ( 19.42250999205614548, 15.98035201082150714, -5.440088680355545492 ) ) ;
#22020 = CARTESIAN_POINT ( 'NONE',  ( 7.361572987183169658, 54.96726448433413026, -9.846743663894592657 ) ) ;
#22021 = CARTESIAN_POINT ( 'NONE',  ( -1.099225684535947600, 54.54030133659708923, 6.408140936763237150 ) ) ;
#22022 =( LENGTH_UNIT ( ) NAMED_UNIT ( * ) SI_UNIT ( .MILLI., .METRE. ) );
#22023 = ORIENTED_EDGE ( 'NONE', *, *, #22063, .F. ) ;
#22024 = EDGE_CURVE ( 'NONE', #46930, #46487, #86217, .T. ) ;
#22025 = CARTESIAN_POINT ( 'NONE',  ( 0.5774900079438607392, 18.48035201082150536, 5.440088680355550821 ) ) ;
#22026 = CARTESIAN_POINT ( 'NONE',  ( -1.099225684535947600, 13.70696800326375353, -6.408140936763238038 ) ) ;
#22027 = DIRECTION ( 'NONE',  ( 1.000000000000000000, 0.000000000000000000, 0.000000000000000000 ) ) ;
#22028 = AXIS2_PLACEMENT_3D ( 'NONE', #14556, #5575, #21559 ) ;
#22029 = CARTESIAN_POINT ( 'NONE',  ( 0.1532563361054100626, 50.80059781766745175, -2.638427012816831230 ) ) ;
#22030 = CARTESIAN_POINT ( 'NONE',  ( 10.00000000000000000, 36.81368534415484106, -10.88017736071110342 ) ) ;
#22031 = CARTESIAN_POINT ( 'NONE',  ( 10.00000000000000000, 17.87363466993041783, -12.81628187352647608 ) ) ;
#22033 = CARTESIAN_POINT ( 'NONE',  ( -6.732636091893171582, -88.11213685669366669, -2.750000000000000444 ) ) ;
#22032 = CARTESIAN_POINT ( 'NONE',  ( 0.5774900079438590739, 42.64701867748816966, -5.440088680355550821 ) ) ;
#22034 = CARTESIAN_POINT ( 'NONE',  ( 14.49999999999999822, 61.00000000000000000, 6.000000000000000000 ) ) ;
#22035 = CARTESIAN_POINT ( 'NONE',  ( 19.38216949554541202, 50.99863466993042493, 9.382169495545424454 ) ) ;
#22036 = ORIENTED_EDGE ( 'NONE', *, *, #67143, .T. ) ;
#22037 = CARTESIAN_POINT ( 'NONE',  ( 19.42250999205614548, 45.98035201082150536, -5.440088680355545492 ) ) ;
#22039 = CARTESIAN_POINT ( 'NONE',  ( 24.16423886937409904, 4.095415501580634832, 3.795296366450317205 ) ) ;
#22038 = CARTESIAN_POINT ( 'NONE',  ( -2.816281873526473856, 29.33196800326376064, 3.434112377981055619 ) ) ;
#22040 = CARTESIAN_POINT ( 'NONE',  ( 2.035157376598824452, 43.68868534415484106, 7.964842623401179544 ) ) ;
#22041 = CARTESIAN_POINT ( 'NONE',  ( 3.420591144908446957, 15.00000000000000000, 14.60477854057958425 ) ) ;
#22042 = AXIS2_PLACEMENT_3D ( 'NONE', #52172, #22177, #30634 ) ;
#22043 = CARTESIAN_POINT ( 'NONE',  ( 12.63842701281683922, 64.55059781766745175, -9.846743663894590881 ) ) ;
#22044 = CARTESIAN_POINT ( 'NONE',  ( 5.076628168052703671, 16.84226448433411960, 8.527530157486179263 ) ) ;
#22045 = CARTESIAN_POINT ( 'NONE',  ( 5.076628168052703671, 11.84226448433411960, 8.527530157486179263 ) ) ;
#22046 = CARTESIAN_POINT ( 'NONE',  ( -14.17193700899791153, 0.000000000000000000, 1.489530601563921808 ) ) ;
#22047 = CARTESIAN_POINT ( 'NONE',  ( 24.16423886937410614, 49.30374883491396787, 8.672049930838204340E-16 ) ) ;
#22048 = CARTESIAN_POINT ( 'NONE',  ( 9.402796353261066997, 14.49999999999999112, 11.68706210897770070 ) ) ;
#22049 = CIRCLE ( 'NONE', #63499, 6.349999999999995204 ) ;
#22050 = CARTESIAN_POINT ( 'NONE',  ( -6.607869636406716651, -50.96183896326274265, -3.750000000003224976 ) ) ;
#22051 = COLOUR_RGB ( '', 0.09019608, 0.27058824, 0.51372549) ;
#22052 = ORIENTED_EDGE ( 'NONE', *, *, #63005, .T. ) ;
#22053 = CARTESIAN_POINT ( 'NONE',  ( 13.79529636645030344, 58.26208216824728936, 14.16423886937410614 ) ) ;
#22055 = EDGE_CURVE ( 'NONE', #31483, #55265, #49838, .T. ) ;
#22054 = CARTESIAN_POINT ( 'NONE',  ( 4.559911319644449179, 2.230352010821504916, -9.422509992056141925 ) ) ;
#22056 = CARTESIAN_POINT ( 'NONE',  ( 5.076628168052704559, 35.17559781766745175, -8.527530157486179263 ) ) ;
#22057 = CARTESIAN_POINT ( 'NONE',  ( -2.816281873526473856, 39.12363466993041783, 9.499525473075851096E-16 ) ) ;
#22059 = CARTESIAN_POINT ( 'NONE',  ( 17.08211943468705130, 8.470415501580635720, 12.26659068614894998 ) ) ;
#22058 = CARTESIAN_POINT ( 'NONE',  ( -8.004782461319722486, 84.51756810411900744, -3.749999999999998668 ) ) ;
#22060 = CARTESIAN_POINT ( 'NONE',  ( 0.5774900079438590739, 12.64701867748817143, -5.440088680355550821 ) ) ;
#22061 = CARTESIAN_POINT ( 'NONE',  ( 24.16423886937410614, 54.51208216824730357, -3.795296366450302550 ) ) ;
#22062 = CARTESIAN_POINT ( 'NONE',  ( 18.52753015748618282, 38.92559781766745175, -4.923371831947291888 ) ) ;
#22063 = EDGE_CURVE ( 'NONE', #54112, #93500, #5351, .T. ) ;
#22064 = CARTESIAN_POINT ( 'NONE',  ( 19.39188664607695500, 40.83703382326399378, -6.499999999999968026 ) ) ;
#22065 = CARTESIAN_POINT ( 'NONE',  ( 5.076628168052703671, 21.84226448433411960, 8.527530157486179263 ) ) ;
#22066 = DIRECTION ( 'NONE',  ( 0.000000000000000000, 1.000000000000000000, 0.000000000000000000 ) ) ;
#22067 = CARTESIAN_POINT ( 'NONE',  ( -8.527530157486182816, 20.59226448433412671, -4.923371831947288335 ) ) ;
#22068 = EDGE_LOOP ( 'NONE', ( #56616, #26569, #8486, #80635 ) ) ;
#22069 = ORIENTED_EDGE ( 'NONE', *, *, #65811, .T. ) ;
#22070 = LINE ( 'NONE', #30526, #52568 ) ;
#22071 = ORIENTED_EDGE ( 'NONE', *, *, #80768, .F. ) ;
#22072 = CARTESIAN_POINT ( 'NONE',  ( 5.076628168052704559, 50.17559781766745886, -8.527530157486179263 ) ) ;
#22074 = CARTESIAN_POINT ( 'NONE',  ( 0.5774900079438607392, 38.48035201082150536, 5.440088680355550821 ) ) ;
#22073 = CARTESIAN_POINT ( 'NONE',  ( 4.559911319644449179, 38.89701867748817676, 9.422509992056141925 ) ) ;
#22076 = CARTESIAN_POINT ( 'NONE',  ( 13.43411237798105340, 35.58196800326375353, 12.81628187352647963 ) ) ;
#22075 = CARTESIAN_POINT ( 'NONE',  ( 0.1532563361054082862, 66.21726448433413736, 2.638427012816831674 ) ) ;
#22077 = CARTESIAN_POINT ( 'NONE',  ( 10.00000000000000178, 8.053748834913967869, 14.16423886937410082 ) ) ;
#22078 = CARTESIAN_POINT ( 'NONE',  ( 0.5774900079438590739, 67.64701867748817676, -5.440088680355550821 ) ) ;
#22079 = CARTESIAN_POINT ( 'NONE',  ( 10.00000000000000000, 32.87363466993042493, -12.81628187352647608 ) ) ;
#22080 = ORIENTED_EDGE ( 'NONE', *, *, #3915, .T. ) ;
#22081 = CARTESIAN_POINT ( 'NONE',  ( 2.791683348922237240, 50.38393115100078035, -7.208316651077763204 ) ) ;
#22082 = CARTESIAN_POINT ( 'NONE',  ( -0.8801773607110991993, 7.855352010821506248, -2.915334737309923874 ) ) ;
#22083 = ORIENTED_EDGE ( 'NONE', *, *, #22207, .T. ) ;
#22084 = CARTESIAN_POINT ( 'NONE',  ( 15.44008868035555793, 11.39701867748817143, -9.422509992056140149 ) ) ;
#22085 = VERTEX_POINT ( 'NONE', #4853 ) ;
#22086 = CARTESIAN_POINT ( 'NONE',  ( 15.44008868035555793, 51.39701867748816966, -9.422509992056140149 ) ) ;
#22087 = CARTESIAN_POINT ( 'NONE',  ( 20.88017736071110519, 60.56368534415484106, 2.639326808657452039E-16 ) ) ;
#22088 = CARTESIAN_POINT ( 'NONE',  ( 10.00000000000000178, 64.31368534415483396, 10.88017736071110342 ) ) ;
#22089 =( NAMED_UNIT ( * ) SI_UNIT ( $, .STERADIAN. ) SOLID_ANGLE_UNIT ( ) );
#22090 = CARTESIAN_POINT ( 'NONE',  ( 10.00000000000000178, 49.31368534415484106, 10.88017736071110342 ) ) ;
#22091 = CARTESIAN_POINT ( 'NONE',  ( -1.926860441876563801, 29.89664270246084499, 3.195792623639529761 ) ) ;
#22092 = CARTESIAN_POINT ( 'NONE',  ( 0.1532563361054083140, 11.00893115100078568, 1.131784320476157264E-15 ) ) ;
#22093 = CARTESIAN_POINT ( 'NONE',  ( 19.72487221294570858, 70.00000000000000000, 6.000000000000000000 ) ) ;
#22094 = CARTESIAN_POINT ( 'NONE',  ( 12.63842701281683034, 27.46726448433411250, 9.846743663894596210 ) ) ;
#22095 = VERTEX_POINT ( 'NONE', #35328 ) ;
#22096 = DIRECTION ( 'NONE',  ( 0.000000000000000000, 0.000000000000000000, 1.000000000000000000 ) ) ;
#22097 = CARTESIAN_POINT ( 'NONE',  ( -2.266590686148945544, 2.220415501580634388, 7.082119434687048631 ) ) ;
#22098 = ORIENTED_EDGE ( 'NONE', *, *, #15413, .T. ) ;
#22099 = CYLINDRICAL_SURFACE ( 'NONE', #80964, 15.00000000000000000 ) ;
#22100 = CARTESIAN_POINT ( 'NONE',  ( 7.084665262690076126, 9.105352010821503583, 10.88017736071109987 ) ) ;
#22101 = CARTESIAN_POINT ( 'NONE',  ( -0.1503990784575242878, 59.24884699246888431, -6.262539305110083276 ) ) ;
#22102 = VERTEX_POINT ( 'NONE', #65822 ) ;
#22103 = PLANE ( 'NONE',  #92731 ) ;
#22104 = CARTESIAN_POINT ( 'NONE',  ( 5.076628168052703671, 41.84226448433411605, 8.527530157486179263 ) ) ;
#22105 = CARTESIAN_POINT ( 'NONE',  ( 66.56412365047464164, 26.99999999999998224, 10.00000000000000000 ) ) ;
#22106 = CARTESIAN_POINT ( 'NONE',  ( -2.816281873526471635, 23.91530133659708568, -3.434112377981056508 ) ) ;
#22107 = CARTESIAN_POINT ( 'NONE',  ( 2.791683348922240793, 21.63393115100078745, 7.208316651077764092 ) ) ;
#22108 = CARTESIAN_POINT ( 'NONE',  ( 0.000000000000000000, 14.49999999999999822, 0.000000000000000000 ) ) ;
#22109 = CARTESIAN_POINT ( 'NONE',  ( 0.1532563361054082862, 21.21726448433412315, 2.638427012816831674 ) ) ;
#22110 = CARTESIAN_POINT ( 'NONE',  ( -2.816281873526473856, -0.6680319967362464695, 3.434112377981055619 ) ) ;
#22111 = VECTOR ( 'NONE', #12567, 1000.000000000000114 ) ;
#22112 = SURFACE_STYLE_USAGE ( .BOTH. , #30080 ) ;
#22113 = VERTEX_POINT ( 'NONE', #27827 ) ;
#22114 = ORIENTED_EDGE ( 'NONE', *, *, #6089, .T. ) ;
#22115 = CARTESIAN_POINT ( 'NONE',  ( 17.96484262340118221, 29.93868534415484106, 7.964842623401181321 ) ) ;
#22116 = CARTESIAN_POINT ( 'NONE',  ( 10.00000000000000178, 18.05374883491396787, 14.16423886937410082 ) ) ;
#22117 = CARTESIAN_POINT ( 'NONE',  ( 19.84674366389459266, 28.30059781766745886, 2.638427012816836559 ) ) ;
#22118 = CARTESIAN_POINT ( 'NONE',  ( 15.44008868035555260, 59.73035201082151247, 9.422509992056143702 ) ) ;
#22120 = CARTESIAN_POINT ( 'NONE',  ( -3.990799379706100325, -9.967613007074422882, -3.750000000000000000 ) ) ;
#22119 = CARTESIAN_POINT ( 'NONE',  ( -2.816281873526473856, 39.33196800326374643, 3.434112377981055619 ) ) ;
#22121 = CARTESIAN_POINT ( 'NONE',  ( 7.084665262690076126, 12.02201867748817143, -10.88017736071110164 ) ) ;
#22122 = B_SPLINE_CURVE_WITH_KNOTS ( 'NONE', 3,
 ( #92739, #84277, #55227, #24263, #93720, #9739 ),
 .UNSPECIFIED., .F., .F.,
 ( 4, 2, 4 ),
 ( 3.409110551494637202E-05, 0.0004400426677367930768, 0.0008459942299586397816 ),
 .UNSPECIFIED. ) ;
#22123 = DIRECTION ( 'NONE',  ( -0.000000000000000000, 0.000000000000000000, 1.000000000000000000 ) ) ;
#22124 = DIRECTION ( 'NONE',  ( -0.000000000000000000, -1.000000000000000000, -0.000000000000000000 ) ) ;
#22125 = CARTESIAN_POINT ( 'NONE',  ( 13.43411237798105340, 5.581968003263753531, 12.81628187352647963 ) ) ;
#22126 = CARTESIAN_POINT ( 'NONE',  ( 1.472469842513823179, 21.42559781766745175, 4.923371831947296329 ) ) ;
#22127 = CARTESIAN_POINT ( 'NONE',  ( -10.88017736071110342, -11.93631465584515894, 3.903127820947815962E-15 ) ) ;
#22128 = CARTESIAN_POINT ( 'NONE',  ( 3.591859063236763294, 33.29030133659708213, -11.09922568453595026 ) ) ;
#22130 = DIRECTION ( 'NONE',  ( -1.000000000000000000, 5.818595309480552676E-17, -0.000000000000000000 ) ) ;
#22129 = CARTESIAN_POINT ( 'NONE',  ( -0.8801773607110991993, 42.85535201082150536, -2.915334737309923874 ) ) ;
#22131 = ADVANCED_FACE ( 'NONE', ( #58313 ), #20340, .F. ) ;
#22132 = CARTESIAN_POINT ( 'NONE',  ( 14.11874224319630855, 0.2301510088455456793, -4.887061453530034072 ) ) ;
#22133 = CARTESIAN_POINT ( 'NONE',  ( 2.800000000000000266, 22.11937003968011695, 0.000000000000000000 ) ) ;
#22134 = CARTESIAN_POINT ( 'NONE',  ( 4.559911319644449179, 37.23035201082150536, -9.422509992056141925 ) ) ;
#22135 = CARTESIAN_POINT ( 'NONE',  ( 2.035157376598824452, 38.68868534415483396, 7.964842623401179544 ) ) ;
#22136 = DIRECTION ( 'NONE',  ( 0.000000000000000000, 0.000000000000000000, 1.000000000000000000 ) ) ;
#22137 = CARTESIAN_POINT ( 'NONE',  ( -3.396451007058964006E-33, -2.700807354125587310E-16, 0.000000000000000000 ) ) ;
#22138 = CARTESIAN_POINT ( 'NONE',  ( 1.472469842513823179, 35.59226448433412315, -4.923371831947296329 ) ) ;
#22139 = CARTESIAN_POINT ( 'NONE',  ( 17.96484262340118221, 6.188685344154836621, -7.964842623401177768 ) ) ;
#22140 = CARTESIAN_POINT ( 'NONE',  ( 13.43411237798106583, 17.66530133659708923, -12.81628187352647252 ) ) ;
#22141 = VERTEX_POINT ( 'NONE', #43324 ) ;
#22142 = CARTESIAN_POINT ( 'NONE',  ( 20.88017736071110164, 30.35535201082151247, 2.915334737309930979 ) ) ;
#22143 = CARTESIAN_POINT ( 'NONE',  ( 12.30000000000000249, 99.99999999999998579, 8.000000000000000000 ) ) ;
#22144 = CARTESIAN_POINT ( 'NONE',  ( 15.44008868035555793, 31.39701867748817676, -9.422509992056140149 ) ) ;
#22145 = CARTESIAN_POINT ( 'NONE',  ( 7.084665262690076126, 67.02201867748817676, -10.88017736071110164 ) ) ;
#22146 = CARTESIAN_POINT ( 'NONE',  ( 6.204703633549690345, 40.76208216824731778, -14.16423886937410259 ) ) ;
#22147 = CARTESIAN_POINT ( 'NONE',  ( 0.1532563361054100626, 30.80059781766744820, -2.638427012816831230 ) ) ;
#22148 = AXIS2_PLACEMENT_3D ( 'NONE', #63193, #55712, #86209 ) ;
#22149 = CARTESIAN_POINT ( 'NONE',  ( 20.88017736071110875, 45.77201867748816966, -2.915334737309920765 ) ) ;
#22150 = CARTESIAN_POINT ( 'NONE',  ( 0.000000000000000000, 0.5000000000000004441, 0.000000000000000000 ) ) ;
#22151 = CARTESIAN_POINT ( 'NONE',  ( 10.00000000000000000, 5.553748834913967869, -14.16423886937410082 ) ) ;
#22152 = VERTEX_POINT ( 'NONE', #35829 ) ;
#22153 = LINE ( 'NONE', #59645, #32155 ) ;
#22154 = CARTESIAN_POINT ( 'NONE',  ( 12.63842701281683034, 52.46726448433413026, 9.846743663894596210 ) ) ;
#22155 = ORIENTED_EDGE ( 'NONE', *, *, #6440, .T. ) ;
#22156 = ORIENTED_EDGE ( 'NONE', *, *, #86479, .F. ) ;
#22157 = CARTESIAN_POINT ( 'NONE',  ( 0.8952175423694801459, 62.60160829253887016, -5.990408912944315212 ) ) ;
#22158 = CARTESIAN_POINT ( 'NONE',  ( 20.36894250292379738, 19.92874883491396787, -10.36894250292379027 ) ) ;
#22160 = EDGE_CURVE ( 'NONE', #53609, #71459, #79854, .T. ) ;
#22159 = CARTESIAN_POINT ( 'NONE',  ( 17.08211943468705130, 18.47041550158063572, 12.26659068614894998 ) ) ;
#22161 = CARTESIAN_POINT ( 'NONE',  ( 10.00000000000000000, 56.81368534415484106, -10.88017736071110342 ) ) ;
#22162 = CARTESIAN_POINT ( 'NONE',  ( 13.79529636645031943, 65.34541550158063217, -14.16423886937409904 ) ) ;
#22163 = CARTESIAN_POINT ( 'NONE',  ( 10.00000000000000000, -2.126365330069579951, -12.81628187352647608 ) ) ;
#22164 = CARTESIAN_POINT ( 'NONE',  ( 12.63842701281683034, 42.46726448433412315, 9.846743663894596210 ) ) ;
#22165 = CARTESIAN_POINT ( 'NONE',  ( -8.000000000000000000, -0.01653120532836994255, 3.750000000000000000 ) ) ;
#22167 = CARTESIAN_POINT ( 'NONE',  ( 13.43411237798105340, 25.58196800326374998, 12.81628187352647963 ) ) ;
#22166 = CARTESIAN_POINT ( 'NONE',  ( 4.559911319644449179, 42.23035201082151247, -9.422509992056141925 ) ) ;
#22168 = CARTESIAN_POINT ( 'NONE',  ( -2.266590686148945544, 12.22041550158063394, 7.082119434687048631 ) ) ;
#22169 = CARTESIAN_POINT ( 'NONE',  ( 10.00000000000000000, 16.81368534415483751, -10.88017736071110342 ) ) ;
#22170 = CARTESIAN_POINT ( 'NONE',  ( 0.5774900079438590739, 17.64701867748817321, -5.440088680355550821 ) ) ;
#22171 = CARTESIAN_POINT ( 'NONE',  ( 7.551349515323100725, 0.000000000000000000, 12.08468537022911349 ) ) ;
#22172 = CARTESIAN_POINT ( 'NONE',  ( 17.96484262340118221, 61.18868534415482685, -7.964842623401177768 ) ) ;
#22173 = STYLED_ITEM ( 'NONE', ( #50408 ), #14065 ) ;
#22174 = CARTESIAN_POINT ( 'NONE',  ( 3.591859063236763294, 48.29030133659708923, -11.09922568453595026 ) ) ;
#22175 = CARTESIAN_POINT ( 'NONE',  ( 4.923371831947295441, -20.65773551566587685, -8.527530157486179263 ) ) ;
#22176 = EDGE_LOOP ( 'NONE', ( #79729, #27986, #41228, #56796 ) ) ;
#22177 = DIRECTION ( 'NONE',  ( 0.000000000000000000, 0.000000000000000000, -1.000000000000000000 ) ) ;
#22178 = ORIENTED_EDGE ( 'NONE', *, *, #55004, .T. ) ;
#22179 = CARTESIAN_POINT ( 'NONE',  ( 6.689969769698956625, 15.00000000000000000, -12.58200319823970226 ) ) ;
#22180 = B_SPLINE_CURVE_WITH_KNOTS ( 'NONE', 3,
 ( #15709, #47153, #77656, #9170, #39688, #1692 ),
 .UNSPECIFIED., .F., .F.,
 ( 4, 2, 4 ),
 ( 0.0002800553958269923053, 0.0006862611673083280749, 0.001092466938789663899 ),
 .UNSPECIFIED. ) ;
#22181 = ORIENTED_EDGE ( 'NONE', *, *, #74263, .T. ) ;
#22182 = CARTESIAN_POINT ( 'NONE',  ( -0.03743638938522463044, 19.25197528031019090, -6.399506433553971974 ) ) ;
#22184 = CARTESIAN_POINT ( 'NONE',  ( 12.91533473730992121, 4.522018677488170546, 10.88017736071110164 ) ) ;
#22183 = CARTESIAN_POINT ( 'NONE',  ( 22.26659068614894466, 53.88708216824731068, 7.082119434687054849 ) ) ;
#22186 = CARTESIAN_POINT ( 'NONE',  ( 14.92337183194729988, 44.34226448433412315, -8.527530157486177487 ) ) ;
#22185 = CARTESIAN_POINT ( 'NONE',  ( 2.791683348922240793, 16.63393115100078745, 7.208316651077764092 ) ) ;
#22187 = CARTESIAN_POINT ( 'NONE',  ( 12.14357320772536575, 54.02013147999952736, 2.900000000000000355 ) ) ;
#22188 = STYLED_ITEM ( 'NONE', ( #85734 ), #59599 ) ;
#22189 = CARTESIAN_POINT ( 'NONE',  ( 20.10493008474206178, 44.71697413083879979, 6.336235997365762707 ) ) ;
#22190 = AXIS2_PLACEMENT_3D ( 'NONE', #51434, #20452, #12447 ) ;
#22191 = CARTESIAN_POINT ( 'NONE',  ( 7.084665262690076126, 67.02201867748817676, -10.88017736071110164 ) ) ;
#22192 = B_SPLINE_CURVE_WITH_KNOTS ( 'NONE', 3,
 ( #15751, #22264, #30719, #83245 ),
 .UNSPECIFIED., .F., .F.,
 ( 4, 4 ),
 ( 1.388456241783856658E-18, 0.002657014572711311178 ),
 .UNSPECIFIED. ) ;
#22193 = CARTESIAN_POINT ( 'NONE',  ( -11.09922568453594316, 24.54030133659709634, 6.408140936763246920 ) ) ;
#22194 = EDGE_LOOP ( 'NONE', ( #51470, #46718, #67561, #94648 ) ) ;
#22195 = CARTESIAN_POINT ( 'NONE',  ( 24.16423886937410614, 39.51208216824731068, -3.795296366450302550 ) ) ;
#22196 = CARTESIAN_POINT ( 'NONE',  ( 0.6178305044545838731, 19.74863466993042138, 9.382169495545420901 ) ) ;
#22197 = ORIENTED_EDGE ( 'NONE', *, *, #86392, .F. ) ;
#22198 = CARTESIAN_POINT ( 'NONE',  ( 10.00000000000000178, 55.37363466993042493, 12.81628187352647608 ) ) ;
#22199 = ADVANCED_FACE ( 'NONE', ( #71861 ), #95774, .T. ) ;
#22200 = CARTESIAN_POINT ( 'NONE',  ( -0.8801773607111009756, 23.06368534415484106, 1.068504757029289695E-15 ) ) ;
#22201 = CARTESIAN_POINT ( 'NONE',  ( 7.361572987183170547, 37.05059781766744464, 9.846743663894590881 ) ) ;
#22202 = CARTESIAN_POINT ( 'NONE',  ( 2.035157376598824452, 28.68868534415484106, 7.964842623401179544 ) ) ;
#22203 = CARTESIAN_POINT ( 'NONE',  ( 22.81628187352648496, 61.83196800326376774, -3.434112377981050290 ) ) ;
#22204 = CARTESIAN_POINT ( 'NONE',  ( 19.72487221294570858, 70.00000000000000000, 6.000000000000000000 ) ) ;
#22205 = CARTESIAN_POINT ( 'NONE',  ( 12.63842701281683922, 54.55059781766745175, -9.846743663894590881 ) ) ;
#22206 = CARTESIAN_POINT ( 'NONE',  ( 5.076628168052704559, 50.17559781766745886, -8.527530157486179263 ) ) ;
#22207 = EDGE_CURVE ( 'NONE', #91180, #92042, #55886, .T. ) ;
#22208 = AXIS2_PLACEMENT_3D ( 'NONE', #41870, #49346, #33349 ) ;
#22210 = ORIENTED_EDGE ( 'NONE', *, *, #14370, .T. ) ;
#22209 = DIRECTION ( 'NONE',  ( 0.000000000000000000, 0.000000000000000000, 1.000000000000000000 ) ) ;
#22211 = CARTESIAN_POINT ( 'NONE',  ( -3.270351084886894188, 14.95037111082768710, 14.38617789677959991 ) ) ;
#22212 = DIRECTION ( 'NONE',  ( 0.000000000000000000, 1.000000000000000000, 0.000000000000000000 ) ) ;
#22213 = DIRECTION ( 'NONE',  ( -1.000000000000000000, -0.000000000000000000, -0.000000000000000000 ) ) ;
#22214 = ORIENTED_EDGE ( 'NONE', *, *, #64320, .T. ) ;
#22215 = FACE_OUTER_BOUND ( 'NONE', #46547, .T. ) ;
#22216 = CARTESIAN_POINT ( 'NONE',  ( 10.00000000000000178, 32.25893115100078745, 9.846743663894594434 ) ) ;
#22217 = DIRECTION ( 'NONE',  ( -1.000000000000000000, 0.000000000000000000, 0.000000000000000000 ) ) ;
#22218 = CARTESIAN_POINT ( 'NONE',  ( -2.816281873526473856, 39.33196800326374643, 3.434112377981055619 ) ) ;
#22219 = LINE ( 'NONE', #93151, #91474 ) ;
#22220 = ORIENTED_EDGE ( 'NONE', *, *, #64702, .T. ) ;
#22221 = CIRCLE ( 'NONE', #63654, 15.00000000000000000 ) ;
#22222 = CARTESIAN_POINT ( 'NONE',  ( 18.52753015748618282, 58.92559781766745886, -4.923371831947291888 ) ) ;
#22223 = DIRECTION ( 'NONE',  ( -0.000000000000000000, -1.000000000000000000, -0.000000000000000000 ) ) ;
#22224 = CARTESIAN_POINT ( 'NONE',  ( 5.076628168052704559, 35.17559781766745175, -8.527530157486179263 ) ) ;
#22225 = CARTESIAN_POINT ( 'NONE',  ( 17.08211943468705130, 28.47041550158063572, 12.26659068614894998 ) ) ;
#22226 = CARTESIAN_POINT ( 'NONE',  ( 17.20831665107776587, 44.13393115100078745, -7.208316651077762316 ) ) ;
#22227 = CARTESIAN_POINT ( 'NONE',  ( 6.565887622018943937, 53.08196800326374643, -12.81628187352647608 ) ) ;
#22228 = CARTESIAN_POINT ( 'NONE',  ( -15.00000000000000000, 83.99999999999998579, 4.000000000000000000 ) ) ;
#22229 = CARTESIAN_POINT ( 'NONE',  ( 19.84674366389459621, 8.508931151000785675, 7.409399052514197653E-17 ) ) ;
#22230 = FILL_AREA_STYLE ('',( #75208 ) ) ;
#22231 = CARTESIAN_POINT ( 'NONE',  ( 14.92337183194729988, 44.34226448433412315, -8.527530157486177487 ) ) ;
#22232 = CARTESIAN_POINT ( 'NONE',  ( 20.88017736071110164, 40.35535201082150536, 2.915334737309930979 ) ) ;
#22233 = CARTESIAN_POINT ( 'NONE',  ( -11.81378540890925066, 15.00000000000000000, -7.968498874458281200 ) ) ;
#22234 = CARTESIAN_POINT ( 'NONE',  ( -0.8801773607110991993, 52.85535201082151247, -2.915334737309923874 ) ) ;
#22235 = ORIENTED_EDGE ( 'NONE', *, *, #78802, .T. ) ;
#22236 = CARTESIAN_POINT ( 'NONE',  ( -10.58981376305295008, 15.00000000000000000, 9.535111140613638625 ) ) ;
#22237 = CARTESIAN_POINT ( 'NONE',  ( 20.88017736071110519, 20.56368534415484106, 2.639326808657452039E-16 ) ) ;
#22239 = CARTESIAN_POINT ( 'NONE',  ( 15.44008868035555260, 49.73035201082150536, 9.422509992056143702 ) ) ;
#22238 = CARTESIAN_POINT ( 'NONE',  ( 6.565887622018943937, -1.918031996736246692, -12.81628187352647608 ) ) ;
#22240 = CARTESIAN_POINT ( 'NONE',  ( 2.035157376598822676, 67.43868534415484817, -7.964842623401177768 ) ) ;
#22241 = PRESENTATION_STYLE_ASSIGNMENT (( #250 ) ) ;
#22242 = TOROIDAL_SURFACE ( 'NONE', #81245, 0.5000000000000000000, 0.2500000000000000000 ) ;
#22244 = LINE ( 'NONE', #75224, #94215 ) ;
#22243 = CARTESIAN_POINT ( 'NONE',  ( 10.00000000000000000, 41.81368534415484106, -10.88017736071110342 ) ) ;
#22245 = CARTESIAN_POINT ( 'NONE',  ( 5.076628168052703671, 6.842264484334118713, 8.527530157486179263 ) ) ;
#22246 = CARTESIAN_POINT ( 'NONE',  ( 7.361572987183169658, 24.96726448433412315, -9.846743663894592657 ) ) ;
#22247 = DIRECTION ( 'NONE',  ( 1.000000000000000000, -0.000000000000000000, -0.000000000000000000 ) ) ;
#22248 = CARTESIAN_POINT ( 'NONE',  ( 14.16423886937410259, 19.30374883491398208, -2.602085213965210642E-15 ) ) ;
#22249 = CARTESIAN_POINT ( 'NONE',  ( 0.1532563361054083140, 61.00893115100078745, 1.131784320476157264E-15 ) ) ;
#22251 = CARTESIAN_POINT ( 'NONE',  ( 0.2751277870542981341, 18.21833443783937767, 6.500000000000002665 ) ) ;
#22250 = CARTESIAN_POINT ( 'NONE',  ( -0.8801773607110991993, 2.855352010821504471, -2.915334737309923874 ) ) ;
#22252 = CARTESIAN_POINT ( 'NONE',  ( 3.384479038598308343, 14.76984929998921636, -14.55223509985378350 ) ) ;
#22254 = CARTESIAN_POINT ( 'NONE',  ( 13.79529636645031943, 20.34541550158063572, -14.16423886937409904 ) ) ;
#22253 = CIRCLE ( 'NONE', #54139, 13.75000000000001776 ) ;
#22255 = EDGE_CURVE ( 'NONE', #7251, #33002, #83800, .T. ) ;
#22256 = CARTESIAN_POINT ( 'NONE',  ( 22.26659068614894466, 48.88708216824730357, 7.082119434687054849 ) ) ;
#22257 = CARTESIAN_POINT ( 'NONE',  ( 12.91533473730993009, 6.605352010821504471, -10.88017736071109987 ) ) ;
#22258 = ORIENTED_EDGE ( 'NONE', *, *, #73127, .T. ) ;
#22259 = CARTESIAN_POINT ( 'NONE',  ( 18.52753015748618282, 18.92559781766745175, -4.923371831947291888 ) ) ;
#22260 = CARTESIAN_POINT ( 'NONE',  ( 12.91533473730993009, 31.60535201082150891, -10.88017736071109987 ) ) ;
#22261 = EDGE_CURVE ( 'NONE', #63379, #23275, #97340, .T. ) ;
#22262 = CARTESIAN_POINT ( 'NONE',  ( 19.84674366389459621, 43.50893115100078745, 7.409399052514197653E-17 ) ) ;
#22264 = CARTESIAN_POINT ( 'NONE',  ( 1.046131998950046382, 5.738109087357264215, 6.500000000000002665 ) ) ;
#22263 = CARTESIAN_POINT ( 'NONE',  ( -4.164238869374099927, 2.012082168247300906, 3.795296366450308767 ) ) ;
#22265 = CARTESIAN_POINT ( 'NONE',  ( 2.393480905993052854, 0.5000000000000004441, 14.80781041047752922 ) ) ;
#22266 = CARTESIAN_POINT ( 'NONE',  ( 19.84674366389459621, 3.508931151000785231, 7.409399052514197653E-17 ) ) ;
#22267 = CARTESIAN_POINT ( 'NONE',  ( 3.591859063236761518, 34.95696800326375353, 11.09922568453594849 ) ) ;
#22268 = CARTESIAN_POINT ( 'NONE',  ( 2.791683348922237240, 45.38393115100079456, -7.208316651077763204 ) ) ;
#22269 = ORIENTED_EDGE ( 'NONE', *, *, #80502, .F. ) ;
#22270 = CARTESIAN_POINT ( 'NONE',  ( 1.472469842513823179, 10.59226448433411782, -4.923371831947296329 ) ) ;
#22271 = CARTESIAN_POINT ( 'NONE',  ( 10.72174155805500995, -40.27583460507576518, -3.749999999996413536 ) ) ;
#22272 = CARTESIAN_POINT ( 'NONE',  ( 0.000000000000000000, 14.49999999999999822, 0.000000000000000000 ) ) ;
#22273 = CARTESIAN_POINT ( 'NONE',  ( 15.44008868035555260, 14.73035201082150536, 9.422509992056143702 ) ) ;
#22274 = AXIS2_PLACEMENT_3D ( 'NONE', #6193, #20200, #36698 ) ;
#22275 = CARTESIAN_POINT ( 'NONE',  ( 6.204703633549690345, 47.84541550158064638, 14.16423886937410082 ) ) ;
#22276 = CARTESIAN_POINT ( 'NONE',  ( 10.00000000000000178, 39.31368534415484106, 10.88017736071110342 ) ) ;
#22277 = CARTESIAN_POINT ( 'NONE',  ( -0.1049300847420624322, 32.21697413083879269, -6.336235997365760042 ) ) ;
#22278 =( NAMED_UNIT ( * ) PLANE_ANGLE_UNIT ( ) SI_UNIT ( $, .RADIAN. ) );
#22279 = CARTESIAN_POINT ( 'NONE',  ( 1.472469842513823179, 21.42559781766745175, 4.923371831947296329 ) ) ;
#22280 = CARTESIAN_POINT ( 'NONE',  ( 19.84674366389459266, 33.71726448433410894, -2.638427012816827677 ) ) ;
#22281 = FILL_AREA_STYLE ('',( #15280 ) ) ;
#22282 = CARTESIAN_POINT ( 'NONE',  ( 17.20831665107776587, 47.88393115100078745, 7.208316651077764980 ) ) ;
#22283 = AXIS2_PLACEMENT_3D ( 'NONE', #8014, #76988, #23522 ) ;
#22284 = CARTESIAN_POINT ( 'NONE',  ( 15.44008868035555793, 41.39701867748817676, -9.422509992056140149 ) ) ;
#22285 = VERTEX_POINT ( 'NONE', #30779 ) ;
#22286 = CARTESIAN_POINT ( 'NONE',  ( 13.43411237798105340, 55.58196800326374643, 12.81628187352647963 ) ) ;
#22288 = EDGE_CURVE ( 'NONE', #31232, #51688, #60305, .T. ) ;
#22287 = DIRECTION ( 'NONE',  ( 0.8870108331782150524, 0.000000000000000000, 0.4617486132350466232 ) ) ;
#22289 = CARTESIAN_POINT ( 'NONE',  ( 14.92337183194729988, 4.342264484334117824, -8.527530157486177487 ) ) ;
#22290 = CARTESIAN_POINT ( 'NONE',  ( 6.565887622018943937, 60.16530133659707502, 12.81628187352647430 ) ) ;
#22292 = CARTESIAN_POINT ( 'NONE',  ( 19.84674366389459266, 38.30059781766745175, 2.638427012816836559 ) ) ;
#22291 = CARTESIAN_POINT ( 'NONE',  ( 19.42250999205614193, 5.147018677488171434, 5.440088680355555262 ) ) ;
#22293 = CARTESIAN_POINT ( 'NONE',  ( 10.58521204051726627, 15.00000000000000000, 11.99294302885416563 ) ) ;
#22294 = DIRECTION ( 'NONE',  ( -0.6755902076156641289, 0.000000000000000000, 0.7372773368101204206 ) ) ;
#22295 = CARTESIAN_POINT ( 'NONE',  ( -2.266590686148945544, 41.38708216824729647, -7.082119434687050408 ) ) ;
#22296 = CARTESIAN_POINT ( 'NONE',  ( 2.791683348922237240, 55.38393115100078745, -7.208316651077763204 ) ) ;
#22297 = CARTESIAN_POINT ( 'NONE',  ( 17.72850354356589619, 33.99078749795486942, 10.00000000000000000 ) ) ;
#22298 = CARTESIAN_POINT ( 'NONE',  ( 7.084665262690076126, 32.02201867748816966, -10.88017736071110164 ) ) ;
#22299 = EDGE_CURVE ( 'NONE', #1418, #61640, #28435, .T. ) ;
#22300 = CARTESIAN_POINT ( 'NONE',  ( 19.84674366389459266, 3.717264484334118713, -2.638427012816827677 ) ) ;
#22301 = MECHANICAL_DESIGN_GEOMETRIC_PRESENTATION_REPRESENTATION (  '', ( #89220 ), #55765 ) ;
#22302 = DIRECTION ( 'NONE',  ( 1.000000000000000000, 0.000000000000000000, 0.000000000000000000 ) ) ;
#22303 = VERTEX_POINT ( 'NONE', #14326 ) ;
#22304 = CARTESIAN_POINT ( 'NONE',  ( 10.00000000000000000, 62.87363466993042493, -12.81628187352647608 ) ) ;
#22305 = VERTEX_POINT ( 'NONE', #67315 ) ;
#22306 = CARTESIAN_POINT ( 'NONE',  ( 10.00000000000000178, 2.258931151000784787, 9.846743663894594434 ) ) ;
#22307 = VERTEX_POINT ( 'NONE', #28812 ) ;
#22308 = CARTESIAN_POINT ( 'NONE',  ( 24.16423886937409904, 4.095415501580634832, 3.795296366450317205 ) ) ;
#22309 = CARTESIAN_POINT ( 'NONE',  ( 17.20831665107776587, 7.883931151000784787, 7.208316651077764980 ) ) ;
#22310 = CARTESIAN_POINT ( 'NONE',  ( 20.88017736071110875, 25.77201867748816966, -2.915334737309920765 ) ) ;
#22311 = AXIS2_PLACEMENT_3D ( 'NONE', #1863, #79310, #3314 ) ;
#22312 = CARTESIAN_POINT ( 'NONE',  ( 0.000000000000000000, 14.49999999999999822, 0.000000000000000000 ) ) ;
#22313 = EDGE_LOOP ( 'NONE', ( #7387, #79572, #13659, #8869 ) ) ;
#22314 = CARTESIAN_POINT ( 'NONE',  ( 0.5774900079438607392, 23.48035201082150536, 5.440088680355550821 ) ) ;
#22315 = EDGE_LOOP ( 'NONE', ( #24287, #31511, #33362, #7941, #5966, #11215 ) ) ;
#22316 = CARTESIAN_POINT ( 'NONE',  ( -0.8801773607111009756, 33.06368534415484106, 1.068504757029289695E-15 ) ) ;
#22317 = DIRECTION ( 'NONE',  ( -1.000000000000000000, 0.000000000000000000, 0.000000000000000000 ) ) ;
#22318 = ORIENTED_EDGE ( 'NONE', *, *, #9855, .T. ) ;
#22319 = EDGE_LOOP ( 'NONE', ( #92932, #14861, #81947, #97585 ) ) ;
#22320 = CARTESIAN_POINT ( 'NONE',  ( 3.591859063236763294, 18.29030133659708568, -11.09922568453595026 ) ) ;
#22321 = CARTESIAN_POINT ( 'NONE',  ( 19.42250999205614548, 65.98035201082151957, -5.440088680355545492 ) ) ;
#22322 = CARTESIAN_POINT ( 'NONE',  ( -8.606322355891443010, 3.794835101497137347E-16, 11.66967075398801335 ) ) ;
#22324 = DIRECTION ( 'NONE',  ( -0.000000000000000000, -1.000000000000000000, -0.000000000000000000 ) ) ;
#22323 = CARTESIAN_POINT ( 'NONE',  ( 10.00000000000000000, 21.81368534415484106, -10.88017736071110342 ) ) ;
#22325 = CARTESIAN_POINT ( 'NONE',  ( 10.00000000000000000, 9.758931151000785675, -9.846743663894594434 ) ) ;
#22326 = CARTESIAN_POINT ( 'NONE',  ( 20.88017736071110164, 30.35535201082151247, 2.915334737309930979 ) ) ;
#22327 = EDGE_CURVE ( 'NONE', #48119, #58781, #53395, .T. ) ;
#22328 = ORIENTED_EDGE ( 'NONE', *, *, #47764, .F. ) ;
#22329 = CARTESIAN_POINT ( 'NONE',  ( 19.38216949554541202, 60.99863466993042493, 9.382169495545424454 ) ) ;
#22330 = CARTESIAN_POINT ( 'NONE',  ( 20.88017736071110519, 45.56368534415484106, 2.639326808657452039E-16 ) ) ;
#22331 = CARTESIAN_POINT ( 'NONE',  ( -46.34323875807881166, 103.6109741468810483, -6.190393423093143888 ) ) ;
#22332 = CARTESIAN_POINT ( 'NONE',  ( 10.00000000000000178, 50.37363466993042493, 12.81628187352647608 ) ) ;
#22333 = CARTESIAN_POINT ( 'NONE',  ( 10.00000000000000000, 51.81368534415484106, -10.88017736071110342 ) ) ;
#22334 = CARTESIAN_POINT ( 'NONE',  ( 3.591859063236763294, -1.709698663402913210, -11.09922568453595026 ) ) ;
#22335 = PRESENTATION_STYLE_ASSIGNMENT (( #83811 ) ) ;
#22336 = CARTESIAN_POINT ( 'NONE',  ( 17.20831665107776587, 14.13393115100078568, -7.208316651077762316 ) ) ;
#22337 = CARTESIAN_POINT ( 'NONE',  ( 13.43411237798105340, 60.58196800326376064, 12.81628187352647963 ) ) ;
#22338 = CARTESIAN_POINT ( 'NONE',  ( 4.379999999999999893, 0.09082567841931840635, -3.750000000000000000 ) ) ;
#22339 = CARTESIAN_POINT ( 'NONE',  ( 0.1532563361054100626, 10.80059781766745175, -2.638427012816831230 ) ) ;
#22340 = CARTESIAN_POINT ( 'NONE',  ( 21.09922568453594849, 6.206968003263753531, 6.408140936763242479 ) ) ;
#22342 = CARTESIAN_POINT ( 'NONE',  ( 17.20831665107776587, 59.13393115100078745, -7.208316651077762316 ) ) ;
#22341 = SURFACE_SIDE_STYLE ('',( #7338 ) ) ;
#22343 = CARTESIAN_POINT ( 'NONE',  ( 7.084665262690076126, 39.10535201082150536, 10.88017736071109987 ) ) ;
#22344 = CARTESIAN_POINT ( 'NONE',  ( 12.63842701281683034, 52.46726448433413026, 9.846743663894596210 ) ) ;
#22345 = DIRECTION ( 'NONE',  ( -0.000000000000000000, -1.000000000000000000, -0.000000000000000000 ) ) ;
#22346 = AXIS2_PLACEMENT_3D ( 'NONE', #53185, #12717, #51213 ) ;
#22347 = CARTESIAN_POINT ( 'NONE',  ( 17.20831665107776587, 24.13393115100078035, -7.208316651077762316 ) ) ;
#22348 = CARTESIAN_POINT ( 'NONE',  ( 18.52753015748617571, 13.09226448433411960, 4.923371831947298993 ) ) ;
#22350 = ORIENTED_EDGE ( 'NONE', *, *, #47634, .T. ) ;
#22349 = CARTESIAN_POINT ( 'NONE',  ( 10.00000000000000000, 2.873634669930420049, -12.81628187352647608 ) ) ;
#22351 = CARTESIAN_POINT ( 'NONE',  ( 18.52753015748618282, 58.92559781766745886, -4.923371831947291888 ) ) ;
#22352 = CARTESIAN_POINT ( 'NONE',  ( 4.380000001225145212, 0.09385850579744531297, -2.500000000000000000 ) ) ;
#22353 = CARTESIAN_POINT ( 'NONE',  ( 2.917880565312948704, 67.63708216824730357, 12.26659068614894643 ) ) ;
#22354 = CARTESIAN_POINT ( 'NONE',  ( 1.472469842513823179, 45.59226448433412315, -4.923371831947296329 ) ) ;
#22355 = ORIENTED_EDGE ( 'NONE', *, *, #24095, .F. ) ;
#22356 = ADVANCED_FACE ( 'NONE', ( #30286 ), #90292, .F. ) ;
#22357 = CARTESIAN_POINT ( 'NONE',  ( 18.72515096720591643, 66.07228050351029935, -6.499999999999699796 ) ) ;
#22358 = CARTESIAN_POINT ( 'NONE',  ( 12.91533473730992121, 4.522018677488170546, 10.88017736071110164 ) ) ;
#22359 = DIRECTION ( 'NONE',  ( -0.000000000000000000, -0.000000000000000000, -1.000000000000000000 ) ) ;
#22360 = CARTESIAN_POINT ( 'NONE',  ( -0.8801773607111009756, 38.06368534415484106, 1.068504757029289695E-15 ) ) ;
#22361 = CARTESIAN_POINT ( 'NONE',  ( 17.08211943468705840, 45.13708216824730357, -12.26659068614894466 ) ) ;
#22363 = CARTESIAN_POINT ( 'NONE',  ( 9.876730923139232843, 14.63595249122789177, 11.28938378619070271 ) ) ;
#22362 = CARTESIAN_POINT ( 'NONE',  ( 2.035157376598824452, 3.688685344154837953, 7.964842623401179544 ) ) ;
#22364 = CARTESIAN_POINT ( 'NONE',  ( 7.361572987183169658, 4.967264484334119601, -9.846743663894592657 ) ) ;
#22365 = PRESENTATION_LAYER_ASSIGNMENT (  '', '', ( #15929 ) ) ;
#22366 = CARTESIAN_POINT ( 'NONE',  ( 19.84674366389459266, 28.30059781766745886, 2.638427012816836559 ) ) ;
#22367 = CARTESIAN_POINT ( 'NONE',  ( 16.40814093676324603, 12.45696800326375353, -11.09922568453594671 ) ) ;
#22368 = FACE_OUTER_BOUND ( 'NONE', #42683, .T. ) ;
#22369 = EDGE_CURVE ( 'NONE', #59748, #10735, #97840, .T. ) ;
#22370 = DIRECTION ( 'NONE',  ( 1.000000000000000000, 0.000000000000000000, 0.000000000000000000 ) ) ;
#22371 = CARTESIAN_POINT ( 'NONE',  ( 20.36894250292379738, 14.92874883491396432, -10.36894250292379027 ) ) ;
#22372 = CARTESIAN_POINT ( 'NONE',  ( 2.791683348922240793, 26.63393115100078745, 7.208316651077764092 ) ) ;
#22373 = LINE ( 'NONE', #76345, #14591 ) ;
#22374 = ORIENTED_EDGE ( 'NONE', *, *, #57735, .F. ) ;
#22375 = CARTESIAN_POINT ( 'NONE',  ( 24.16423886937410614, 34.30374883491396787, 8.672049930838204340E-16 ) ) ;
#22376 = EDGE_CURVE ( 'NONE', #32092, #37045, #4777, .T. ) ;
#22377 = EDGE_CURVE ( 'NONE', #54264, #93214, #62219, .T. ) ;
#22378 = CARTESIAN_POINT ( 'NONE',  ( 5.076628168052704559, 15.17559781766745175, -8.527530157486179263 ) ) ;
#22380 = CARTESIAN_POINT ( 'NONE',  ( -13.16767742306207545, 14.95037115938073491, -6.653539137814823867 ) ) ;
#22379 = DIRECTION ( 'NONE',  ( -0.9636304532086211738, 0.000000000000000000, -0.2672383760782636175 ) ) ;
#22381 = CARTESIAN_POINT ( 'NONE',  ( 15.44008868035555793, 31.39701867748817676, -9.422509992056140149 ) ) ;
#22382 = CARTESIAN_POINT ( 'NONE',  ( 19.38216949554541557, 57.24863466993042493, -9.382169495545420901 ) ) ;
#22383 = CARTESIAN_POINT ( 'NONE',  ( 10.00000000000000178, 9.313685344154839285, 10.88017736071110342 ) ) ;
#22384 = CARTESIAN_POINT ( 'NONE',  ( 22.81628187352647785, 31.62363466993042138, 6.195893100308588602E-16 ) ) ;
#22385 = SURFACE_SIDE_STYLE ('',( #52860 ) ) ;
#22386 = VERTEX_POINT ( 'NONE', #22811 ) ;
#22387 = CARTESIAN_POINT ( 'NONE',  ( 3.969999999999999751, 10.25000000000000000, -2.750000000000000000 ) ) ;
#22388 = DIRECTION ( 'NONE',  ( 1.257568779154408793E-17, 1.000000000000000000, -0.000000000000000000 ) ) ;
#22389 = CARTESIAN_POINT ( 'NONE',  ( 20.36894250292379738, 39.92874883491396787, -10.36894250292379027 ) ) ;
#22390 = CARTESIAN_POINT ( 'NONE',  ( -4.164238869374099039, 11.80374883491396965, 8.674139862899312516E-16 ) ) ;
#22391 = CARTESIAN_POINT ( 'NONE',  ( 20.88017736071110875, 10.77201867748817143, -2.915334737309920765 ) ) ;
#22392 = CARTESIAN_POINT ( 'NONE',  ( 20.88017736071110164, 40.35535201082150536, 2.915334737309930979 ) ) ;
#22393 = CARTESIAN_POINT ( 'NONE',  ( 0.000000000000000000, -97.00000000000000000, -2.750000000000000000 ) ) ;
#22394 = CARTESIAN_POINT ( 'NONE',  ( 13.99999999999999822, 11.50000000000000000, 6.000000000000000000 ) ) ;
#22395 = CARTESIAN_POINT ( 'NONE',  ( 20.88017736071110519, 55.56368534415484817, 2.639326808657452039E-16 ) ) ;
#22396 = CARTESIAN_POINT ( 'NONE',  ( 2.035157376598822676, 62.43868534415483396, -7.964842623401177768 ) ) ;
#22397 = CARTESIAN_POINT ( 'NONE',  ( 21.09922568453594849, 21.20696800326375353, 6.408140936763242479 ) ) ;
#22398 = CARTESIAN_POINT ( 'NONE',  ( -0.1023957841222421367, 30.13377557478298385, 6.340343622311920946 ) ) ;
#22399 = CARTESIAN_POINT ( 'NONE',  ( 2.791683348922240793, 41.63393115100078745, 7.208316651077764092 ) ) ;
#22400 = UNCERTAINTY_MEASURE_WITH_UNIT (LENGTH_MEASURE( 1.000000000000000082E-05 ), #69495, 'distance_accuracy_value', 'NONE');
#22401 = CIRCLE ( 'NONE', #89469, 0.2500000000000002220 ) ;
#22402 = CARTESIAN_POINT ( 'NONE',  ( 19.38216949554541202, 15.99863466993042138, 9.382169495545424454 ) ) ;
#22403 = CARTESIAN_POINT ( 'NONE',  ( 1.274849032794223680, 28.57228050351031001, 6.499999999999884537 ) ) ;
#22404 = CARTESIAN_POINT ( 'NONE',  ( 15.44008868035555260, 4.730352010821504471, 9.422509992056143702 ) ) ;
#22405 = CARTESIAN_POINT ( 'NONE',  ( 18.52753015748618282, 38.92559781766745175, -4.923371831947291888 ) ) ;
#22406 = CARTESIAN_POINT ( 'NONE',  ( 3.591859063236763294, 58.29030133659708923, -11.09922568453595026 ) ) ;
#22407 = CARTESIAN_POINT ( 'NONE',  ( 10.00000000000000000, 14.75893115100078568, -9.846743663894594434 ) ) ;
#22408 = CARTESIAN_POINT ( 'NONE',  ( 2.917880565312948704, 2.637082168247300906, 12.26659068614894643 ) ) ;
#22409 = CARTESIAN_POINT ( 'NONE',  ( 18.72515096720568195, 31.07228050351032422, -6.500000000000018652 ) ) ;
#22410 = CARTESIAN_POINT ( 'NONE',  ( 7.084665262690076126, 37.02201867748817676, -10.88017736071110164 ) ) ;
#22411 = EDGE_CURVE ( 'NONE', #68868, #3541, #14827, .T. ) ;
#22412 = AXIS2_PLACEMENT_3D ( 'NONE', #32074, #24114, #69118 ) ;
#22413 = CARTESIAN_POINT ( 'NONE',  ( 4.559911319644449179, 32.23035201082150536, -9.422509992056141925 ) ) ;
#22414 = CARTESIAN_POINT ( 'NONE',  ( 17.96484262340118221, 16.18868534415483396, -7.964842623401177768 ) ) ;
#22415 = ORIENTED_EDGE ( 'NONE', *, *, #13989, .T. ) ;
#22416 =( BOUNDED_CURVE ( )  B_SPLINE_CURVE ( 2, ( #86223, #36910, #90881, #67402, #90380, #21918, #52397, #82896, #22409 ),
 .UNSPECIFIED., .F., .F. ) 
 B_SPLINE_CURVE_WITH_KNOTS ( ( 3, 2, 2, 2, 3 ),
 ( 0.4034289457926085731, 0.4047619047619047672, 0.4107142857142856984, 0.4166666666666666852, 0.4179996256359633233 ),
 .UNSPECIFIED. ) 
 CURVE ( )  GEOMETRIC_REPRESENTATION_ITEM ( )  RATIONAL_B_SPLINE_CURVE ( ( 0.9881565478350746723, 0.9923695281211503127, 1.000000000000000000, 0.9659258262890683122, 1.000000000000000000, 0.9659258262890683122, 1.000000000000000000, 0.9923695281211478703, 0.9881565478350720078 ) ) 
 REPRESENTATION_ITEM ( '' )  );
#22417 = CIRCLE ( 'NONE', #78278, 14.49999999999999822 ) ;
#22418 = CARTESIAN_POINT ( 'NONE',  ( 10.00000000000000178, 24.31368534415484106, 10.88017736071110342 ) ) ;
#22419 = CARTESIAN_POINT ( 'NONE',  ( 3.591859063236761518, 49.95696800326375353, 11.09922568453594849 ) ) ;
#22420 = CARTESIAN_POINT ( 'NONE',  ( -0.8801773607111009756, 48.06368534415484817, 1.068504757029289695E-15 ) ) ;
#22422 = CARTESIAN_POINT ( 'NONE',  ( 19.42250999205614548, 45.98035201082150536, -5.440088680355545492 ) ) ;
#22421 =( NAMED_UNIT ( * ) SI_UNIT ( $, .STERADIAN. ) SOLID_ANGLE_UNIT ( ) );
#22423 = VERTEX_POINT ( 'NONE', #91792 ) ;
#22424 = CARTESIAN_POINT ( 'NONE',  ( 17.20831665107776587, 57.88393115100078745, 7.208316651077764980 ) ) ;
#22425 = CARTESIAN_POINT ( 'NONE',  ( 12.91533473730993009, 31.60535201082150891, -10.88017736071109987 ) ) ;
#22426 = CARTESIAN_POINT ( 'NONE',  ( 5.365144748710862110, -17.52568678401977920, 4.000000000000000000 ) ) ;
#22427 = PRESENTATION_STYLE_ASSIGNMENT (( #90899 ) ) ;
#22428 = FACE_OUTER_BOUND ( 'NONE', #6283, .T. ) ;
#22429 = CARTESIAN_POINT ( 'NONE',  ( 6.204703633549690345, 47.84541550158064638, 14.16423886937410082 ) ) ;
#22430 = CARTESIAN_POINT ( 'NONE',  ( 12.91533473730993009, 56.60535201082151247, -10.88017736071109987 ) ) ;
#22431 = DIRECTION ( 'NONE',  ( 1.000000000000000000, 0.000000000000000000, 0.000000000000000000 ) ) ;
#22432 =( NAMED_UNIT ( * ) SI_UNIT ( $, .STERADIAN. ) SOLID_ANGLE_UNIT ( ) );
#22433 = CARTESIAN_POINT ( 'NONE',  ( 18.52753015748618282, 58.92559781766745886, -4.923371831947291888 ) ) ;
#22434 = CARTESIAN_POINT ( 'NONE',  ( 7.084665262690076126, 4.105352010821503583, 10.88017736071109987 ) ) ;
#22435 = CARTESIAN_POINT ( 'NONE',  ( 14.92337183194729633, 32.67559781766745175, 8.527530157486181039 ) ) ;
#22436 = ORIENTED_EDGE ( 'NONE', *, *, #10761, .F. ) ;
#22437 = CARTESIAN_POINT ( 'NONE',  ( 19.84674366389459266, 33.71726448433410894, -2.638427012816827677 ) ) ;
#22438 = CARTESIAN_POINT ( 'NONE',  ( -3.434112377981047626, -14.83469866340291610, 12.81628187352647963 ) ) ;
#22439 = CARTESIAN_POINT ( 'NONE',  ( -0.8801773607111008646, 28.27201867748817321, 2.915334737309923430 ) ) ;
#22440 = CARTESIAN_POINT ( 'NONE',  ( 18.52753015748618282, 33.92559781766745886, -4.923371831947291888 ) ) ;
#22441 = CARTESIAN_POINT ( 'NONE',  ( -2.816281873526473856, 19.12363466993042138, 9.499525473075851096E-16 ) ) ;
#22443 = CARTESIAN_POINT ( 'NONE',  ( 2.035157376598824452, 58.68868534415482685, 7.964842623401179544 ) ) ;
#22442 = CARTESIAN_POINT ( 'NONE',  ( 13.99999999999999822, 11.50000000000000000, 6.500000000000000888 ) ) ;
#22444 = CARTESIAN_POINT ( 'NONE',  ( 20.88017736071110164, 35.35535201082150536, 2.915334737309930979 ) ) ;
#22445 = CARTESIAN_POINT ( 'NONE',  ( 13.79529636645030344, 48.26208216824728936, 14.16423886937410614 ) ) ;
#22446 = VECTOR ( 'NONE', #98234, 1000.000000000000000 ) ;
#22447 = CARTESIAN_POINT ( 'NONE',  ( -9.399392868737665552, 3.795627280083113010E-16, -11.04089732309487104 ) ) ;
#22448 = VERTEX_POINT ( 'NONE', #45805 ) ;
#22449 = CARTESIAN_POINT ( 'NONE',  ( 3.591859063236761518, 19.95696800326375353, 11.09922568453594849 ) ) ;
#22450 = CARTESIAN_POINT ( 'NONE',  ( -0.8801773607111009756, 3.063685344154837509, 1.068504757029289695E-15 ) ) ;
#22451 = CARTESIAN_POINT ( 'NONE',  ( 17.96484262340118221, 41.18868534415484106, -7.964842623401177768 ) ) ;
#22452 = FACE_OUTER_BOUND ( 'NONE', #5779, .T. ) ;
#22453 = ORIENTED_EDGE ( 'NONE', *, *, #68187, .F. ) ;
#22454 = CARTESIAN_POINT ( 'NONE',  ( 12.91533473730993009, 56.60535201082151247, -10.88017736071109987 ) ) ;
#22455 = CARTESIAN_POINT ( 'NONE',  ( 7.361572987183169658, 29.96726448433411960, -9.846743663894592657 ) ) ;
#22456 = CARTESIAN_POINT ( 'NONE',  ( 7.361572987183170547, 27.05059781766745175, 9.846743663894590881 ) ) ;
#22457 = CARTESIAN_POINT ( 'NONE',  ( 7.361572987183169658, 14.96726448433411960, -9.846743663894592657 ) ) ;
#22459 = CARTESIAN_POINT ( 'NONE',  ( 22.81628187352647785, 41.62363466993042493, 6.195893100308588602E-16 ) ) ;
#22458 = CARTESIAN_POINT ( 'NONE',  ( -6.982525766850296023, -88.11956318484570261, 2.500000000000000888 ) ) ;
#22461 = CARTESIAN_POINT ( 'NONE',  ( -7.771322705631315664, 15.00000000000000000, -12.24159072199926257 ) ) ;
#22460 = CARTESIAN_POINT ( 'NONE',  ( 18.52753015748617571, 13.09226448433411960, 4.923371831947298993 ) ) ;
#22462 = CARTESIAN_POINT ( 'NONE',  ( 4.906773990575424627, -8.256880746075378141, -4.000000000000000000 ) ) ;
#22464 = ORIENTED_EDGE ( 'NONE', *, *, #59715, .T. ) ;
#22463 = CARTESIAN_POINT ( 'NONE',  ( 17.20831665107776587, 27.88393115100078390, 7.208316651077764980 ) ) ;
#22465 = LINE ( 'NONE', #37969, #13449 ) ;
#22466 = CARTESIAN_POINT ( 'NONE',  ( -2.816281873526473856, 14.12363466993041961, 9.499525473075851096E-16 ) ) ;
#22467 = CARTESIAN_POINT ( 'NONE',  ( 12.91533473730993009, 51.60535201082149825, -10.88017736071109987 ) ) ;
#22468 = CARTESIAN_POINT ( 'NONE',  ( 13.79529636645030344, 28.26208216824729647, 14.16423886937410614 ) ) ;
#22469 = AXIS2_PLACEMENT_3D ( 'NONE', #33416, #33904, #88410 ) ;
#22470 = UNCERTAINTY_MEASURE_WITH_UNIT (LENGTH_MEASURE( 1.000000000000000082E-05 ), #95002, 'distance_accuracy_value', 'NONE');
#22471 = CARTESIAN_POINT ( 'NONE',  ( -10.03950393934412411, 88.95408272062866217, 5.473102654073078277 ) ) ;
#22472 = CARTESIAN_POINT ( 'NONE',  ( 24.16423886937410614, 34.51208216824731068, -3.795296366450302550 ) ) ;
#22473 = CIRCLE ( 'NONE', #27227, 0.2500000000000000000 ) ;
#22474 = CARTESIAN_POINT ( 'NONE',  ( 22.26659068614895176, 44.72041550158063927, -7.082119434687042414 ) ) ;
#22475 = CARTESIAN_POINT ( 'NONE',  ( -2.266590686148945544, 7.220415501580634832, 7.082119434687048631 ) ) ;
#22477 = CARTESIAN_POINT ( 'NONE',  ( -13.11254139118232231, 91.00000000000000000, -8.000000000000000000 ) ) ;
#22476 = CARTESIAN_POINT ( 'NONE',  ( 10.00000000000000178, 23.05374883491397142, 14.16423886937410082 ) ) ;
#22478 = CARTESIAN_POINT ( 'NONE',  ( 12.91533473730993009, 51.60535201082149825, -10.88017736071109987 ) ) ;
#22479 = CARTESIAN_POINT ( 'NONE',  ( 5.510795456469524289, -25.29786701974074603, -2.750000000000000000 ) ) ;
#22480 = CARTESIAN_POINT ( 'NONE',  ( 0.1532563361054100626, 35.80059781766745175, -2.638427012816831230 ) ) ;
#22481 = ADVANCED_FACE ( 'NONE', ( #29305 ), #51324, .F. ) ;
#22484 = CIRCLE ( 'NONE', #22274, 6.499999999999995559 ) ;
#22483 = CARTESIAN_POINT ( 'NONE',  ( 19.84674366389459266, 48.30059781766745175, 2.638427012816836559 ) ) ;
#22482 = CARTESIAN_POINT ( 'NONE',  ( 0.000000000000000000, 0.5000000000000004441, 0.000000000000000000 ) ) ;
#22485 = CARTESIAN_POINT ( 'NONE',  ( -0.8801773607110991993, 17.85535201082150536, -2.915334737309923874 ) ) ;
#22486 = CARTESIAN_POINT ( 'NONE',  ( -1.099225684535947600, 54.54030133659708923, 6.408140936763237150 ) ) ;
#22487 = CARTESIAN_POINT ( 'NONE',  ( 18.52753015748617571, 63.09226448433412315, 4.923371831947298993 ) ) ;
#22488 = CARTESIAN_POINT ( 'NONE',  ( 20.00000000000000711, 81.00008901408247652, -4.500000004388789776 ) ) ;
#22489 = CARTESIAN_POINT ( 'NONE',  ( 0.1532563361054100626, 25.80059781766744820, -2.638427012816831230 ) ) ;
#22490 = CARTESIAN_POINT ( 'NONE',  ( 10.00000000000000000, 52.87363466993041783, -12.81628187352647608 ) ) ;
#22491 = CARTESIAN_POINT ( 'NONE',  ( 14.16423886937410259, -20.69625116508602858, -2.602085213965210642E-15 ) ) ;
#22492 = CARTESIAN_POINT ( 'NONE',  ( 19.42250999205614193, 45.14701867748817676, 5.440088680355555262 ) ) ;
#22493 = CARTESIAN_POINT ( 'NONE',  ( 19.84674366389459266, 53.30059781766744464, 2.638427012816836559 ) ) ;
#22494 = ADVANCED_FACE ( 'NONE', ( #81808 ), #90981, .T. ) ;
#22495 = CARTESIAN_POINT ( 'NONE',  ( -2.266590686148945544, 41.38708216824729647, -7.082119434687050408 ) ) ;
#22496 = EDGE_LOOP ( 'NONE', ( #32964, #24980, #57810, #90047 ) ) ;
#22497 = CARTESIAN_POINT ( 'NONE',  ( 2.917880565312948704, 2.637082168247300906, 12.26659068614894643 ) ) ;
#22498 = EDGE_CURVE ( 'NONE', #10866, #47816, #59800, .T. ) ;
#22499 = CARTESIAN_POINT ( 'NONE',  ( 10.00000000000000000, 56.81368534415484106, -10.88017736071110342 ) ) ;
#22500 = CARTESIAN_POINT ( 'NONE',  ( 10.00000000000000000, 66.81368534415484817, -10.88017736071110342 ) ) ;
#22501 = CARTESIAN_POINT ( 'NONE',  ( 17.08211943468705840, 55.13708216824731068, -12.26659068614894466 ) ) ;
#22502 = CARTESIAN_POINT ( 'NONE',  ( 22.81628187352648496, 11.83196800326375531, -3.434112377981050290 ) ) ;
#22503 = DIRECTION ( 'NONE',  ( 0.000000000000000000, 0.000000000000000000, 1.000000000000000000 ) ) ;
#22504 = CARTESIAN_POINT ( 'NONE',  ( -0.8801773607111009756, 48.06368534415484817, 1.068504757029289695E-15 ) ) ;
#22505 = LINE ( 'NONE', #52977, #26238 ) ;
#22506 = DIRECTION ( 'NONE',  ( -1.000000000000000000, 0.000000000000000000, 0.000000000000000000 ) ) ;
#22507 = CARTESIAN_POINT ( 'NONE',  ( 20.36894250292379382, 53.67874883491397497, 10.36894250292379205 ) ) ;
#22508 = CARTESIAN_POINT ( 'NONE',  ( -10.88017736071110342, 23.06368534415484461, 3.903127820947815962E-15 ) ) ;
#22509 = CARTESIAN_POINT ( 'NONE',  ( 2.035157376598822676, 12.43868534415483751, -7.964842623401177768 ) ) ;
#22510 = CARTESIAN_POINT ( 'NONE',  ( 12.91533473730992121, 24.52201867748816966, 10.88017736071110164 ) ) ;
#22511 = CARTESIAN_POINT ( 'NONE',  ( 7.361572987183169658, 59.96726448433410894, -9.846743663894592657 ) ) ;
#22512 = CARTESIAN_POINT ( 'NONE',  ( -2.816281873526473856, 44.33196800326375353, 3.434112377981055619 ) ) ;
#22513 = CARTESIAN_POINT ( 'NONE',  ( 19.72487221294571214, 37.80223176428831522, -6.499999999999988454 ) ) ;
#22514 = EDGE_LOOP ( 'NONE', ( #43675, #11998, #10517, #90710 ) ) ;
#22515 = CARTESIAN_POINT ( 'NONE',  ( -0.8801773607111008646, 13.27201867748817143, 2.915334737309923430 ) ) ;
#22516 = CARTESIAN_POINT ( 'NONE',  ( -2.816281873526473856, 14.12363466993041961, 9.499525473075851096E-16 ) ) ;
#22517 = DIRECTION ( 'NONE',  ( 1.000000000000000000, 0.000000000000000000, 0.000000000000000000 ) ) ;
#22518 = VECTOR ( 'NONE', #3438, 1000.000000000000000 ) ;
#22519 = CARTESIAN_POINT ( 'NONE',  ( 17.20831665107776587, 54.13393115100079456, -7.208316651077762316 ) ) ;
#22520 = CARTESIAN_POINT ( 'NONE',  ( 20.88017736071110519, 35.56368534415484106, 2.639326808657452039E-16 ) ) ;
#22521 = CARTESIAN_POINT ( 'NONE',  ( -1.099225684535947600, 19.54030133659708568, 6.408140936763237150 ) ) ;
#22522 = CARTESIAN_POINT ( 'NONE',  ( 4.559911319644449179, 48.89701867748817676, 9.422509992056141925 ) ) ;
#22523 =( BOUNDED_CURVE ( )  B_SPLINE_CURVE ( 2, ( #44220, #74724, #42269, #72740, #4273, #34747, #65236, #95761, #27246, #19754, #80754 ),
 .UNSPECIFIED., .F., .F. ) 
 B_SPLINE_CURVE_WITH_KNOTS ( ( 3, 2, 2, 2, 2, 3 ),
 ( 0.5443736480827608970, 0.5444444444444443976, 0.5500000000000000444, 0.5555555555555555802, 0.5611111111111111160, 0.5666666666666666519 ),
 .UNSPECIFIED. ) 
 CURVE ( )  GEOMETRIC_REPRESENTATION_ITEM ( )  RATIONAL_B_SPLINE_CURVE ( ( 0.9991426288945820522, 0.9995657810453010272, 1.000000000000000000, 0.9659258262890683122, 1.000000000000000000, 0.9659258262890683122, 1.000000000000000000, 0.9659258262890683122, 1.000000000000000000, 0.9659258262890683122, 1.000000000000000000 ) ) 
 REPRESENTATION_ITEM ( '' )  );
#22524 = CARTESIAN_POINT ( 'NONE',  ( 18.72515096720571037, 55.05509018479936145, 6.499999999999982236 ) ) ;
#22525 = CARTESIAN_POINT ( 'NONE',  ( -2.816281873526473856, 54.12363466993041783, 9.499525473075851096E-16 ) ) ;
#22526 = ORIENTED_EDGE ( 'NONE', *, *, #44244, .F. ) ;
#22527 = CARTESIAN_POINT ( 'NONE',  ( -9.065164099344672266, 14.49999999999999112, 11.95084933600764820 ) ) ;
#22528 = CARTESIAN_POINT ( 'NONE',  ( 10.00000000000000000, 46.81368534415484106, -10.88017736071110342 ) ) ;
#22530 = CARTESIAN_POINT ( 'NONE',  ( 10.00000000000000000, 5.553748834913967869, -14.16423886937410082 ) ) ;
#22529 = CARTESIAN_POINT ( 'NONE',  ( 0.6178305044545818747, 33.49863466993042493, -9.382169495545419124 ) ) ;
#22531 = EDGE_CURVE ( 'NONE', #50677, #48484, #31269, .T. ) ;
#22532 = CARTESIAN_POINT ( 'NONE',  ( 4.559911319644449179, 57.23035201082150536, -9.422509992056141925 ) ) ;
#22533 = CARTESIAN_POINT ( 'NONE',  ( 6.204703633549690345, 45.76208216824729647, -14.16423886937410259 ) ) ;
#22534 = CARTESIAN_POINT ( 'NONE',  ( 11.35178980618967337, 14.49999999999999822, 9.804941009311999522 ) ) ;
#22535 = CARTESIAN_POINT ( 'NONE',  ( 19.84674366389459266, 13.30059781766745353, 2.638427012816836559 ) ) ;
#22536 = CARTESIAN_POINT ( 'NONE',  ( 12.63842701281683922, 4.550597817667451750, -9.846743663894590881 ) ) ;
#22537 = CARTESIAN_POINT ( 'NONE',  ( 2.599899806584774264, 0.4361964623231012195, -6.495912400107028084 ) ) ;
#22538 = CARTESIAN_POINT ( 'NONE',  ( 17.08211943468705840, 45.13708216824730357, -12.26659068614894466 ) ) ;
#22539 = VECTOR ( 'NONE', #74206, 1000.000000000000000 ) ;
#22540 = CARTESIAN_POINT ( 'NONE',  ( 20.24186590665278018, 25.59014588040357197, -6.114288769123027656 ) ) ;
#22541 = CARTESIAN_POINT ( 'NONE',  ( -4.787219229845119273, -17.54708441700886468, -3.999999999999998224 ) ) ;
#22542 = AXIS2_PLACEMENT_3D ( 'NONE', #18564, #18075, #93072 ) ;
#22543 = VERTEX_POINT ( 'NONE', #31766 ) ;
#22544 = EDGE_LOOP ( 'NONE', ( #50191, #91783, #19622, #66090 ) ) ;
#22545 = CARTESIAN_POINT ( 'NONE',  ( 2.035157376598822676, 12.43868534415483751, -7.964842623401177768 ) ) ;
#22546 = CARTESIAN_POINT ( 'NONE',  ( -2.266590686148945544, 57.22041550158063217, 7.082119434687048631 ) ) ;
#22547 = CARTESIAN_POINT ( 'NONE',  ( 19.84674366389459266, 48.30059781766745175, 2.638427012816836559 ) ) ;
#22548 = CARTESIAN_POINT ( 'NONE',  ( 19.38216949554541202, 40.99863466993042493, 9.382169495545424454 ) ) ;
#22549 = DIRECTION ( 'NONE',  ( 0.000000000000000000, 0.000000000000000000, -1.000000000000000000 ) ) ;
#22551 = CARTESIAN_POINT ( 'NONE',  ( 6.204703633549690345, 0.7620821682473009062, -14.16423886937410259 ) ) ;
#22550 = CARTESIAN_POINT ( 'NONE',  ( 3.897244926435189161, 15.00000000000000000, 13.96644127842154148 ) ) ;
#22552 = CARTESIAN_POINT ( 'NONE',  ( 10.00000000000000000, 6.813685344154838397, -10.88017736071110342 ) ) ;
#22553 = CARTESIAN_POINT ( 'NONE',  ( -0.3689425029237898834, 61.17874883491396076, -10.36894250292378850 ) ) ;
#22554 = CARTESIAN_POINT ( 'NONE',  ( 7.361572987183170547, 42.05059781766745886, 9.846743663894590881 ) ) ;
#22555 = DIRECTION ( 'NONE',  ( -0.7489557207889991908, 0.000000000000000000, -0.6626200482157409422 ) ) ;
#22556 = CARTESIAN_POINT ( 'NONE',  ( 0.1532563361054100626, 20.80059781766744464, -2.638427012816831230 ) ) ;
#22557 =( GEOMETRIC_REPRESENTATION_CONTEXT ( 3 ) GLOBAL_UNCERTAINTY_ASSIGNED_CONTEXT ( ( #97417 ) ) GLOBAL_UNIT_ASSIGNED_CONTEXT ( ( #23265, #45756, #18088 ) ) REPRESENTATION_CONTEXT ( 'NONE', 'WORKASPACE' ) );
#22558 =( LENGTH_UNIT ( ) NAMED_UNIT ( * ) SI_UNIT ( .MILLI., .METRE. ) );
#22559 = CARTESIAN_POINT ( 'NONE',  ( -2.638427012816840111, 9.967264484334121377, -9.846743663894590881 ) ) ;
#22560 = ORIENTED_EDGE ( 'NONE', *, *, #73061, .T. ) ;
#22561 = ORIENTED_EDGE ( 'NONE', *, *, #73026, .F. ) ;
#22562 = FILL_AREA_STYLE_COLOUR ( '', #73331 ) ;
#22563 = ORIENTED_EDGE ( 'NONE', *, *, #52791, .T. ) ;
#22564 = CARTESIAN_POINT ( 'NONE',  ( 10.00000000000000178, 62.25893115100078745, 9.846743663894594434 ) ) ;
#22566 = CARTESIAN_POINT ( 'NONE',  ( 12.91533473730993009, 36.60535201082151247, -10.88017736071109987 ) ) ;
#22565 = CARTESIAN_POINT ( 'NONE',  ( -0.8801773607111008646, 33.27201867748817676, 2.915334737309923430 ) ) ;
#22568 = CARTESIAN_POINT ( 'NONE',  ( 22.81628187352647785, 31.41530133659709279, 3.434112377981063169 ) ) ;
#22567 = CARTESIAN_POINT ( 'NONE',  ( 10.00000000000000178, 67.25893115100079456, 9.846743663894594434 ) ) ;
#22569 = CARTESIAN_POINT ( 'NONE',  ( 20.36894250292379738, 9.928748834913966093, -10.36894250292379027 ) ) ;
#22570 = CARTESIAN_POINT ( 'NONE',  ( 3.591859063236761518, 39.95696800326375353, 11.09922568453594849 ) ) ;
#22571 = ORIENTED_EDGE ( 'NONE', *, *, #63228, .T. ) ;
#22572 = CARTESIAN_POINT ( 'NONE',  ( 17.20831665107776587, 47.88393115100078745, 7.208316651077764980 ) ) ;
#22573 = CARTESIAN_POINT ( 'NONE',  ( -4.164238869374099927, 67.01208216824728936, 3.795296366450308767 ) ) ;
#22574 = ORIENTED_EDGE ( 'NONE', *, *, #98608, .T. ) ;
#22575 = CARTESIAN_POINT ( 'NONE',  ( 15.44008868035555793, 21.39701867748817321, -9.422509992056140149 ) ) ;
#22576 = ORIENTED_EDGE ( 'NONE', *, *, #52334, .T. ) ;
#22577 = CARTESIAN_POINT ( 'NONE',  ( 19.42250999205614193, 55.14701867748817676, 5.440088680355555262 ) ) ;
#22578 = CARTESIAN_POINT ( 'NONE',  ( -0.8801773607111008646, 58.27201867748816966, 2.915334737309923430 ) ) ;
#22580 = EDGE_CURVE ( 'NONE', #9323, #18983, #63849, .T. ) ;
#22579 = CARTESIAN_POINT ( 'NONE',  ( 4.559911319644449179, 58.89701867748817676, 9.422509992056141925 ) ) ;
#22581 = CARTESIAN_POINT ( 'NONE',  ( 19.42250999205614193, 50.14701867748817676, 5.440088680355555262 ) ) ;
#22582 = TOROIDAL_SURFACE ( 'NONE', #84807, 14.49999999999999822, 0.5000000000000000000 ) ;
#22583 = DIRECTION ( 'NONE',  ( 0.08715574274765139351, 0.9961946980917461003, -0.000000000000000000 ) ) ;
#22584 = EDGE_CURVE ( 'NONE', #76576, #18416, #93260, .T. ) ;
#22586 = ORIENTED_EDGE ( 'NONE', *, *, #89735, .F. ) ;
#22585 = CARTESIAN_POINT ( 'NONE',  ( 10.88666287821217082, -94.01511732729316861, 4.000000000000000000 ) ) ;
#22587 = STYLED_ITEM ( 'NONE', ( #9846 ), #80415 ) ;
#22588 = CARTESIAN_POINT ( 'NONE',  ( 19.84674366389459266, 48.30059781766745175, 2.638427012816836559 ) ) ;
#22589 = VERTEX_POINT ( 'NONE', #70778 ) ;
#22590 = DIRECTION ( 'NONE',  ( 0.000000000000000000, 0.000000000000000000, -1.000000000000000000 ) ) ;
#22591 = CARTESIAN_POINT ( 'NONE',  ( -4.250000000000000000, 36.75000000000000000, -3.750000000000000000 ) ) ;
#22592 = CARTESIAN_POINT ( 'NONE',  ( 24.16423886937410614, 9.512082168247301794, -3.795296366450302550 ) ) ;
#22593 = CARTESIAN_POINT ( 'NONE',  ( -0.1503990784575321704, 8.101585745166424601, 6.262539305110068177 ) ) ;
#22594 = CARTESIAN_POINT ( 'NONE',  ( 0.5774900079438590739, 2.647018677488171434, -5.440088680355550821 ) ) ;
#22595 = CARTESIAN_POINT ( 'NONE',  ( 1.274849032794280523, 48.57228050351032067, 6.499999999999960032 ) ) ;
#22597 = ORIENTED_EDGE ( 'NONE', *, *, #5887, .F. ) ;
#22596 = CARTESIAN_POINT ( 'NONE',  ( 0.6178305044545818747, 43.49863466993042493, -9.382169495545419124 ) ) ;
#22598 = CARTESIAN_POINT ( 'NONE',  ( 10.00000000000000178, 70.00000000000000000, 0.000000000000000000 ) ) ;
#22599 = CARTESIAN_POINT ( 'NONE',  ( 14.92337183194729633, 47.67559781766745175, 8.527530157486181039 ) ) ;
#22600 = COLOUR_RGB ( '', 0.09019608, 0.27058824, 0.51372549) ;
#22601 = CARTESIAN_POINT ( 'NONE',  ( 0.1532563361054083140, 1.008931151000784787, 1.131784320476157264E-15 ) ) ;
#22602 = CARTESIAN_POINT ( 'NONE',  ( 3.591859063236761518, 14.95696800326375531, 11.09922568453594849 ) ) ;
#22603 = CARTESIAN_POINT ( 'NONE',  ( 19.84674366389459621, 23.50893115100078390, 7.409399052514197653E-17 ) ) ;
#22604 = CARTESIAN_POINT ( 'NONE',  ( 2.791683348922237240, 20.38393115100078745, -7.208316651077763204 ) ) ;
#22605 = CARTESIAN_POINT ( 'NONE',  ( 22.81628187352647785, 1.623634669930420271, 6.195893100308588602E-16 ) ) ;
#22606 = SURFACE_STYLE_FILL_AREA ( #123 ) ;
#22607 = AXIS2_PLACEMENT_3D ( 'NONE', #76795, #7335, #83319 ) ;
#22608 = EDGE_CURVE ( 'NONE', #20984, #35180, #77267, .T. ) ;
#22609 = ORIENTED_EDGE ( 'NONE', *, *, #54863, .F. ) ;
#22610 = VERTEX_POINT ( 'NONE', #55259 ) ;
#22611 = EDGE_CURVE ( 'NONE', #32046, #13614, #63246, .T. ) ;
#22612 = CARTESIAN_POINT ( 'NONE',  ( 4.559911319644449179, 18.89701867748817321, 9.422509992056141925 ) ) ;
#22613 = CARTESIAN_POINT ( 'NONE',  ( 22.26659068614894466, 13.88708216824730179, 7.082119434687054849 ) ) ;
#22614 = CARTESIAN_POINT ( 'NONE',  ( 7.361572987183170547, 27.05059781766745175, 9.846743663894590881 ) ) ;
#22615 = CARTESIAN_POINT ( 'NONE',  ( 5.076628168052704559, 5.175597817667451750, -8.527530157486179263 ) ) ;
#22616 = CIRCLE ( 'NONE', #92825, 15.00000000000000000 ) ;
#22618 = DIRECTION ( 'NONE',  ( -0.000000000000000000, -0.000000000000000000, -1.000000000000000000 ) ) ;
#22617 = CARTESIAN_POINT ( 'NONE',  ( 21.09922568453594849, 41.20696800326375353, 6.408140936763242479 ) ) ;
#22619 = CARTESIAN_POINT ( 'NONE',  ( 0.5774900079438590739, 17.64701867748817321, -5.440088680355550821 ) ) ;
#22620 = LINE ( 'NONE', #53097, #77329 ) ;
#22621 = CARTESIAN_POINT ( 'NONE',  ( 13.43411237798106583, 2.665301336597086568, -12.81628187352647252 ) ) ;
#22622 = CARTESIAN_POINT ( 'NONE',  ( 19.84674366389459266, 23.71726448433412315, -2.638427012816827677 ) ) ;
#22623 = CARTESIAN_POINT ( 'NONE',  ( 9.422509992056141925, -14.85298132251182324, 5.440088680355547268 ) ) ;
#22624 = CARTESIAN_POINT ( 'NONE',  ( 0.6178305044545838731, 39.74863466993041072, 9.382169495545420901 ) ) ;
#22625 = FILL_AREA_STYLE ('',( #60101 ) ) ;
#22626 = COLOUR_RGB ( '', 0.08235294, 0.09019608, 0.10196078) ;
#22628 = CARTESIAN_POINT ( 'NONE',  ( 13.07964015051225104, 0.2306972965111895035, -7.222261988160741275 ) ) ;
#22627 = CARTESIAN_POINT ( 'NONE',  ( 20.88017736071110164, 40.35535201082150536, 2.915334737309930979 ) ) ;
#22629 = CARTESIAN_POINT ( 'NONE',  ( -14.36383853300403501, 0.04962896932678149270, -3.367113227849129586 ) ) ;
#22630 = DIRECTION ( 'NONE',  ( -1.000000000000000000, 0.000000000000000000, 0.000000000000000000 ) ) ;
#22631 = CARTESIAN_POINT ( 'NONE',  ( 15.44008868035555260, 44.73035201082151247, 9.422509992056143702 ) ) ;
#22632 = CARTESIAN_POINT ( 'NONE',  ( -0.8801773607111008646, 38.27201867748816255, 2.915334737309923430 ) ) ;
#22633 = CARTESIAN_POINT ( 'NONE',  ( 20.03932841506541607, 60.62161441960504504, -6.397827110479004986 ) ) ;
#22634 = CARTESIAN_POINT ( 'NONE',  ( -0.8801773607111009756, 63.06368534415484106, 1.068504757029289695E-15 ) ) ;
#22635 = CARTESIAN_POINT ( 'NONE',  ( 1.472469842513823179, 55.59226448433412315, -4.923371831947296329 ) ) ;
#22637 = FACE_OUTER_BOUND ( 'NONE', #53774, .T. ) ;
#22636 = CARTESIAN_POINT ( 'NONE',  ( -0.8801773607110991993, 7.855352010821504471, -2.915334737309923874 ) ) ;
#22638 = CARTESIAN_POINT ( 'NONE',  ( 22.81628187352648496, 6.831968003263753531, -3.434112377981050290 ) ) ;
#22639 = ORIENTED_EDGE ( 'NONE', *, *, #17049, .F. ) ;
#22640 = CARTESIAN_POINT ( 'NONE',  ( 7.084665262690076126, 44.10535201082151247, 10.88017736071109987 ) ) ;
#22642 = CARTESIAN_POINT ( 'NONE',  ( 18.95785429995052596, 7.242161081720063009, 6.499999999999870326 ) ) ;
#22641 = CARTESIAN_POINT ( 'NONE',  ( 10.00000000000000178, 67.25893115100079456, 9.846743663894594434 ) ) ;
#22643 = ADVANCED_FACE ( 'NONE', ( #8778 ), #20837, .F. ) ;
#22644 = CARTESIAN_POINT ( 'NONE',  ( 7.084665262690076126, 29.10535201082150181, 10.88017736071109987 ) ) ;
#22645 = CARTESIAN_POINT ( 'NONE',  ( 0.1532563361054082862, 16.21726448433411960, 2.638427012816831674 ) ) ;
#22646 = CARTESIAN_POINT ( 'NONE',  ( 22.26659068614894466, 33.88708216824730357, 7.082119434687054849 ) ) ;
#22647 = CARTESIAN_POINT ( 'NONE',  ( 5.076628168052703671, 26.84226448433411960, 8.527530157486179263 ) ) ;
#22648 = CARTESIAN_POINT ( 'NONE',  ( 20.88017736071110519, 40.56368534415484106, 2.639326808657452039E-16 ) ) ;
#22649 = CARTESIAN_POINT ( 'NONE',  ( -0.1038446121089033197, 34.24302437010793909, -6.337995344473782211 ) ) ;
#22650 = CARTESIAN_POINT ( 'NONE',  ( 24.16423886937410614, 9.303748834913967869, 8.672049930838204340E-16 ) ) ;
#22651 = STYLED_ITEM ( 'NONE', ( #49761 ), #39648 ) ;
#22652 = B_SPLINE_CURVE_WITH_KNOTS ( 'NONE', 3,
 ( #67013, #97534, #83500, #60491 ),
 .UNSPECIFIED., .F., .F.,
 ( 4, 4 ),
 ( 2.478060227011367563E-17, 0.002392975128318452962 ),
 .UNSPECIFIED. ) ;
#22653 = DIRECTION ( 'NONE',  ( 0.000000000000000000, 0.000000000000000000, 1.000000000000000000 ) ) ;
#22654 = CARTESIAN_POINT ( 'NONE',  ( 12.63842701281683922, 54.55059781766745175, -9.846743663894590881 ) ) ;
#22655 = ORIENTED_EDGE ( 'NONE', *, *, #41779, .T. ) ;
#22656 = EDGE_LOOP ( 'NONE', ( #25323, #92039, #66649, #53288, #43791, #62256, #50079, #38554 ) ) ;
#22657 = AXIS2_PLACEMENT_3D ( 'NONE', #39847, #94804, #21280 ) ;
#22658 = CARTESIAN_POINT ( 'NONE',  ( 2.917880565312950480, 25.97041550158063572, -12.26659068614894821 ) ) ;
#22659 = CARTESIAN_POINT ( 'NONE',  ( 2.917880565312950480, 25.97041550158063572, -12.26659068614894821 ) ) ;
#22660 = CARTESIAN_POINT ( 'NONE',  ( 10.00000000000000000, 9.758931151000785675, -9.846743663894594434 ) ) ;
#22661 = CARTESIAN_POINT ( 'NONE',  ( 24.16423886937409904, 64.09541550158064638, 3.795296366450317205 ) ) ;
#22662 = CARTESIAN_POINT ( 'NONE',  ( 0.6178305044545838731, 9.748634669930416052, 9.382169495545420901 ) ) ;
#22663 = CARTESIAN_POINT ( 'NONE',  ( 14.92337183194729633, 52.67559781766745175, 8.527530157486181039 ) ) ;
#22664 = CARTESIAN_POINT ( 'NONE',  ( -10.54702889487960071, -44.61188042012589960, 4.000000000000000000 ) ) ;
#22666 = CARTESIAN_POINT ( 'NONE',  ( 21.09922568453595559, 17.04030133659708923, -6.408140936763230044 ) ) ;
#22665 = CARTESIAN_POINT ( 'NONE',  ( 17.96484262340118221, 39.93868534415484106, 7.964842623401181321 ) ) ;
#22667 = CARTESIAN_POINT ( 'NONE',  ( -4.164238869374098151, 11.59541550158063217, -3.795296366450310543 ) ) ;
#22668 = CARTESIAN_POINT ( 'NONE',  ( 0.5774900079438590739, 12.64701867748817321, -5.440088680355550821 ) ) ;
#22669 = CARTESIAN_POINT ( 'NONE',  ( 2.035157376598822676, 27.43868534415483396, -7.964842623401177768 ) ) ;
#22670 = CARTESIAN_POINT ( 'NONE',  ( -0.8801773607111009756, 53.06368534415484106, 1.068504757029289695E-15 ) ) ;
#22671 = CARTESIAN_POINT ( 'NONE',  ( 16.40814093676323893, 50.79030133659708923, 11.09922568453595026 ) ) ;
#22672 = CARTESIAN_POINT ( 'NONE',  ( 9.846743663894594434, -21.49106884899921255, -2.168404344971008868E-15 ) ) ;
#22673 = ORIENTED_EDGE ( 'NONE', *, *, #1785, .T. ) ;
#22674 = CARTESIAN_POINT ( 'NONE',  ( 20.04068437667225311, 34.71974360917721469, 6.396802510829709298 ) ) ;
#22675 = DIRECTION ( 'NONE',  ( 0.000000000000000000, -1.000000000000000000, 0.000000000000000000 ) ) ;
#22676 = ORIENTED_EDGE ( 'NONE', *, *, #87309, .T. ) ;
#22677 = CARTESIAN_POINT ( 'NONE',  ( 0.1955144967548954060, 19.32703681773340421, -6.500000000002791545 ) ) ;
#22679 = CARTESIAN_POINT ( 'NONE',  ( 10.00000000000000178, 68.05374883491397497, 14.16423886937410082 ) ) ;
#22678 = CARTESIAN_POINT ( 'NONE',  ( 24.16423886937410614, 59.51208216824728936, -3.795296366450302550 ) ) ;
#22681 = CARTESIAN_POINT ( 'NONE',  ( 2.791683348922237240, 55.38393115100078745, -7.208316651077763204 ) ) ;
#22680 = CARTESIAN_POINT ( 'NONE',  ( 5.076628168052703671, 21.84226448433411960, 8.527530157486179263 ) ) ;
#22682 = CARTESIAN_POINT ( 'NONE',  ( 14.49999999999999822, 60.50000000000000711, -6.000000000000000000 ) ) ;
#22683 = CARTESIAN_POINT ( 'NONE',  ( 20.15039907845753220, 44.72266099184918176, 6.262539305110078836 ) ) ;
#22684 = CARTESIAN_POINT ( 'NONE',  ( 14.92337183194729988, 9.342264484334119601, -8.527530157486177487 ) ) ;
#22685 = VECTOR ( 'NONE', #39106, 1000.000000000000000 ) ;
#22686 =( GEOMETRIC_REPRESENTATION_CONTEXT ( 3 ) GLOBAL_UNCERTAINTY_ASSIGNED_CONTEXT ( ( #98150 ) ) GLOBAL_UNIT_ASSIGNED_CONTEXT ( ( #7931, #53913, #91909 ) ) REPRESENTATION_CONTEXT ( 'NONE', 'WORKASPACE' ) );
#22687 = CARTESIAN_POINT ( 'NONE',  ( 9.382169495545415572, 22.24863466993043204, -9.382169495545422677 ) ) ;
#22688 = ORIENTED_EDGE ( 'NONE', *, *, #94306, .T. ) ;
#22689 = PRESENTATION_LAYER_ASSIGNMENT (  '', '', ( #70570 ) ) ;
#22690 = CARTESIAN_POINT ( 'NONE',  ( 13.79529636645031943, 30.34541550158063927, -14.16423886937409904 ) ) ;
#22691 = CARTESIAN_POINT ( 'NONE',  ( 10.00000000000000178, 48.05374883491396787, 14.16423886937410082 ) ) ;
#22692 = ORIENTED_EDGE ( 'NONE', *, *, #76212, .T. ) ;
#22693 = CARTESIAN_POINT ( 'NONE',  ( -1.099225684535947600, 63.70696800326376774, -6.408140936763238038 ) ) ;
#22694 = CARTESIAN_POINT ( 'NONE',  ( 19.42250999205614548, 25.98035201082150891, -5.440088680355545492 ) ) ;
#22695 = CARTESIAN_POINT ( 'NONE',  ( 1.472469842513823179, 56.42559781766745886, 4.923371831947296329 ) ) ;
#22696 = CARTESIAN_POINT ( 'NONE',  ( 17.96484262340118221, 19.93868534415484106, 7.964842623401181321 ) ) ;
#22697 = STYLED_ITEM ( 'NONE', ( #66601 ), #74641 ) ;
#22698 = CARTESIAN_POINT ( 'NONE',  ( 6.382347221874423937, 15.00000000000000000, -13.57444820018227638 ) ) ;
#22699 = CARTESIAN_POINT ( 'NONE',  ( 0.9082943533636174127, 4.777657996272472852E-16, 14.47152380945585648 ) ) ;
#22700 = CARTESIAN_POINT ( 'NONE',  ( 5.076628168052704559, 55.17559781766745175, -8.527530157486179263 ) ) ;
#22701 = CARTESIAN_POINT ( 'NONE',  ( 14.92337183194729988, 44.34226448433412315, -8.527530157486177487 ) ) ;
#22702 = EDGE_CURVE ( 'NONE', #71617, #9146, #35158, .T. ) ;
#22703 = DIRECTION ( 'NONE',  ( 0.000000000000000000, 1.000000000000000000, 0.000000000000000000 ) ) ;
#22704 = CARTESIAN_POINT ( 'NONE',  ( -3.420591144908668557, 14.63606885998604490, 14.60477854057957003 ) ) ;
#22705 = CARTESIAN_POINT ( 'NONE',  ( 18.52753015748617571, 8.092264484334117824, 4.923371831947298993 ) ) ;
#22706 = VERTEX_POINT ( 'NONE', #47259 ) ;
#22707 = CYLINDRICAL_SURFACE ( 'NONE', #36597, 19.99999999999999645 ) ;
#22708 = CARTESIAN_POINT ( 'NONE',  ( 7.361572987183169658, 34.96726448433411605, -9.846743663894592657 ) ) ;
#22709 = LINE ( 'NONE', #69674, #21316 ) ;
#22710 = CARTESIAN_POINT ( 'NONE',  ( 16.40814093676323893, 40.79030133659708923, 11.09922568453595026 ) ) ;
#22711 = FACE_OUTER_BOUND ( 'NONE', #45134, .T. ) ;
#22712 = DIRECTION ( 'NONE',  ( -0.000000000000000000, -1.000000000000000000, -0.000000000000000000 ) ) ;
#22713 = DIRECTION ( 'NONE',  ( 0.000000000000000000, 0.000000000000000000, 1.000000000000000000 ) ) ;
#22714 = CARTESIAN_POINT ( 'NONE',  ( 10.00000000000000178, 42.25893115100078745, 9.846743663894594434 ) ) ;
#22715 = CARTESIAN_POINT ( 'NONE',  ( 24.16423886937410614, 29.30374883491396787, 8.672049930838204340E-16 ) ) ;
#22716 = CARTESIAN_POINT ( 'NONE',  ( 0.1532563361054082862, 46.21726448433411605, 2.638427012816831674 ) ) ;
#22717 = DIRECTION ( 'NONE',  ( 0.9953961983671778535, 0.000000000000000000, 0.09584575252023383451 ) ) ;
#22718 = CARTESIAN_POINT ( 'NONE',  ( 1.472469842513823179, 5.592264484334118713, -4.923371831947296329 ) ) ;
#22719 = PRESENTATION_STYLE_ASSIGNMENT (( #31180 ) ) ;
#22720 = CARTESIAN_POINT ( 'NONE',  ( 14.92337183194729988, 49.34226448433411605, -8.527530157486177487 ) ) ;
#22721 = CARTESIAN_POINT ( 'NONE',  ( 2.035157376598822676, 52.43868534415483396, -7.964842623401177768 ) ) ;
#22722 = CARTESIAN_POINT ( 'NONE',  ( 18.52753015748617571, 38.09226448433412315, 4.923371831947298993 ) ) ;
#22723 = DIRECTION ( 'NONE',  ( 0.3987490689252466414, 0.000000000000000000, 0.9170600743851238246 ) ) ;
#22724 = AXIS2_PLACEMENT_3D ( 'NONE', #18726, #41242, #39756 ) ;
#22725 = EDGE_CURVE ( 'NONE', #13373, #91555, #55689, .T. ) ;
#22726 = CARTESIAN_POINT ( 'NONE',  ( -0.8801773607111009756, 48.06368534415484817, 1.068504757029289695E-15 ) ) ;
#22727 = EDGE_LOOP ( 'NONE', ( #48673, #52691, #63192, #5836, #58292 ) ) ;
#22728 = EDGE_CURVE ( 'NONE', #37192, #5083, #101, .T. ) ;
#22729 = CARTESIAN_POINT ( 'NONE',  ( 6.715867195167361636, 4.143177415744058416E-16, 12.85095824508331930 ) ) ;
#22730 = CARTESIAN_POINT ( 'NONE',  ( 12.91533473730992121, 29.52201867748817321, 10.88017736071110164 ) ) ;
#22732 = CARTESIAN_POINT ( 'NONE',  ( 12.91533473730993009, 46.60535201082150536, -10.88017736071109987 ) ) ;
#22731 = CARTESIAN_POINT ( 'NONE',  ( 0.6178305044545818747, -1.501365330069579951, -9.382169495545419124 ) ) ;
#22733 = LINE ( 'NONE', #51743, #90337 ) ;
#22734 = CARTESIAN_POINT ( 'NONE',  ( 20.03932841506542673, 10.62161441960501307, -6.397827110478957913 ) ) ;
#22735 = CARTESIAN_POINT ( 'NONE',  ( 18.72515096720568195, 21.07228050351032422, -6.500000000000018652 ) ) ;
#22737 = CARTESIAN_POINT ( 'NONE',  ( 20.00000000000000711, 96.99160806218867492, -4.500000000000000888 ) ) ;
#22736 = CARTESIAN_POINT ( 'NONE',  ( -0.8801773607111008646, 38.27201867748816255, 2.915334737309923430 ) ) ;
#22738 = CARTESIAN_POINT ( 'NONE',  ( 14.92337183194729988, 14.34226448433411782, -8.527530157486177487 ) ) ;
#22739 = CARTESIAN_POINT ( 'NONE',  ( 10.00000000000000178, 37.25893115100078745, 9.846743663894594434 ) ) ;
#22740 = CARTESIAN_POINT ( 'NONE',  ( 20.10239578412224404, 57.63377557478296609, -6.340343622311915617 ) ) ;
#22741 = CARTESIAN_POINT ( 'NONE',  ( 3.469446951953614189E-15, 18.05374883491397853, 14.16423886937410259 ) ) ;
#22742 = CARTESIAN_POINT ( 'NONE',  ( 17.20831665107776587, 62.88393115100078745, 7.208316651077764980 ) ) ;
#22743 = CARTESIAN_POINT ( 'NONE',  ( 20.36894250292379738, 64.92874883491397497, -10.36894250292379027 ) ) ;
#22744 = DIRECTION ( 'NONE',  ( -0.02177529129954165754, -0.9997628902338895340, -2.778676860659971196E-13 ) ) ;
#22745 = CARTESIAN_POINT ( 'NONE',  ( -4.164238869374098151, 21.59541550158063217, -3.795296366450310543 ) ) ;
#22746 = CARTESIAN_POINT ( 'NONE',  ( 20.36894250292379738, 49.92874883491396787, -10.36894250292379027 ) ) ;
#22747 = CARTESIAN_POINT ( 'NONE',  ( 0.1532563361054083140, 16.00893115100078390, 1.131784320476157264E-15 ) ) ;
#22748 = ORIENTED_EDGE ( 'NONE', *, *, #97611, .T. ) ;
#22749 = CARTESIAN_POINT ( 'NONE',  ( 0.1532563361054100626, 20.80059781766744464, -2.638427012816831230 ) ) ;
#22750 = CARTESIAN_POINT ( 'NONE',  ( 12.91533473730993009, 26.60535201082150536, -10.88017736071109987 ) ) ;
#22751 = CARTESIAN_POINT ( 'NONE',  ( 7.361572987183169658, 54.96726448433413026, -9.846743663894592657 ) ) ;
#22753 = FILL_AREA_STYLE_COLOUR ( '', #59928 ) ;
#22752 = CARTESIAN_POINT ( 'NONE',  ( -4.164238869374099927, 12.01208216824730357, 3.795296366450308767 ) ) ;
#22754 = DIRECTION ( 'NONE',  ( 0.08715574274765139351, 0.9961946980917461003, 0.000000000000000000 ) ) ;
#22755 = VECTOR ( 'NONE', #88601, 999.9999999999998863 ) ;
#22756 = CARTESIAN_POINT ( 'NONE',  ( 10.00000000000000178, 12.25893115100078568, 9.846743663894594434 ) ) ;
#22757 = CARTESIAN_POINT ( 'NONE',  ( 0.6178305044545818747, 33.49863466993042493, -9.382169495545419124 ) ) ;
#22758 = CARTESIAN_POINT ( 'NONE',  ( 19.84674366389459621, 38.50893115100078745, 7.409399052514197653E-17 ) ) ;
#22759 = ORIENTED_EDGE ( 'NONE', *, *, #56214, .T. ) ;
#22760 = CARTESIAN_POINT ( 'NONE',  ( 1.472469842513823179, 26.42559781766745175, 4.923371831947296329 ) ) ;
#22761 = VECTOR ( 'NONE', #93601, 1000.000000000000000 ) ;
#22762 = CARTESIAN_POINT ( 'NONE',  ( 11.15633344613943123, -69.21805206906502406, -4.000000000000000000 ) ) ;
#22763 = DIRECTION ( 'NONE',  ( 0.000000000000000000, 1.000000000000000000, 0.000000000000000000 ) ) ;
#22764 = CARTESIAN_POINT ( 'NONE',  ( -2.266590686148945544, 56.38708216824731068, -7.082119434687050408 ) ) ;
#22765 = CARTESIAN_POINT ( 'NONE',  ( 19.42250999205614548, 45.98035201082150536, -5.440088680355545492 ) ) ;
#22766 = SURFACE_SIDE_STYLE ('',( #56086 ) ) ;
#22767 = CARTESIAN_POINT ( 'NONE',  ( 7.361572987183169658, 39.96726448433411605, -9.846743663894592657 ) ) ;
#22768 = CARTESIAN_POINT ( 'NONE',  ( -0.8801773607111008646, 13.27201867748817143, 2.915334737309923430 ) ) ;
#22769 = CARTESIAN_POINT ( 'NONE',  ( 10.00000000000000000, 39.75893115100078745, -9.846743663894594434 ) ) ;
#22770 = VECTOR ( 'NONE', #7985, 1000.000000000000000 ) ;
#22771 = DIRECTION ( 'NONE',  ( 4.263256414560601746E-14, 0.000000000000000000, 1.000000000000000000 ) ) ;
#22772 = CARTESIAN_POINT ( 'NONE',  ( 0.1532563361054083140, 51.00893115100078745, 1.131784320476157264E-15 ) ) ;
#22773 = B_SPLINE_CURVE_WITH_KNOTS ( 'NONE', 3,
 ( #3776, #34731, #65222, #95749 ),
 .UNSPECIFIED., .F., .F.,
 ( 4, 4 ),
 ( 6.254634441385501517E-18, 0.002392975128318428676 ),
 .UNSPECIFIED. ) ;
#22774 = EDGE_CURVE ( 'NONE', #69260, #83143, #38795, .T. ) ;
#22775 = CARTESIAN_POINT ( 'NONE',  ( 10.00000000000000178, 54.31368534415484106, 10.88017736071110342 ) ) ;
#22776 = VERTEX_POINT ( 'NONE', #39784 ) ;
#22777 = ORIENTED_EDGE ( 'NONE', *, *, #45451, .T. ) ;
#22778 = CARTESIAN_POINT ( 'NONE',  ( -2.816281873526473856, 54.12363466993041783, 9.499525473075851096E-16 ) ) ;
#22779 = DIRECTION ( 'NONE',  ( -0.9981347984218665870, 0.000000000000000000, -0.06104853953486361756 ) ) ;
#22780 = CARTESIAN_POINT ( 'NONE',  ( 18.52753015748617571, 13.09226448433411960, 4.923371831947298993 ) ) ;
#22781 = CARTESIAN_POINT ( 'NONE',  ( -2.816281873526471635, 58.91530133659707502, -3.434112377981056508 ) ) ;
#22783 = CARTESIAN_POINT ( 'NONE',  ( 18.52753015748618282, 48.92559781766745886, -4.923371831947291888 ) ) ;
#22782 = CARTESIAN_POINT ( 'NONE',  ( 10.00000000000000178, 9.313685344154839285, 10.88017736071110342 ) ) ;
#22784 = CARTESIAN_POINT ( 'NONE',  ( 20.00000000000000355, 95.40264689492315142, 4.636598376030806712 ) ) ;
#22785 = CARTESIAN_POINT ( 'NONE',  ( 0.1532563361054082862, 1.217264484334117824, 2.638427012816831674 ) ) ;
#22786 = CARTESIAN_POINT ( 'NONE',  ( 10.00000000000000000, 25.55374883491396787, -14.16423886937410082 ) ) ;
#22787 = CARTESIAN_POINT ( 'NONE',  ( 24.16423886937410614, 44.30374883491397497, 8.672049930838204340E-16 ) ) ;
#22788 = CARTESIAN_POINT ( 'NONE',  ( 18.52753015748618282, 58.92559781766745886, -4.923371831947291888 ) ) ;
#22789 = FACE_OUTER_BOUND ( 'NONE', #51953, .T. ) ;
#22790 = CARTESIAN_POINT ( 'NONE',  ( -0.8801773607110991993, 47.85535201082150536, -2.915334737309923874 ) ) ;
#22791 = CARTESIAN_POINT ( 'NONE',  ( 2.791683348922240793, 1.633931151000784565, 7.208316651077764092 ) ) ;
#22792 = CIRCLE ( 'NONE', #69099, 0.5000000000000004441 ) ;
#22793 = ORIENTED_EDGE ( 'NONE', *, *, #66846, .F. ) ;
#22794 = CARTESIAN_POINT ( 'NONE',  ( 21.09922568453594849, 61.20696800326376064, 6.408140936763242479 ) ) ;
#22795 = CARTESIAN_POINT ( 'NONE',  ( 10.00000000000000000, 4.758931151000784787, -9.846743663894594434 ) ) ;
#22796 = ORIENTED_EDGE ( 'NONE', *, *, #89716, .T. ) ;
#22797 = CARTESIAN_POINT ( 'NONE',  ( 22.26659068614895176, 14.72041550158063572, -7.082119434687042414 ) ) ;
#22798 = CARTESIAN_POINT ( 'NONE',  ( 5.076628168052704559, 15.17559781766745175, -8.527530157486179263 ) ) ;
#22799 = CARTESIAN_POINT ( 'NONE',  ( 12.91533473730992121, 34.52201867748817676, 10.88017736071110164 ) ) ;
#22800 = DIRECTION ( 'NONE',  ( 3.730349362740525976E-14, 0.000000000000000000, 1.000000000000000000 ) ) ;
#22801 = ORIENTED_EDGE ( 'NONE', *, *, #47541, .T. ) ;
#22802 = CARTESIAN_POINT ( 'NONE',  ( 20.88017736071110164, 25.35535201082150891, 2.915334737309930979 ) ) ;
#22803 = VECTOR ( 'NONE', #7450, 1000.000000000000000 ) ;
#22804 = ORIENTED_EDGE ( 'NONE', *, *, #4631, .T. ) ;
#22805 = CARTESIAN_POINT ( 'NONE',  ( 15.44008868035555793, 36.39701867748816966, -9.422509992056140149 ) ) ;
#22806 = DIRECTION ( 'NONE',  ( 0.000000000000000000, 0.000000000000000000, 1.000000000000000000 ) ) ;
#22807 = ORIENTED_EDGE ( 'NONE', *, *, #87764, .T. ) ;
#22808 = ORIENTED_EDGE ( 'NONE', *, *, #704, .F. ) ;
#22809 = CARTESIAN_POINT ( 'NONE',  ( -2.816281873526473856, 19.12363466993042138, 9.499525473075851096E-16 ) ) ;
#22810 = CARTESIAN_POINT ( 'NONE',  ( 17.20831665107776587, 14.13393115100078568, -7.208316651077762316 ) ) ;
#22811 = CARTESIAN_POINT ( 'NONE',  ( 9.159723438033129383, 15.00000000000000000, 10.91613331444548507 ) ) ;
#22812 = CARTESIAN_POINT ( 'NONE',  ( 5.076628168052703671, 16.84226448433411960, 8.527530157486179263 ) ) ;
#22813 = CARTESIAN_POINT ( 'NONE',  ( 10.00000000000000000, 31.81368534415483751, -10.88017736071110342 ) ) ;
#22814 = EDGE_CURVE ( 'NONE', #8560, #33923, #25285, .T. ) ;
#22815 = AXIS2_PLACEMENT_3D ( 'NONE', #51402, #60372, #44388 ) ;
#22816 = ORIENTED_EDGE ( 'NONE', *, *, #60765, .T. ) ;
#22817 = CARTESIAN_POINT ( 'NONE',  ( 6.565887622018943937, 65.16530133659709634, 12.81628187352647430 ) ) ;
#22818 = CARTESIAN_POINT ( 'NONE',  ( 7.084665262690076126, 44.10535201082151247, 10.88017736071109987 ) ) ;
#22819 = CARTESIAN_POINT ( 'NONE',  ( -0.2418659066527499291, 22.23410085661203794, -6.114288769123083611 ) ) ;
#22820 = AXIS2_PLACEMENT_3D ( 'NONE', #51619, #14622, #43610 ) ;
#22821 = CARTESIAN_POINT ( 'NONE',  ( -2.816281873526473856, 54.12363466993041783, 9.499525473075851096E-16 ) ) ;
#22822 = CARTESIAN_POINT ( 'NONE',  ( 7.084665262690076126, 57.02201867748817676, -10.88017736071110164 ) ) ;
#22823 = AXIS2_PLACEMENT_3D ( 'NONE', #36723, #30674, #68211 ) ;
#22824 = PRESENTATION_LAYER_ASSIGNMENT (  '', '', ( #19596 ) ) ;
#22825 = CARTESIAN_POINT ( 'NONE',  ( -2.816281873526473856, -0.6680319967362464695, 3.434112377981055619 ) ) ;
#22827 = FILL_AREA_STYLE ('',( #53303 ) ) ;
#22826 = COLOUR_RGB ( '', 0.09019608, 0.27058824, 0.51372549) ;
#22828 = CARTESIAN_POINT ( 'NONE',  ( 7.361572987183169658, 34.96726448433411605, -9.846743663894592657 ) ) ;
#22829 = CARTESIAN_POINT ( 'NONE',  ( -2.816281873526473856, 54.12363466993041783, 9.499525473075851096E-16 ) ) ;
#22830 = LINE ( 'NONE', #61787, #70498 ) ;
#22831 = CARTESIAN_POINT ( 'NONE',  ( 7.361572987183170547, 2.050597817667451750, 9.846743663894590881 ) ) ;
#22832 = AXIS2_PLACEMENT_3D ( 'NONE', #35762, #35262, #66757 ) ;
#22833 = CARTESIAN_POINT ( 'NONE',  ( -2.816281873526473856, 14.12363466993041961, 9.499525473075851096E-16 ) ) ;
#22835 = CARTESIAN_POINT ( 'NONE',  ( -7.595945211628163385, 15.00000000000000000, -12.35117874301652030 ) ) ;
#22834 = FACE_OUTER_BOUND ( 'NONE', #39284, .T. ) ;
#22836 = CARTESIAN_POINT ( 'NONE',  ( 20.88017736071110519, 35.56368534415484106, 2.639326808657452039E-16 ) ) ;
#22837 = CARTESIAN_POINT ( 'NONE',  ( 19.84674366389459621, 63.50893115100078745, 7.409399052514197653E-17 ) ) ;
#22838 = CARTESIAN_POINT ( 'NONE',  ( 0.000000000000000000, 0.000000000000000000, 0.000000000000000000 ) ) ;
#22839 = CARTESIAN_POINT ( 'NONE',  ( 14.92337183194729633, 17.67559781766745175, 8.527530157486181039 ) ) ;
#22840 = CARTESIAN_POINT ( 'NONE',  ( 12.63842701281683922, 9.550597817667449974, -9.846743663894590881 ) ) ;
#22842 = ORIENTED_EDGE ( 'NONE', *, *, #79791, .T. ) ;
#22841 = CARTESIAN_POINT ( 'NONE',  ( -2.816281873526473856, 19.12363466993042138, 9.499525473075851096E-16 ) ) ;
#22843 = CARTESIAN_POINT ( 'NONE',  ( -0.8801773607111009756, 3.063685344154837509, 1.068504757029289695E-15 ) ) ;
#22844 = CARTESIAN_POINT ( 'NONE',  ( 10.00000000000000000, 59.75893115100078745, -9.846743663894594434 ) ) ;
#22845 = ADVANCED_FACE ( 'NONE', ( #86260 ), #47761, .F. ) ;
#22846 = CARTESIAN_POINT ( 'NONE',  ( 6.933985542754713904, -73.15302115696529484, -2.499999999998392397 ) ) ;
#22847 = CARTESIAN_POINT ( 'NONE',  ( 12.91533473730992121, 9.522018677488171434, 10.88017736071110164 ) ) ;
#22848 = CARTESIAN_POINT ( 'NONE',  ( 10.00000000000000000, 39.75893115100078745, -9.846743663894594434 ) ) ;
#22849 = CARTESIAN_POINT ( 'NONE',  ( 0.9940297508537879745, -0.03417435944610275333, -14.21528771620249820 ) ) ;
#22850 = ADVANCED_FACE ( 'NONE', ( #81212 ), #64222, .F. ) ;
#22851 = CARTESIAN_POINT ( 'NONE',  ( 7.084665262690076126, 9.105352010821503583, 10.88017736071109987 ) ) ;
#22852 = CARTESIAN_POINT ( 'NONE',  ( 19.72487221294570858, 69.50000000000000000, -6.500000000000000888 ) ) ;
#22853 = CARTESIAN_POINT ( 'NONE',  ( 17.96484262340118221, 31.18868534415483751, -7.964842623401177768 ) ) ;
#22854 = VECTOR ( 'NONE', #89429, 1000.000000000000000 ) ;
#22856 = CYLINDRICAL_SURFACE ( 'NONE', #79802, 3.000000000000002665 ) ;
#22855 = CARTESIAN_POINT ( 'NONE',  ( 22.26659068614895176, 59.72041550158063927, -7.082119434687042414 ) ) ;
#22857 = CARTESIAN_POINT ( 'NONE',  ( 14.92337183194729988, 4.342264484334117824, -8.527530157486177487 ) ) ;
#22858 = CARTESIAN_POINT ( 'NONE',  ( 0.1532563361054100626, 20.80059781766744464, -2.638427012816831230 ) ) ;
#22859 = CARTESIAN_POINT ( 'NONE',  ( -1.099225684535947600, 14.54030133659708568, 6.408140936763237150 ) ) ;
#22860 = DIRECTION ( 'NONE',  ( -5.818595309480553908E-17, -1.000000000000000000, -0.000000000000000000 ) ) ;
#22861 = CARTESIAN_POINT ( 'NONE',  ( -0.3077640640441539621, 70.00000000000000000, 5.999999999999999112 ) ) ;
#22862 = AXIS2_PLACEMENT_3D ( 'NONE', #1978, #16969, #23498 ) ;
#22863 = CARTESIAN_POINT ( 'NONE',  ( 19.84674366389459621, 58.50893115100078745, 7.409399052514197653E-17 ) ) ;
#22864 = CARTESIAN_POINT ( 'NONE',  ( -18.89999999999999147, 99.99999999999998579, -7.750000000000000000 ) ) ;
#22865 = CARTESIAN_POINT ( 'NONE',  ( -11.05192081855196662, -57.06859629173521853, -4.000000000000000000 ) ) ;
#22866 = CARTESIAN_POINT ( 'NONE',  ( 10.00000000000000000, 15.55374883491396787, -14.16423886937410082 ) ) ;
#22867 = AXIS2_PLACEMENT_3D ( 'NONE', #27220, #20725, #66205 ) ;
#22868 = CARTESIAN_POINT ( 'NONE',  ( 19.84674366389459266, 23.71726448433412315, -2.638427012816827677 ) ) ;
#22869 = DIRECTION ( 'NONE',  ( 0.000000000000000000, 0.000000000000000000, 1.000000000000000000 ) ) ;
#22870 = ORIENTED_EDGE ( 'NONE', *, *, #8291, .F. ) ;
#22871 = CARTESIAN_POINT ( 'NONE',  ( 24.16423886937410614, 59.51208216824728936, -3.795296366450302550 ) ) ;
#22872 = CARTESIAN_POINT ( 'NONE',  ( 7.361572987183170547, 7.050597817667451750, 9.846743663894590881 ) ) ;
#22874 = CARTESIAN_POINT ( 'NONE',  ( -13.34343830728397329, 14.63606867472037720, -6.852200678592815564 ) ) ;
#22873 = LINE ( 'NONE', #16839, #45155 ) ;
#22875 = CARTESIAN_POINT ( 'NONE',  ( 12.91533473730992121, 34.52201867748817676, 10.88017736071110164 ) ) ;
#22876 = CARTESIAN_POINT ( 'NONE',  ( 0.6178305044545838731, 49.74863466993041072, 9.382169495545420901 ) ) ;
#22877 = CARTESIAN_POINT ( 'NONE',  ( 0.5774900079438607392, 8.480352010821505360, 5.440088680355550821 ) ) ;
#22878 = CARTESIAN_POINT ( 'NONE',  ( 19.38216949554541557, 32.24863466993041783, -9.382169495545420901 ) ) ;
#22879 = CARTESIAN_POINT ( 'NONE',  ( 13.43411237798105340, 0.5819680032637533085, 12.81628187352647963 ) ) ;
#22880 = CARTESIAN_POINT ( 'NONE',  ( 18.52753015748617571, 8.092264484334117824, 4.923371831947298993 ) ) ;
#22881 = ORIENTED_EDGE ( 'NONE', *, *, #23455, .T. ) ;
#22882 = CARTESIAN_POINT ( 'NONE',  ( -15.00000000000004974, 91.00000000000000000, 4.000000000000000000 ) ) ;
#22883 = CARTESIAN_POINT ( 'NONE',  ( -7.858204384948651366, -3.138042374739517193, -4.000000000000000000 ) ) ;
#22884 = CARTESIAN_POINT ( 'NONE',  ( -4.164238869374099927, 42.01208216824728936, 3.795296366450308767 ) ) ;
#22885 = CARTESIAN_POINT ( 'NONE',  ( 6.204703633549690345, 17.84541550158063217, 14.16423886937410082 ) ) ;
#22886 = CARTESIAN_POINT ( 'NONE',  ( 20.88017736071110875, 5.772018677488170546, -2.915334737309920765 ) ) ;
#22887 = CARTESIAN_POINT ( 'NONE',  ( 17.96484262340118221, 31.18868534415483751, -7.964842623401177768 ) ) ;
#22888 = DIRECTION ( 'NONE',  ( 0.06975647374412534407, 0.9975640502598241977, -0.000000000000000000 ) ) ;
#22889 = CARTESIAN_POINT ( 'NONE',  ( 14.48718990079892599, 4.585916678612670543E-16, -0.6093675230840440715 ) ) ;
#22890 = CARTESIAN_POINT ( 'NONE',  ( -0.8801773607110991993, 62.85535201082150536, -2.915334737309923874 ) ) ;
#22891 = LINE ( 'NONE', #76370, #51330 ) ;
#22892 = CARTESIAN_POINT ( 'NONE',  ( 16.40814093676323893, 25.79030133659708923, 11.09922568453595026 ) ) ;
#22893 = DIRECTION ( 'NONE',  ( 1.000000000000000000, 0.000000000000000000, -0.000000000000000000 ) ) ;
#22894 = CARTESIAN_POINT ( 'NONE',  ( 5.795997163830076460, -0.03417435944610275333, 13.01802277140709663 ) ) ;
#22895 = CARTESIAN_POINT ( 'NONE',  ( 17.20831665107776587, 34.13393115100078745, -7.208316651077762316 ) ) ;
#22896 = ADVANCED_FACE ( 'NONE', ( #72707 ), #11256, .T. ) ;
#22897 = CARTESIAN_POINT ( 'NONE',  ( 6.565887622018943937, 20.16530133659708213, 12.81628187352647430 ) ) ;
#22898 = CARTESIAN_POINT ( 'NONE',  ( 12.63842701281683922, 14.55059781766744997, -9.846743663894590881 ) ) ;
#22899 = CARTESIAN_POINT ( 'NONE',  ( 19.42250999205614548, 5.980352010821504471, -5.440088680355545492 ) ) ;
#22900 = CARTESIAN_POINT ( 'NONE',  ( 18.52753015748618282, 33.92559781766745886, -4.923371831947291888 ) ) ;
#22901 = CARTESIAN_POINT ( 'NONE',  ( 8.879999999999999005, 20.99999999999999645, 1.249999999999987121 ) ) ;
#22902 = AXIS2_PLACEMENT_3D ( 'NONE', #57113, #11618, #79133 ) ;
#22904 = CARTESIAN_POINT ( 'NONE',  ( 2.917880565312950480, 0.9704155015806342766, -12.26659068614894821 ) ) ;
#22903 = CARTESIAN_POINT ( 'NONE',  ( 14.92337183194729633, 22.67559781766745175, 8.527530157486181039 ) ) ;
#22905 = CARTESIAN_POINT ( 'NONE',  ( 6.204703633549690345, 7.845415501580634832, 14.16423886937410082 ) ) ;
#22906 = DIRECTION ( 'NONE',  ( 0.8526401643540846287, 0.000000000000000000, 0.5224985647159611224 ) ) ;
#22907 = CARTESIAN_POINT ( 'NONE',  ( 15.44008868035555793, 36.39701867748816966, -9.422509992056140149 ) ) ;
#22909 = CARTESIAN_POINT ( 'NONE',  ( -4.164238869374098151, 46.59541550158063927, -3.795296366450310543 ) ) ;
#22908 = CARTESIAN_POINT ( 'NONE',  ( 19.42250999205614193, 15.14701867748817143, 5.440088680355555262 ) ) ;
#22910 =( GEOMETRIC_REPRESENTATION_CONTEXT ( 3 ) GLOBAL_UNCERTAINTY_ASSIGNED_CONTEXT ( ( #21480 ) ) GLOBAL_UNIT_ASSIGNED_CONTEXT ( ( #65012, #57036, #20528 ) ) REPRESENTATION_CONTEXT ( 'NONE', 'WORKASPACE' ) );
#22911 = EDGE_CURVE ( 'NONE', #35183, #45903, #4243, .T. ) ;
#22912 = CARTESIAN_POINT ( 'NONE',  ( 17.96484262340118221, 34.93868534415482685, 7.964842623401181321 ) ) ;
#22913 = CARTESIAN_POINT ( 'NONE',  ( 0.5774900079438607392, 18.48035201082150536, 5.440088680355550821 ) ) ;
#22914 = ORIENTED_EDGE ( 'NONE', *, *, #26120, .F. ) ;
#22915 = CARTESIAN_POINT ( 'NONE',  ( 19.42250999205614193, 45.14701867748817676, 5.440088680355555262 ) ) ;
#22916 = CARTESIAN_POINT ( 'NONE',  ( 10.00000000000000000, 42.87363466993042493, -12.81628187352647608 ) ) ;
#22917 = CARTESIAN_POINT ( 'NONE',  ( 15.44008868035555793, 46.39701867748817676, -9.422509992056140149 ) ) ;
#22919 = CARTESIAN_POINT ( 'NONE',  ( -0.8801773607111009756, 53.06368534415484106, 1.068504757029289695E-15 ) ) ;
#22918 = CARTESIAN_POINT ( 'NONE',  ( 1.472469842513823179, 46.42559781766745175, 4.923371831947296329 ) ) ;
#22920 = ORIENTED_EDGE ( 'NONE', *, *, #66589, .T. ) ;
#22921 = CARTESIAN_POINT ( 'NONE',  ( 20.88017736071110875, 55.77201867748816966, -2.915334737309920765 ) ) ;
#22922 = CARTESIAN_POINT ( 'NONE',  ( 4.823529266124356063, -6.402884419280910677, 4.000000000000000000 ) ) ;
#22923 = CARTESIAN_POINT ( 'NONE',  ( -0.1049300847420624738, 37.21697413083879979, -6.336235997365760930 ) ) ;
#22924 = CARTESIAN_POINT ( 'NONE',  ( -4.164238869374098151, 46.59541550158063927, -3.795296366450310543 ) ) ;
#22925 = CARTESIAN_POINT ( 'NONE',  ( 20.88017736071110164, 60.35535201082151957, 2.915334737309930979 ) ) ;
#22926 = B_SPLINE_CURVE_WITH_KNOTS ( 'NONE', 3,
 ( #59117, #37136, #89134, #52612, #60605, #83616 ),
 .UNSPECIFIED., .F., .F.,
 ( 4, 2, 4 ),
 ( 3.409110551494638557E-05, 0.0004400426677367922637, 0.0008459942299586381553 ),
 .UNSPECIFIED. ) ;
#22928 = B_SPLINE_CURVE_WITH_KNOTS ( 'NONE', 3,
 ( #30233, #43761, #36773, #83254, #28763, #67767 ),
 .UNSPECIFIED., .F., .F.,
 ( 4, 2, 4 ),
 ( 0.0002800056097852249184, 0.0006862108940693780260, 0.001092416178353531079 ),
 .UNSPECIFIED. ) ;
#22927 = DIRECTION ( 'NONE',  ( 0.000000000000000000, 1.000000000000000000, 0.000000000000000000 ) ) ;
#22929 = CARTESIAN_POINT ( 'NONE',  ( -3.750000000000001776, 0.08806741915675847521, -4.000000000000000000 ) ) ;
#22930 = CARTESIAN_POINT ( 'NONE',  ( 7.361572987183170547, 62.05059781766745886, 9.846743663894590881 ) ) ;
#22931 = PRESENTATION_STYLE_ASSIGNMENT (( #6423 ) ) ;
#22932 = CARTESIAN_POINT ( 'NONE',  ( 18.52753015748617571, 38.09226448433412315, 4.923371831947298993 ) ) ;
#22933 = ORIENTED_EDGE ( 'NONE', *, *, #21856, .T. ) ;
#22934 = CARTESIAN_POINT ( 'NONE',  ( 18.52753015748618282, 28.92559781766745175, -4.923371831947291888 ) ) ;
#22935 = CARTESIAN_POINT ( 'NONE',  ( 11.09922568453594671, -2.959698663402905883, -6.408140936763241591 ) ) ;
#22936 = CARTESIAN_POINT ( 'NONE',  ( 10.00000000000000178, 24.31368534415484106, 10.88017736071110342 ) ) ;
#22937 = CARTESIAN_POINT ( 'NONE',  ( 2.791683348922240793, 36.63393115100078035, 7.208316651077764092 ) ) ;
#22938 = CARTESIAN_POINT ( 'NONE',  ( 3.591859063236763294, 18.29030133659708568, -11.09922568453595026 ) ) ;
#22940 = CARTESIAN_POINT ( 'NONE',  ( 20.88017736071110875, 60.77201867748817676, -2.915334737309920765 ) ) ;
#22939 = FACE_OUTER_BOUND ( 'NONE', #12097, .T. ) ;
#22942 = CARTESIAN_POINT ( 'NONE',  ( 0.6178305044545838731, 64.74863466993043914, 9.382169495545420901 ) ) ;
#22941 = CARTESIAN_POINT ( 'NONE',  ( 17.96484262340118221, 46.18868534415484106, -7.964842623401177768 ) ) ;
#22943 = CARTESIAN_POINT ( 'NONE',  ( 24.16423886937410614, 59.30374883491397497, 8.672049930838204340E-16 ) ) ;
#22944 = ADVANCED_FACE ( 'NONE', ( #3756 ), #7809, .T. ) ;
#22945 = CARTESIAN_POINT ( 'NONE',  ( -2.816281873526473856, 24.33196800326375353, 3.434112377981055619 ) ) ;
#22946 = EDGE_CURVE ( 'NONE', #89322, #86711, #18753, .T. ) ;
#22947 = DIRECTION ( 'NONE',  ( 0.000000000000000000, 0.000000000000000000, 1.000000000000000000 ) ) ;
#22948 = ADVANCED_FACE ( 'NONE', ( #34713 ), #95728, .T. ) ;
#22949 = VERTEX_POINT ( 'NONE', #95219 ) ;
#22950 = CARTESIAN_POINT ( 'NONE',  ( 21.09922568453594849, 21.20696800326375353, 6.408140936763242479 ) ) ;
#22951 = CARTESIAN_POINT ( 'NONE',  ( -0.8801773607110991993, 17.85535201082150536, -2.915334737309923874 ) ) ;
#22952 = CARTESIAN_POINT ( 'NONE',  ( 2.035157376598824452, 63.68868534415484106, 7.964842623401179544 ) ) ;
#22953 = CYLINDRICAL_SURFACE ( 'NONE', #45733, 11.92686044187656513 ) ;
#22954 = EDGE_LOOP ( 'NONE', ( #45216, #16042, #6312, #85188, #90535, #73467 ) ) ;
#22955 = CARTESIAN_POINT ( 'NONE',  ( -0.8801773607110991993, 52.85535201082151247, -2.915334737309923874 ) ) ;
#22956 = CARTESIAN_POINT ( 'NONE',  ( 10.00000000000000178, 42.25893115100078745, 9.846743663894594434 ) ) ;
#22957 = EDGE_CURVE ( 'NONE', #70902, #2423, #86755, .T. ) ;
#22958 = CARTESIAN_POINT ( 'NONE',  ( 1.472469842513823179, 21.42559781766745175, 4.923371831947296329 ) ) ;
#22959 = CARTESIAN_POINT ( 'NONE',  ( 17.20831665107776587, 19.13393115100078035, -7.208316651077762316 ) ) ;
#22960 = CARTESIAN_POINT ( 'NONE',  ( 21.92686044187656691, 57.18830936912751639, 4.562052436263911564E-16 ) ) ;
#22962 = CARTESIAN_POINT ( 'NONE',  ( 21.09922568453595559, 37.04030133659708923, -6.408140936763230044 ) ) ;
#22961 = CARTESIAN_POINT ( 'NONE',  ( -1.028725271592155099, -1.208271517246092823E-15, 4.540618777627624780 ) ) ;
#22963 = CARTESIAN_POINT ( 'NONE',  ( 14.92337183194729633, 17.67559781766745175, 8.527530157486181039 ) ) ;
#22964 = DIRECTION ( 'NONE',  ( 0.8788171126619711560, 0.000000000000000000, -0.4771587602595978028 ) ) ;
#22966 = ORIENTED_EDGE ( 'NONE', *, *, #31079, .F. ) ;
#22965 = CARTESIAN_POINT ( 'NONE',  ( 5.076628168052703671, 36.84226448433412315, 8.527530157486179263 ) ) ;
#22967 = LINE ( 'NONE', #30925, #96547 ) ;
#22968 = CARTESIAN_POINT ( 'NONE',  ( 22.81628187352647785, 16.62363466993042138, 6.195893100308588602E-16 ) ) ;
#22969 = MECHANICAL_DESIGN_GEOMETRIC_PRESENTATION_REPRESENTATION (  '', ( #96403 ), #94812 ) ;
#22970 = CARTESIAN_POINT ( 'NONE',  ( 19.42250999205614548, 50.98035201082151247, -5.440088680355545492 ) ) ;
#22971 = CARTESIAN_POINT ( 'NONE',  ( -4.164238869374098151, 36.59541550158063217, -3.795296366450310543 ) ) ;
#22972 = CARTESIAN_POINT ( 'NONE',  ( -13.38735934609733036, 90.81479509783585513, 7.611013694203884405 ) ) ;
#22973 = ADVANCED_FACE ( 'NONE', ( #11728 ), #73205, .T. ) ;
#22974 = VECTOR ( 'NONE', #19926, 1000.000000000000000 ) ;
#22975 = CARTESIAN_POINT ( 'NONE',  ( 10.00000000000000178, 33.05374883491396787, 14.16423886937410082 ) ) ;
#22976 = CARTESIAN_POINT ( 'NONE',  ( 13.79529636645031943, 55.34541550158062506, -14.16423886937409904 ) ) ;
#22977 = CARTESIAN_POINT ( 'NONE',  ( 20.36894250292379738, 14.92874883491396432, -10.36894250292379027 ) ) ;
#22979 = CARTESIAN_POINT ( 'NONE',  ( 19.39188664607693013, 35.83703382326400089, -6.500000000000031974 ) ) ;
#22978 = CARTESIAN_POINT ( 'NONE',  ( -4.164238869374098151, 26.59541550158063217, -3.795296366450310543 ) ) ;
#22980 = CARTESIAN_POINT ( 'NONE',  ( 4.559911319644449179, 42.23035201082151247, -9.422509992056141925 ) ) ;
#22981 = CARTESIAN_POINT ( 'NONE',  ( -11.25000000000000178, 10.11803362898265846, 3.674383000693412496E-15 ) ) ;
#22983 = CARTESIAN_POINT ( 'NONE',  ( 19.84674366389459621, 43.50893115100078745, 7.409399052514197653E-17 ) ) ;
#22982 = CARTESIAN_POINT ( 'NONE',  ( 10.00000000000000178, 69.31368534415484817, 10.88017736071110342 ) ) ;
#22984 = CARTESIAN_POINT ( 'NONE',  ( 0.5774900079438590739, 22.64701867748817321, -5.440088680355550821 ) ) ;
#22985 = LINE ( 'NONE', #69451, #77001 ) ;
#22986 = CARTESIAN_POINT ( 'NONE',  ( 7.361572987183170547, 62.05059781766745886, 9.846743663894590881 ) ) ;
#22987 = CARTESIAN_POINT ( 'NONE',  ( 20.00000000000000711, 84.99347556687297356, -4.825407043045644606 ) ) ;
#22988 = CARTESIAN_POINT ( 'NONE',  ( 14.92337183194729633, 32.67559781766745175, 8.527530157486181039 ) ) ;
#22989 = CARTESIAN_POINT ( 'NONE',  ( 13.43411237798106583, 57.66530133659708923, -12.81628187352647252 ) ) ;
#22990 = CARTESIAN_POINT ( 'NONE',  ( -10.36894250292379205, -3.821251165086027246, -10.36894250292378672 ) ) ;
#22991 = CARTESIAN_POINT ( 'NONE',  ( 12.63842701281683034, 42.46726448433412315, 9.846743663894596210 ) ) ;
#22992 = CARTESIAN_POINT ( 'NONE',  ( 12.63842701281683034, 47.46726448433412315, 9.846743663894596210 ) ) ;
#22993 = CARTESIAN_POINT ( 'NONE',  ( 2.917880565312948704, 42.63708216824729647, 12.26659068614894643 ) ) ;
#22994 = ORIENTED_EDGE ( 'NONE', *, *, #19435, .F. ) ;
#22995 = CARTESIAN_POINT ( 'NONE',  ( -0.3689425029237898834, 11.17874883491396787, -10.36894250292378850 ) ) ;
#22996 = CARTESIAN_POINT ( 'NONE',  ( 0.5774900079438607392, 68.48035201082150536, 5.440088680355550821 ) ) ;
#22997 = DIRECTION ( 'NONE',  ( -0.000000000000000000, -0.000000000000000000, 1.000000000000000000 ) ) ;
#22998 = CARTESIAN_POINT ( 'NONE',  ( 10.00000000000000178, 63.05374883491396076, 14.16423886937410082 ) ) ;
#22999 = CARTESIAN_POINT ( 'NONE',  ( 6.565887622018943937, 15.16530133659708568, 12.81628187352647430 ) ) ;
#23000 = CARTESIAN_POINT ( 'NONE',  ( -0.1503990784575279516, 53.10158574516643171, 6.262539305110076171 ) ) ;
#23001 = CARTESIAN_POINT ( 'NONE',  ( 10.00000000000000178, 59.31368534415484106, 10.88017736071110342 ) ) ;
#23002 = CARTESIAN_POINT ( 'NONE',  ( -0.3289641300567998083, 28.07879003517447458, 5.963430220938281678 ) ) ;
#23003 = CARTESIAN_POINT ( 'NONE',  ( -46.94000000000240647, 102.7387969410441002, -6.737038697110588004 ) ) ;
#23004 = CARTESIAN_POINT ( 'NONE',  ( -4.164238869374099039, 61.80374883491397497, 8.674139862899312516E-16 ) ) ;
#23005 = CARTESIAN_POINT ( 'NONE',  ( -7.964842623401172439, 33.68868534415485527, 7.964842623401183097 ) ) ;
#23006 = CARTESIAN_POINT ( 'NONE',  ( 7.084665262690076126, 17.02201867748817676, -10.88017736071110164 ) ) ;
#23007 = CARTESIAN_POINT ( 'NONE',  ( 7.084665262690076126, 24.10535201082150181, 10.88017736071109987 ) ) ;
#23008 = CARTESIAN_POINT ( 'NONE',  ( 19.84674366389459266, 58.30059781766745886, 2.638427012816836559 ) ) ;
#23009 = CARTESIAN_POINT ( 'NONE',  ( 14.92337183194729988, 54.34226448433412315, -8.527530157486177487 ) ) ;
#23010 = CARTESIAN_POINT ( 'NONE',  ( 0.6178305044545838731, 44.74863466993042493, 9.382169495545420901 ) ) ;
#23011 = CARTESIAN_POINT ( 'NONE',  ( 0.1532563361054082862, 1.217264484334117824, 2.638427012816831674 ) ) ;
#23012 = VERTEX_POINT ( 'NONE', #41756 ) ;
#23013 = CARTESIAN_POINT ( 'NONE',  ( 20.88017736071110519, 10.56368534415483751, 2.639326808657452039E-16 ) ) ;
#23014 = ADVANCED_FACE ( 'NONE', ( #19233 ), #72226, .T. ) ;
#23015 = CARTESIAN_POINT ( 'NONE',  ( -1.099225684535947600, 24.54030133659708923, 6.408140936763237150 ) ) ;
#23016 = FACE_OUTER_BOUND ( 'NONE', #76694, .T. ) ;
#23017 = CARTESIAN_POINT ( 'NONE',  ( 2.791683348922237240, 50.38393115100078035, -7.208316651077763204 ) ) ;
#23018 = CARTESIAN_POINT ( 'NONE',  ( 10.00000000000000178, 39.31368534415484106, 10.88017736071110342 ) ) ;
#23019 = CARTESIAN_POINT ( 'NONE',  ( 19.38216949554541202, 15.99863466993042138, 9.382169495545424454 ) ) ;
#23021 = CARTESIAN_POINT ( 'NONE',  ( 4.629999999999991900, 76.07179676972444327, 4.000000000000000000 ) ) ;
#23020 = CARTESIAN_POINT ( 'NONE',  ( 0.5774900079438590739, 47.64701867748817676, -5.440088680355550821 ) ) ;
#23022 = CARTESIAN_POINT ( 'NONE',  ( 21.09922568453595559, 52.04030133659708923, -6.408140936763230044 ) ) ;
#23023 = ORIENTED_EDGE ( 'NONE', *, *, #35057, .F. ) ;
#23024 = CARTESIAN_POINT ( 'NONE',  ( 0.1532563361054100626, 65.80059781766745175, -2.638427012816831230 ) ) ;
#23025 = CARTESIAN_POINT ( 'NONE',  ( 7.084665262690076126, 52.02201867748816255, -10.88017736071110164 ) ) ;
#23027 = CARTESIAN_POINT ( 'NONE',  ( 24.16423886937409904, 19.09541550158063927, 3.795296366450317205 ) ) ;
#23026 = CARTESIAN_POINT ( 'NONE',  ( 13.43411237798105340, 40.58196800326375353, 12.81628187352647963 ) ) ;
#23028 = CARTESIAN_POINT ( 'NONE',  ( 2.035157376598824452, 53.68868534415484817, 7.964842623401179544 ) ) ;
#23029 = CARTESIAN_POINT ( 'NONE',  ( 19.84674366389459621, 63.50893115100078745, 7.409399052514197653E-17 ) ) ;
#23030 = CARTESIAN_POINT ( 'NONE',  ( 5.076628168052704559, 20.17559781766745175, -8.527530157486179263 ) ) ;
#23031 = CARTESIAN_POINT ( 'NONE',  ( 17.20831665107776587, 2.883931151000785231, 7.208316651077764980 ) ) ;
#23032 = LINE ( 'NONE', #38519, #20328 ) ;
#23033 = CARTESIAN_POINT ( 'NONE',  ( 17.08211943468705840, 40.13708216824731068, -12.26659068614894466 ) ) ;
#23034 = CARTESIAN_POINT ( 'NONE',  ( 21.92686044187657046, 25.16212336850780673, 4.562052436263912550E-16 ) ) ;
#23035 = CARTESIAN_POINT ( 'NONE',  ( 2.035157376598822676, 7.438685344154837509, -7.964842623401177768 ) ) ;
#23036 = DIRECTION ( 'NONE',  ( 0.000000000000000000, 0.000000000000000000, 1.000000000000000000 ) ) ;
#23037 = ORIENTED_EDGE ( 'NONE', *, *, #63126, .F. ) ;
#23038 = CARTESIAN_POINT ( 'NONE',  ( 0.5774900079438590739, 7.647018677488171434, -5.440088680355550821 ) ) ;
#23039 = CARTESIAN_POINT ( 'NONE',  ( 6.204703633549690345, 67.84541550158060375, 14.16423886937410082 ) ) ;
#23040 = CARTESIAN_POINT ( 'NONE',  ( 17.20831665107776587, 44.13393115100078745, -7.208316651077762316 ) ) ;
#23041 = CARTESIAN_POINT ( 'NONE',  ( 6.565887622018943937, 40.16530133659708923, 12.81628187352647430 ) ) ;
#23042 =( NAMED_UNIT ( * ) PLANE_ANGLE_UNIT ( ) SI_UNIT ( $, .RADIAN. ) );
#23045 = CARTESIAN_POINT ( 'NONE',  ( 6.204703633549690345, 2.845415501580634388, 14.16423886937410082 ) ) ;
#23044 = CARTESIAN_POINT ( 'NONE',  ( 18.72515096720583827, 56.07228050351029225, -6.499999999999802824 ) ) ;
#23043 = VECTOR ( 'NONE', #86889, 1000.000000000000000 ) ;
#23046 = CARTESIAN_POINT ( 'NONE',  ( 7.084665262690076126, 32.02201867748816966, -10.88017736071110164 ) ) ;
#23047 = CARTESIAN_POINT ( 'NONE',  ( -4.164238869374099927, 67.01208216824728936, 3.795296366450308767 ) ) ;
#23048 = CARTESIAN_POINT ( 'NONE',  ( 1.472469842513823179, 45.59226448433412315, -4.923371831947296329 ) ) ;
#23049 = DIRECTION ( 'NONE',  ( 0.000000000000000000, 1.000000000000000000, 0.000000000000000000 ) ) ;
#23050 = CARTESIAN_POINT ( 'NONE',  ( 2.791683348922237240, 20.38393115100078745, -7.208316651077763204 ) ) ;
#23051 = CIRCLE ( 'NONE', #45361, 0.5000000000000004441 ) ;
#23052 =( NAMED_UNIT ( * ) SI_UNIT ( $, .STERADIAN. ) SOLID_ANGLE_UNIT ( ) );
#23053 = CARTESIAN_POINT ( 'NONE',  ( 7.208316651077764980, 17.88393115100078745, 7.208316651077762316 ) ) ;
#23054 = ORIENTED_EDGE ( 'NONE', *, *, #51347, .T. ) ;
#23056 = EDGE_CURVE ( 'NONE', #63858, #89913, #48737, .T. ) ;
#23055 = CARTESIAN_POINT ( 'NONE',  ( 0.000000000000000000, 15.00000000000000000, 0.000000000000000000 ) ) ;
#23057 = ORIENTED_EDGE ( 'NONE', *, *, #51230, .T. ) ;
#23058 = CARTESIAN_POINT ( 'NONE',  ( 18.52753015748618282, 58.92559781766745886, -4.923371831947291888 ) ) ;
#23060 = CARTESIAN_POINT ( 'NONE',  ( 12.91533473730992121, 39.52201867748817676, 10.88017736071110164 ) ) ;
#23059 = CARTESIAN_POINT ( 'NONE',  ( 0.5774900079438607392, 33.48035201082150536, 5.440088680355550821 ) ) ;
#23062 = CARTESIAN_POINT ( 'NONE',  ( 16.40814093676323893, 30.79030133659708923, 11.09922568453595026 ) ) ;
#23061 = FILL_AREA_STYLE ('',( #66569 ) ) ;
#23063 = CARTESIAN_POINT ( 'NONE',  ( 6.204703633549690345, 17.84541550158063217, 14.16423886937410082 ) ) ;
#23064 = EDGE_CURVE ( 'NONE', #70379, #7185, #94237, .T. ) ;
#23065 = ADVANCED_FACE ( 'NONE', ( #41273 ), #24057, .T. ) ;
#23066 = EDGE_CURVE ( 'NONE', #48953, #84655, #3255, .T. ) ;
#23067 = CARTESIAN_POINT ( 'NONE',  ( 10.00000000000000000, 47.87363466993042493, -12.81628187352647608 ) ) ;
#23068 = EDGE_CURVE ( 'NONE', #1670, #98319, #43700, .T. ) ;
#23069 = ORIENTED_EDGE ( 'NONE', *, *, #75508, .T. ) ;
#23070 = CARTESIAN_POINT ( 'NONE',  ( 18.52753015748617571, 48.09226448433412315, 4.923371831947298993 ) ) ;
#23071 = CARTESIAN_POINT ( 'NONE',  ( 0.5774900079438590739, 2.647018677488171434, -5.440088680355550821 ) ) ;
#23072 = EDGE_LOOP ( 'NONE', ( #97333, #8514, #71398, #77742 ) ) ;
#23073 = CARTESIAN_POINT ( 'NONE',  ( 7.084665262690076126, 22.02201867748817321, -10.88017736071110164 ) ) ;
#23074 = ORIENTED_EDGE ( 'NONE', *, *, #36622, .T. ) ;
#23075 = CARTESIAN_POINT ( 'NONE',  ( 2.035157376598822676, 67.43868534415484817, -7.964842623401177768 ) ) ;
#23076 = CARTESIAN_POINT ( 'NONE',  ( 19.42250999205614548, 55.98035201082150536, -5.440088680355545492 ) ) ;
#23077 = CARTESIAN_POINT ( 'NONE',  ( 0.5774900079438590739, 67.64701867748817676, -5.440088680355550821 ) ) ;
#23078 = DIRECTION ( 'NONE',  ( 0.7604059656000387024, 0.000000000000000000, -0.6494480483301745544 ) ) ;
#23079 = CARTESIAN_POINT ( 'NONE',  ( 15.44008868035555793, 51.39701867748816966, -9.422509992056140149 ) ) ;
#23080 = CARTESIAN_POINT ( 'NONE',  ( 64.56412365047462742, 26.99999999999999645, -10.00000000000000000 ) ) ;
#23081 = AXIS2_PLACEMENT_3D ( 'NONE', #77846, #9355, #31357 ) ;
#23082 = CARTESIAN_POINT ( 'NONE',  ( 1.959929470562273179, 10.51528370094808196, -5.767676674365838529 ) ) ;
#23084 = ORIENTED_EDGE ( 'NONE', *, *, #60532, .T. ) ;
#23083 =( LENGTH_UNIT ( ) NAMED_UNIT ( * ) SI_UNIT ( .MILLI., .METRE. ) );
#23085 = CARTESIAN_POINT ( 'NONE',  ( 7.361572987183170547, 37.05059781766744464, 9.846743663894590881 ) ) ;
#23086 = ORIENTED_EDGE ( 'NONE', *, *, #13960, .T. ) ;
#23087 = CARTESIAN_POINT ( 'NONE',  ( 4.380000000000002558, 1.019547802438462547, -3.750000000000000000 ) ) ;
#23088 = FILL_AREA_STYLE ('',( #109 ) ) ;
#23089 = EDGE_CURVE ( 'NONE', #20606, #6963, #82689, .T. ) ;
#23090 = CARTESIAN_POINT ( 'NONE',  ( 6.204703633549690345, 17.84541550158063217, 14.16423886937410082 ) ) ;
#23091 = CARTESIAN_POINT ( 'NONE',  ( 3.897244926436124857, 3.990182060915936250E-16, 13.96644127841333294 ) ) ;
#23092 = CARTESIAN_POINT ( 'NONE',  ( 3.969999999999999751, 36.75000000000000000, 2.750000000000000000 ) ) ;
#23093 = CARTESIAN_POINT ( 'NONE',  ( 19.42250999205614548, 5.980352010821504471, -5.440088680355545492 ) ) ;
#23094 = CARTESIAN_POINT ( 'NONE',  ( 1.959929470562273179, 66.50257860105348584, 5.767676674365838529 ) ) ;
#23096 = ORIENTED_EDGE ( 'NONE', *, *, #46328, .T. ) ;
#23095 = CARTESIAN_POINT ( 'NONE',  ( -2.816281873526473856, 39.33196800326374643, 3.434112377981055619 ) ) ;
#23097 = DIRECTION ( 'NONE',  ( -1.000000000000000000, 5.782411586589362323E-17, -0.000000000000000000 ) ) ;
#23098 = CARTESIAN_POINT ( 'NONE',  ( 18.52753015748617571, 53.09226448433412315, 4.923371831947298993 ) ) ;
#23099 = CARTESIAN_POINT ( 'NONE',  ( 10.00000000000000178, 15.37363466993042138, 12.81628187352647608 ) ) ;
#23100 = CARTESIAN_POINT ( 'NONE',  ( 0.1532563361054082862, 21.21726448433412315, 2.638427012816831674 ) ) ;
#23101 = DIRECTION ( 'NONE',  ( 0.9914448613738086058, 0.000000000000000000, 0.1305261922200653124 ) ) ;
#23102 = CARTESIAN_POINT ( 'NONE',  ( 10.00000000000000178, 15.37363466993042138, 12.81628187352647608 ) ) ;
#23103 = CARTESIAN_POINT ( 'NONE',  ( 12.63842701281683922, 9.550597817667449974, -9.846743663894590881 ) ) ;
#23104 = STYLED_ITEM ( 'NONE', ( #46803 ), #30996 ) ;
#23105 = VERTEX_POINT ( 'NONE', #13701 ) ;
#23106 = ORIENTED_EDGE ( 'NONE', *, *, #56544, .T. ) ;
#23107 = CIRCLE ( 'NONE', #75767, 0.5000000000000005551 ) ;
#23108 = CARTESIAN_POINT ( 'NONE',  ( 12.91533473730992121, 19.52201867748816611, 10.88017736071110164 ) ) ;
#23109 = CARTESIAN_POINT ( 'NONE',  ( -2.266590686148945544, 21.38708216824730357, -7.082119434687050408 ) ) ;
#23110 = CARTESIAN_POINT ( 'NONE',  ( 10.00000000000000178, 47.25893115100078745, 9.846743663894594434 ) ) ;
#23111 = CARTESIAN_POINT ( 'NONE',  ( 2.035157376598824452, 63.68868534415484106, 7.964842623401179544 ) ) ;
#23113 = CARTESIAN_POINT ( 'NONE',  ( 0.000000000000000000, 0.5000000000000004441, 0.000000000000000000 ) ) ;
#23112 = CARTESIAN_POINT ( 'NONE',  ( 13.43411237798105340, 45.58196800326374643, 12.81628187352647963 ) ) ;
#23114 = CARTESIAN_POINT ( 'NONE',  ( 4.559911319644449179, 13.89701867748817143, 9.422509992056141925 ) ) ;
#23115 = MECHANICAL_DESIGN_GEOMETRIC_PRESENTATION_REPRESENTATION (  '', ( #66187 ), #90104 ) ;
#23116 = CARTESIAN_POINT ( 'NONE',  ( 0.000000000000000000, 15.00000000000000000, 0.000000000000000000 ) ) ;
#23117 = CARTESIAN_POINT ( 'NONE',  ( 3.591859063236763294, 13.29030133659708746, -11.09922568453595026 ) ) ;
#23118 = CARTESIAN_POINT ( 'NONE',  ( 1.472469842513823179, 30.59226448433411960, -4.923371831947296329 ) ) ;
#23119 = CARTESIAN_POINT ( 'NONE',  ( -5.440088680355547268, -6.102981322511823237, 9.422509992056143702 ) ) ;
#23120 = CARTESIAN_POINT ( 'NONE',  ( -1.099225684535947600, 38.70696800326375353, -6.408140936763238038 ) ) ;
#23121 = CIRCLE ( 'NONE', #19879, 2.899999999999999911 ) ;
#23122 = CARTESIAN_POINT ( 'NONE',  ( 18.72515096720609051, 25.05509018479941119, 6.499999999999470646 ) ) ;
#23124 = CARTESIAN_POINT ( 'NONE',  ( 2.603489959281060973, 26.58210964143323096, 6.499999999999401368 ) ) ;
#23123 = CARTESIAN_POINT ( 'NONE',  ( 7.084665262690076126, 52.02201867748816255, -10.88017736071110164 ) ) ;
#23125 = CARTESIAN_POINT ( 'NONE',  ( 18.72515096720583827, 30.05509018479937566, 6.499999999999810818 ) ) ;
#23126 = CARTESIAN_POINT ( 'NONE',  ( 7.084665262690076126, 37.02201867748817676, -10.88017736071110164 ) ) ;
#23127 = CARTESIAN_POINT ( 'NONE',  ( -0.8801773607111008646, 43.27201867748817676, 2.915334737309923430 ) ) ;
#23128 = CARTESIAN_POINT ( 'NONE',  ( 14.92337183194729988, 64.34226448433412315, -8.527530157486177487 ) ) ;
#23129 = LINE ( 'NONE', #98149, #41175 ) ;
#23130 = UNCERTAINTY_MEASURE_WITH_UNIT (LENGTH_MEASURE( 1.000000000000000082E-05 ), #20942, 'distance_accuracy_value', 'NONE');
#23131 =( BOUNDED_SURFACE ( )  B_SPLINE_SURFACE ( 1, 2, ( 
 ( #93856, #49333, #94345, #93362, #2886, #64812, #47365, #47855, #3355, #25384, #17386, #24887, #18361, #9375, #55372, #48839, #33817, #39877, #64324, #86366, #94835, #56839, #87337, #18852, #11338, #24396, #54864, #32359, #78360, #40380, #51311, #57324, #28314, #72812, #88816, #73315, #58300, #4353, #50311, #28798, #65309, #34819, #36312, #20329, #80826, #73804, #43797, #50823, #36812, #81316, #13813, #12812, #87818, #96838, #42830, #51807, #44297, #5335, #95835, #5819, #19822, #27318, #57815, #74799, #88324, #12325, #66806, #35815, #4839, #6307, #97328, #58805, #80331, #35314, #81793, #65808, #96340, #27815, #43311, #11830, #66301, #89312, #13310, #49821, #74290, #20821, #59299, #89796, #21314, #82291, #95331, #26830, #19338, #42338, #16282, #324, #23302, #29292, #30767, #44788, #60778, #45290, #30277, #75293, #22314, #806, #37316, #6802, #8287, #91281, #52786, #45795, #15795, #22802, #8769, #53281, #84774, #83787, #59790, #68793, #14819, #23798, #46763, #76287, #67808, #76769, #90787, #98325, #29782, #77258, #60293, #83294, #38784, #7801, #75785, #67303, #69285, #61272, #52301, #15310, #91781, #53780, #38298, #97830, #31260, #7308, #98823, #84298, #46283, #61756, #92274, #54261, #37809, #90282, #21817, #82795, #14318, #68304, #78244, #63725, #39771, #55757, #94724, #39285, #79230, #18245, #33711, #31756, #87217, #40748, #86249, #47748, #10255, #69774, #10741, #71253, #32243, #9759, #70270, #92757, #56726, #40261, #79725, #1304, #77750, #25277, #70767, #41260, #62252, #9265, #3244, #32738, #78749, #2281, #63237, #64210, #2775, #1787, #93740, #18740, #24282, #71734, #33231, #62744, #17761, #93244, #54747, #49223, #48238, #85267, #16774, #24769, #94225, #25757, #26232, #47250, #55247, #85762, #56249, #86743, #48725, #17274, #36191, #81197, #49701, #65692, #28683, #72214, #34700, #66181, #88201, #72693, #80211, #96215, #95206, #11716, #27697, #96716, #64694, #28193, #57700, #43193, #43685, #5215, #42711, #66691, #89191, #59177, #58690, #89682, #73681, #20703, #3744, #35697, #87704, #4726, #19710, #73193, #19219, #65195, #74170, #42228, #4230, #51195, #35188, #95716, #88692, #81677, #58181, #51696, #20201, #21197, #50704, #34202, #12699, #50196, #97218, #11225, #13192, #27199, #5704, #80708, #12202, #41745, #26711, #57208, #44677, #93003, #92510, #29658, #93502, #85515, #47011, #67185, #75670, #85021, #77502, #62010, #62998, #54997, #60168, #14698, #9014, #7181, #54508, #24038, #1548, #21697, #17026, #45167, #37686, #39531, #98202, #22191, #70023, #82677, #98704, #40013, #82175, #24537, #62500, #78006, #74683, #32500, #16535 ),
 ( #52182, #68184, #90663, #47504, #6195, #14196, #9512, #31509, #31993, #52671, #83172, #70517, #2039, #75171, #25027, #13687, #44173, #6681, #36699, #97709, #37200, #67691, #29176, #59676, #90166, #41507, #11475, #10015, #72456, #3020, #87471, #87956, #49463, #86980, #11966, #34454, #4483, #3988, #34949, #18985, #41992, #17525, #79969, #32989, #48978, #33469, #18490, #63492, #10494, #19473, #25518, #93995, #95473, #79487, #41006, #33956, #64946, #10987, #95971, #71975, #72953, #3499, #47991, #56968, #63965, #42470, #65448, #64460, #56005, #26963, #78988, #86508, #18005, #55513, #48486, #71507, #57463, #94967, #94479, #86012, #49963, #80467, #40516, #26469, #78502, #71013, #2535, #25996, #56491, #73942, #58943, #51943, #51445, #97459, #36446, #44426, #65945, #29415, #89444, #81933, #89930, #43441, #66438, #82427, #27944, #43928, #82927, #27456, #67439, #6430, #21950, #19956, #75422, #28924, #74426, #35942, #59428, #57948, #97960, #21445, #20459, #96973, #20958, #13953, #13441, #74931, #66938, #36942, #96472, #59920, #5954, #90408, #52429, #5470, #28446, #14445, #58436, #44915, #6937, #88455, #37444, #67935, #50450, #80957, #12456, #42962, #73443, #4968, #35450, #88951, #50949, #81444, #12945, #7926, #98950, #52911, #16902, #68921, #39893, #98455, #37938, #84417, #38423, #39408, #22440, #68428, #62374, #91904, #38915, #449, #30900, #24412, #69403, #30406, #53908, #47378, #60417, #22937, #54385, #76411, #60908, #91411, #15914, #83425, #53405, #46405, #84898, #14943, #16410, #45922, #31386, #31874, #92391, #61394, #54878, #77379, #77877, #46888, #9389, #61886, #8892, #90912, #23916, #75917, #23429, #76894, #8408, #7441, #83914, #92878, #15442, #924, #69902, #1422, #85389, #29911, #45412, #33351, #11844, #63845, #87833, #94358, #62878, #71860, #17882, #26843, #19351, #48854, #40397, #79849, #93870, #70892, #2409, #49835, #9893, #32868, #11352, #79363, #48366, #80347, #72336, #33832, #55386, #25877, #3371, #64340, #10871, #70396, #41872, #78871, #94851, #63368, #86867, #57338, #1914, #3868, #49348, #64827, #93376, #32373, #26351, #18375, #10380, #41392, #24903, #34331, #56853, #25397, #40883, #55882, #85887, #17401, #71388, #47869, #78374, #86380, #56378, #2901, #95344, #87352, #18866, #6314, #35827, #81805, #12822, #81327, #67313, #13323, #80837, #96849, #59798, #4366, #65819, #97337, #20338, #4850, #12337, #28324, #27332, #42841, #58815, #28810, #95848, #59308, #88826, #74303, #74808, #36322, #73814, #97838, #21327, #90289, #89806, #21827, #5828, #51815, #34832, #66815, #19835, #66313, #50834, #5348, #50324, #96354, #36821 ) ),
 .UNSPECIFIED., .F., .F., .F. ) 
 B_SPLINE_SURFACE_WITH_KNOTS ( ( 2, 2 ),
 ( 3, 2, 2, 2, 2, 2, 2, 2, 2, 2, 2, 2, 2, 2, 2, 2, 2, 2, 2, 2, 2, 2, 2, 2, 2, 2, 2, 2, 2, 2, 2, 2, 2, 2, 2, 2, 2, 2, 2, 2, 2, 2, 2, 2, 2, 2, 2, 2, 2, 2, 2, 2, 2, 2, 2, 2, 2, 2, 2, 2, 2, 2, 2, 2, 2, 2, 2, 2, 2, 2, 2, 2, 2, 2, 2, 2, 2, 2, 2, 2, 2, 2, 2, 2, 2, 2, 2, 2, 2, 2, 2, 2, 2, 2, 2, 2, 2, 2, 2, 2, 2, 2, 2, 2, 2, 2, 2, 2, 2, 2, 2, 2, 2, 2, 2, 2, 2, 2, 2, 2, 2, 2, 2, 2, 2, 2, 2, 2, 2, 2, 2, 2, 2, 2, 2, 2, 2, 2, 2, 2, 2, 2, 2, 2, 2, 2, 2, 2, 2, 2, 2, 2, 2, 2, 2, 2, 2, 2, 2, 2, 2, 2, 3 ),
 ( 0.000000000000000000, 1.000000000000000000 ),
 ( 0.000000000000000000, 0.005952380952380952051, 0.01190476190476190410, 0.01785714285714285615, 0.02380952380952380820, 0.02976190476190476025, 0.03571428571428571230, 0.04166666666666666435, 0.04761904761904761640, 0.05357142857142856845, 0.05952380952380952051, 0.06547619047619047949, 0.07142857142857142461, 0.07738095238095238360, 0.08333333333333332871, 0.08928571428571428770, 0.09523809523809523281, 0.1011904761904761918, 0.1071428571428571369, 0.1130952380952380959, 0.1190476190476190410, 0.1250000000000000000, 0.1309523809523809590, 0.1369047619047619180, 0.1428571428571428492, 0.1488095238095238082, 0.1547619047619047672, 0.1607142857142857262, 0.1666666666666666574, 0.1726190476190476164, 0.1785714285714285754, 0.1845238095238095344, 0.1904761904761904656, 0.1964285714285714246, 0.2023809523809523836, 0.2083333333333333426, 0.2142857142857142738, 0.2202380952380952328, 0.2261904761904761918, 0.2321428571428571508, 0.2380952380952380820, 0.2440476190476190410, 0.2500000000000000000, 0.2559523809523809312, 0.2619047619047619180, 0.2678571428571428492, 0.2738095238095238360, 0.2797619047619047672, 0.2857142857142856984, 0.2916666666666666852, 0.2976190476190476164, 0.3035714285714285476, 0.3095238095238095344, 0.3154761904761904656, 0.3214285714285714524, 0.3273809523809523836, 0.3333333333333333148, 0.3392857142857143016, 0.3452380952380952328, 0.3511904761904761640, 0.3571428571428571508, 0.3630952380952380820, 0.3690476190476190688, 0.3750000000000000000, 0.3809523809523809312, 0.3869047619047619180, 0.3928571428571428492, 0.3988095238095238360, 0.4047619047619047672, 0.4107142857142856984, 0.4166666666666666852, 0.4226190476190476164, 0.4285714285714285476, 0.4345238095238095344, 0.4404761904761904656, 0.4464285714285714524, 0.4523809523809523836, 0.4583333333333333148, 0.4642857142857143016, 0.4702380952380952328, 0.4761904761904761640, 0.4821428571428571508, 0.4880952380952380820, 0.4940476190476190688, 0.5000000000000000000, 0.5059523809523809312, 0.5119047619047618625, 0.5178571428571429047, 0.5238095238095238360, 0.5297619047619047672, 0.5357142857142856984, 0.5416666666666666297, 0.5476190476190476719, 0.5535714285714286031, 0.5595238095238095344, 0.5654761904761904656, 0.5714285714285713969, 0.5773809523809523281, 0.5833333333333333703, 0.5892857142857143016, 0.5952380952380952328, 0.6011904761904761640, 0.6071428571428570953, 0.6130952380952381375, 0.6190476190476190688, 0.6250000000000000000, 0.6309523809523809312, 0.6369047619047618625, 0.6428571428571429047, 0.6488095238095238360, 0.6547619047619047672, 0.6607142857142856984, 0.6666666666666666297, 0.6726190476190476719, 0.6785714285714286031, 0.6845238095238095344, 0.6904761904761904656, 0.6964285714285713969, 0.7023809523809523281, 0.7083333333333333703, 0.7142857142857143016, 0.7202380952380952328, 0.7261904761904761640, 0.7321428571428570953, 0.7380952380952381375, 0.7440476190476190688, 0.7500000000000000000, 0.7559523809523809312, 0.7619047619047618625, 0.7678571428571429047, 0.7738095238095238360, 0.7797619047619047672, 0.7857142857142856984, 0.7916666666666666297, 0.7976190476190476719, 0.8035714285714286031, 0.8095238095238095344, 0.8154761904761904656, 0.8214285714285713969, 0.8273809523809523281, 0.8333333333333333703, 0.8392857142857143016, 0.8452380952380952328, 0.8511904761904761640, 0.8571428571428570953, 0.8630952380952381375, 0.8690476190476190688, 0.8750000000000000000, 0.8809523809523809312, 0.8869047619047618625, 0.8928571428571429047, 0.8988095238095238360, 0.9047619047619047672, 0.9107142857142856984, 0.9166666666666666297, 0.9226190476190476719, 0.9285714285714286031, 0.9345238095238095344, 0.9404761904761904656, 0.9464285714285713969, 0.9523809523809523281, 0.9583333333333333703, 0.9642857142857143016 ),
 .UNSPECIFIED. ) 
 GEOMETRIC_REPRESENTATION_ITEM ( )  RATIONAL_B_SPLINE_SURFACE ( (
 ( 1.000000000000000000, 0.9659258262890683122, 1.000000000000000000, 0.9659258262890683122, 1.000000000000000000, 0.9659258262890683122, 1.000000000000000000, 0.9659258262890683122, 1.000000000000000000, 0.9659258262890683122, 1.000000000000000000, 0.9659258262890683122, 1.000000000000000000, 0.9659258262890683122, 1.000000000000000000, 0.9659258262890683122, 1.000000000000000000, 0.9659258262890683122, 1.000000000000000000, 0.9659258262890683122, 1.000000000000000000, 0.9659258262890683122, 1.000000000000000000, 0.9659258262890683122, 1.000000000000000000, 0.9659258262890683122, 1.000000000000000000, 0.9659258262890683122, 1.000000000000000000, 0.9659258262890683122, 1.000000000000000000, 0.9659258262890683122, 1.000000000000000000, 0.9659258262890683122, 1.000000000000000000, 0.9659258262890683122, 1.000000000000000000, 0.9659258262890683122, 1.000000000000000000, 0.9659258262890683122, 1.000000000000000000, 0.9659258262890683122, 1.000000000000000000, 0.9659258262890683122, 1.000000000000000000, 0.9659258262890683122, 1.000000000000000000, 0.9659258262890683122, 1.000000000000000000, 0.9659258262890683122, 1.000000000000000000, 0.9659258262890683122, 1.000000000000000000, 0.9659258262890683122, 1.000000000000000000, 0.9659258262890683122, 1.000000000000000000, 0.9659258262890683122, 1.000000000000000000, 0.9659258262890683122, 1.000000000000000000, 0.9659258262890683122, 1.000000000000000000, 0.9659258262890683122, 1.000000000000000000, 0.9659258262890683122, 1.000000000000000000, 0.9659258262890683122, 1.000000000000000000, 0.9659258262890683122, 1.000000000000000000, 0.9659258262890683122, 1.000000000000000000, 0.9659258262890683122, 1.000000000000000000, 0.9659258262890683122, 1.000000000000000000, 0.9659258262890683122, 1.000000000000000000, 0.9659258262890683122, 1.000000000000000000, 0.9659258262890683122, 1.000000000000000000, 0.9659258262890683122, 1.000000000000000000, 0.9659258262890683122, 1.000000000000000000, 0.9659258262890683122, 1.000000000000000000, 0.9659258262890683122, 1.000000000000000000, 0.9659258262890683122, 1.000000000000000000, 0.9659258262890683122, 1.000000000000000000, 0.9659258262890683122, 1.000000000000000000, 0.9659258262890683122, 1.000000000000000000, 0.9659258262890683122, 1.000000000000000000, 0.9659258262890683122, 1.000000000000000000, 0.9659258262890683122, 1.000000000000000000, 0.9659258262890683122, 1.000000000000000000, 0.9659258262890683122, 1.000000000000000000, 0.9659258262890683122, 1.000000000000000000, 0.9659258262890683122, 1.000000000000000000, 0.9659258262890683122, 1.000000000000000000, 0.9659258262890683122, 1.000000000000000000, 0.9659258262890683122, 1.000000000000000000, 0.9659258262890683122, 1.000000000000000000, 0.9659258262890683122, 1.000000000000000000, 0.9659258262890683122, 1.000000000000000000, 0.9659258262890683122, 1.000000000000000000, 0.9659258262890683122, 1.000000000000000000, 0.9659258262890683122, 1.000000000000000000, 0.9659258262890683122, 1.000000000000000000, 0.9659258262890683122, 1.000000000000000000, 0.9659258262890683122, 1.000000000000000000, 0.9659258262890683122, 1.000000000000000000, 0.9659258262890683122, 1.000000000000000000, 0.9659258262890683122, 1.000000000000000000, 0.9659258262890683122, 1.000000000000000000, 0.9659258262890683122, 1.000000000000000000, 0.9659258262890683122, 1.000000000000000000, 0.9659258262890683122, 1.000000000000000000, 0.9659258262890683122, 1.000000000000000000, 0.9659258262890683122, 1.000000000000000000, 0.9659258262890683122, 1.000000000000000000, 0.9659258262890683122, 1.000000000000000000, 0.9659258262890683122, 1.000000000000000000, 0.9659258262890683122, 1.000000000000000000, 0.9659258262890683122, 1.000000000000000000, 0.9659258262890683122, 1.000000000000000000, 0.9659258262890683122, 1.000000000000000000, 0.9659258262890683122, 1.000000000000000000, 0.9659258262890683122, 1.000000000000000000, 0.9659258262890683122, 1.000000000000000000, 0.9659258262890683122, 1.000000000000000000, 0.9659258262890683122, 1.000000000000000000, 0.9659258262890683122, 1.000000000000000000, 0.9659258262890683122, 1.000000000000000000, 0.9659258262890683122, 1.000000000000000000, 0.9659258262890683122, 1.000000000000000000, 0.9659258262890683122, 1.000000000000000000, 0.9659258262890683122, 1.000000000000000000, 0.9659258262890683122, 1.000000000000000000, 0.9659258262890683122, 1.000000000000000000, 0.9659258262890683122, 1.000000000000000000, 0.9659258262890683122, 1.000000000000000000, 0.9659258262890683122, 1.000000000000000000, 0.9659258262890683122, 1.000000000000000000, 0.9659258262890683122, 1.000000000000000000, 0.9659258262890683122, 1.000000000000000000, 0.9659258262890683122, 1.000000000000000000, 0.9659258262890683122, 1.000000000000000000, 0.9659258262890683122, 1.000000000000000000, 0.9659258262890683122, 1.000000000000000000, 0.9659258262890683122, 1.000000000000000000, 0.9659258262890683122, 1.000000000000000000, 0.9659258262890683122, 1.000000000000000000, 0.9659258262890683122, 1.000000000000000000, 0.9659258262890683122, 1.000000000000000000, 0.9659258262890683122, 1.000000000000000000, 0.9659258262890683122, 1.000000000000000000, 0.9659258262890683122, 1.000000000000000000, 0.9659258262890683122, 1.000000000000000000, 0.9659258262890683122, 1.000000000000000000, 0.9659258262890683122, 1.000000000000000000, 0.9659258262890683122, 1.000000000000000000, 0.9659258262890683122, 1.000000000000000000, 0.9659258262890683122, 1.000000000000000000, 0.9659258262890683122, 1.000000000000000000, 0.9659258262890683122, 1.000000000000000000, 0.9659258262890683122, 1.000000000000000000, 0.9659258262890683122, 1.000000000000000000, 0.9659258262890683122, 1.000000000000000000, 0.9659258262890683122, 1.000000000000000000, 0.9659258262890683122, 1.000000000000000000, 0.9659258262890683122, 1.000000000000000000, 0.9659258262890683122, 1.000000000000000000, 0.9659258262890683122, 1.000000000000000000, 0.9659258262890683122, 1.000000000000000000, 0.9659258262890683122, 1.000000000000000000, 0.9659258262890683122, 1.000000000000000000, 0.9659258262890683122, 1.000000000000000000, 0.9659258262890683122, 1.000000000000000000, 0.9659258262890683122, 1.000000000000000000, 0.9659258262890683122, 1.000000000000000000, 0.9659258262890683122, 1.000000000000000000, 0.9659258262890683122, 1.000000000000000000, 0.9659258262890683122, 1.000000000000000000, 0.9659258262890683122, 1.000000000000000000, 0.9659258262890683122, 1.000000000000000000, 0.9659258262890683122, 1.000000000000000000, 0.9659258262890683122, 1.000000000000000000, 0.9659258262890683122, 1.000000000000000000, 0.9659258262890683122, 1.000000000000000000, 0.9659258262890683122, 1.000000000000000000, 0.9659258262890683122, 1.000000000000000000, 0.9659258262890683122, 1.000000000000000000, 0.9659258262890683122, 1.000000000000000000, 0.9659258262890683122, 1.000000000000000000, 0.9659258262890683122, 1.000000000000000000, 0.9659258262890683122, 1.000000000000000000, 0.9659258262890683122, 1.000000000000000000, 0.9659258262890683122, 1.000000000000000000, 0.9659258262890683122, 1.000000000000000000, 0.9659258262890683122, 1.000000000000000000, 0.9659258262890683122, 1.000000000000000000, 0.9659258262890683122, 1.000000000000000000, 0.9659258262890683122, 1.000000000000000000, 0.9659258262890683122, 1.000000000000000000),
 ( 1.000000000000000000, 0.9659258262890683122, 1.000000000000000000, 0.9659258262890683122, 1.000000000000000000, 0.9659258262890683122, 1.000000000000000000, 0.9659258262890683122, 1.000000000000000000, 0.9659258262890683122, 1.000000000000000000, 0.9659258262890683122, 1.000000000000000000, 0.9659258262890683122, 1.000000000000000000, 0.9659258262890683122, 1.000000000000000000, 0.9659258262890683122, 1.000000000000000000, 0.9659258262890683122, 1.000000000000000000, 0.9659258262890683122, 1.000000000000000000, 0.9659258262890683122, 1.000000000000000000, 0.9659258262890683122, 1.000000000000000000, 0.9659258262890683122, 1.000000000000000000, 0.9659258262890683122, 1.000000000000000000, 0.9659258262890683122, 1.000000000000000000, 0.9659258262890683122, 1.000000000000000000, 0.9659258262890683122, 1.000000000000000000, 0.9659258262890683122, 1.000000000000000000, 0.9659258262890683122, 1.000000000000000000, 0.9659258262890683122, 1.000000000000000000, 0.9659258262890683122, 1.000000000000000000, 0.9659258262890683122, 1.000000000000000000, 0.9659258262890683122, 1.000000000000000000, 0.9659258262890683122, 1.000000000000000000, 0.9659258262890683122, 1.000000000000000000, 0.9659258262890683122, 1.000000000000000000, 0.9659258262890683122, 1.000000000000000000, 0.9659258262890683122, 1.000000000000000000, 0.9659258262890683122, 1.000000000000000000, 0.9659258262890683122, 1.000000000000000000, 0.9659258262890683122, 1.000000000000000000, 0.9659258262890683122, 1.000000000000000000, 0.9659258262890683122, 1.000000000000000000, 0.9659258262890683122, 1.000000000000000000, 0.9659258262890683122, 1.000000000000000000, 0.9659258262890683122, 1.000000000000000000, 0.9659258262890683122, 1.000000000000000000, 0.9659258262890683122, 1.000000000000000000, 0.9659258262890683122, 1.000000000000000000, 0.9659258262890683122, 1.000000000000000000, 0.9659258262890683122, 1.000000000000000000, 0.9659258262890683122, 1.000000000000000000, 0.9659258262890683122, 1.000000000000000000, 0.9659258262890683122, 1.000000000000000000, 0.9659258262890683122, 1.000000000000000000, 0.9659258262890683122, 1.000000000000000000, 0.9659258262890683122, 1.000000000000000000, 0.9659258262890683122, 1.000000000000000000, 0.9659258262890683122, 1.000000000000000000, 0.9659258262890683122, 1.000000000000000000, 0.9659258262890683122, 1.000000000000000000, 0.9659258262890683122, 1.000000000000000000, 0.9659258262890683122, 1.000000000000000000, 0.9659258262890683122, 1.000000000000000000, 0.9659258262890683122, 1.000000000000000000, 0.9659258262890683122, 1.000000000000000000, 0.9659258262890683122, 1.000000000000000000, 0.9659258262890683122, 1.000000000000000000, 0.9659258262890683122, 1.000000000000000000, 0.9659258262890683122, 1.000000000000000000, 0.9659258262890683122, 1.000000000000000000, 0.9659258262890683122, 1.000000000000000000, 0.9659258262890683122, 1.000000000000000000, 0.9659258262890683122, 1.000000000000000000, 0.9659258262890683122, 1.000000000000000000, 0.9659258262890683122, 1.000000000000000000, 0.9659258262890683122, 1.000000000000000000, 0.9659258262890683122, 1.000000000000000000, 0.9659258262890683122, 1.000000000000000000, 0.9659258262890683122, 1.000000000000000000, 0.9659258262890683122, 1.000000000000000000, 0.9659258262890683122, 1.000000000000000000, 0.9659258262890683122, 1.000000000000000000, 0.9659258262890683122, 1.000000000000000000, 0.9659258262890683122, 1.000000000000000000, 0.9659258262890683122, 1.000000000000000000, 0.9659258262890683122, 1.000000000000000000, 0.9659258262890683122, 1.000000000000000000, 0.9659258262890683122, 1.000000000000000000, 0.9659258262890683122, 1.000000000000000000, 0.9659258262890683122, 1.000000000000000000, 0.9659258262890683122, 1.000000000000000000, 0.9659258262890683122, 1.000000000000000000, 0.9659258262890683122, 1.000000000000000000, 0.9659258262890683122, 1.000000000000000000, 0.9659258262890683122, 1.000000000000000000, 0.9659258262890683122, 1.000000000000000000, 0.9659258262890683122, 1.000000000000000000, 0.9659258262890683122, 1.000000000000000000, 0.9659258262890683122, 1.000000000000000000, 0.9659258262890683122, 1.000000000000000000, 0.9659258262890683122, 1.000000000000000000, 0.9659258262890683122, 1.000000000000000000, 0.9659258262890683122, 1.000000000000000000, 0.9659258262890683122, 1.000000000000000000, 0.9659258262890683122, 1.000000000000000000, 0.9659258262890683122, 1.000000000000000000, 0.9659258262890683122, 1.000000000000000000, 0.9659258262890683122, 1.000000000000000000, 0.9659258262890683122, 1.000000000000000000, 0.9659258262890683122, 1.000000000000000000, 0.9659258262890683122, 1.000000000000000000, 0.9659258262890683122, 1.000000000000000000, 0.9659258262890683122, 1.000000000000000000, 0.9659258262890683122, 1.000000000000000000, 0.9659258262890683122, 1.000000000000000000, 0.9659258262890683122, 1.000000000000000000, 0.9659258262890683122, 1.000000000000000000, 0.9659258262890683122, 1.000000000000000000, 0.9659258262890683122, 1.000000000000000000, 0.9659258262890683122, 1.000000000000000000, 0.9659258262890683122, 1.000000000000000000, 0.9659258262890683122, 1.000000000000000000, 0.9659258262890683122, 1.000000000000000000, 0.9659258262890683122, 1.000000000000000000, 0.9659258262890683122, 1.000000000000000000, 0.9659258262890683122, 1.000000000000000000, 0.9659258262890683122, 1.000000000000000000, 0.9659258262890683122, 1.000000000000000000, 0.9659258262890683122, 1.000000000000000000, 0.9659258262890683122, 1.000000000000000000, 0.9659258262890683122, 1.000000000000000000, 0.9659258262890683122, 1.000000000000000000, 0.9659258262890683122, 1.000000000000000000, 0.9659258262890683122, 1.000000000000000000, 0.9659258262890683122, 1.000000000000000000, 0.9659258262890683122, 1.000000000000000000, 0.9659258262890683122, 1.000000000000000000, 0.9659258262890683122, 1.000000000000000000, 0.9659258262890683122, 1.000000000000000000, 0.9659258262890683122, 1.000000000000000000, 0.9659258262890683122, 1.000000000000000000, 0.9659258262890683122, 1.000000000000000000, 0.9659258262890683122, 1.000000000000000000, 0.9659258262890683122, 1.000000000000000000, 0.9659258262890683122, 1.000000000000000000, 0.9659258262890683122, 1.000000000000000000, 0.9659258262890683122, 1.000000000000000000, 0.9659258262890683122, 1.000000000000000000, 0.9659258262890683122, 1.000000000000000000, 0.9659258262890683122, 1.000000000000000000, 0.9659258262890683122, 1.000000000000000000, 0.9659258262890683122, 1.000000000000000000, 0.9659258262890683122, 1.000000000000000000, 0.9659258262890683122, 1.000000000000000000, 0.9659258262890683122, 1.000000000000000000, 0.9659258262890683122, 1.000000000000000000, 0.9659258262890683122, 1.000000000000000000, 0.9659258262890683122, 1.000000000000000000, 0.9659258262890683122, 1.000000000000000000, 0.9659258262890683122, 1.000000000000000000, 0.9659258262890683122, 1.000000000000000000, 0.9659258262890683122, 1.000000000000000000, 0.9659258262890683122, 1.000000000000000000, 0.9659258262890683122, 1.000000000000000000, 0.9659258262890683122, 1.000000000000000000, 0.9659258262890683122, 1.000000000000000000, 0.9659258262890683122, 1.000000000000000000, 0.9659258262890683122, 1.000000000000000000, 0.9659258262890683122, 1.000000000000000000, 0.9659258262890683122, 1.000000000000000000) ) ) 
 REPRESENTATION_ITEM ( '' )  SURFACE ( )  );
#23132 = CARTESIAN_POINT ( 'NONE',  ( 17.20831665107776587, 57.88393115100078745, 7.208316651077764980 ) ) ;
#23134 = CARTESIAN_POINT ( 'NONE',  ( 9.402796353261136275, 0.3639308891339645968, -11.68706210897760833 ) ) ;
#23133 = CARTESIAN_POINT ( 'NONE',  ( 7.084665262690076126, 9.105352010821503583, 10.88017736071109987 ) ) ;
#23135 = CARTESIAN_POINT ( 'NONE',  ( 13.43411237798105340, 15.58196800326374998, 12.81628187352647963 ) ) ;
#23136 = ORIENTED_EDGE ( 'NONE', *, *, #4848, .F. ) ;
#23137 = CARTESIAN_POINT ( 'NONE',  ( 12.91533473730993009, 41.60535201082149825, -10.88017736071109987 ) ) ;
#23139 = DIRECTION ( 'NONE',  ( 0.1478094111295981949, 0.000000000000000000, 0.9890158633619187123 ) ) ;
#23138 = CARTESIAN_POINT ( 'NONE',  ( 17.20831665107776587, 62.88393115100078745, 7.208316651077764980 ) ) ;
#23140 = CARTESIAN_POINT ( 'NONE',  ( 2.035157376598824452, 13.68868534415483751, 7.964842623401179544 ) ) ;
#23141 = CARTESIAN_POINT ( 'NONE',  ( 10.00000000000000000, 21.81368534415484106, -10.88017736071110342 ) ) ;
#23142 = CARTESIAN_POINT ( 'NONE',  ( -4.164238869374098151, 41.59541550158061796, -3.795296366450310543 ) ) ;
#23143 = CARTESIAN_POINT ( 'NONE',  ( 2.791683348922237240, 30.38393115100078390, -7.208316651077763204 ) ) ;
#23144 = CARTESIAN_POINT ( 'NONE',  ( 0.5774900079438607392, 53.48035201082151247, 5.440088680355550821 ) ) ;
#23145 = SURFACE_SIDE_STYLE ('',( #40105 ) ) ;
#23146 = CARTESIAN_POINT ( 'NONE',  ( -2.266590686148945544, 1.387082168247301128, -7.082119434687050408 ) ) ;
#23148 = ADVANCED_FACE ( 'NONE', ( #29672 ), #6206, .F. ) ;
#23147 =( GEOMETRIC_REPRESENTATION_CONTEXT ( 3 ) GLOBAL_UNCERTAINTY_ASSIGNED_CONTEXT ( ( #94316 ) ) GLOBAL_UNIT_ASSIGNED_CONTEXT ( ( #69164, #70148, #31139 ) ) REPRESENTATION_CONTEXT ( 'NONE', 'WORKASPACE' ) );
#23149 = PLANE ( 'NONE',  #28942 ) ;
#23150 = CARTESIAN_POINT ( 'NONE',  ( 17.20831665107776587, 54.13393115100079456, -7.208316651077762316 ) ) ;
#23151 = EDGE_LOOP ( 'NONE', ( #52189, #38969, #25874, #80178 ) ) ;
#23152 = VERTEX_POINT ( 'NONE', #59686 ) ;
#23153 = CARTESIAN_POINT ( 'NONE',  ( 6.204703633549690345, 35.76208216824729647, -14.16423886937410259 ) ) ;
#23154 = CARTESIAN_POINT ( 'NONE',  ( -2.266590686148945544, 17.22041550158063572, 7.082119434687048631 ) ) ;
#23155 = CARTESIAN_POINT ( 'NONE',  ( 12.63842701281683034, 2.467264484334118269, 9.846743663894596210 ) ) ;
#23156 = CARTESIAN_POINT ( 'NONE',  ( -1.099225684535947600, 8.706968003263753531, -6.408140936763238038 ) ) ;
#23157 = CARTESIAN_POINT ( 'NONE',  ( 5.428133280998944876, 0.000000000000000000, -0.5226697871167509390 ) ) ;
#23158 = CARTESIAN_POINT ( 'NONE',  ( -11.62541523590571657, -75.76371818141868175, 3.750000000000000000 ) ) ;
#23160 = CARTESIAN_POINT ( 'NONE',  ( 3.591859063236763294, 18.29030133659708568, -11.09922568453595026 ) ) ;
#23159 = CARTESIAN_POINT ( 'NONE',  ( 10.00000000000000000, 41.81368534415484106, -10.88017736071110342 ) ) ;
#23161 = CARTESIAN_POINT ( 'NONE',  ( -4.164238869374099927, 27.01208216824730357, 3.795296366450308767 ) ) ;
#23162 = CARTESIAN_POINT ( 'NONE',  ( 0.5774900079438607392, 18.48035201082150536, 5.440088680355550821 ) ) ;
#23163 = CARTESIAN_POINT ( 'NONE',  ( 20.88017736071110875, 25.77201867748816966, -2.915334737309920765 ) ) ;
#23164 = CARTESIAN_POINT ( 'NONE',  ( -9.065164099344649173, 14.63606892172464136, 11.95084933600763399 ) ) ;
#23165 = CARTESIAN_POINT ( 'NONE',  ( 4.559911319644449179, 53.89701867748817676, 9.422509992056141925 ) ) ;
#23166 = CARTESIAN_POINT ( 'NONE',  ( 22.81628187352648496, 51.83196800326376064, -3.434112377981050290 ) ) ;
#23167 = CARTESIAN_POINT ( 'NONE',  ( 2.638427012816829897, -20.44940218233254470, -9.846743663894592657 ) ) ;
#23168 = EDGE_LOOP ( 'NONE', ( #13376, #4583, #316, #82008, #75846, #4304 ) ) ;
#23169 = CARTESIAN_POINT ( 'NONE',  ( 10.00000000000000178, 70.00000000000000000, 0.000000000000000000 ) ) ;
#23170 = AXIS2_PLACEMENT_3D ( 'NONE', #77949, #1979, #8475 ) ;
#23171 = ORIENTED_EDGE ( 'NONE', *, *, #29581, .T. ) ;
#23172 = CARTESIAN_POINT ( 'NONE',  ( 34.56412365047463453, 13.99999999999999645, 9.500000000000000000 ) ) ;
#23173 = VERTEX_POINT ( 'NONE', #67199 ) ;
#23175 = CARTESIAN_POINT ( 'NONE',  ( -0.3689425029237881626, 62.42874883491396787, 10.36894250292379027 ) ) ;
#23174 = CARTESIAN_POINT ( 'NONE',  ( 6.204703633549690345, 60.76208216824730357, -14.16423886937410259 ) ) ;
#23177 = CARTESIAN_POINT ( 'NONE',  ( 10.00000000000000000, 64.75893115100078035, -9.846743663894594434 ) ) ;
#23176 = CARTESIAN_POINT ( 'NONE',  ( 14.92337183194729633, 27.67559781766745530, 8.527530157486181039 ) ) ;
#23178 = CARTESIAN_POINT ( 'NONE',  ( 0.000000000000000000, 15.00000000000000000, 0.000000000000000000 ) ) ;
#23179 = DIRECTION ( 'NONE',  ( 1.049065152435176504E-16, -1.000000000000000000, 0.000000000000000000 ) ) ;
#23180 = ADVANCED_FACE ( 'NONE', ( #20718 ), #44688, .T. ) ;
#23181 = CARTESIAN_POINT ( 'NONE',  ( 0.6178305044545818747, 3.498634669930420049, -9.382169495545419124 ) ) ;
#23182 = CARTESIAN_POINT ( 'NONE',  ( 12.81628187352647608, 26.41530133659709989, 3.434112377981052511 ) ) ;
#23183 = EDGE_CURVE ( 'NONE', #88041, #97822, #75183, .T. ) ;
#23184 = ORIENTED_EDGE ( 'NONE', *, *, #67276, .T. ) ;
#23185 = CARTESIAN_POINT ( 'NONE',  ( -4.164238869374099927, 27.01208216824730357, 3.795296366450308767 ) ) ;
#23186 = ORIENTED_EDGE ( 'NONE', *, *, #6708, .T. ) ;
#23187 = CARTESIAN_POINT ( 'NONE',  ( 6.204703633549690345, 47.84541550158064638, 14.16423886937410082 ) ) ;
#23188 = ORIENTED_EDGE ( 'NONE', *, *, #90448, .T. ) ;
#23189 = CARTESIAN_POINT ( 'NONE',  ( 6.565887622018943937, 63.08196800326376064, -12.81628187352647608 ) ) ;
#23190 = CARTESIAN_POINT ( 'NONE',  ( 17.96484262340118221, 29.93868534415484106, 7.964842623401181321 ) ) ;
#23191 = CARTESIAN_POINT ( 'NONE',  ( 5.076628168052703671, 51.84226448433412315, 8.527530157486179263 ) ) ;
#23192 = CARTESIAN_POINT ( 'NONE',  ( 20.88017736071110875, 25.77201867748816966, -2.915334737309920765 ) ) ;
#23193 = CARTESIAN_POINT ( 'NONE',  ( 13.99999999999999822, 61.50000000000000711, 6.500000000000000888 ) ) ;
#23194 = CARTESIAN_POINT ( 'NONE',  ( -5.780262629516634831, -39.80185923444031459, 2.499999999999999556 ) ) ;
#23195 = CARTESIAN_POINT ( 'NONE',  ( 0.1532563361054082862, 56.21726448433411605, 2.638427012816831674 ) ) ;
#23196 = CARTESIAN_POINT ( 'NONE',  ( 12.63842701281683922, 49.55059781766744464, -9.846743663894590881 ) ) ;
#23197 = CARTESIAN_POINT ( 'NONE',  ( -3.897244926436316703, 15.00000000000000000, 13.96644127841325300 ) ) ;
#23198 = DIRECTION ( 'NONE',  ( -0.000000000000000000, -0.000000000000000000, -1.000000000000000000 ) ) ;
#23199 = CARTESIAN_POINT ( 'NONE',  ( 10.00000000000000000, -0.2410688489992152128, -9.846743663894594434 ) ) ;
#23200 = CARTESIAN_POINT ( 'NONE',  ( -9.065164099344400483, 0.3639310782753642504, -11.95084933600781341 ) ) ;
#23201 = ORIENTED_EDGE ( 'NONE', *, *, #71865, .T. ) ;
#23202 = CARTESIAN_POINT ( 'NONE',  ( 10.19513985507835763, 14.49999999999999112, -11.00268709613223450 ) ) ;
#23203 = CARTESIAN_POINT ( 'NONE',  ( 14.92337183194729633, 32.67559781766745175, 8.527530157486181039 ) ) ;
#23204 = DIRECTION ( 'NONE',  ( 3.552713678800500929E-14, 0.000000000000000000, 1.000000000000000000 ) ) ;
#23205 = CARTESIAN_POINT ( 'NONE',  ( 3.591859063236761518, 39.95696800326375353, 11.09922568453594849 ) ) ;
#23206 = CARTESIAN_POINT ( 'NONE',  ( 10.00000000000000178, 0.000000000000000000, 0.000000000000000000 ) ) ;
#23207 = EDGE_CURVE ( 'NONE', #62480, #29582, #52683, .T. ) ;
#23208 = DIRECTION ( 'NONE',  ( -1.000000000000000000, 0.000000000000000000, 0.000000000000000000 ) ) ;
#23209 = ORIENTED_EDGE ( 'NONE', *, *, #8322, .F. ) ;
#23210 = PLANE ( 'NONE',  #25260 ) ;
#23211 = FACE_OUTER_BOUND ( 'NONE', #12420, .T. ) ;
#23212 = CARTESIAN_POINT ( 'NONE',  ( 2.791683348922237240, 55.38393115100078745, -7.208316651077763204 ) ) ;
#23213 = CARTESIAN_POINT ( 'NONE',  ( 17.08211943468705840, 35.13708216824730357, -12.26659068614894466 ) ) ;
#23214 = CARTESIAN_POINT ( 'NONE',  ( 14.92337183194729988, 59.34226448433412315, -8.527530157486177487 ) ) ;
#23215 = CARTESIAN_POINT ( 'NONE',  ( -14.03351048042399007, 0.000000000000000000, 2.474486531753619989 ) ) ;
#23216 = CARTESIAN_POINT ( 'NONE',  ( 18.52753015748618282, 3.925597817667451306, -4.923371831947291888 ) ) ;
#23217 = CARTESIAN_POINT ( 'NONE',  ( 19.38216949554541557, 47.24863466993041783, -9.382169495545420901 ) ) ;
#23218 = VECTOR ( 'NONE', #63283, 1000.000000000000000 ) ;
#23219 = CARTESIAN_POINT ( 'NONE',  ( 18.52753015748618282, 48.92559781766745886, -4.923371831947291888 ) ) ;
#23220 = CARTESIAN_POINT ( 'NONE',  ( 12.91533473730993009, 56.60535201082151247, -10.88017736071109987 ) ) ;
#23221 = CARTESIAN_POINT ( 'NONE',  ( 17.20831665107776587, 47.88393115100078745, 7.208316651077764980 ) ) ;
#23222 = PRODUCT_CONTEXT ( 'NONE', #26983, 'mechanical' ) ;
#23223 = CARTESIAN_POINT ( 'NONE',  ( 0.9082943533637201083, 4.650128654361622927E-16, -14.47152380945585115 ) ) ;
#23224 = AXIS2_PLACEMENT_3D ( 'NONE', #1739, #48186, #70714 ) ;
#23225 = CARTESIAN_POINT ( 'NONE',  ( 4.559911319644449179, 57.23035201082150536, -9.422509992056141925 ) ) ;
#23226 = ORIENTED_EDGE ( 'NONE', *, *, #86995, .F. ) ;
#23227 = DIRECTION ( 'NONE',  ( -0.000000000000000000, -1.000000000000000000, -0.000000000000000000 ) ) ;
#23228 = CARTESIAN_POINT ( 'NONE',  ( 4.559911319644449179, 28.89701867748817321, 9.422509992056141925 ) ) ;
#23230 = CARTESIAN_POINT ( 'NONE',  ( -0.8801773607110991993, 52.85535201082151247, -2.915334737309923874 ) ) ;
#23229 = CARTESIAN_POINT ( 'NONE',  ( -2.816281873526471635, -1.084698663402913210, -3.434112377981056508 ) ) ;
#23231 = CARTESIAN_POINT ( 'NONE',  ( -14.94699059465099822, 15.00000000000000000, -1.259949270175015013 ) ) ;
#23232 = CARTESIAN_POINT ( 'NONE',  ( 17.39651004071842166, 12.93575266056827822, 6.499999999999998224 ) ) ;
#23233 =( NAMED_UNIT ( * ) PLANE_ANGLE_UNIT ( ) SI_UNIT ( $, .RADIAN. ) );
#23235 = LINE ( 'NONE', #59727, #74333 ) ;
#23234 = CARTESIAN_POINT ( 'NONE',  ( 20.88017736071110164, 40.35535201082150536, 2.915334737309930979 ) ) ;
#23236 = CARTESIAN_POINT ( 'NONE',  ( 17.20831665107776587, 17.88393115100078745, 7.208316651077764980 ) ) ;
#23237 = AXIS2_PLACEMENT_3D ( 'NONE', #81475, #50491, #42028 ) ;
#23238 = CARTESIAN_POINT ( 'NONE',  ( 0.1532563361054082862, 41.21726448433411605, 2.638427012816831674 ) ) ;
#23239 = FACE_OUTER_BOUND ( 'NONE', #6650, .T. ) ;
#23240 = CARTESIAN_POINT ( 'NONE',  ( -14.16423886937410437, 16.59541550158064283, -3.795296366450299885 ) ) ;
#23241 = CARTESIAN_POINT ( 'NONE',  ( 19.84674366389459621, 58.50893115100078745, 7.409399052514197653E-17 ) ) ;
#23242 = CARTESIAN_POINT ( 'NONE',  ( 10.00000000000000178, 63.05374883491396076, 14.16423886937410082 ) ) ;
#23243 = PLANE ( 'NONE',  #45260 ) ;
#23244 = CARTESIAN_POINT ( 'NONE',  ( 20.36894250292379738, 19.92874883491396787, -10.36894250292379027 ) ) ;
#23245 = CARTESIAN_POINT ( 'NONE',  ( 24.16423886937410614, 49.30374883491396787, 8.672049930838204340E-16 ) ) ;
#23246 = AXIS2_PLACEMENT_3D ( 'NONE', #48957, #62478, #1528 ) ;
#23247 = CARTESIAN_POINT ( 'NONE',  ( 19.84674366389459621, 28.50893115100078745, 7.409399052514197653E-17 ) ) ;
#23248 = CARTESIAN_POINT ( 'NONE',  ( 18.52753015748617571, 13.09226448433411960, 4.923371831947298993 ) ) ;
#23249 = CARTESIAN_POINT ( 'NONE',  ( 19.42250999205614193, 5.147018677488171434, 5.440088680355555262 ) ) ;
#23250 = ORIENTED_EDGE ( 'NONE', *, *, #82865, .F. ) ;
#23251 = CARTESIAN_POINT ( 'NONE',  ( 0.1532563361054100626, 30.80059781766744820, -2.638427012816831230 ) ) ;
#23252 = CARTESIAN_POINT ( 'NONE',  ( 15.44008868035555260, 29.73035201082150891, 9.422509992056143702 ) ) ;
#23253 = CARTESIAN_POINT ( 'NONE',  ( 0.1532563361054082862, 61.21726448433412315, 2.638427012816831674 ) ) ;
#23255 = FILL_AREA_STYLE ('',( #22753 ) ) ;
#23254 = CARTESIAN_POINT ( 'NONE',  ( 24.16423886937410614, 4.303748834913967869, 8.672049930838204340E-16 ) ) ;
#23256 = PLANE ( 'NONE',  #34389 ) ;
#23257 = CARTESIAN_POINT ( 'NONE',  ( 1.472469842513823179, 6.425597817667451750, 4.923371831947296329 ) ) ;
#23258 = CARTESIAN_POINT ( 'NONE',  ( 21.09922568453594849, 41.20696800326375353, 6.408140936763242479 ) ) ;
#23259 = CARTESIAN_POINT ( 'NONE',  ( 2.791683348922240793, 36.63393115100078035, 7.208316651077764092 ) ) ;
#23260 = ORIENTED_EDGE ( 'NONE', *, *, #23797, .F. ) ;
#23261 = CARTESIAN_POINT ( 'NONE',  ( 19.84674366389459266, 23.30059781766745530, 2.638427012816836559 ) ) ;
#23262 = CARTESIAN_POINT ( 'NONE',  ( 10.34945593949844600, -32.01313548011462018, -4.000000000000000000 ) ) ;
#23263 = CARTESIAN_POINT ( 'NONE',  ( 20.36894250292379382, 58.67874883491396076, 10.36894250292379205 ) ) ;
#23264 = CARTESIAN_POINT ( 'NONE',  ( 0.5774900079438590739, 52.64701867748817676, -5.440088680355550821 ) ) ;
#23265 =( LENGTH_UNIT ( ) NAMED_UNIT ( * ) SI_UNIT ( .MILLI., .METRE. ) );
#23266 = CARTESIAN_POINT ( 'NONE',  ( 12.63842701281683034, 37.46726448433411605, 9.846743663894596210 ) ) ;
#23267 = CARTESIAN_POINT ( 'NONE',  ( 15.44008868035555260, 9.730352010821505360, 9.422509992056143702 ) ) ;
#23268 = CARTESIAN_POINT ( 'NONE',  ( 18.52753015748617571, 38.09226448433412315, 4.923371831947298993 ) ) ;
#23269 = CARTESIAN_POINT ( 'NONE',  ( 17.84635730667654840, 38.63791097397319163, 6.500000000000047073 ) ) ;
#23270 = CARTESIAN_POINT ( 'NONE',  ( 2.791683348922237240, 45.38393115100079456, -7.208316651077763204 ) ) ;
#23271 = ADVANCED_FACE ( 'NONE', ( #37214 ), #44186, .F. ) ;
#23272 = CARTESIAN_POINT ( 'NONE',  ( 4.559911319644449179, 48.89701867748817676, 9.422509992056141925 ) ) ;
#23273 = UNCERTAINTY_MEASURE_WITH_UNIT (LENGTH_MEASURE( 1.000000000000000082E-05 ), #6774, 'distance_accuracy_value', 'NONE');
#23274 = ORIENTED_EDGE ( 'NONE', *, *, #72107, .F. ) ;
#23275 = VERTEX_POINT ( 'NONE', #59190 ) ;
#23276 = CARTESIAN_POINT ( 'NONE',  ( -14.97687855664612577, 0.3639309658595348829, 0.8325315005899682763 ) ) ;
#23277 = CIRCLE ( 'NONE', #39259, 15.00000000000000000 ) ;
#23278 = DIRECTION ( 'NONE',  ( 0.000000000000000000, -0.000000000000000000, -1.000000000000000000 ) ) ;
#23279 = CARTESIAN_POINT ( 'NONE',  ( 17.20831665107776587, 2.883931151000785231, 7.208316651077764980 ) ) ;
#23280 = CARTESIAN_POINT ( 'NONE',  ( 10.00000000000000000, 57.87363466993042493, -12.81628187352647608 ) ) ;
#23282 = CARTESIAN_POINT ( 'NONE',  ( 0.1532563361054083140, 51.00893115100078745, 1.131784320476157264E-15 ) ) ;
#23281 = CARTESIAN_POINT ( 'NONE',  ( 0.5774900079438590739, 2.647018677488171434, -5.440088680355550821 ) ) ;
#23283 = CARTESIAN_POINT ( 'NONE',  ( 10.84451454130507209, 4.631809541732465460E-16, -9.625305416630832056 ) ) ;
#23284 = CARTESIAN_POINT ( 'NONE',  ( -2.266590686148945544, 31.38708216824730002, -7.082119434687050408 ) ) ;
#23285 = CARTESIAN_POINT ( 'NONE',  ( 24.16423886937410614, 64.30374883491396076, 8.672049930838204340E-16 ) ) ;
#23286 = CARTESIAN_POINT ( 'NONE',  ( 2.791683348922240793, 51.63393115100078745, 7.208316651077764092 ) ) ;
#23287 = LINE ( 'NONE', #53765, #61855 ) ;
#23288 = CARTESIAN_POINT ( 'NONE',  ( 10.00000000000000178, 49.31368534415484106, 10.88017736071110342 ) ) ;
#23289 = CARTESIAN_POINT ( 'NONE',  ( 4.559911319644449179, 67.23035201082150536, -9.422509992056141925 ) ) ;
#23290 = SURFACE_SIDE_STYLE ('',( #7296 ) ) ;
#23291 = VERTEX_POINT ( 'NONE', #75681 ) ;
#23292 = B_SPLINE_CURVE_WITH_KNOTS ( 'NONE', 3,
 ( #90115, #97163, #21642, #42175, #50146, #28631 ),
 .UNSPECIFIED., .F., .F.,
 ( 4, 2, 4 ),
 ( 0.0002800008091676911060, 0.0006862060465022900516, 0.001092411283836889051 ),
 .UNSPECIFIED. ) ;
#23293 = CARTESIAN_POINT ( 'NONE',  ( 21.09922568453594849, 56.20696800326375353, 6.408140936763242479 ) ) ;
#23294 = CARTESIAN_POINT ( 'NONE',  ( 14.92337183194729988, 9.342264484334119601, -8.527530157486177487 ) ) ;
#23295 = VERTEX_POINT ( 'NONE', #7195 ) ;
#23296 = AXIS2_PLACEMENT_3D ( 'NONE', #76221, #45719, #7734 ) ;
#23297 = CARTESIAN_POINT ( 'NONE',  ( 10.00000000000000000, 20.55374883491396787, -14.16423886937410082 ) ) ;
#23298 = CARTESIAN_POINT ( 'NONE',  ( 18.52753015748617571, 18.09226448433411960, 4.923371831947298993 ) ) ;
#23299 = CARTESIAN_POINT ( 'NONE',  ( 12.91533473730993009, 31.60535201082150891, -10.88017736071109987 ) ) ;
#23300 = LINE ( 'NONE', #68302, #34550 ) ;
#23301 = ORIENTED_EDGE ( 'NONE', *, *, #15078, .T. ) ;
#23302 = CARTESIAN_POINT ( 'NONE',  ( 10.00000000000000000, 21.81368534415484106, -10.88017736071110342 ) ) ;
#23303 = EDGE_CURVE ( 'NONE', #37161, #30649, #41623, .T. ) ;
#23304 = AXIS2_PLACEMENT_3D ( 'NONE', #32342, #78340, #25845 ) ;
#23305 = ADVANCED_FACE ( 'NONE', ( #68196 ), #98717, .F. ) ;
#23306 = EDGE_LOOP ( 'NONE', ( #11193, #54128, #14522, #80202 ) ) ;
#23307 = CARTESIAN_POINT ( 'NONE',  ( 19.42250999205614548, 35.98035201082151247, -5.440088680355545492 ) ) ;
#23308 = SURFACE_SIDE_STYLE ('',( #53285 ) ) ;
#23309 = ORIENTED_EDGE ( 'NONE', *, *, #58713, .T. ) ;
#23310 = CARTESIAN_POINT ( 'NONE',  ( 19.38216949554541202, 15.99863466993042138, 9.382169495545424454 ) ) ;
#23311 = CARTESIAN_POINT ( 'NONE',  ( 14.92337183194729633, 7.675597817667451750, 8.527530157486181039 ) ) ;
#23312 = CARTESIAN_POINT ( 'NONE',  ( 13.75801628063878645, 4.006593314786880238E-16, 4.578972376164555769 ) ) ;
#23313 = CARTESIAN_POINT ( 'NONE',  ( 17.20831665107776587, 22.88393115100078745, 7.208316651077764980 ) ) ;
#23314 = CARTESIAN_POINT ( 'NONE',  ( 7.084665262690076126, 34.10535201082151247, 10.88017736071109987 ) ) ;
#23315 = CIRCLE ( 'NONE', #26495, 62.50000000000000000 ) ;
#23316 = AXIS2_PLACEMENT_3D ( 'NONE', #87333, #11335, #41854 ) ;
#23317 = CIRCLE ( 'NONE', #98340, 14.49999999999999822 ) ;
#23318 = VERTEX_POINT ( 'NONE', #22699 ) ;
#23319 = CARTESIAN_POINT ( 'NONE',  ( 3.591859063236763294, 63.29030133659708923, -11.09922568453595026 ) ) ;
#23320 = CARTESIAN_POINT ( 'NONE',  ( 17.96484262340118221, 51.18868534415483396, -7.964842623401177768 ) ) ;
#23321 = DIRECTION ( 'NONE',  ( -0.8038568606172125097, 0.000000000000000000, -0.5948227867513478095 ) ) ;
#23322 = AXIS2_PLACEMENT_3D ( 'NONE', #73700, #13705, #65211 ) ;
#23323 = CARTESIAN_POINT ( 'NONE',  ( 0.6178305044545838731, 59.74863466993041783, 9.382169495545420901 ) ) ;
#23324 = CARTESIAN_POINT ( 'NONE',  ( 20.88017736071110519, 65.56368534415483396, 2.639326808657452039E-16 ) ) ;
#23325 = CARTESIAN_POINT ( 'NONE',  ( -1.099225684535947600, 4.540301336597087456, 6.408140936763237150 ) ) ;
#23326 = PLANE ( 'NONE',  #24327 ) ;
#23327 = CARTESIAN_POINT ( 'NONE',  ( 2.791683348922240793, 31.63393115100078745, 7.208316651077764092 ) ) ;
#23328 = CARTESIAN_POINT ( 'NONE',  ( -1.099225684535947600, 48.70696800326375353, -6.408140936763238038 ) ) ;
#23329 = DIRECTION ( 'NONE',  ( 0.000000000000000000, 1.000000000000000000, 0.000000000000000000 ) ) ;
#23330 = CARTESIAN_POINT ( 'NONE',  ( 17.20831665107776587, 24.13393115100078035, -7.208316651077762316 ) ) ;
#23331 = CARTESIAN_POINT ( 'NONE',  ( 16.40814093676324603, 17.45696800326375353, -11.09922568453594671 ) ) ;
#23333 = CARTESIAN_POINT ( 'NONE',  ( -3.521970974752482331, -0.8418515890118015710, -2.749999999999999556 ) ) ;
#23332 = PRESENTATION_STYLE_ASSIGNMENT (( #82820 ) ) ;
#23334 = CARTESIAN_POINT ( 'NONE',  ( 12.91533473730993009, 36.60535201082151247, -10.88017736071109987 ) ) ;
#23335 = CARTESIAN_POINT ( 'NONE',  ( 7.361572987183169658, 64.96726448433412315, -9.846743663894592657 ) ) ;
#23336 = CARTESIAN_POINT ( 'NONE',  ( -1.926860441876562247, 32.45379003517447813, -3.195792623639530650 ) ) ;
#23337 = CARTESIAN_POINT ( 'NONE',  ( 19.84674366389459621, 23.50893115100078390, 7.409399052514197653E-17 ) ) ;
#23338 = CARTESIAN_POINT ( 'NONE',  ( 19.84674366389459621, 13.50893115100078568, 7.409399052514197653E-17 ) ) ;
#23339 = CARTESIAN_POINT ( 'NONE',  ( 4.559911319644449179, 13.89701867748817143, 9.422509992056141925 ) ) ;
#23340 = CARTESIAN_POINT ( 'NONE',  ( 6.565887622018943937, 13.08196800326374998, -12.81628187352647608 ) ) ;
#23341 = CARTESIAN_POINT ( 'NONE',  ( 0.1532563361054100626, 65.80059781766745175, -2.638427012816831230 ) ) ;
#23342 = CARTESIAN_POINT ( 'NONE',  ( 6.324684870375198109, -50.88968658555813818, -2.499999999999999112 ) ) ;
#23343 = CARTESIAN_POINT ( 'NONE',  ( 19.42250999205614548, 5.980352010821504471, -5.440088680355545492 ) ) ;
#23344 = CARTESIAN_POINT ( 'NONE',  ( 17.20831665107776587, 42.88393115100077324, 7.208316651077764980 ) ) ;
#23345 = CARTESIAN_POINT ( 'NONE',  ( 6.574847571011208203, -50.89175608700130482, 2.750000000000000444 ) ) ;
#23346 = CARTESIAN_POINT ( 'NONE',  ( 0.5774900079438590739, 17.64701867748817321, -5.440088680355550821 ) ) ;
#23348 = B_SPLINE_CURVE_WITH_KNOTS ( 'NONE', 3,
 ( #85960, #24480, #77449, #32448, #63436, #17469 ),
 .UNSPECIFIED., .F., .F.,
 ( 4, 2, 4 ),
 ( 0.000000000000000000, 0.0002565770811490879037, 0.0005131541622981758075 ),
 .UNSPECIFIED. ) ;
#23347 = CARTESIAN_POINT ( 'NONE',  ( -4.494156999534594021, 0.000000000000000000, -3.088748530746273868 ) ) ;
#23349 = CARTESIAN_POINT ( 'NONE',  ( 20.88017736071110875, 30.77201867748816966, -2.915334737309920765 ) ) ;
#23351 = DIRECTION ( 'NONE',  ( -1.000000000000000000, 0.000000000000000000, 0.000000000000000000 ) ) ;
#23350 = CARTESIAN_POINT ( 'NONE',  ( -0.8801773607111008646, 3.272018677488171434, 2.915334737309923430 ) ) ;
#23352 = FILL_AREA_STYLE ('',( #84346 ) ) ;
#23353 = CARTESIAN_POINT ( 'NONE',  ( 19.84674366389459621, 18.50893115100078745, 7.409399052514197653E-17 ) ) ;
#23354 = CARTESIAN_POINT ( 'NONE',  ( 22.81628187352648496, 11.83196800326375531, -3.434112377981050290 ) ) ;
#23355 = CIRCLE ( 'NONE', #17003, 62.00000000000000000 ) ;
#23356 = CARTESIAN_POINT ( 'NONE',  ( 6.767445849361247490, 0.5000000000000004441, -13.38662304974496564 ) ) ;
#23357 = CARTESIAN_POINT ( 'NONE',  ( 19.84674366389459266, 63.30059781766745886, 2.638427012816836559 ) ) ;
#23358 = CARTESIAN_POINT ( 'NONE',  ( -13.14228782657333738, 0.3639308284105124414, -7.230509711182424581 ) ) ;
#23359 = CARTESIAN_POINT ( 'NONE',  ( -9.823941624412537266, -32.16601312909467225, -4.000000000000000000 ) ) ;
#23360 = CARTESIAN_POINT ( 'NONE',  ( 17.08211943468705840, 5.137082168247300906, -12.26659068614894466 ) ) ;
#23361 = CARTESIAN_POINT ( 'NONE',  ( 19.84674366389459621, 33.50893115100078745, 7.409399052514197653E-17 ) ) ;
#23362 = FILL_AREA_STYLE_COLOUR ( '', #44816 ) ;
#23363 = ORIENTED_EDGE ( 'NONE', *, *, #50335, .T. ) ;
#23364 = CARTESIAN_POINT ( 'NONE',  ( 17.08211943468705840, 60.13708216824729647, -12.26659068614894466 ) ) ;
#23365 = CARTESIAN_POINT ( 'NONE',  ( 19.84674366389459266, 13.71726448433411782, -2.638427012816827677 ) ) ;
#23366 = CARTESIAN_POINT ( 'NONE',  ( 4.219999999999999751, 10.00000000000000000, 3.750000000000000000 ) ) ;
#23367 = CARTESIAN_POINT ( 'NONE',  ( 19.42250999205614193, 45.14701867748817676, 5.440088680355555262 ) ) ;
#23368 = CARTESIAN_POINT ( 'NONE',  ( -2.816281873526473856, 49.12363466993042493, 9.499525473075851096E-16 ) ) ;
#23369 = CARTESIAN_POINT ( 'NONE',  ( 2.035157376598824452, 13.68868534415483751, 7.964842623401179544 ) ) ;
#23370 = CARTESIAN_POINT ( 'NONE',  ( 3.591859063236763294, 43.29030133659708923, -11.09922568453595026 ) ) ;
#23371 = CARTESIAN_POINT ( 'NONE',  ( 22.81628187352647785, 1.415301336597087012, 3.434112377981063169 ) ) ;
#23372 =( NAMED_UNIT ( * ) SI_UNIT ( $, .STERADIAN. ) SOLID_ANGLE_UNIT ( ) );
#23373 = ORIENTED_EDGE ( 'NONE', *, *, #2422, .F. ) ;
#23374 =( NAMED_UNIT ( * ) SI_UNIT ( $, .STERADIAN. ) SOLID_ANGLE_UNIT ( ) );
#23375 = B_SPLINE_CURVE_WITH_KNOTS ( 'NONE', 3,
 ( #42879, #65860, #11889, #12373, #27863, #42389 ),
 .UNSPECIFIED., .F., .F.,
 ( 4, 2, 4 ),
 ( 0.0002800032591452434271, 0.0006862085204419991757, 0.001092413781738754870 ),
 .UNSPECIFIED. ) ;
#23376 = LINE ( 'NONE', #38369, #94145 ) ;
#23377 = CARTESIAN_POINT ( 'NONE',  ( -2.266590686148945544, 42.22041550158063217, 7.082119434687048631 ) ) ;
#23378 = CARTESIAN_POINT ( 'NONE',  ( 20.36894250292379738, 14.92874883491396432, -10.36894250292379027 ) ) ;
#23379 = CARTESIAN_POINT ( 'NONE',  ( 4.559911319644449179, 23.89701867748817321, 9.422509992056141925 ) ) ;
#23380 = CARTESIAN_POINT ( 'NONE',  ( 17.96484262340118221, 36.18868534415484106, -7.964842623401177768 ) ) ;
#23381 = CARTESIAN_POINT ( 'NONE',  ( -14.62232599144295087, 15.00000000000000888, -0.3548652576990713459 ) ) ;
#23382 = CARTESIAN_POINT ( 'NONE',  ( 3.969999999999999751, 10.25000000000000000, 4.000000000000000000 ) ) ;
#23383 = CARTESIAN_POINT ( 'NONE',  ( 19.42250999205614193, 60.14701867748817676, 5.440088680355555262 ) ) ;
#23384 = CARTESIAN_POINT ( 'NONE',  ( -0.8801773607110991993, 62.85535201082150536, -2.915334737309923874 ) ) ;
#23385 = CARTESIAN_POINT ( 'NONE',  ( 16.40814093676324603, 27.45696800326375708, -11.09922568453594671 ) ) ;
#23386 = CARTESIAN_POINT ( 'NONE',  ( 14.40939250469963895, 15.00000000000000000, -1.618458416365745389 ) ) ;
#23387 = DIRECTION ( 'NONE',  ( 0.000000000000000000, 0.000000000000000000, -1.000000000000000000 ) ) ;
#23388 = CARTESIAN_POINT ( 'NONE',  ( 2.791683348922237240, 5.383931151000785675, -7.208316651077763204 ) ) ;
#23389 = CARTESIAN_POINT ( 'NONE',  ( 1.472469842513823179, 41.42559781766745886, 4.923371831947296329 ) ) ;
#23390 = EDGE_CURVE ( 'NONE', #38291, #42828, #65494, .T. ) ;
#23391 = CARTESIAN_POINT ( 'NONE',  ( 2.035157376598822676, 7.438685344154837509, -7.964842623401177768 ) ) ;
#23392 = AXIS2_PLACEMENT_3D ( 'NONE', #28740, #98762, #38236 ) ;
#23393 =( BOUNDED_SURFACE ( )  B_SPLINE_SURFACE ( 1, 2, ( 
 ( #51323, #80349, #88828, #87354, #64829, #26845, #95347, #36324, #94852, #12824, #43810, #19837, #95851, #50326, #50836, #81807, #13326, #5830, #26353, #27334, #11353, #81329, #80838, #12338, #4368, #28326, #19353, #34833, #41873, #65821, #42843, #18868, #56854, #65326, #49349, #73327, #43323, #4852, #11846, #35327, #49837, #96355, #34333, #27826, #87834, #20339, #58312, #73816, #5350, #35828, #66314, #3869, #96850, #89325, #20834, #79851, #72337, #57341, #42355, #72830, #62133, #14325, #52797, #92641, #69657, #67819, #29793, #52311, #46650, #16660, #36822, #83301, #37329, #82803, #44796, #8655, #75301, #70158, #47643, #90291, #6813, #6315, #24165, #98335, #67314, #39168, #47135, #60304, #90797, #78139, #24659, #31641, #97839, #54636, #85154, #51818, #22323, #1183, #28811, #55128, #74809, #59310, #66817, #32128, #97339, #44307, #77632, #77146, #9149, #29304, #59799, #21828, #16166, #1675, #39666, #62627, #17163, #93132, #85644, #9649, #89808, #21329, #82304, #13826, #48616, #94615, #11605, #33119, #4122, #57101, #95096, #79617, #32630, #10147, #78640, #34097, #55641, #88089, #71140, #42122, #2173, #19107, #79120, #87110, #33602, #10633, #87597, #18625, #72588, #63613, #63129, #34585, #49587, #3140, #49116, #27089, #40642, #80602, #41145, #56139, #18144, #11118, #86634, #65079, #19602, #94119, #71630, #2668, #64588, #64099, #25646, #41637, #80100, #26130, #56621, #50097, #95603, #3630, #72103, #26604, #57592, #25166, #40146, #70650, #93631, #86141, #48125, #17655, #12100, #75065, #42603, #88583, #82071, #21087, #29064, #50595, #73573, #5098, #66583, #14087, #13081, #96605, #60056, #81087, #28581, #67583, #73081, #52080, #98092, #52561, #20596, #97110, #82573, #35589, #6572, #59572, #67075, #51585, #4617, #12588, #43088, #6086, #27589, #90557, #66077, #44567, #35078, #90065, #51082, #59072, #5601, #81574, #21589, #89576, #37084, #28082, #65578, #29551, #22086, #74069, #13581, #96105, #58580, #58079, #43576, #20091, #89082, #36080, #44065, #74572, #97603, #36588, #68565, #69055, #38074, #591, #22577, #54040, #76056, #77039, #31034, #76545, #8552, #46058, #8063, #91049, #38560, #84550, #15578, #61534, #92043, #16049, #23571, #83567, #39051, #30543, #46538, #69546, #1064, #84057, #31529, #96, #62024, #92525, #53048, #24052, #53544, #54522, #32011, #68073, #85038, #39550, #61043, #16550, #75565, #15087, #45558, #7585, #24555, #83065, #47025, #62513, #77516, #9033, #70039, #1562, #93018, #14586, #45055, #7078, #37580, #98600, #30050, #60559, #91556, #23075, #87487, #78513, #63507, #2053, #26012, #56022, #85530, #71027, #17538 ),
 ( #48993, #18018, #79002, #63013, #48501, #56505, #86521, #10507, #41022, #86997, #71524, #55526, #79503, #2550, #3033, #11002, #18503, #33482, #63979, #40529, #94492, #3512, #25041, #41521, #25530, #33007, #94007, #71989, #33971, #56982, #34470, #10028, #64475, #93516, #94981, #26487, #86023, #19002, #49478, #79986, #11488, #64963, #42008, #72475, #48006, #4007, #95489, #40028, #55013, #17042, #47521, #78024, #9527, #70531, #32516, #13459, #26980, #4499, #43455, #81458, #28464, #34964, #57964, #88468, #58452, #43943, #4984, #50468, #97475, #65462, #20476, #36461, #57479, #81948, #28939, #87975, #35464, #50963, #74441, #19970, #5967, #80485, #49978, #12960, #65961, #66452, #73957, #27471, #96987, #19486, #5485, #58959, #66956, #11984, #89458, #72968, #80973, #12472, #73456, #42976, #59443, #20975, #96488, #35956, #42487, #95990, #27959, #51459, #88967, #72789, #2865, #11317, #9858, #86342, #48330, #17845, #57794, #17365, #34292, #65288, #41356, #18338, #10837, #72303, #4326, #34798, #95815, #47834, #48818, #32828, #3833, #79327, #71825, #25842, #49800, #40845, #56340, #63327, #87313, #3334, #78337, #33316, #78834, #10345, #71347, #40357, #63811, #27295, #41836, #93835, #19314, #86834, #80308, #64303, #94321, #64789, #33796, #95306, #94814, #26317, #55847, #26810, #56815, #18831, #49311, #70858, #79813, #2373, #57304, #87796, #11808, #42316, #25361, #8945, #503, #16459, #977, #46456, #8460, #69953, #76949, #32429, #9943, #53959, #38965, #68971, #54927, #31440, #30951, #1472, #77934, #92442, #23965, #40446, #85943, #92929, #61450, #85443, #24462, #15492, #54439, #31926, #91466, #17454, #38478, #22991, #30457, #93432, #47921, #91957, #53457, #60956, #24954, #83965, #7979, #62426, #39463, #47436, #23487, #84466, #15964, #84948, #62930, #61941, #69458, #78426, #46939, #77432, #70947, #45974, #70446, #76464, #16951, #9442, #39943, #1963, #55439, #65378, #19402, #57394, #41927, #93926, #71437, #40939, #95400, #17934, #50381, #33399, #72882, #63423, #80399, #41444, #49397, #94902, #71904, #49888, #79898, #34883, #94411, #25452, #4419, #11903, #64392, #11404, #88390, #2951, #42893, #10919, #55935, #2465, #3428, #19889, #72389, #87884, #56900, #86915, #87405, #56428, #18921, #63898, #3917, #25926, #26899, #34386, #26400, #42405, #64874, #95906, #10431, #27387, #57878, #33887, #80890, #12388, #32921, #86435, #18424, #48419, #48907, #78921, #79423, #74861, #74352, #89372, #51872, #75350, #82355, #43371, #59358, #43857, #20884, #51373, #13876, #81860, #6864, #52845, #96901, #13372, #12873, #97890, #5878, #73871, #44359, #21878, #36374 ) ),
 .UNSPECIFIED., .F., .F., .T. ) 
 B_SPLINE_SURFACE_WITH_KNOTS ( ( 2, 2 ),
 ( 3, 2, 2, 2, 2, 2, 2, 2, 2, 2, 2, 2, 2, 2, 2, 2, 2, 2, 2, 2, 2, 2, 2, 2, 2, 2, 2, 2, 2, 2, 2, 2, 2, 2, 2, 2, 2, 2, 2, 2, 2, 2, 2, 2, 2, 2, 2, 2, 2, 2, 2, 2, 2, 2, 2, 2, 2, 2, 2, 2, 2, 2, 2, 2, 2, 2, 2, 2, 2, 2, 2, 2, 2, 2, 2, 2, 2, 2, 2, 2, 2, 2, 2, 2, 2, 2, 2, 2, 2, 2, 2, 2, 2, 2, 2, 2, 2, 2, 2, 2, 2, 2, 2, 2, 2, 2, 2, 2, 2, 2, 2, 2, 2, 2, 2, 2, 2, 2, 2, 2, 2, 2, 2, 2, 2, 2, 2, 2, 2, 2, 2, 2, 2, 2, 2, 2, 2, 2, 2, 2, 2, 2, 2, 2, 2, 2, 2, 2, 2, 2, 2, 2, 2, 2, 2, 2, 2, 2, 2, 2, 2, 2, 3 ),
 ( 0.000000000000000000, 1.000000000000000000 ),
 ( 0.000000000000000000, 0.005952380952380952051, 0.01190476190476190410, 0.01785714285714285615, 0.02380952380952380820, 0.02976190476190476025, 0.03571428571428571230, 0.04166666666666666435, 0.04761904761904761640, 0.05357142857142856845, 0.05952380952380952051, 0.06547619047619047949, 0.07142857142857142461, 0.07738095238095238360, 0.08333333333333332871, 0.08928571428571428770, 0.09523809523809523281, 0.1011904761904761918, 0.1071428571428571369, 0.1130952380952380959, 0.1190476190476190410, 0.1250000000000000000, 0.1309523809523809590, 0.1369047619047619180, 0.1428571428571428492, 0.1488095238095238082, 0.1547619047619047672, 0.1607142857142857262, 0.1666666666666666574, 0.1726190476190476164, 0.1785714285714285754, 0.1845238095238095344, 0.1904761904761904656, 0.1964285714285714246, 0.2023809523809523836, 0.2083333333333333426, 0.2142857142857142738, 0.2202380952380952328, 0.2261904761904761918, 0.2321428571428571508, 0.2380952380952380820, 0.2440476190476190410, 0.2500000000000000000, 0.2559523809523809312, 0.2619047619047619180, 0.2678571428571428492, 0.2738095238095238360, 0.2797619047619047672, 0.2857142857142856984, 0.2916666666666666852, 0.2976190476190476164, 0.3035714285714285476, 0.3095238095238095344, 0.3154761904761904656, 0.3214285714285714524, 0.3273809523809523836, 0.3333333333333333148, 0.3392857142857143016, 0.3452380952380952328, 0.3511904761904761640, 0.3571428571428571508, 0.3630952380952380820, 0.3690476190476190688, 0.3750000000000000000, 0.3809523809523809312, 0.3869047619047619180, 0.3928571428571428492, 0.3988095238095238360, 0.4047619047619047672, 0.4107142857142856984, 0.4166666666666666852, 0.4226190476190476164, 0.4285714285714285476, 0.4345238095238095344, 0.4404761904761904656, 0.4464285714285714524, 0.4523809523809523836, 0.4583333333333333148, 0.4642857142857143016, 0.4702380952380952328, 0.4761904761904761640, 0.4821428571428571508, 0.4880952380952380820, 0.4940476190476190688, 0.5000000000000000000, 0.5059523809523809312, 0.5119047619047618625, 0.5178571428571429047, 0.5238095238095238360, 0.5297619047619047672, 0.5357142857142856984, 0.5416666666666666297, 0.5476190476190476719, 0.5535714285714286031, 0.5595238095238095344, 0.5654761904761904656, 0.5714285714285713969, 0.5773809523809523281, 0.5833333333333333703, 0.5892857142857143016, 0.5952380952380952328, 0.6011904761904761640, 0.6071428571428570953, 0.6130952380952381375, 0.6190476190476190688, 0.6250000000000000000, 0.6309523809523809312, 0.6369047619047618625, 0.6428571428571429047, 0.6488095238095238360, 0.6547619047619047672, 0.6607142857142856984, 0.6666666666666666297, 0.6726190476190476719, 0.6785714285714286031, 0.6845238095238095344, 0.6904761904761904656, 0.6964285714285713969, 0.7023809523809523281, 0.7083333333333333703, 0.7142857142857143016, 0.7202380952380952328, 0.7261904761904761640, 0.7321428571428570953, 0.7380952380952381375, 0.7440476190476190688, 0.7500000000000000000, 0.7559523809523809312, 0.7619047619047618625, 0.7678571428571429047, 0.7738095238095238360, 0.7797619047619047672, 0.7857142857142856984, 0.7916666666666666297, 0.7976190476190476719, 0.8035714285714286031, 0.8095238095238095344, 0.8154761904761904656, 0.8214285714285713969, 0.8273809523809523281, 0.8333333333333333703, 0.8392857142857143016, 0.8452380952380952328, 0.8511904761904761640, 0.8571428571428570953, 0.8630952380952381375, 0.8690476190476190688, 0.8750000000000000000, 0.8809523809523809312, 0.8869047619047618625, 0.8928571428571429047, 0.8988095238095238360, 0.9047619047619047672, 0.9107142857142856984, 0.9166666666666666297, 0.9226190476190476719, 0.9285714285714286031, 0.9345238095238095344, 0.9404761904761904656, 0.9464285714285713969, 0.9523809523809523281, 0.9583333333333333703, 0.9642857142857143016 ),
 .UNSPECIFIED. ) 
 GEOMETRIC_REPRESENTATION_ITEM ( )  RATIONAL_B_SPLINE_SURFACE ( (
 ( 1.000000000000000000, 0.9659258262890683122, 1.000000000000000000, 0.9659258262890683122, 1.000000000000000000, 0.9659258262890683122, 1.000000000000000000, 0.9659258262890683122, 1.000000000000000000, 0.9659258262890683122, 1.000000000000000000, 0.9659258262890683122, 1.000000000000000000, 0.9659258262890683122, 1.000000000000000000, 0.9659258262890683122, 1.000000000000000000, 0.9659258262890683122, 1.000000000000000000, 0.9659258262890683122, 1.000000000000000000, 0.9659258262890683122, 1.000000000000000000, 0.9659258262890683122, 1.000000000000000000, 0.9659258262890683122, 1.000000000000000000, 0.9659258262890683122, 1.000000000000000000, 0.9659258262890683122, 1.000000000000000000, 0.9659258262890683122, 1.000000000000000000, 0.9659258262890683122, 1.000000000000000000, 0.9659258262890683122, 1.000000000000000000, 0.9659258262890683122, 1.000000000000000000, 0.9659258262890683122, 1.000000000000000000, 0.9659258262890683122, 1.000000000000000000, 0.9659258262890683122, 1.000000000000000000, 0.9659258262890683122, 1.000000000000000000, 0.9659258262890683122, 1.000000000000000000, 0.9659258262890683122, 1.000000000000000000, 0.9659258262890683122, 1.000000000000000000, 0.9659258262890683122, 1.000000000000000000, 0.9659258262890683122, 1.000000000000000000, 0.9659258262890683122, 1.000000000000000000, 0.9659258262890683122, 1.000000000000000000, 0.9659258262890683122, 1.000000000000000000, 0.9659258262890683122, 1.000000000000000000, 0.9659258262890683122, 1.000000000000000000, 0.9659258262890683122, 1.000000000000000000, 0.9659258262890683122, 1.000000000000000000, 0.9659258262890683122, 1.000000000000000000, 0.9659258262890683122, 1.000000000000000000, 0.9659258262890683122, 1.000000000000000000, 0.9659258262890683122, 1.000000000000000000, 0.9659258262890683122, 1.000000000000000000, 0.9659258262890683122, 1.000000000000000000, 0.9659258262890683122, 1.000000000000000000, 0.9659258262890683122, 1.000000000000000000, 0.9659258262890683122, 1.000000000000000000, 0.9659258262890683122, 1.000000000000000000, 0.9659258262890683122, 1.000000000000000000, 0.9659258262890683122, 1.000000000000000000, 0.9659258262890683122, 1.000000000000000000, 0.9659258262890683122, 1.000000000000000000, 0.9659258262890683122, 1.000000000000000000, 0.9659258262890683122, 1.000000000000000000, 0.9659258262890683122, 1.000000000000000000, 0.9659258262890683122, 1.000000000000000000, 0.9659258262890683122, 1.000000000000000000, 0.9659258262890683122, 1.000000000000000000, 0.9659258262890683122, 1.000000000000000000, 0.9659258262890683122, 1.000000000000000000, 0.9659258262890683122, 1.000000000000000000, 0.9659258262890683122, 1.000000000000000000, 0.9659258262890683122, 1.000000000000000000, 0.9659258262890683122, 1.000000000000000000, 0.9659258262890683122, 1.000000000000000000, 0.9659258262890683122, 1.000000000000000000, 0.9659258262890683122, 1.000000000000000000, 0.9659258262890683122, 1.000000000000000000, 0.9659258262890683122, 1.000000000000000000, 0.9659258262890683122, 1.000000000000000000, 0.9659258262890683122, 1.000000000000000000, 0.9659258262890683122, 1.000000000000000000, 0.9659258262890683122, 1.000000000000000000, 0.9659258262890683122, 1.000000000000000000, 0.9659258262890683122, 1.000000000000000000, 0.9659258262890683122, 1.000000000000000000, 0.9659258262890683122, 1.000000000000000000, 0.9659258262890683122, 1.000000000000000000, 0.9659258262890683122, 1.000000000000000000, 0.9659258262890683122, 1.000000000000000000, 0.9659258262890683122, 1.000000000000000000, 0.9659258262890683122, 1.000000000000000000, 0.9659258262890683122, 1.000000000000000000, 0.9659258262890683122, 1.000000000000000000, 0.9659258262890683122, 1.000000000000000000, 0.9659258262890683122, 1.000000000000000000, 0.9659258262890683122, 1.000000000000000000, 0.9659258262890683122, 1.000000000000000000, 0.9659258262890683122, 1.000000000000000000, 0.9659258262890683122, 1.000000000000000000, 0.9659258262890683122, 1.000000000000000000, 0.9659258262890683122, 1.000000000000000000, 0.9659258262890683122, 1.000000000000000000, 0.9659258262890683122, 1.000000000000000000, 0.9659258262890683122, 1.000000000000000000, 0.9659258262890683122, 1.000000000000000000, 0.9659258262890683122, 1.000000000000000000, 0.9659258262890683122, 1.000000000000000000, 0.9659258262890683122, 1.000000000000000000, 0.9659258262890683122, 1.000000000000000000, 0.9659258262890683122, 1.000000000000000000, 0.9659258262890683122, 1.000000000000000000, 0.9659258262890683122, 1.000000000000000000, 0.9659258262890683122, 1.000000000000000000, 0.9659258262890683122, 1.000000000000000000, 0.9659258262890683122, 1.000000000000000000, 0.9659258262890683122, 1.000000000000000000, 0.9659258262890683122, 1.000000000000000000, 0.9659258262890683122, 1.000000000000000000, 0.9659258262890683122, 1.000000000000000000, 0.9659258262890683122, 1.000000000000000000, 0.9659258262890683122, 1.000000000000000000, 0.9659258262890683122, 1.000000000000000000, 0.9659258262890683122, 1.000000000000000000, 0.9659258262890683122, 1.000000000000000000, 0.9659258262890683122, 1.000000000000000000, 0.9659258262890683122, 1.000000000000000000, 0.9659258262890683122, 1.000000000000000000, 0.9659258262890683122, 1.000000000000000000, 0.9659258262890683122, 1.000000000000000000, 0.9659258262890683122, 1.000000000000000000, 0.9659258262890683122, 1.000000000000000000, 0.9659258262890683122, 1.000000000000000000, 0.9659258262890683122, 1.000000000000000000, 0.9659258262890683122, 1.000000000000000000, 0.9659258262890683122, 1.000000000000000000, 0.9659258262890683122, 1.000000000000000000, 0.9659258262890683122, 1.000000000000000000, 0.9659258262890683122, 1.000000000000000000, 0.9659258262890683122, 1.000000000000000000, 0.9659258262890683122, 1.000000000000000000, 0.9659258262890683122, 1.000000000000000000, 0.9659258262890683122, 1.000000000000000000, 0.9659258262890683122, 1.000000000000000000, 0.9659258262890683122, 1.000000000000000000, 0.9659258262890683122, 1.000000000000000000, 0.9659258262890683122, 1.000000000000000000, 0.9659258262890683122, 1.000000000000000000, 0.9659258262890683122, 1.000000000000000000, 0.9659258262890683122, 1.000000000000000000, 0.9659258262890683122, 1.000000000000000000, 0.9659258262890683122, 1.000000000000000000, 0.9659258262890683122, 1.000000000000000000, 0.9659258262890683122, 1.000000000000000000, 0.9659258262890683122, 1.000000000000000000, 0.9659258262890683122, 1.000000000000000000, 0.9659258262890683122, 1.000000000000000000, 0.9659258262890683122, 1.000000000000000000, 0.9659258262890683122, 1.000000000000000000, 0.9659258262890683122, 1.000000000000000000, 0.9659258262890683122, 1.000000000000000000, 0.9659258262890683122, 1.000000000000000000, 0.9659258262890683122, 1.000000000000000000, 0.9659258262890683122, 1.000000000000000000, 0.9659258262890683122, 1.000000000000000000, 0.9659258262890683122, 1.000000000000000000, 0.9659258262890683122, 1.000000000000000000, 0.9659258262890683122, 1.000000000000000000, 0.9659258262890683122, 1.000000000000000000, 0.9659258262890683122, 1.000000000000000000, 0.9659258262890683122, 1.000000000000000000, 0.9659258262890683122, 1.000000000000000000, 0.9659258262890683122, 1.000000000000000000, 0.9659258262890683122, 1.000000000000000000, 0.9659258262890683122, 1.000000000000000000),
 ( 1.000000000000000000, 0.9659258262890683122, 1.000000000000000000, 0.9659258262890683122, 1.000000000000000000, 0.9659258262890683122, 1.000000000000000000, 0.9659258262890683122, 1.000000000000000000, 0.9659258262890683122, 1.000000000000000000, 0.9659258262890683122, 1.000000000000000000, 0.9659258262890683122, 1.000000000000000000, 0.9659258262890683122, 1.000000000000000000, 0.9659258262890683122, 1.000000000000000000, 0.9659258262890683122, 1.000000000000000000, 0.9659258262890683122, 1.000000000000000000, 0.9659258262890683122, 1.000000000000000000, 0.9659258262890683122, 1.000000000000000000, 0.9659258262890683122, 1.000000000000000000, 0.9659258262890683122, 1.000000000000000000, 0.9659258262890683122, 1.000000000000000000, 0.9659258262890683122, 1.000000000000000000, 0.9659258262890683122, 1.000000000000000000, 0.9659258262890683122, 1.000000000000000000, 0.9659258262890683122, 1.000000000000000000, 0.9659258262890683122, 1.000000000000000000, 0.9659258262890683122, 1.000000000000000000, 0.9659258262890683122, 1.000000000000000000, 0.9659258262890683122, 1.000000000000000000, 0.9659258262890683122, 1.000000000000000000, 0.9659258262890683122, 1.000000000000000000, 0.9659258262890683122, 1.000000000000000000, 0.9659258262890683122, 1.000000000000000000, 0.9659258262890683122, 1.000000000000000000, 0.9659258262890683122, 1.000000000000000000, 0.9659258262890683122, 1.000000000000000000, 0.9659258262890683122, 1.000000000000000000, 0.9659258262890683122, 1.000000000000000000, 0.9659258262890683122, 1.000000000000000000, 0.9659258262890683122, 1.000000000000000000, 0.9659258262890683122, 1.000000000000000000, 0.9659258262890683122, 1.000000000000000000, 0.9659258262890683122, 1.000000000000000000, 0.9659258262890683122, 1.000000000000000000, 0.9659258262890683122, 1.000000000000000000, 0.9659258262890683122, 1.000000000000000000, 0.9659258262890683122, 1.000000000000000000, 0.9659258262890683122, 1.000000000000000000, 0.9659258262890683122, 1.000000000000000000, 0.9659258262890683122, 1.000000000000000000, 0.9659258262890683122, 1.000000000000000000, 0.9659258262890683122, 1.000000000000000000, 0.9659258262890683122, 1.000000000000000000, 0.9659258262890683122, 1.000000000000000000, 0.9659258262890683122, 1.000000000000000000, 0.9659258262890683122, 1.000000000000000000, 0.9659258262890683122, 1.000000000000000000, 0.9659258262890683122, 1.000000000000000000, 0.9659258262890683122, 1.000000000000000000, 0.9659258262890683122, 1.000000000000000000, 0.9659258262890683122, 1.000000000000000000, 0.9659258262890683122, 1.000000000000000000, 0.9659258262890683122, 1.000000000000000000, 0.9659258262890683122, 1.000000000000000000, 0.9659258262890683122, 1.000000000000000000, 0.9659258262890683122, 1.000000000000000000, 0.9659258262890683122, 1.000000000000000000, 0.9659258262890683122, 1.000000000000000000, 0.9659258262890683122, 1.000000000000000000, 0.9659258262890683122, 1.000000000000000000, 0.9659258262890683122, 1.000000000000000000, 0.9659258262890683122, 1.000000000000000000, 0.9659258262890683122, 1.000000000000000000, 0.9659258262890683122, 1.000000000000000000, 0.9659258262890683122, 1.000000000000000000, 0.9659258262890683122, 1.000000000000000000, 0.9659258262890683122, 1.000000000000000000, 0.9659258262890683122, 1.000000000000000000, 0.9659258262890683122, 1.000000000000000000, 0.9659258262890683122, 1.000000000000000000, 0.9659258262890683122, 1.000000000000000000, 0.9659258262890683122, 1.000000000000000000, 0.9659258262890683122, 1.000000000000000000, 0.9659258262890683122, 1.000000000000000000, 0.9659258262890683122, 1.000000000000000000, 0.9659258262890683122, 1.000000000000000000, 0.9659258262890683122, 1.000000000000000000, 0.9659258262890683122, 1.000000000000000000, 0.9659258262890683122, 1.000000000000000000, 0.9659258262890683122, 1.000000000000000000, 0.9659258262890683122, 1.000000000000000000, 0.9659258262890683122, 1.000000000000000000, 0.9659258262890683122, 1.000000000000000000, 0.9659258262890683122, 1.000000000000000000, 0.9659258262890683122, 1.000000000000000000, 0.9659258262890683122, 1.000000000000000000, 0.9659258262890683122, 1.000000000000000000, 0.9659258262890683122, 1.000000000000000000, 0.9659258262890683122, 1.000000000000000000, 0.9659258262890683122, 1.000000000000000000, 0.9659258262890683122, 1.000000000000000000, 0.9659258262890683122, 1.000000000000000000, 0.9659258262890683122, 1.000000000000000000, 0.9659258262890683122, 1.000000000000000000, 0.9659258262890683122, 1.000000000000000000, 0.9659258262890683122, 1.000000000000000000, 0.9659258262890683122, 1.000000000000000000, 0.9659258262890683122, 1.000000000000000000, 0.9659258262890683122, 1.000000000000000000, 0.9659258262890683122, 1.000000000000000000, 0.9659258262890683122, 1.000000000000000000, 0.9659258262890683122, 1.000000000000000000, 0.9659258262890683122, 1.000000000000000000, 0.9659258262890683122, 1.000000000000000000, 0.9659258262890683122, 1.000000000000000000, 0.9659258262890683122, 1.000000000000000000, 0.9659258262890683122, 1.000000000000000000, 0.9659258262890683122, 1.000000000000000000, 0.9659258262890683122, 1.000000000000000000, 0.9659258262890683122, 1.000000000000000000, 0.9659258262890683122, 1.000000000000000000, 0.9659258262890683122, 1.000000000000000000, 0.9659258262890683122, 1.000000000000000000, 0.9659258262890683122, 1.000000000000000000, 0.9659258262890683122, 1.000000000000000000, 0.9659258262890683122, 1.000000000000000000, 0.9659258262890683122, 1.000000000000000000, 0.9659258262890683122, 1.000000000000000000, 0.9659258262890683122, 1.000000000000000000, 0.9659258262890683122, 1.000000000000000000, 0.9659258262890683122, 1.000000000000000000, 0.9659258262890683122, 1.000000000000000000, 0.9659258262890683122, 1.000000000000000000, 0.9659258262890683122, 1.000000000000000000, 0.9659258262890683122, 1.000000000000000000, 0.9659258262890683122, 1.000000000000000000, 0.9659258262890683122, 1.000000000000000000, 0.9659258262890683122, 1.000000000000000000, 0.9659258262890683122, 1.000000000000000000, 0.9659258262890683122, 1.000000000000000000, 0.9659258262890683122, 1.000000000000000000, 0.9659258262890683122, 1.000000000000000000, 0.9659258262890683122, 1.000000000000000000, 0.9659258262890683122, 1.000000000000000000, 0.9659258262890683122, 1.000000000000000000, 0.9659258262890683122, 1.000000000000000000, 0.9659258262890683122, 1.000000000000000000, 0.9659258262890683122, 1.000000000000000000, 0.9659258262890683122, 1.000000000000000000, 0.9659258262890683122, 1.000000000000000000, 0.9659258262890683122, 1.000000000000000000, 0.9659258262890683122, 1.000000000000000000, 0.9659258262890683122, 1.000000000000000000, 0.9659258262890683122, 1.000000000000000000, 0.9659258262890683122, 1.000000000000000000, 0.9659258262890683122, 1.000000000000000000, 0.9659258262890683122, 1.000000000000000000, 0.9659258262890683122, 1.000000000000000000, 0.9659258262890683122, 1.000000000000000000, 0.9659258262890683122, 1.000000000000000000, 0.9659258262890683122, 1.000000000000000000, 0.9659258262890683122, 1.000000000000000000, 0.9659258262890683122, 1.000000000000000000, 0.9659258262890683122, 1.000000000000000000, 0.9659258262890683122, 1.000000000000000000, 0.9659258262890683122, 1.000000000000000000, 0.9659258262890683122, 1.000000000000000000) ) ) 
 REPRESENTATION_ITEM ( '' )  SURFACE ( )  );
#23394 = AXIS2_PLACEMENT_3D ( 'NONE', #22312, #85760, #26231 ) ;
#23395 = CARTESIAN_POINT ( 'NONE',  ( 19.38216949554541557, 27.24863466993041783, -9.382169495545420901 ) ) ;
#23396 = CARTESIAN_POINT ( 'NONE',  ( 10.00000000000000000, 9.758931151000785675, -9.846743663894594434 ) ) ;
#23397 = CARTESIAN_POINT ( 'NONE',  ( -0.8801773607111009756, 8.063685344154837509, 1.068504757029289695E-15 ) ) ;
#23398 = CIRCLE ( 'NONE', #29783, 0.2500000000000002220 ) ;
#23399 = CARTESIAN_POINT ( 'NONE',  ( 18.52753015748617571, 33.09226448433411605, 4.923371831947298993 ) ) ;
#23400 = CARTESIAN_POINT ( 'NONE',  ( 14.92337183194729988, 29.34226448433411960, -8.527530157486177487 ) ) ;
#23401 =( BOUNDED_CURVE ( )  B_SPLINE_CURVE ( 2, ( #73385, #25935, #49901, #50391, #35391, #58373, #65883, #56436, #96410, #88894, #20403, #50890, #40948 ),
 .UNSPECIFIED., .F., .F. ) 
 B_SPLINE_CURVE_WITH_KNOTS ( ( 3, 2, 2, 2, 2, 2, 3 ),
 ( 0.6666666666666667407, 0.6722222222222223875, 0.6777777777777779233, 0.6833333333333333481, 0.6888888888888888840, 0.6944444444444444198, 0.6999999999999999556 ),
 .UNSPECIFIED. ) 
 CURVE ( )  GEOMETRIC_REPRESENTATION_ITEM ( )  RATIONAL_B_SPLINE_CURVE ( ( 0.9999999999999993339, 0.9659258262890689783, 1.000000000000000000, 0.9659258262890683122, 1.000000000000000000, 0.9659258262890683122, 1.000000000000000000, 0.9659258262890683122, 1.000000000000000000, 0.9659258262890683122, 1.000000000000000000, 0.9659258262890683122, 1.000000000000000000 ) ) 
 REPRESENTATION_ITEM ( '' )  );
#23402 = CARTESIAN_POINT ( 'NONE',  ( -2.266590686148945544, 16.38708216824730357, -7.082119434687050408 ) ) ;
#23403 = CARTESIAN_POINT ( 'NONE',  ( 20.88017736071110519, 35.56368534415484106, 2.639326808657452039E-16 ) ) ;
#23404 = CARTESIAN_POINT ( 'NONE',  ( 20.88017736071110164, 5.355352010821502695, 2.915334737309930979 ) ) ;
#23405 = CARTESIAN_POINT ( 'NONE',  ( 10.00000000000000178, 34.31368534415484106, 10.88017736071110342 ) ) ;
#23406 = CARTESIAN_POINT ( 'NONE',  ( 7.084665262690076126, 34.10535201082151247, 10.88017736071109987 ) ) ;
#23407 = ORIENTED_EDGE ( 'NONE', *, *, #2058, .T. ) ;
#23408 = CARTESIAN_POINT ( 'NONE',  ( 2.035157376598824452, 33.68868534415484106, 7.964842623401179544 ) ) ;
#23409 = CARTESIAN_POINT ( 'NONE',  ( 22.81628187352647785, 61.41530133659709634, 3.434112377981063169 ) ) ;
#23411 = AXIS2_PLACEMENT_3D ( 'NONE', #85680, #26159, #56654 ) ;
#23410 = CARTESIAN_POINT ( 'NONE',  ( 0.5774900079438607392, 43.48035201082151247, 5.440088680355550821 ) ) ;
#23412 = CARTESIAN_POINT ( 'NONE',  ( 7.084665262690076126, 47.02201867748818387, -10.88017736071110164 ) ) ;
#23413 = VERTEX_POINT ( 'NONE', #97231 ) ;
#23414 = COLOUR_RGB ( '', 0.31764706, 0.68627451, 0.89019608) ;
#23415 = CARTESIAN_POINT ( 'NONE',  ( 15.44008868035555260, 44.73035201082151247, 9.422509992056143702 ) ) ;
#23416 = DIRECTION ( 'NONE',  ( 0.000000000000000000, 0.000000000000000000, 1.000000000000000000 ) ) ;
#23418 = ADVANCED_FACE ( 'NONE', ( #66197 ), #96729, .F. ) ;
#23417 = AXIS2_PLACEMENT_3D ( 'NONE', #85561, #17072, #47555 ) ;
#23419 =( NAMED_UNIT ( * ) PLANE_ANGLE_UNIT ( ) SI_UNIT ( $, .RADIAN. ) );
#23420 = CARTESIAN_POINT ( 'NONE',  ( -0.3689425029237898834, 66.17874883491396076, -10.36894250292378850 ) ) ;
#23421 = CARTESIAN_POINT ( 'NONE',  ( 12.63842701281683034, 2.467264484334118269, 9.846743663894596210 ) ) ;
#23422 = DIRECTION ( 'NONE',  ( 0.000000000000000000, -1.000000000000000000, 0.000000000000000000 ) ) ;
#23423 = DIRECTION ( 'NONE',  ( 0.8320502943378436100, -0.5547001962252291474, 0.000000000000000000 ) ) ;
#23424 = LINE ( 'NONE', #67430, #42857 ) ;
#23425 = CARTESIAN_POINT ( 'NONE',  ( 14.92337183194729633, 37.67559781766745175, 8.527530157486181039 ) ) ;
#23426 = ORIENTED_EDGE ( 'NONE', *, *, #38954, .T. ) ;
#23427 = CARTESIAN_POINT ( 'NONE',  ( 17.20831665107776587, 32.88393115100078745, 7.208316651077764980 ) ) ;
#23428 = CARTESIAN_POINT ( 'NONE',  ( 17.96484262340118221, 44.93868534415483396, 7.964842623401181321 ) ) ;
#23429 = CARTESIAN_POINT ( 'NONE',  ( 10.00000000000000178, 42.25893115100078745, 9.846743663894594434 ) ) ;
#23430 = CARTESIAN_POINT ( 'NONE',  ( 19.38216949554541202, 20.99863466993042138, 9.382169495545424454 ) ) ;
#23432 = CARTESIAN_POINT ( 'NONE',  ( 7.084665262690076126, 59.10535201082150536, 10.88017736071109987 ) ) ;
#23431 = DIRECTION ( 'NONE',  ( 0.000000000000000000, -1.000000000000000000, 0.000000000000000000 ) ) ;
#23434 = CARTESIAN_POINT ( 'NONE',  ( 17.96484262340118221, 6.188685344154836621, -7.964842623401177768 ) ) ;
#23433 = CARTESIAN_POINT ( 'NONE',  ( -0.8801773607111008646, 48.27201867748816966, 2.915334737309923430 ) ) ;
#23435 = CARTESIAN_POINT ( 'NONE',  ( 24.16423886937410614, 59.51208216824728936, -3.795296366450302550 ) ) ;
#23436 = COLOUR_RGB ( '', 0.72549020, 0.75294118, 0.79215686) ;
#23437 = CARTESIAN_POINT ( 'NONE',  ( -1.099225684535947600, 24.54030133659708923, 6.408140936763237150 ) ) ;
#23438 = CARTESIAN_POINT ( 'NONE',  ( 1.959929470562281395, 50.51528370094808196, -5.767676674365853629 ) ) ;
#23439 = ORIENTED_EDGE ( 'NONE', *, *, #16221, .T. ) ;
#23440 = CARTESIAN_POINT ( 'NONE',  ( 13.43411237798105340, 20.58196800326374643, 12.81628187352647963 ) ) ;
#23441 = CARTESIAN_POINT ( 'NONE',  ( 17.96484262340118221, 24.93868534415484461, 7.964842623401181321 ) ) ;
#23442 = VECTOR ( 'NONE', #75027, 1000.000000000000000 ) ;
#23443 = CARTESIAN_POINT ( 'NONE',  ( 20.88017736071110519, 55.56368534415484817, 2.639326808657452039E-16 ) ) ;
#23444 = ORIENTED_EDGE ( 'NONE', *, *, #18847, .F. ) ;
#23445 = EDGE_CURVE ( 'NONE', #95671, #83096, #75072, .T. ) ;
#23446 = CARTESIAN_POINT ( 'NONE',  ( 7.361572987183169658, 4.967264484334119601, -9.846743663894592657 ) ) ;
#23447 = CARTESIAN_POINT ( 'NONE',  ( 12.63842701281683034, 47.46726448433412315, 9.846743663894596210 ) ) ;
#23448 = CARTESIAN_POINT ( 'NONE',  ( 18.52753015748618282, 38.92559781766745175, -4.923371831947291888 ) ) ;
#23449 = CARTESIAN_POINT ( 'NONE',  ( -9.075906804202377387, -0.03417435944610275333, 13.17214151599831595 ) ) ;
#23450 = CIRCLE ( 'NONE', #61748, 19.99999999999999645 ) ;
#23451 = CARTESIAN_POINT ( 'NONE',  ( 18.52753015748617571, 33.09226448433411605, 4.923371831947298993 ) ) ;
#23452 = CARTESIAN_POINT ( 'NONE',  ( 19.72487221294571569, 54.78217586085238366, 6.499999999999995559 ) ) ;
#23454 = CARTESIAN_POINT ( 'NONE',  ( 0.6178305044545818747, 43.49863466993042493, -9.382169495545419124 ) ) ;
#23453 = CARTESIAN_POINT ( 'NONE',  ( 14.02068044289385718, 14.49999999999999112, -5.331089937175661930 ) ) ;
#23455 = EDGE_CURVE ( 'NONE', #37561, #86252, #46060, .T. ) ;
#23457 = DIRECTION ( 'NONE',  ( 0.000000000000000000, 1.000000000000000000, 0.000000000000000000 ) ) ;
#23456 = CARTESIAN_POINT ( 'NONE',  ( 0.1532563361054100626, 20.80059781766744464, -2.638427012816831230 ) ) ;
#23458 = DIRECTION ( 'NONE',  ( 0.2334453638559024768, 0.000000000000000000, 0.9723699203976773342 ) ) ;
#23460 = VERTEX_POINT ( 'NONE', #31154 ) ;
#23459 = CARTESIAN_POINT ( 'NONE',  ( 2.791683348922240793, 51.63393115100078745, 7.208316651077764092 ) ) ;
#23461 = CARTESIAN_POINT ( 'NONE',  ( 10.00000000000000000, 62.87363466993042493, -12.81628187352647608 ) ) ;
#23462 = CARTESIAN_POINT ( 'NONE',  ( -1.457314710996519436, 0.000000000000000000, -5.254907083456964223 ) ) ;
#23463 = CARTESIAN_POINT ( 'NONE',  ( 19.38216949554541202, 5.998634669930420493, 9.382169495545424454 ) ) ;
#23464 = CARTESIAN_POINT ( 'NONE',  ( 4.559911319644449179, 53.89701867748817676, 9.422509992056141925 ) ) ;
#23465 = AXIS2_PLACEMENT_3D ( 'NONE', #38695, #69194, #67716 ) ;
#23466 = CARTESIAN_POINT ( 'NONE',  ( 10.00000000000000178, 38.05374883491396787, 14.16423886937410082 ) ) ;
#23467 = CARTESIAN_POINT ( 'NONE',  ( 2.791683348922237240, 0.3839311510007847872, -7.208316651077763204 ) ) ;
#23468 = DIRECTION ( 'NONE',  ( 0.06975647374412567714, 0.9975640502598243087, 0.000000000000000000 ) ) ;
#23469 = CARTESIAN_POINT ( 'NONE',  ( 22.26659068614894466, 33.88708216824730357, 7.082119434687054849 ) ) ;
#23470 = EDGE_CURVE ( 'NONE', #93321, #14585, #6406, .T. ) ;
#23471 = CARTESIAN_POINT ( 'NONE',  ( 10.00000000000000178, 53.05374883491396787, 14.16423886937410082 ) ) ;
#23472 = CARTESIAN_POINT ( 'NONE',  ( 24.16423886937409904, 29.09541550158063572, 3.795296366450317205 ) ) ;
#23474 = CARTESIAN_POINT ( 'NONE',  ( 19.05866839779138644, 35.95508385108959004, -6.499999999999965361 ) ) ;
#23473 = CARTESIAN_POINT ( 'NONE',  ( 6.204703633549690345, 25.76208216824730712, -14.16423886937410259 ) ) ;
#23475 = CARTESIAN_POINT ( 'NONE',  ( 4.722628015970558479, -9.822377395415374579, -3.750000000000000888 ) ) ;
#23477 = CARTESIAN_POINT ( 'NONE',  ( 0.1532563361054083140, 46.00893115100079456, 1.131784320476157264E-15 ) ) ;
#23476 = CARTESIAN_POINT ( 'NONE',  ( 5.678900477199343655, -28.62996443930155266, 2.750000000000000000 ) ) ;
#23478 = VECTOR ( 'NONE', #16735, 1000.000000000000227 ) ;
#23479 = VERTEX_POINT ( 'NONE', #39672 ) ;
#23480 = CARTESIAN_POINT ( 'NONE',  ( 12.91533473730993009, 21.60535201082150536, -10.88017736071109987 ) ) ;
#23481 = CARTESIAN_POINT ( 'NONE',  ( -12.69000000000001371, 93.50000000000000000, -10.09898361729590199 ) ) ;
#23482 = CARTESIAN_POINT ( 'NONE',  ( 7.361572987183169658, 59.96726448433410894, -9.846743663894592657 ) ) ;
#23483 = CARTESIAN_POINT ( 'NONE',  ( 0.1532563361054082862, 36.21726448433410894, 2.638427012816831674 ) ) ;
#23484 = CARTESIAN_POINT ( 'NONE',  ( -2.816281873526471635, 53.91530133659709634, -3.434112377981056508 ) ) ;
#23485 = CARTESIAN_POINT ( 'NONE',  ( 3.469446951953614189E-15, -6.946251165086028578, 14.16423886937410259 ) ) ;
#23486 = VECTOR ( 'NONE', #83637, 1000.000000000000000 ) ;
#23487 = CARTESIAN_POINT ( 'NONE',  ( 5.076628168052704559, 45.17559781766745175, -8.527530157486179263 ) ) ;
#23488 = CARTESIAN_POINT ( 'NONE',  ( 1.472469842513823179, 56.42559781766745886, 4.923371831947296329 ) ) ;
#23489 = CARTESIAN_POINT ( 'NONE',  ( -0.3689425029237898834, 41.17874883491397497, -10.36894250292378850 ) ) ;
#23490 = PRESENTATION_LAYER_ASSIGNMENT (  '', '', ( #10692 ) ) ;
#23491 = VERTEX_POINT ( 'NONE', #33972 ) ;
#23492 = CARTESIAN_POINT ( 'NONE',  ( 20.36894250292379738, 9.928748834913966093, -10.36894250292379027 ) ) ;
#23493 = CARTESIAN_POINT ( 'NONE',  ( 12.91533473730992121, 59.52201867748816966, 10.88017736071110164 ) ) ;
#23494 = CARTESIAN_POINT ( 'NONE',  ( -4.164238869374098151, 61.59541550158063217, -3.795296366450310543 ) ) ;
#23495 = CARTESIAN_POINT ( 'NONE',  ( 10.00000000000000000, 17.87363466993041783, -12.81628187352647608 ) ) ;
#23496 = CARTESIAN_POINT ( 'NONE',  ( 15.44008868035555793, 61.39701867748817676, -9.422509992056140149 ) ) ;
#23497 = CARTESIAN_POINT ( 'NONE',  ( 4.441537491530695547, -2.700695904843435802, -4.000000000000000000 ) ) ;
#23498 = DIRECTION ( 'NONE',  ( 1.000000000000000000, 0.000000000000000000, 0.000000000000000000 ) ) ;
#23499 = CARTESIAN_POINT ( 'NONE',  ( 6.565887622018943937, 30.16530133659708568, 12.81628187352647430 ) ) ;
#23500 = CARTESIAN_POINT ( 'NONE',  ( 17.08211943468705840, 65.13708216824730357, -12.26659068614894466 ) ) ;
#23501 = DIRECTION ( 'NONE',  ( -5.818595309480553908E-17, -1.000000000000000000, -0.000000000000000000 ) ) ;
#23502 = CARTESIAN_POINT ( 'NONE',  ( 2.035157376598824452, 28.68868534415484106, 7.964842623401179544 ) ) ;
#23503 = CARTESIAN_POINT ( 'NONE',  ( 15.44008868035555260, 24.73035201082150891, 9.422509992056143702 ) ) ;
#23504 = CARTESIAN_POINT ( 'NONE',  ( 12.63842701281683034, 57.46726448433411605, 9.846743663894596210 ) ) ;
#23505 = CARTESIAN_POINT ( 'NONE',  ( 10.00000000000000178, 57.25893115100078745, 9.846743663894594434 ) ) ;
#23506 = CARTESIAN_POINT ( 'NONE',  ( -2.816281873526471635, 48.91530133659708213, -3.434112377981056508 ) ) ;
#23507 = PRESENTATION_STYLE_ASSIGNMENT (( #69482 ) ) ;
#23508 = ORIENTED_EDGE ( 'NONE', *, *, #6093, .F. ) ;
#23509 = CARTESIAN_POINT ( 'NONE',  ( 4.559911319644449179, 22.23035201082150536, -9.422509992056141925 ) ) ;
#23510 = EDGE_CURVE ( 'NONE', #24815, #64665, #77643, .T. ) ;
#23511 = CARTESIAN_POINT ( 'NONE',  ( 3.591859063236763294, 13.29030133659708746, -11.09922568453595026 ) ) ;
#23512 = CARTESIAN_POINT ( 'NONE',  ( -13.74385066382887466, 14.76930270348882779, 5.860428621090259860 ) ) ;
#23513 = CARTESIAN_POINT ( 'NONE',  ( 7.361572987183169658, 49.96726448433410894, -9.846743663894592657 ) ) ;
#23514 = EDGE_CURVE ( 'NONE', #39776, #81069, #37116, .T. ) ;
#23515 = CARTESIAN_POINT ( 'NONE',  ( 19.42250999205614193, 45.14701867748817676, 5.440088680355555262 ) ) ;
#23516 = CIRCLE ( 'NONE', #81011, 14.49999999999999822 ) ;
#23517 = CARTESIAN_POINT ( 'NONE',  ( -2.816281873526471635, 23.91530133659708568, -3.434112377981056508 ) ) ;
#23519 = CARTESIAN_POINT ( 'NONE',  ( 0.7375392941518293943, 0.5000000000000004441, -14.98185688723470932 ) ) ;
#23518 = CARTESIAN_POINT ( 'NONE',  ( 17.96484262340118221, 66.18868534415483396, -7.964842623401177768 ) ) ;
#23520 = SURFACE_STYLE_USAGE ( .BOTH. , #39497 ) ;
#23521 = ORIENTED_EDGE ( 'NONE', *, *, #78131, .T. ) ;
#23522 = DIRECTION ( 'NONE',  ( 0.000000000000000000, 0.000000000000000000, -1.000000000000000000 ) ) ;
#23523 = CARTESIAN_POINT ( 'NONE',  ( 10.00000000000000178, 44.31368534415484106, 10.88017736071110342 ) ) ;
#23525 = CARTESIAN_POINT ( 'NONE',  ( 2.917880565312948704, 12.63708216824730179, 12.26659068614894643 ) ) ;
#23524 = CARTESIAN_POINT ( 'NONE',  ( 3.591859063236763294, 48.29030133659708923, -11.09922568453595026 ) ) ;
#23526 = CARTESIAN_POINT ( 'NONE',  ( 5.076628168052704559, 10.17559781766745175, -8.527530157486179263 ) ) ;
#23527 = CARTESIAN_POINT ( 'NONE',  ( 10.00000000000000178, 67.25893115100079456, 9.846743663894594434 ) ) ;
#23528 = CARTESIAN_POINT ( 'NONE',  ( 7.361572987183169658, 4.967264484334119601, -9.846743663894592657 ) ) ;
#23529 = DIRECTION ( 'NONE',  ( -1.000000000000000000, 0.000000000000000000, 0.000000000000000000 ) ) ;
#23530 = CARTESIAN_POINT ( 'NONE',  ( -4.164238869374098151, 41.59541550158061796, -3.795296366450310543 ) ) ;
#23531 = LINE ( 'NONE', #84998, #87286 ) ;
#23532 = CARTESIAN_POINT ( 'NONE',  ( 20.88017736071110875, 5.772018677488170546, -2.915334737309920765 ) ) ;
#23533 = DIRECTION ( 'NONE',  ( -0.000000000000000000, -1.000000000000000000, -0.000000000000000000 ) ) ;
#23534 = VERTEX_POINT ( 'NONE', #91675 ) ;
#23535 = ORIENTED_EDGE ( 'NONE', *, *, #89345, .F. ) ;
#23536 = CARTESIAN_POINT ( 'NONE',  ( 17.96484262340118221, 4.938685344154837509, 7.964842623401181321 ) ) ;
#23537 = CARTESIAN_POINT ( 'NONE',  ( 19.42250999205614548, 5.980352010821504471, -5.440088680355545492 ) ) ;
#23538 = CARTESIAN_POINT ( 'NONE',  ( 14.92337183194729633, 37.67559781766745175, 8.527530157486181039 ) ) ;
#23539 = EDGE_CURVE ( 'NONE', #46963, #19684, #94493, .T. ) ;
#23540 = CARTESIAN_POINT ( 'NONE',  ( 13.43411237798106583, 32.66530133659708213, -12.81628187352647252 ) ) ;
#23541 = CARTESIAN_POINT ( 'NONE',  ( -18.00000000000000355, 75.73428692542562146, 2.900000000000000355 ) ) ;
#23543 = CARTESIAN_POINT ( 'NONE',  ( 10.00000000000000178, 3.053748834913967425, 14.16423886937410082 ) ) ;
#23542 = CARTESIAN_POINT ( 'NONE',  ( -10.19513985507843223, 14.49999999999999112, 11.00268709613216522 ) ) ;
#23544 = CARTESIAN_POINT ( 'NONE',  ( 0.5774900079438590739, 27.64701867748817676, -5.440088680355550821 ) ) ;
#23545 = CARTESIAN_POINT ( 'NONE',  ( 7.084665262690076126, 7.022018677488170546, -10.88017736071110164 ) ) ;
#23546 = CARTESIAN_POINT ( 'NONE',  ( 17.20831665107776587, 37.88393115100078745, 7.208316651077764980 ) ) ;
#23547 = CYLINDRICAL_SURFACE ( 'NONE', #18896, 1.249999999999987121 ) ;
#23548 = CARTESIAN_POINT ( 'NONE',  ( 12.63842701281683922, 19.55059781766745175, -9.846743663894590881 ) ) ;
#23549 = EDGE_CURVE ( 'NONE', #39290, #61288, #10898, .T. ) ;
#23550 = B_SPLINE_CURVE_WITH_KNOTS ( 'NONE', 3,
 ( #81135, #73628, #12638, #95145, #26655, #27141 ),
 .UNSPECIFIED., .F., .F.,
 ( 4, 2, 4 ),
 ( 0.0002800170536516727576, 0.0006862224498868463134, 0.001092427846122019869 ),
 .UNSPECIFIED. ) ;
#23551 = CARTESIAN_POINT ( 'NONE',  ( 10.00000000000000000, -0.2410688489992152128, -9.846743663894594434 ) ) ;
#23552 = CARTESIAN_POINT ( 'NONE',  ( -2.638427012816824124, 32.05059781766745886, 9.846743663894596210 ) ) ;
#23553 = ORIENTED_EDGE ( 'NONE', *, *, #46190, .F. ) ;
#23554 = DIRECTION ( 'NONE',  ( -0.000000000000000000, 1.000000000000000000, -0.000000000000000000 ) ) ;
#23555 = ORIENTED_EDGE ( 'NONE', *, *, #69909, .T. ) ;
#23556 = CARTESIAN_POINT ( 'NONE',  ( 19.84674366389459621, 53.50893115100078745, 7.409399052514197653E-17 ) ) ;
#23558 = CARTESIAN_POINT ( 'NONE',  ( 12.91533473730993009, 41.60535201082149825, -10.88017736071109987 ) ) ;
#23557 = CARTESIAN_POINT ( 'NONE',  ( -0.8801773607110991993, 32.85535201082151247, -2.915334737309923874 ) ) ;
#23560 = CARTESIAN_POINT ( 'NONE',  ( -2.816281873526471635, 33.91530133659708213, -3.434112377981056508 ) ) ;
#23559 = CARTESIAN_POINT ( 'NONE',  ( 2.035157376598822676, 2.438685344154837953, -7.964842623401177768 ) ) ;
#23561 = CARTESIAN_POINT ( 'NONE',  ( 20.36894250292379738, 14.92874883491396432, -10.36894250292379027 ) ) ;
#23562 = VECTOR ( 'NONE', #84679, 1000.000000000000000 ) ;
#23563 = CIRCLE ( 'NONE', #82624, 3.690000000000000391 ) ;
#23564 = CARTESIAN_POINT ( 'NONE',  ( 3.591859063236763294, 48.29030133659708923, -11.09922568453595026 ) ) ;
#23565 = ORIENTED_EDGE ( 'NONE', *, *, #96580, .T. ) ;
#23566 = CARTESIAN_POINT ( 'NONE',  ( 17.20831665107776587, 42.88393115100077324, 7.208316651077764980 ) ) ;
#23567 = CARTESIAN_POINT ( 'NONE',  ( 15.44008868035555260, 24.73035201082150891, 9.422509992056143702 ) ) ;
#23568 = VERTEX_POINT ( 'NONE', #54153 ) ;
#23569 = CARTESIAN_POINT ( 'NONE',  ( 2.035157376598822676, 17.43868534415483751, -7.964842623401177768 ) ) ;
#23570 = EDGE_LOOP ( 'NONE', ( #10616, #97753, #81261 ) ) ;
#23571 = CARTESIAN_POINT ( 'NONE',  ( 0.5774900079438607392, 58.48035201082151247, 5.440088680355550821 ) ) ;
#23572 = CARTESIAN_POINT ( 'NONE',  ( -0.8801773607110991993, 67.85535201082151957, -2.915334737309923874 ) ) ;
#23573 = CARTESIAN_POINT ( 'NONE',  ( -0.8801773607111008646, 68.27201867748817676, 2.915334737309923430 ) ) ;
#23574 = CARTESIAN_POINT ( 'NONE',  ( 1.472469842513823179, 10.59226448433411782, -4.923371831947296329 ) ) ;
#23575 = CARTESIAN_POINT ( 'NONE',  ( 14.92337183194729988, 4.342264484334117824, -8.527530157486177487 ) ) ;
#23576 = CARTESIAN_POINT ( 'NONE',  ( -4.431036607602660382, 0.5000000000000004441, 14.33059365769907956 ) ) ;
#23577 = ADVANCED_FACE ( 'NONE', ( #35465 ), #39966, .T. ) ;
#23579 = ORIENTED_EDGE ( 'NONE', *, *, #72024, .F. ) ;
#23578 = CARTESIAN_POINT ( 'NONE',  ( 10.00000000000000000, 9.758931151000785675, -9.846743663894594434 ) ) ;
#23580 = CARTESIAN_POINT ( 'NONE',  ( 1.472469842513823179, 45.59226448433412315, -4.923371831947296329 ) ) ;
#23581 = ORIENTED_EDGE ( 'NONE', *, *, #65000, .F. ) ;
#23582 = VERTEX_POINT ( 'NONE', #26981 ) ;
#23583 = CYLINDRICAL_SURFACE ( 'NONE', #74562, 15.00000000000000000 ) ;
#23584 = DIRECTION ( 'NONE',  ( -1.000000000000000000, -0.000000000000000000, 0.000000000000000000 ) ) ;
#23585 =( GEOMETRIC_REPRESENTATION_CONTEXT ( 3 ) GLOBAL_UNCERTAINTY_ASSIGNED_CONTEXT ( ( #3458 ) ) GLOBAL_UNIT_ASSIGNED_CONTEXT ( ( #32392, #95873, #41412 ) ) REPRESENTATION_CONTEXT ( 'NONE', 'WORKASPACE' ) );
#23586 = CARTESIAN_POINT ( 'NONE',  ( -14.97687855664607248, 15.00000000000000000, -0.8325315005902533816 ) ) ;
#23587 = CARTESIAN_POINT ( 'NONE',  ( 10.00000000000000000, 15.55374883491396787, -14.16423886937410082 ) ) ;
#23588 = AXIS2_PLACEMENT_3D ( 'NONE', #91198, #22723, #83711 ) ;
#23589 = CARTESIAN_POINT ( 'NONE',  ( -0.1503990784575328643, 35.12777174578612716, 6.262539305110068177 ) ) ;
#23591 = CARTESIAN_POINT ( 'NONE',  ( 19.42250999205614548, 60.98035201082151247, -5.440088680355545492 ) ) ;
#23590 = CARTESIAN_POINT ( 'NONE',  ( 0.000000000000000000, 0.5000000000000000000, 6.500000000000000888 ) ) ;
#23592 = CARTESIAN_POINT ( 'NONE',  ( 19.42250999205614193, 20.14701867748817321, 5.440088680355555262 ) ) ;
#23593 = CARTESIAN_POINT ( 'NONE',  ( 0.000000000000000000, -97.00000000000000000, 4.000000000000000000 ) ) ;
#23594 = VERTEX_POINT ( 'NONE', #58960 ) ;
#23595 = CARTESIAN_POINT ( 'NONE',  ( 18.52753015748618282, 3.925597817667451306, -4.923371831947291888 ) ) ;
#23596 = CARTESIAN_POINT ( 'NONE',  ( 1.472469842513823179, 0.5922644843341181575, -4.923371831947296329 ) ) ;
#23597 = CARTESIAN_POINT ( 'NONE',  ( -2.816281873526473856, 29.12363466993041783, 9.499525473075851096E-16 ) ) ;
#23598 = CARTESIAN_POINT ( 'NONE',  ( 0.1532563361054083140, 26.00893115100078745, 1.131784320476157264E-15 ) ) ;
#23599 =( LENGTH_UNIT ( ) NAMED_UNIT ( * ) SI_UNIT ( .MILLI., .METRE. ) );
#23600 = CARTESIAN_POINT ( 'NONE',  ( -2.816281873526471635, 18.91530133659708213, -3.434112377981056508 ) ) ;
#23601 = MECHANICAL_DESIGN_GEOMETRIC_PRESENTATION_REPRESENTATION (  '', ( #74682 ), #12434 ) ;
#23602 = CARTESIAN_POINT ( 'NONE',  ( 19.84674366389459621, 3.508931151000785231, 7.409399052514197653E-17 ) ) ;
#23603 = ORIENTED_EDGE ( 'NONE', *, *, #92151, .T. ) ;
#23604 = VERTEX_POINT ( 'NONE', #20976 ) ;
#23605 = CARTESIAN_POINT ( 'NONE',  ( 4.559911319644449179, 17.23035201082150536, -9.422509992056141925 ) ) ;
#23606 = CARTESIAN_POINT ( 'NONE',  ( 2.917880565312948704, 12.63708216824730179, 12.26659068614894643 ) ) ;
#23607 = CARTESIAN_POINT ( 'NONE',  ( 10.00000000000000000, 34.75893115100078745, -9.846743663894594434 ) ) ;
#23608 = EDGE_CURVE ( 'NONE', #54278, #25526, #90760, .T. ) ;
#23609 = CARTESIAN_POINT ( 'NONE',  ( 20.88017736071110164, 65.35535201082150536, 2.915334737309930979 ) ) ;
#23611 = PLANE ( 'NONE',  #33607 ) ;
#23610 = CARTESIAN_POINT ( 'NONE',  ( 22.81628187352647785, 41.41530133659708923, 3.434112377981063169 ) ) ;
#23612 = CARTESIAN_POINT ( 'NONE',  ( -0.8801773607110991993, 22.85535201082150181, -2.915334737309923874 ) ) ;
#23613 = DIRECTION ( 'NONE',  ( -0.000000000000000000, -1.000000000000000000, -0.000000000000000000 ) ) ;
#23614 = VECTOR ( 'NONE', #18732, 1000.000000000000000 ) ;
#23615 = CARTESIAN_POINT ( 'NONE',  ( 6.565887622018943937, 15.16530133659708568, 12.81628187352647430 ) ) ;
#23616 = CARTESIAN_POINT ( 'NONE',  ( -2.816281873526473856, 14.33196800326375531, 3.434112377981055619 ) ) ;
#23617 = CARTESIAN_POINT ( 'NONE',  ( 5.076628168052703671, 46.84226448433412315, 8.527530157486179263 ) ) ;
#23618 = CARTESIAN_POINT ( 'NONE',  ( -2.915334737309917656, -0.8946479891784895333, 10.88017736071110164 ) ) ;
#23619 = CARTESIAN_POINT ( 'NONE',  ( -2.816281873526473856, 54.12363466993041783, 9.499525473075851096E-16 ) ) ;
#23620 = SURFACE_SIDE_STYLE ('',( #3080 ) ) ;
#23622 = CARTESIAN_POINT ( 'NONE',  ( 12.26500600480480863, -7.132017415881208855E-16, 0.000000000000000000 ) ) ;
#23621 = CARTESIAN_POINT ( 'NONE',  ( 12.91533473730992121, 54.52201867748816255, 10.88017736071110164 ) ) ;
#23623 = AXIS2_PLACEMENT_3D ( 'NONE', #98386, #7369, #54315 ) ;
#23624 = VECTOR ( 'NONE', #6733, 999.9999999999998863 ) ;
#23625 = CARTESIAN_POINT ( 'NONE',  ( 13.75801628063881488, 4.740223025775510804E-16, -4.578972376164461622 ) ) ;
#23626 = FILL_AREA_STYLE_COLOUR ( '', #47998 ) ;
#23627 = AXIS2_PLACEMENT_3D ( 'NONE', #49689, #3728, #34189 ) ;
#23628 = CARTESIAN_POINT ( 'NONE',  ( 0.5774900079438607392, 43.48035201082151247, 5.440088680355550821 ) ) ;
#23629 = CARTESIAN_POINT ( 'NONE',  ( 20.88017736071110519, 50.56368534415484106, 2.639326808657452039E-16 ) ) ;
#23630 = CARTESIAN_POINT ( 'NONE',  ( 2.791683348922237240, 65.38393115100078035, -7.208316651077763204 ) ) ;
#23631 = CARTESIAN_POINT ( 'NONE',  ( 19.42250999205614193, 65.14701867748817676, 5.440088680355555262 ) ) ;
#23632 = EDGE_CURVE ( 'NONE', #27600, #6181, #59143, .T. ) ;
#23633 = EDGE_CURVE ( 'NONE', #20168, #89098, #24019, .T. ) ;
#23634 = CARTESIAN_POINT ( 'NONE',  ( 1.472469842513823179, 56.42559781766745886, 4.923371831947296329 ) ) ;
#23636 = CARTESIAN_POINT ( 'NONE',  ( -10.14667048435152097, 4.576487713787624877E-16, 10.35833375027034542 ) ) ;
#23635 = CARTESIAN_POINT ( 'NONE',  ( 17.96484262340118221, 11.18868534415483929, -7.964842623401177768 ) ) ;
#23637 = CARTESIAN_POINT ( 'NONE',  ( 22.81628187352647785, 11.62363466993042138, 6.195893100308588602E-16 ) ) ;
#23638 = ORIENTED_EDGE ( 'NONE', *, *, #98139, .F. ) ;
#23639 = CARTESIAN_POINT ( 'NONE',  ( 4.559911319644449179, 38.89701867748817676, 9.422509992056141925 ) ) ;
#23641 = DIRECTION ( 'NONE',  ( -5.818595309480553908E-17, -1.000000000000000000, -0.000000000000000000 ) ) ;
#23640 = CARTESIAN_POINT ( 'NONE',  ( 0.6178305044545838731, 9.748634669930416052, 9.382169495545420901 ) ) ;
#23642 = CARTESIAN_POINT ( 'NONE',  ( 20.88017736071110875, 15.77201867748817143, -2.915334737309920765 ) ) ;
#23643 = CARTESIAN_POINT ( 'NONE',  ( 10.00000000000000178, 29.31368534415483751, 10.88017736071110342 ) ) ;
#23644 = CARTESIAN_POINT ( 'NONE',  ( -2.266590686148945544, 31.38708216824730002, -7.082119434687050408 ) ) ;
#23645 = CARTESIAN_POINT ( 'NONE',  ( 14.92337183194729633, 27.67559781766745530, 8.527530157486181039 ) ) ;
#23646 = CARTESIAN_POINT ( 'NONE',  ( 17.96484262340118221, 61.18868534415482685, -7.964842623401177768 ) ) ;
#23647 = LINE ( 'NONE', #16620, #23486 ) ;
#23648 = CARTESIAN_POINT ( 'NONE',  ( 17.08211943468705130, 8.470415501580635720, 12.26659068614894998 ) ) ;
#23649 = CARTESIAN_POINT ( 'NONE',  ( -46.91882540200030860, 103.2386372682362179, 5.912220560523961055 ) ) ;
#23650 = CARTESIAN_POINT ( 'NONE',  ( 10.00000000000000000, 59.75893115100078745, -9.846743663894594434 ) ) ;
#23651 = ORIENTED_EDGE ( 'NONE', *, *, #67474, .F. ) ;
#23652 = B_SPLINE_CURVE_WITH_KNOTS ( 'NONE', 3,
 ( #48971, #79479, #65441, #95965 ),
 .UNSPECIFIED., .F., .F.,
 ( 4, 4 ),
 ( 1.876390332415650501E-16, 0.001060528352562002848 ),
 .UNSPECIFIED. ) ;
#23653 = CARTESIAN_POINT ( 'NONE',  ( 24.16423886937410614, 29.51208216824729647, -3.795296366450302550 ) ) ;
#23654 = CARTESIAN_POINT ( 'NONE',  ( -4.164238869374099039, 36.80374883491396787, 8.674139862899312516E-16 ) ) ;
#23655 = CARTESIAN_POINT ( 'NONE',  ( 10.00000000000000178, 7.258931151000785675, 9.846743663894594434 ) ) ;
#23656 = CARTESIAN_POINT ( 'NONE',  ( 5.076628168052703671, 56.84226448433412315, 8.527530157486179263 ) ) ;
#23657 = CARTESIAN_POINT ( 'NONE',  ( -10.07339213347369444, -32.14942050451527678, 4.000000000000000000 ) ) ;
#23659 = CARTESIAN_POINT ( 'NONE',  ( 0.6178305044545838731, 24.74863466993042493, 9.382169495545420901 ) ) ;
#23658 = CARTESIAN_POINT ( 'NONE',  ( 17.96484262340118221, 59.93868534415484106, 7.964842623401181321 ) ) ;
#23660 = CARTESIAN_POINT ( 'NONE',  ( -2.266590686148945544, 32.22041550158063927, 7.082119434687048631 ) ) ;
#23661 = CARTESIAN_POINT ( 'NONE',  ( 7.084665262690076126, 12.02201867748817321, -10.88017736071110164 ) ) ;
#23662 = CARTESIAN_POINT ( 'NONE',  ( -0.8801773607110991993, 32.85535201082151247, -2.915334737309923874 ) ) ;
#23663 = CARTESIAN_POINT ( 'NONE',  ( -0.1503990784575328643, 70.00000000000000000, -6.262539305110068177 ) ) ;
#23664 = CARTESIAN_POINT ( 'NONE',  ( 10.00000000000000000, 51.81368534415484106, -10.88017736071110342 ) ) ;
#23665 = EDGE_CURVE ( 'NONE', #78252, #72885, #9632, .T. ) ;
#23666 = CARTESIAN_POINT ( 'NONE',  ( 7.208316651077762316, -5.866068848999215213, -7.208316651077764980 ) ) ;
#23667 = ORIENTED_EDGE ( 'NONE', *, *, #90758, .T. ) ;
#23668 = DIRECTION ( 'NONE',  ( 0.9170600743851183845, 0.000000000000000000, 0.3987490689252593534 ) ) ;
#23669 = CARTESIAN_POINT ( 'NONE',  ( -0.2418659066527787949, 12.23410085661204150, -6.114288769123032985 ) ) ;
#23670 = ORIENTED_EDGE ( 'NONE', *, *, #24292, .T. ) ;
#23671 = CARTESIAN_POINT ( 'NONE',  ( 10.00000000000000000, 0.5537488349139675359, -14.16423886937410082 ) ) ;
#23673 = CARTESIAN_POINT ( 'NONE',  ( -4.164238869374098151, 61.59541550158063217, -3.795296366450310543 ) ) ;
#23672 = CARTESIAN_POINT ( 'NONE',  ( 13.79529636645030344, 58.26208216824728936, 14.16423886937410614 ) ) ;
#23675 = CARTESIAN_POINT ( 'NONE',  ( 0.1532563361054082862, 61.21726448433412315, 2.638427012816831674 ) ) ;
#23674 = CARTESIAN_POINT ( 'NONE',  ( 1.472469842513823179, 31.42559781766745530, 4.923371831947296329 ) ) ;
#23676 = CARTESIAN_POINT ( 'NONE',  ( 21.92686044187657046, 60.16212336850780673, 4.562052436263912550E-16 ) ) ;
#23677 = CARTESIAN_POINT ( 'NONE',  ( 4.629999999999999893, 4.857171655774867594E-16, -4.000000000000000000 ) ) ;
#23678 = CIRCLE ( 'NONE', #79537, 1.499999999999998668 ) ;
#23679 = CARTESIAN_POINT ( 'NONE',  ( 22.81628187352648496, 6.831968003263753531, -3.434112377981050290 ) ) ;
#23680 = CARTESIAN_POINT ( 'NONE',  ( 12.81628187352647608, 21.62363466993041783, -2.602085213965210642E-15 ) ) ;
#23681 = ORIENTED_EDGE ( 'NONE', *, *, #27099, .T. ) ;
#23682 = CARTESIAN_POINT ( 'NONE',  ( 6.204703633549690345, 47.84541550158064638, 14.16423886937410082 ) ) ;
#23683 = CARTESIAN_POINT ( 'NONE',  ( 24.16423886937409904, 44.09541550158063927, 3.795296366450317205 ) ) ;
#23684 = EDGE_LOOP ( 'NONE', ( #21599, #66305, #64836, #54068 ) ) ;
#23685 = CARTESIAN_POINT ( 'NONE',  ( 21.09922568453594849, 61.20696800326376064, 6.408140936763242479 ) ) ;
#23686 = COLOUR_RGB ( '', 0.31764706, 0.68627451, 0.89019608) ;
#23687 = CARTESIAN_POINT ( 'NONE',  ( 0.5774900079438607392, 23.48035201082150536, 5.440088680355550821 ) ) ;
#23688 = CARTESIAN_POINT ( 'NONE',  ( 14.92337183194729633, 47.67559781766745175, 8.527530157486181039 ) ) ;
#23689 = CARTESIAN_POINT ( 'NONE',  ( 12.91533473730993009, 31.60535201082150891, -10.88017736071109987 ) ) ;
#23690 = CARTESIAN_POINT ( 'NONE',  ( -4.818654718866499209, -24.96058166501294906, 2.499999999999999112 ) ) ;
#23691 = CARTESIAN_POINT ( 'NONE',  ( 7.361572987183170547, 52.05059781766745175, 9.846743663894590881 ) ) ;
#23692 = LINE ( 'NONE', #17658, #90492 ) ;
#23693 = PRESENTATION_LAYER_ASSIGNMENT (  '', '', ( #10892 ) ) ;
#23694 = EDGE_CURVE ( 'NONE', #54148, #37077, #20846, .T. ) ;
#23695 = AXIS2_PLACEMENT_3D ( 'NONE', #97577, #29038, #53025 ) ;
#23697 = VERTEX_POINT ( 'NONE', #80853 ) ;
#23696 = DIRECTION ( 'NONE',  ( -0.000000000000000000, 1.000000000000000000, -0.000000000000000000 ) ) ;
#23698 = LINE ( 'NONE', #54158, #74513 ) ;
#23699 = CARTESIAN_POINT ( 'NONE',  ( 12.63842701281683034, 7.467264484334118713, 9.846743663894596210 ) ) ;
#23700 = CARTESIAN_POINT ( 'NONE',  ( -18.89999999999999147, 91.25000000000000000, -8.000000000000000000 ) ) ;
#23701 = ORIENTED_EDGE ( 'NONE', *, *, #58102, .F. ) ;
#23702 = FILL_AREA_STYLE_COLOUR ( '', #56928 ) ;
#23703 = CARTESIAN_POINT ( 'NONE',  ( 0.1532563361054082862, 31.21726448433412315, 2.638427012816831674 ) ) ;
#23704 = CARTESIAN_POINT ( 'NONE',  ( 6.767445849361160448, 14.49999999999999112, 13.38662304974508110 ) ) ;
#23705 =( NAMED_UNIT ( * ) PLANE_ANGLE_UNIT ( ) SI_UNIT ( $, .RADIAN. ) );
#23706 = LINE ( 'NONE', #33133, #34716 ) ;
#23707 = EDGE_LOOP ( 'NONE', ( #69622, #30924, #98727, #27975 ) ) ;
#23708 = CARTESIAN_POINT ( 'NONE',  ( -9.705452947461587598, 2.500000000000008438, -5.689172442861014645 ) ) ;
#23709 = CARTESIAN_POINT ( 'NONE',  ( 15.00000000000000000, 77.07179676972447169, 6.500000000000000888 ) ) ;
#23710 = CARTESIAN_POINT ( 'NONE',  ( 12.63842701281683922, 59.55059781766744464, -9.846743663894590881 ) ) ;
#23711 = CARTESIAN_POINT ( 'NONE',  ( 13.79529636645030344, 33.26208216824730357, 14.16423886937410614 ) ) ;
#23712 = CARTESIAN_POINT ( 'NONE',  ( 18.52753015748617571, 53.09226448433412315, 4.923371831947298993 ) ) ;
#23713 = CARTESIAN_POINT ( 'NONE',  ( -11.36220558718850882, 3.877685541201178108E-16, -9.008345252845398221 ) ) ;
#23714 = CARTESIAN_POINT ( 'NONE',  ( 2.791683348922237240, 25.38393115100078390, -7.208316651077763204 ) ) ;
#23715 = CARTESIAN_POINT ( 'NONE',  ( 19.38216949554541557, 57.24863466993042493, -9.382169495545420901 ) ) ;
#23716 = CARTESIAN_POINT ( 'NONE',  ( 22.26659068614895176, 4.720415501580633943, -7.082119434687042414 ) ) ;
#23717 = ADVANCED_FACE ( 'NONE', ( #36335 ), #57506, .T. ) ;
#23718 = CARTESIAN_POINT ( 'NONE',  ( 2.791683348922240793, 66.63393115100079456, 7.208316651077764092 ) ) ;
#23719 = CARTESIAN_POINT ( 'NONE',  ( -0.8801773607110991993, 47.85535201082150536, -2.915334737309923874 ) ) ;
#23720 = CARTESIAN_POINT ( 'NONE',  ( 19.84674366389459621, 38.50893115100078745, 7.409399052514197653E-17 ) ) ;
#23721 = CARTESIAN_POINT ( 'NONE',  ( 6.905552584539410788, -69.44516986207491982, -2.750000000000000444 ) ) ;
#23722 = ORIENTED_EDGE ( 'NONE', *, *, #54271, .T. ) ;
#23723 = CARTESIAN_POINT ( 'NONE',  ( 2.603489959281614308, 51.58210964143330557, 6.500000000000031086 ) ) ;
#23724 = CARTESIAN_POINT ( 'NONE',  ( 20.88017736071110875, 25.77201867748816966, -2.915334737309920765 ) ) ;
#23726 = CARTESIAN_POINT ( 'NONE',  ( 12.91533473730993009, 56.60535201082151247, -10.88017736071109987 ) ) ;
#23725 = CARTESIAN_POINT ( 'NONE',  ( 0.1532563361054100626, 65.80059781766745175, -2.638427012816831230 ) ) ;
#23727 = CARTESIAN_POINT ( 'NONE',  ( 20.88017736071110519, 65.56368534415483396, 2.639326808657452039E-16 ) ) ;
#23728 = CARTESIAN_POINT ( 'NONE',  ( -5.200846386093647133, 0.000000000000000000, 1.639820566680907588 ) ) ;
#23729 = DIRECTION ( 'NONE',  ( 0.000000000000000000, 0.000000000000000000, -1.000000000000000000 ) ) ;
#23731 = DIRECTION ( 'NONE',  ( -1.000000000000000000, 0.000000000000000000, 0.000000000000000000 ) ) ;
#23730 = CARTESIAN_POINT ( 'NONE',  ( 0.5774900079438607392, 33.48035201082150536, 5.440088680355550821 ) ) ;
#23732 = CARTESIAN_POINT ( 'NONE',  ( 18.52753015748618282, 43.92559781766745175, -4.923371831947291888 ) ) ;
#23733 = SURFACE_STYLE_FILL_AREA ( #29721 ) ;
#23734 = CARTESIAN_POINT ( 'NONE',  ( -10.36894250292379205, 21.17874883491397497, -10.36894250292378672 ) ) ;
#23735 = CARTESIAN_POINT ( 'NONE',  ( 13.43411237798106583, 7.665301336597086568, -12.81628187352647252 ) ) ;
#23736 = EDGE_CURVE ( 'NONE', #73066, #74650, #61010, .T. ) ;
#23737 = CARTESIAN_POINT ( 'NONE',  ( 17.96484262340118221, 19.93868534415484106, 7.964842623401181321 ) ) ;
#23738 = SURFACE_SIDE_STYLE ('',( #7245 ) ) ;
#23739 = CARTESIAN_POINT ( 'NONE',  ( 10.00000000000000000, 20.55374883491396787, -14.16423886937410082 ) ) ;
#23740 = CARTESIAN_POINT ( 'NONE',  ( 22.26659068614895176, 64.72041550158064638, -7.082119434687042414 ) ) ;
#23741 = PRESENTATION_LAYER_ASSIGNMENT (  '', '', ( #54048 ) ) ;
#23742 = CARTESIAN_POINT ( 'NONE',  ( 10.00000000000000178, 12.25893115100078568, 9.846743663894594434 ) ) ;
#23743 = CARTESIAN_POINT ( 'NONE',  ( 20.10239578412225114, 32.63377557478297319, -6.340343622311915617 ) ) ;
#23744 = ADVANCED_FACE ( 'NONE', ( #57843 ), #54367, .T. ) ;
#23745 = VERTEX_POINT ( 'NONE', #13339 ) ;
#23746 = CARTESIAN_POINT ( 'NONE',  ( 7.361572987183169658, 19.96726448433411960, -9.846743663894592657 ) ) ;
#23747 = CARTESIAN_POINT ( 'NONE',  ( 17.96484262340118221, 26.18868534415483396, -7.964842623401177768 ) ) ;
#23748 = CARTESIAN_POINT ( 'NONE',  ( 2.791683348922237240, 65.38393115100078035, -7.208316651077763204 ) ) ;
#23749 = CARTESIAN_POINT ( 'NONE',  ( 2.917880565312948704, 12.63708216824730179, 12.26659068614894643 ) ) ;
#23750 = CARTESIAN_POINT ( 'NONE',  ( 8.879999999999991900, 27.04366094290857347, 3.000000000000000000 ) ) ;
#23751 = EDGE_CURVE ( 'NONE', #79627, #69540, #22417, .T. ) ;
#23752 = CARTESIAN_POINT ( 'NONE',  ( 17.20831665107776587, 12.88393115100078390, 7.208316651077764980 ) ) ;
#23753 = CARTESIAN_POINT ( 'NONE',  ( 3.591859063236763294, 43.29030133659708923, -11.09922568453595026 ) ) ;
#23754 = CARTESIAN_POINT ( 'NONE',  ( 7.361572987183170547, 42.05059781766745886, 9.846743663894590881 ) ) ;
#23755 = EDGE_LOOP ( 'NONE', ( #32187, #18398 ) ) ;
#23756 = CARTESIAN_POINT ( 'NONE',  ( 7.361572987183170547, 17.05059781766745530, 9.846743663894590881 ) ) ;
#23757 = DIRECTION ( 'NONE',  ( -4.205390244792255888E-16, 1.000000000000000000, 8.410780489584511775E-16 ) ) ;
#23758 = CARTESIAN_POINT ( 'NONE',  ( 24.16423886937410614, 49.30374883491396787, 8.672049930838204340E-16 ) ) ;
#23759 = CARTESIAN_POINT ( 'NONE',  ( 17.96484262340118221, 54.93868534415484106, 7.964842623401181321 ) ) ;
#23760 = PRESENTATION_LAYER_ASSIGNMENT (  '', '', ( #20524 ) ) ;
#23761 = CARTESIAN_POINT ( 'NONE',  ( 10.00000000000000178, 3.053748834913967425, 14.16423886937410082 ) ) ;
#23762 = CARTESIAN_POINT ( 'NONE',  ( 17.96484262340118221, 56.18868534415484817, -7.964842623401177768 ) ) ;
#23763 = CARTESIAN_POINT ( 'NONE',  ( 0.1532563361054082862, 36.21726448433410894, 2.638427012816831674 ) ) ;
#23764 = CARTESIAN_POINT ( 'NONE',  ( 10.00000000000000000, 6.813685344154838397, -10.88017736071110342 ) ) ;
#23765 = CARTESIAN_POINT ( 'NONE',  ( 19.84674366389459266, 48.30059781766745175, 2.638427012816836559 ) ) ;
#23766 = CARTESIAN_POINT ( 'NONE',  ( -0.8801773607110991993, 47.85535201082150536, -2.915334737309923874 ) ) ;
#23767 = ORIENTED_EDGE ( 'NONE', *, *, #39425, .T. ) ;
#23768 = VECTOR ( 'NONE', #23423, 1000.000000000000000 ) ;
#23769 = VERTEX_POINT ( 'NONE', #12350 ) ;
#23770 = VERTEX_POINT ( 'NONE', #42856 ) ;
#23771 = CARTESIAN_POINT ( 'NONE',  ( 4.600000000000003197, 98.49999999999998579, -8.525133428036873795 ) ) ;
#23772 =( NAMED_UNIT ( * ) PLANE_ANGLE_UNIT ( ) SI_UNIT ( $, .RADIAN. ) );
#23773 = CARTESIAN_POINT ( 'NONE',  ( 7.361572987183169658, 39.96726448433411605, -9.846743663894592657 ) ) ;
#23774 = CARTESIAN_POINT ( 'NONE',  ( 19.84674366389459621, 28.50893115100078745, 7.409399052514197653E-17 ) ) ;
#23775 = CARTESIAN_POINT ( 'NONE',  ( -1.099225684535947600, 58.70696800326375353, -6.408140936763238038 ) ) ;
#23777 = CARTESIAN_POINT ( 'NONE',  ( 1.472469842513823179, 50.59226448433411605, -4.923371831947296329 ) ) ;
#23776 = CARTESIAN_POINT ( 'NONE',  ( -0.8801773607111008646, 13.27201867748817321, 2.915334737309923430 ) ) ;
#23778 = CARTESIAN_POINT ( 'NONE',  ( 10.70613742633256926, 15.00000000000000000, -9.778988772285213571 ) ) ;
#23779 = CARTESIAN_POINT ( 'NONE',  ( 10.00000000000000178, 53.05374883491396787, 14.16423886937410082 ) ) ;
#23780 = CARTESIAN_POINT ( 'NONE',  ( 14.92337183194729988, 59.34226448433412315, -8.527530157486177487 ) ) ;
#23781 = CARTESIAN_POINT ( 'NONE',  ( 18.00000000000000000, 78.80384757729336798, 4.000000000000000000 ) ) ;
#23782 = CARTESIAN_POINT ( 'NONE',  ( 12.91533473730993009, 46.60535201082150536, -10.88017736071109987 ) ) ;
#23783 = EDGE_CURVE ( 'NONE', #50106, #73111, #58829, .T. ) ;
#23784 = CARTESIAN_POINT ( 'NONE',  ( 5.076628168052703671, 11.84226448433411960, 8.527530157486179263 ) ) ;
#23785 = CARTESIAN_POINT ( 'NONE',  ( -6.607869636366940469, -50.96183896326462559, 4.000000000003224088 ) ) ;
#23786 = AXIS2_PLACEMENT_3D ( 'NONE', #13209, #44191, #91177 ) ;
#23787 = ORIENTED_EDGE ( 'NONE', *, *, #88420, .F. ) ;
#23788 = LINE ( 'NONE', #54253, #57116 ) ;
#23789 = ORIENTED_EDGE ( 'NONE', *, *, #16094, .T. ) ;
#23790 = CARTESIAN_POINT ( 'NONE',  ( 17.20831665107776587, 14.13393115100078568, -7.208316651077762316 ) ) ;
#23791 = ORIENTED_EDGE ( 'NONE', *, *, #58336, .F. ) ;
#23792 = CARTESIAN_POINT ( 'NONE',  ( 6.204703633549690345, 22.84541550158062861, 14.16423886937410082 ) ) ;
#23793 = CARTESIAN_POINT ( 'NONE',  ( 7.361572987183170547, 22.05059781766745530, 9.846743663894590881 ) ) ;
#23794 = CARTESIAN_POINT ( 'NONE',  ( 7.084665262690076126, 42.02201867748816966, -10.88017736071110164 ) ) ;
#23795 = CARTESIAN_POINT ( 'NONE',  ( 3.881785064875274749, 15.00000000000000888, -14.10213074188652982 ) ) ;
#23797 = EDGE_CURVE ( 'NONE', #43121, #72571, #15337, .T. ) ;
#23796 = EDGE_LOOP ( 'NONE', ( #80289, #5809, #63714, #61125, #83307, #12818, #20721, #26235, #17917, #30348, #93017, #16846 ) ) ;
#23798 = CARTESIAN_POINT ( 'NONE',  ( 7.084665262690076126, 27.02201867748817676, -10.88017736071110164 ) ) ;
#23799 = CARTESIAN_POINT ( 'NONE',  ( -7.684764310694971456, 0.5000000000000004441, 12.88194075009929840 ) ) ;
#23800 = ORIENTED_EDGE ( 'NONE', *, *, #97888, .F. ) ;
#23801 =( NAMED_UNIT ( * ) PLANE_ANGLE_UNIT ( ) SI_UNIT ( $, .RADIAN. ) );
#23802 = ORIENTED_EDGE ( 'NONE', *, *, #33326, .T. ) ;
#23803 = ORIENTED_EDGE ( 'NONE', *, *, #4755, .F. ) ;
#23804 = CARTESIAN_POINT ( 'NONE',  ( 10.00000000000000000, 17.87363466993041783, -12.81628187352647608 ) ) ;
#23805 = CARTESIAN_POINT ( 'NONE',  ( 2.791683348922237240, 10.38393115100078390, -7.208316651077763204 ) ) ;
#23806 = CARTESIAN_POINT ( 'NONE',  ( 0.000000000000000000, 14.49999999999999822, 0.000000000000000000 ) ) ;
#23807 = CARTESIAN_POINT ( 'NONE',  ( -10.44000000000001194, 92.00000000000000000, -10.09898361729590199 ) ) ;
#23808 = CARTESIAN_POINT ( 'NONE',  ( 5.076628168052704559, 20.17559781766745175, -8.527530157486179263 ) ) ;
#23809 = CARTESIAN_POINT ( 'NONE',  ( 15.44008868035555260, 29.73035201082150891, 9.422509992056143702 ) ) ;
#23810 = ORIENTED_EDGE ( 'NONE', *, *, #25889, .T. ) ;
#23811 = DIRECTION ( 'NONE',  ( 2.107602052970794797E-16, -1.000000000000000000, 0.000000000000000000 ) ) ;
#23812 = CARTESIAN_POINT ( 'NONE',  ( 10.00000000000000178, 54.31368534415484106, 10.88017736071110342 ) ) ;
#23813 = CARTESIAN_POINT ( 'NONE',  ( -0.1503990784575280903, 23.10158574516642815, 6.262539305110076171 ) ) ;
#23814 = FACE_OUTER_BOUND ( 'NONE', #62761, .T. ) ;
#23815 = CARTESIAN_POINT ( 'NONE',  ( 17.96484262340118221, 64.93868534415483396, 7.964842623401181321 ) ) ;
#23816 = CARTESIAN_POINT ( 'NONE',  ( 21.09922568453595559, 2.040301336597086568, -6.408140936763230044 ) ) ;
#23817 = CARTESIAN_POINT ( 'NONE',  ( 5.625000000000006217, 11.78470029564932098, 9.742785792574933268 ) ) ;
#23818 = ADVANCED_FACE ( 'NONE', ( #75810 ), #59321, .F. ) ;
#23819 = CARTESIAN_POINT ( 'NONE',  ( 10.00000000000000178, 27.25893115100078390, 9.846743663894594434 ) ) ;
#23820 = CARTESIAN_POINT ( 'NONE',  ( 19.38216949554541557, 52.24863466993041072, -9.382169495545420901 ) ) ;
#23821 = CARTESIAN_POINT ( 'NONE',  ( -0.000000000000000000, 78.19920772666813491, 8.807240371166628279 ) ) ;
#23822 = CARTESIAN_POINT ( 'NONE',  ( 0.1532563361054100626, 25.80059781766744820, -2.638427012816831230 ) ) ;
#23823 = CARTESIAN_POINT ( 'NONE',  ( 22.81628187352647785, 21.62363466993041783, 6.195893100308588602E-16 ) ) ;
#23825 = DIRECTION ( 'NONE',  ( 0.000000000000000000, 1.000000000000000000, -0.000000000000000000 ) ) ;
#23824 = DIRECTION ( 'NONE',  ( -0.000000000000000000, -1.000000000000000000, -0.000000000000000000 ) ) ;
#23826 = CARTESIAN_POINT ( 'NONE',  ( 20.88017736071110164, 50.35535201082151247, 2.915334737309930979 ) ) ;
#23828 = CARTESIAN_POINT ( 'NONE',  ( 17.20831665107776587, 57.88393115100078745, 7.208316651077764980 ) ) ;
#23827 = B_SPLINE_CURVE_WITH_KNOTS ( 'NONE', 3,
 ( #95226, #35209, #72716, #3262, #10764, #79746 ),
 .UNSPECIFIED., .F., .F.,
 ( 4, 2, 4 ),
 ( 0.0002800001171688649721, 0.0006862053477355121046, 0.001092410578302159237 ),
 .UNSPECIFIED. ) ;
#23829 = FILL_AREA_STYLE ('',( #54292 ) ) ;
#23830 = ADVANCED_FACE ( 'NONE', ( #91804 ), #98349, .T. ) ;
#23831 = CIRCLE ( 'NONE', #36596, 14.49999999999999822 ) ;
#23832 = CARTESIAN_POINT ( 'NONE',  ( 19.84674366389459621, 23.50893115100078390, 7.409399052514197653E-17 ) ) ;
#23833 = CARTESIAN_POINT ( 'NONE',  ( -0.8801773607110991993, 12.85535201082150358, -2.915334737309923874 ) ) ;
#23834 = CARTESIAN_POINT ( 'NONE',  ( -2.816281873526473856, 19.33196800326375708, 3.434112377981055619 ) ) ;
#23835 =( NAMED_UNIT ( * ) SI_UNIT ( $, .STERADIAN. ) SOLID_ANGLE_UNIT ( ) );
#23836 = DIRECTION ( 'NONE',  ( 0.000000000000000000, -1.000000000000000000, 0.000000000000000000 ) ) ;
#23837 = CARTESIAN_POINT ( 'NONE',  ( 20.88017736071110519, 25.56368534415483751, 2.639326808657452039E-16 ) ) ;
#23838 = FILL_AREA_STYLE ('',( #92801 ) ) ;
#23839 = CARTESIAN_POINT ( 'NONE',  ( 2.035157376598822676, 22.43868534415483396, -7.964842623401177768 ) ) ;
#23840 = DIRECTION ( 'NONE',  ( 1.000000000000000000, 0.000000000000000000, 0.000000000000000000 ) ) ;
#23841 = CARTESIAN_POINT ( 'NONE',  ( 20.88017736071110875, 35.77201867748816966, -2.915334737309920765 ) ) ;
#23843 = CARTESIAN_POINT ( 'NONE',  ( 9.820682251645100891, 14.76930270348881002, 11.26020669458365653 ) ) ;
#23842 = CARTESIAN_POINT ( 'NONE',  ( 20.88017736071110875, 5.772018677488170546, -2.915334737309920765 ) ) ;
#23844 = PRESENTATION_STYLE_ASSIGNMENT (( #91834 ) ) ;
#23845 = CARTESIAN_POINT ( 'NONE',  ( 10.00000000000000000, 29.75893115100078745, -9.846743663894594434 ) ) ;
#23846 = CARTESIAN_POINT ( 'NONE',  ( -2.816281873526471635, 8.915301336597083903, -3.434112377981056508 ) ) ;
#23847 = CARTESIAN_POINT ( 'NONE',  ( 17.99999999999999645, 78.06028276952159217, -3.869891141068608320 ) ) ;
#23848 = CARTESIAN_POINT ( 'NONE',  ( 19.84674366389459266, 63.71726448433412315, -2.638427012816827677 ) ) ;
#23849 = PRESENTATION_LAYER_ASSIGNMENT (  '', '', ( #38198 ) ) ;
#23850 = DIRECTION ( 'NONE',  ( -1.000000000000000000, 0.000000000000000000, -0.000000000000000000 ) ) ;
#23851 = CARTESIAN_POINT ( 'NONE',  ( -2.266590686148945544, 27.22041550158063572, 7.082119434687048631 ) ) ;
#23852 = CARTESIAN_POINT ( 'NONE',  ( 7.361572987183169658, 34.96726448433411605, -9.846743663894592657 ) ) ;
#23853 = EDGE_CURVE ( 'NONE', #97012, #48470, #97784, .T. ) ;
#23854 = PLANE ( 'NONE',  #72015 ) ;
#23855 = ORIENTED_EDGE ( 'NONE', *, *, #49225, .T. ) ;
#23856 = CARTESIAN_POINT ( 'NONE',  ( -4.164238869374098151, 56.59541550158063927, -3.795296366450310543 ) ) ;
#23857 = CARTESIAN_POINT ( 'NONE',  ( 19.84674366389459266, 28.71726448433411960, -2.638427012816827677 ) ) ;
#23859 = CARTESIAN_POINT ( 'NONE',  ( 4.096035146093422341, 15.00000000000000000, 13.90943910019259810 ) ) ;
#23858 = LINE ( 'NONE', #69344, #3572 ) ;
#23860 = CARTESIAN_POINT ( 'NONE',  ( 2.035157376598822676, 47.43868534415484817, -7.964842623401177768 ) ) ;
#23861 = CARTESIAN_POINT ( 'NONE',  ( 22.81628187352647785, 46.62363466993041783, 6.195893100308588602E-16 ) ) ;
#23862 = ADVANCED_FACE ( 'NONE', ( #29807 ), #23326, .F. ) ;
#23863 = CARTESIAN_POINT ( 'NONE',  ( -0.8801773607111008646, 18.27201867748817321, 2.915334737309923430 ) ) ;
#23865 = ORIENTED_EDGE ( 'NONE', *, *, #16980, .T. ) ;
#23864 = CARTESIAN_POINT ( 'NONE',  ( -2.816281873526471635, 48.91530133659708213, -3.434112377981056508 ) ) ;
#23866 = CARTESIAN_POINT ( 'NONE',  ( 7.361572987183170547, 67.05059781766746596, 9.846743663894590881 ) ) ;
#23867 = CARTESIAN_POINT ( 'NONE',  ( 17.20831665107776587, 2.883931151000785231, 7.208316651077764980 ) ) ;
#23868 = EDGE_LOOP ( 'NONE', ( #28339, #36665, #25052, #71727 ) ) ;
#23869 = LINE ( 'NONE', #1373, #11734 ) ;
#23870 = CARTESIAN_POINT ( 'NONE',  ( -7.750000000000000000, 1.019547802438458550, -4.000000000000000000 ) ) ;
#23871 = CARTESIAN_POINT ( 'NONE',  ( 10.00000000000000000, 55.55374883491396787, -14.16423886937410082 ) ) ;
#23872 = CARTESIAN_POINT ( 'NONE',  ( 20.36894250292379382, 18.67874883491397142, 10.36894250292379205 ) ) ;
#23873 = CARTESIAN_POINT ( 'NONE',  ( 15.44008868035555260, 19.73035201082150536, 9.422509992056143702 ) ) ;
#23874 = CARTESIAN_POINT ( 'NONE',  ( 12.91533473730993009, 41.60535201082149825, -10.88017736071109987 ) ) ;
#23875 = DIRECTION ( 'NONE',  ( 0.000000000000000000, 0.000000000000000000, -1.000000000000000000 ) ) ;
#23876 = VECTOR ( 'NONE', #26559, 1000.000000000000000 ) ;
#23877 = CARTESIAN_POINT ( 'NONE',  ( -18.00000000000000355, 75.73428692542562146, -3.000000000000000000 ) ) ;
#23878 = CARTESIAN_POINT ( 'NONE',  ( -0.8801773607111009756, 63.06368534415484106, 1.068504757029289695E-15 ) ) ;
#23879 = CARTESIAN_POINT ( 'NONE',  ( 15.44008868035555793, 66.39701867748817676, -9.422509992056140149 ) ) ;
#23880 = CARTESIAN_POINT ( 'NONE',  ( 19.84674366389459266, 23.71726448433412315, -2.638427012816827677 ) ) ;
#23881 = CARTESIAN_POINT ( 'NONE',  ( 5.240693273018990794, 0.04962883216462460334, 13.79102773477917232 ) ) ;
#23882 = DIRECTION ( 'NONE',  ( 0.000000000000000000, 0.000000000000000000, 1.000000000000000000 ) ) ;
#23883 = CARTESIAN_POINT ( 'NONE',  ( 5.076628168052703671, 11.84226448433411960, 8.527530157486179263 ) ) ;
#23884 = CARTESIAN_POINT ( 'NONE',  ( 14.92337183194729988, 34.34226448433411605, -8.527530157486177487 ) ) ;
#23885 = CARTESIAN_POINT ( 'NONE',  ( 17.96484262340118221, 19.93868534415484106, 7.964842623401181321 ) ) ;
#23886 = CARTESIAN_POINT ( 'NONE',  ( 0.6178305044545838731, 34.74863466993042493, 9.382169495545420901 ) ) ;
#23888 = EDGE_CURVE ( 'NONE', #13765, #53769, #68815, .T. ) ;
#23887 = CARTESIAN_POINT ( 'NONE',  ( 19.84674366389459621, 3.508931151000785231, 7.409399052514197653E-17 ) ) ;
#23889 = LINE ( 'NONE', #69871, #44036 ) ;
#23890 = CARTESIAN_POINT ( 'NONE',  ( 2.791683348922237240, 45.38393115100079456, -7.208316651077763204 ) ) ;
#23891 = CARTESIAN_POINT ( 'NONE',  ( 10.00000000000000178, 32.25893115100078745, 9.846743663894594434 ) ) ;
#23892 = CARTESIAN_POINT ( 'NONE',  ( -4.164238869374099927, 17.01208216824730357, 3.795296366450308767 ) ) ;
#23893 = CARTESIAN_POINT ( 'NONE',  ( -0.8801773607111009756, 38.06368534415484106, 1.068504757029289695E-15 ) ) ;
#23894 = CARTESIAN_POINT ( 'NONE',  ( 17.96484262340118221, 6.188685344154836621, -7.964842623401177768 ) ) ;
#23895 = CARTESIAN_POINT ( 'NONE',  ( 20.88017736071110875, 50.77201867748817676, -2.915334737309920765 ) ) ;
#23896 = CARTESIAN_POINT ( 'NONE',  ( 17.96484262340118221, 34.93868534415482685, 7.964842623401181321 ) ) ;
#23897 = VERTEX_POINT ( 'NONE', #37833 ) ;
#23898 = CARTESIAN_POINT ( 'NONE',  ( 16.40814093676324603, 32.45696800326375353, -11.09922568453594671 ) ) ;
#23899 = CARTESIAN_POINT ( 'NONE',  ( 20.88017736071110164, 40.35535201082150536, 2.915334737309930979 ) ) ;
#23900 = ORIENTED_EDGE ( 'NONE', *, *, #30772, .T. ) ;
#23901 = CARTESIAN_POINT ( 'NONE',  ( -2.816281873526473856, 54.12363466993041783, 9.499525473075851096E-16 ) ) ;
#23902 = CARTESIAN_POINT ( 'NONE',  ( 15.44008868035555793, 51.39701867748816966, -9.422509992056140149 ) ) ;
#23903 = ORIENTED_EDGE ( 'NONE', *, *, #49841, .T. ) ;
#23904 = CARTESIAN_POINT ( 'NONE',  ( 20.88017736071110875, 50.77201867748817676, -2.915334737309920765 ) ) ;
#23905 = CARTESIAN_POINT ( 'NONE',  ( 6.905642986259637794, -69.45547628558860254, 3.750000000000000000 ) ) ;
#23906 = CARTESIAN_POINT ( 'NONE',  ( 4.431036607602490740, 0.3639312379444061274, 14.33059365769916838 ) ) ;
#23907 = CARTESIAN_POINT ( 'NONE',  ( -4.164238869374099927, 57.01208216824731068, 3.795296366450308767 ) ) ;
#23908 = CARTESIAN_POINT ( 'NONE',  ( 19.42250999205614548, 65.98035201082151957, -5.440088680355545492 ) ) ;
#23909 = CARTESIAN_POINT ( 'NONE',  ( 19.42250999205614548, 55.98035201082150536, -5.440088680355545492 ) ) ;
#23910 = CARTESIAN_POINT ( 'NONE',  ( -14.36383853300411140, 14.95037103067321560, 3.367113227848840040 ) ) ;
#23911 = CARTESIAN_POINT ( 'NONE',  ( -14.62129639376012058, 15.00000000000000711, 0.3552502084984235919 ) ) ;
#23912 = CARTESIAN_POINT ( 'NONE',  ( 19.84674366389459266, 28.71726448433411960, -2.638427012816827677 ) ) ;
#23913 = VERTEX_POINT ( 'NONE', #90306 ) ;
#23914 = CARTESIAN_POINT ( 'NONE',  ( 12.63842701281683922, 29.55059781766745175, -9.846743663894590881 ) ) ;
#23915 = CARTESIAN_POINT ( 'NONE',  ( 2.035157376598824452, 33.68868534415484106, 7.964842623401179544 ) ) ;
#23916 = CARTESIAN_POINT ( 'NONE',  ( 5.076628168052703671, 41.84226448433411605, 8.527530157486179263 ) ) ;
#23917 = CARTESIAN_POINT ( 'NONE',  ( 13.43411237798105340, 20.58196800326374643, 12.81628187352647963 ) ) ;
#23919 = CARTESIAN_POINT ( 'NONE',  ( 19.80448550324508616, 1.827036817733421081, 6.500000000002772893 ) ) ;
#23918 = DIRECTION ( 'NONE',  ( -1.000000000000000000, 0.000000000000000000, 0.000000000000000000 ) ) ;
#23920 = CARTESIAN_POINT ( 'NONE',  ( 19.42250999205614193, 45.14701867748817676, 5.440088680355555262 ) ) ;
#23921 = CARTESIAN_POINT ( 'NONE',  ( 22.26659068614895176, 54.72041550158063217, -7.082119434687042414 ) ) ;
#23922 = VECTOR ( 'NONE', #69499, 1000.000000000000000 ) ;
#23923 = CARTESIAN_POINT ( 'NONE',  ( 10.00000000000000178, 25.37363466993041783, 12.81628187352647608 ) ) ;
#23924 = FACE_OUTER_BOUND ( 'NONE', #30389, .T. ) ;
#23925 = ORIENTED_EDGE ( 'NONE', *, *, #88430, .F. ) ;
#23926 = CARTESIAN_POINT ( 'NONE',  ( 19.38216949554541202, 30.99863466993042138, 9.382169495545424454 ) ) ;
#23927 = CARTESIAN_POINT ( 'NONE',  ( 12.91533473730993009, 21.60535201082150536, -10.88017736071109987 ) ) ;
#23928 = CARTESIAN_POINT ( 'NONE',  ( 17.96484262340118221, 56.18868534415484817, -7.964842623401177768 ) ) ;
#23929 = VERTEX_POINT ( 'NONE', #98843 ) ;
#23930 = ORIENTED_EDGE ( 'NONE', *, *, #74909, .T. ) ;
#23931 = EDGE_CURVE ( 'NONE', #40303, #5283, #30297, .T. ) ;
#23932 = CARTESIAN_POINT ( 'NONE',  ( 3.270351084886697457, 0.04962888917231522701, 14.38617789677964609 ) ) ;
#23933 = CARTESIAN_POINT ( 'NONE',  ( 19.42250999205614548, 65.98035201082151957, -5.440088680355545492 ) ) ;
#23934 = CARTESIAN_POINT ( 'NONE',  ( 19.84674366389459266, 53.30059781766744464, 2.638427012816836559 ) ) ;
#23935 = CARTESIAN_POINT ( 'NONE',  ( 0.1532563361054100626, 40.80059781766745886, -2.638427012816831230 ) ) ;
#23936 = CARTESIAN_POINT ( 'NONE',  ( 18.72515096720568906, 15.05509018479935612, 6.500000000000002665 ) ) ;
#23937 = CARTESIAN_POINT ( 'NONE',  ( 18.52753015748617571, 28.09226448433411960, 4.923371831947298993 ) ) ;
#23938 = CARTESIAN_POINT ( 'NONE',  ( 20.15039907845753220, 54.72266099184918886, 6.262539305110078836 ) ) ;
#23939 = LINE ( 'NONE', #69924, #557 ) ;
#23940 = ADVANCED_FACE ( 'NONE', ( #60800 ), #14336, .F. ) ;
#23942 = FACE_OUTER_BOUND ( 'NONE', #58255, .T. ) ;
#23941 = CARTESIAN_POINT ( 'NONE',  ( 12.63842701281683034, 17.46726448433411250, 9.846743663894596210 ) ) ;
#23943 = CARTESIAN_POINT ( 'NONE',  ( -8.000000000000000000, 80.32179676972448590, -4.250000000000000000 ) ) ;
#23945 = EDGE_LOOP ( 'NONE', ( #3041, #27074, #55701, #82438, #59144, #38686 ) ) ;
#23944 = CARTESIAN_POINT ( 'NONE',  ( 0.1532563361054100626, 50.80059781766745175, -2.638427012816831230 ) ) ;
#23946 = CARTESIAN_POINT ( 'NONE',  ( 11.36220558718861717, 15.00000000000000000, -9.008345252845218809 ) ) ;
#23947 = CARTESIAN_POINT ( 'NONE',  ( -1.099225684535947600, 18.70696800326375353, -6.408140936763238038 ) ) ;
#23948 = CARTESIAN_POINT ( 'NONE',  ( 0.5774900079438607392, 48.48035201082150536, 5.440088680355550821 ) ) ;
#23949 = CARTESIAN_POINT ( 'NONE',  ( -0.3689425029237898834, 51.17874883491397497, -10.36894250292378850 ) ) ;
#23950 = CARTESIAN_POINT ( 'NONE',  ( 9.879999999999991900, 20.99999999999999645, -1.249999999999987121 ) ) ;
#23951 = CARTESIAN_POINT ( 'NONE',  ( 13.79529636645031943, 40.34541550158063217, -14.16423886937409904 ) ) ;
#23952 = CARTESIAN_POINT ( 'NONE',  ( 20.36894250292379382, 58.67874883491396076, 10.36894250292379205 ) ) ;
#23953 = CARTESIAN_POINT ( 'NONE',  ( -4.164238869374098151, 21.59541550158063217, -3.795296366450310543 ) ) ;
#23954 = CARTESIAN_POINT ( 'NONE',  ( -4.164238869374099927, 27.01208216824730357, 3.795296366450308767 ) ) ;
#23955 = CARTESIAN_POINT ( 'NONE',  ( 20.15039907845753220, 24.72266099184919241, 6.262539305110077947 ) ) ;
#23957 = CARTESIAN_POINT ( 'NONE',  ( 14.92337183194729633, 37.67559781766745175, 8.527530157486181039 ) ) ;
#23956 = CARTESIAN_POINT ( 'NONE',  ( 4.441081520791478887, -2.684960557648791823, 2.750000000000000000 ) ) ;
#23958 = CARTESIAN_POINT ( 'NONE',  ( -0.8801773607111009756, 23.06368534415484106, 1.068504757029289695E-15 ) ) ;
#23959 = LINE ( 'NONE', #79286, #27527 ) ;
#23960 = DIRECTION ( 'NONE',  ( -2.569960705150826877E-16, 1.000000000000000000, 0.000000000000000000 ) ) ;
#23961 = CARTESIAN_POINT ( 'NONE',  ( 20.00000000000000711, 90.60731807131610083, -5.318367326097200198 ) ) ;
#23962 = CARTESIAN_POINT ( 'NONE',  ( 0.1532563361054082862, 41.21726448433411605, 2.638427012816831674 ) ) ;
#23963 = CARTESIAN_POINT ( 'NONE',  ( 21.09922568453594849, 61.20696800326376064, 6.408140936763242479 ) ) ;
#23964 = CARTESIAN_POINT ( 'NONE',  ( 3.795296366450314540, -11.73791783175269821, 14.16423886937410082 ) ) ;
#23965 = CARTESIAN_POINT ( 'NONE',  ( 10.00000000000000000, 39.75893115100078745, -9.846743663894594434 ) ) ;
#23966 = CARTESIAN_POINT ( 'NONE',  ( 18.52753015748618282, 58.92559781766745886, -4.923371831947291888 ) ) ;
#23967 = CARTESIAN_POINT ( 'NONE',  ( 6.204703633549690345, 35.76208216824729647, -14.16423886937410259 ) ) ;
#23968 = EDGE_CURVE ( 'NONE', #75199, #42131, #52323, .T. ) ;
#23969 = ORIENTED_EDGE ( 'NONE', *, *, #32257, .T. ) ;
#23970 = CARTESIAN_POINT ( 'NONE',  ( 24.16423886937410614, 14.51208216824730179, -3.795296366450302550 ) ) ;
#23971 = CARTESIAN_POINT ( 'NONE',  ( 0.2751277870542967463, 70.00000000000000000, -6.500000000000000888 ) ) ;
#23973 = CARTESIAN_POINT ( 'NONE',  ( 1.274849032794324932, 22.55509018479936145, -6.500000000000021316 ) ) ;
#23972 = DIRECTION ( 'NONE',  ( 0.000000000000000000, 0.000000000000000000, -1.000000000000000000 ) ) ;
#23974 = CARTESIAN_POINT ( 'NONE',  ( -2.266590686148945544, 66.38708216824730357, -7.082119434687050408 ) ) ;
#23975 = CARTESIAN_POINT ( 'NONE',  ( 10.00000000000000178, 5.373634669930420493, 12.81628187352647608 ) ) ;
#23976 = ADVANCED_FACE ( 'NONE', ( #61295 ), #51832, .F. ) ;
#23977 = CARTESIAN_POINT ( 'NONE',  ( 8.979999999999991545, 27.03929484861773958, 3.000000000000000000 ) ) ;
#23978 = CARTESIAN_POINT ( 'NONE',  ( 2.035157376598822676, 67.43868534415484817, -7.964842623401177768 ) ) ;
#23979 = CARTESIAN_POINT ( 'NONE',  ( -6.000000000000009770, 40.99999999999999289, -6.500000000000000888 ) ) ;
#23980 = VECTOR ( 'NONE', #31833, 1000.000000000000000 ) ;
#23981 = CARTESIAN_POINT ( 'NONE',  ( 1.472469842513823179, 30.59226448433411960, -4.923371831947296329 ) ) ;
#23982 = CARTESIAN_POINT ( 'NONE',  ( 0.000000000000000000, 15.00000000000000000, 0.000000000000000000 ) ) ;
#23983 = CARTESIAN_POINT ( 'NONE',  ( -4.164238869374099039, 66.80374883491396076, 8.674139862899312516E-16 ) ) ;
#23984 = CARTESIAN_POINT ( 'NONE',  ( 1.274849032794102888, 3.572280503510291361, 6.499999999999721112 ) ) ;
#23985 = CARTESIAN_POINT ( 'NONE',  ( 15.44008868035555260, 29.73035201082150891, 9.422509992056143702 ) ) ;
#23986 = CARTESIAN_POINT ( 'NONE',  ( -0.8801773607110991993, 22.85535201082150181, -2.915334737309923874 ) ) ;
#23987 = CARTESIAN_POINT ( 'NONE',  ( 5.076628168052704559, 60.17559781766745175, -8.527530157486179263 ) ) ;
#23988 = CARTESIAN_POINT ( 'NONE',  ( 18.52753015748617571, 53.09226448433412315, 4.923371831947298993 ) ) ;
#23989 = CARTESIAN_POINT ( 'NONE',  ( -43.84582565093677431, 106.6410155927914332, -4.576759396000646518 ) ) ;
#23990 = SURFACE_STYLE_FILL_AREA ( #77957 ) ;
#23991 = ORIENTED_EDGE ( 'NONE', *, *, #52463, .T. ) ;
#23992 = AXIS2_PLACEMENT_3D ( 'NONE', #48973, #94473, #86974 ) ;
#23993 = CARTESIAN_POINT ( 'NONE',  ( 10.00000000000000000, 26.81368534415484106, -10.88017736071110342 ) ) ;
#23994 = CARTESIAN_POINT ( 'NONE',  ( -2.816281873526473856, 24.12363466993042138, 9.499525473075851096E-16 ) ) ;
#23995 = CARTESIAN_POINT ( 'NONE',  ( -0.3289641300568005855, 55.10497603579417358, 5.963430220938281678 ) ) ;
#23996 = CARTESIAN_POINT ( 'NONE',  ( 10.00000000000000178, 62.25893115100078745, 9.846743663894594434 ) ) ;
#23997 = CARTESIAN_POINT ( 'NONE',  ( 19.42250999205614548, 50.98035201082151247, -5.440088680355545492 ) ) ;
#23998 = CARTESIAN_POINT ( 'NONE',  ( 6.565887622018943937, 20.16530133659708213, 12.81628187352647430 ) ) ;
#24000 = CARTESIAN_POINT ( 'NONE',  ( 19.42250999205614193, 15.14701867748817143, 5.440088680355555262 ) ) ;
#23999 = CARTESIAN_POINT ( 'NONE',  ( 20.88017736071110875, 60.77201867748817676, -2.915334737309920765 ) ) ;
#24001 = CARTESIAN_POINT ( 'NONE',  ( -0.1503990784575328643, 50.12777174578613426, 6.262539305110068177 ) ) ;
#24002 = ORIENTED_EDGE ( 'NONE', *, *, #35382, .T. ) ;
#24003 = DIRECTION ( 'NONE',  ( 1.000000000000000000, -0.000000000000000000, 0.000000000000000000 ) ) ;
#24004 = CARTESIAN_POINT ( 'NONE',  ( 2.035157376598822676, 52.43868534415483396, -7.964842623401177768 ) ) ;
#24006 = CARTESIAN_POINT ( 'NONE',  ( 22.26659068614895176, 9.720415501580633943, -7.082119434687042414 ) ) ;
#24005 = CARTESIAN_POINT ( 'NONE',  ( 0.6178305044545838731, 44.74863466993042493, 9.382169495545420901 ) ) ;
#24007 = CARTESIAN_POINT ( 'NONE',  ( 1.472469842513823179, 21.42559781766745175, 4.923371831947296329 ) ) ;
#24008 = CARTESIAN_POINT ( 'NONE',  ( 18.52753015748617571, 63.09226448433412315, 4.923371831947298993 ) ) ;
#24009 = TOROIDAL_SURFACE ( 'NONE', #31967, 14.49999999999999822, 0.5000000000000000000 ) ;
#24010 = EDGE_CURVE ( 'NONE', #12669, #71776, #44809, .T. ) ;
#24011 = CARTESIAN_POINT ( 'NONE',  ( 12.63842701281683034, 22.46726448433411605, 9.846743663894596210 ) ) ;
#24012 = CARTESIAN_POINT ( 'NONE',  ( 0.000000000000000000, 0.5000000000000004441, 0.000000000000000000 ) ) ;
#24013 = CARTESIAN_POINT ( 'NONE',  ( 13.79529636645030344, 63.26208216824730357, 14.16423886937410614 ) ) ;
#24014 = ORIENTED_EDGE ( 'NONE', *, *, #22024, .F. ) ;
#24015 = CARTESIAN_POINT ( 'NONE',  ( 10.00000000000000178, 4.313685344154837509, 10.88017736071110342 ) ) ;
#24016 = EDGE_CURVE ( 'NONE', #71199, #67764, #93273, .T. ) ;
#24017 = CARTESIAN_POINT ( 'NONE',  ( 19.42250999205614548, 5.980352010821504471, -5.440088680355545492 ) ) ;
#24018 = CARTESIAN_POINT ( 'NONE',  ( 1.959929470562273179, 15.51528370094808018, -5.767676674365838529 ) ) ;
#24019 = B_SPLINE_CURVE_WITH_KNOTS ( 'NONE', 3,
 ( #27839, #88844, #4866, #5844, #96864, #26366 ),
 .UNSPECIFIED., .F., .F.,
 ( 4, 2, 4 ),
 ( 7.840110604351616646E-18, 0.0002626113303185972870, 0.0005252226606371866594 ),
 .UNSPECIFIED. ) ;
#24020 = ORIENTED_EDGE ( 'NONE', *, *, #75995, .F. ) ;
#24021 = ORIENTED_EDGE ( 'NONE', *, *, #42833, .T. ) ;
#24022 = CARTESIAN_POINT ( 'NONE',  ( 10.00000000000000178, 4.313685344154837509, 10.88017736071110342 ) ) ;
#24023 = CARTESIAN_POINT ( 'NONE',  ( 15.44008868035555260, 9.730352010821505360, 9.422509992056143702 ) ) ;
#24024 = CARTESIAN_POINT ( 'NONE',  ( 0.1532563361054083140, 46.00893115100079456, 1.131784320476157264E-15 ) ) ;
#24025 = CARTESIAN_POINT ( 'NONE',  ( 3.591859063236763294, 43.29030133659708923, -11.09922568453595026 ) ) ;
#24026 = CARTESIAN_POINT ( 'NONE',  ( -3.014428414850141458, 11.88013551118487321, -11.24999999999999822 ) ) ;
#24028 = CARTESIAN_POINT ( 'NONE',  ( 22.26659068614894466, 23.88708216824730357, 7.082119434687054849 ) ) ;
#24027 = CARTESIAN_POINT ( 'NONE',  ( -12.80781515976318907, 15.00000000000000000, 6.246788841744232990 ) ) ;
#24029 = CARTESIAN_POINT ( 'NONE',  ( 12.91533473730992121, 24.52201867748816966, 10.88017736071110164 ) ) ;
#24030 = CARTESIAN_POINT ( 'NONE',  ( 2.035157376598824452, 3.688685344154837953, 7.964842623401179544 ) ) ;
#24031 = CARTESIAN_POINT ( 'NONE',  ( 0.1532563361054082862, 41.21726448433411605, 2.638427012816831674 ) ) ;
#24032 = CARTESIAN_POINT ( 'NONE',  ( -1.514341385896341929, 15.00000000000000000, -15.92432625271835533 ) ) ;
#24033 = CARTESIAN_POINT ( 'NONE',  ( 17.20831665107776587, 39.13393115100079456, -7.208316651077762316 ) ) ;
#24034 = CARTESIAN_POINT ( 'NONE',  ( 0.000000000000000000, 14.49999999999999822, 0.000000000000000000 ) ) ;
#24035 = CARTESIAN_POINT ( 'NONE',  ( -4.923371831947292776, 26.84226448433413381, 8.527530157486181039 ) ) ;
#24036 = ORIENTED_EDGE ( 'NONE', *, *, #54749, .T. ) ;
#24037 = CARTESIAN_POINT ( 'NONE',  ( -0.8801773607111008646, 3.272018677488171434, 2.915334737309923430 ) ) ;
#24038 = CARTESIAN_POINT ( 'NONE',  ( 20.88017736071110164, 65.35535201082150536, 2.915334737309930979 ) ) ;
#24039 = CARTESIAN_POINT ( 'NONE',  ( 19.42250999205614548, 30.98035201082150536, -5.440088680355545492 ) ) ;
#24040 = CARTESIAN_POINT ( 'NONE',  ( 10.00000000000000000, 32.87363466993042493, -12.81628187352647608 ) ) ;
#24041 = CARTESIAN_POINT ( 'NONE',  ( -4.164238869374099039, 16.80374883491396787, 8.674139862899312516E-16 ) ) ;
#24042 = AXIS2_PLACEMENT_3D ( 'NONE', #79319, #41349, #79806 ) ;
#24043 = B_SPLINE_CURVE_WITH_KNOTS ( 'NONE', 3,
 ( #7271, #61238, #38262, #8728, #22277, #83752 ),
 .UNSPECIFIED., .F., .F.,
 ( 4, 2, 4 ),
 ( 0.000000000000000000, 0.0002565770811490928911, 0.0005131541622981857821 ),
 .UNSPECIFIED. ) ;
#24044 = CARTESIAN_POINT ( 'NONE',  ( 16.40814093676324603, 47.45696800326375353, -11.09922568453594671 ) ) ;
#24045 = VERTEX_POINT ( 'NONE', #10277 ) ;
#24046 = CARTESIAN_POINT ( 'NONE',  ( 2.791683348922237240, 45.38393115100079456, -7.208316651077763204 ) ) ;
#24047 = CARTESIAN_POINT ( 'NONE',  ( 20.88017736071110519, 20.56368534415484106, 2.639326808657452039E-16 ) ) ;
#24048 = VERTEX_POINT ( 'NONE', #24796 ) ;
#24049 = AXIS2_PLACEMENT_3D ( 'NONE', #5423, #35893, #14898 ) ;
#24050 = CARTESIAN_POINT ( 'NONE',  ( 15.44008868035555260, 14.73035201082150536, 9.422509992056143702 ) ) ;
#24051 = ORIENTED_EDGE ( 'NONE', *, *, #29948, .F. ) ;
#24052 = CARTESIAN_POINT ( 'NONE',  ( 17.96484262340118221, 61.18868534415482685, -7.964842623401177768 ) ) ;
#24053 = AXIS2_PLACEMENT_3D ( 'NONE', #48563, #57049, #72534 ) ;
#24054 = CARTESIAN_POINT ( 'NONE',  ( -5.419894505350392855, 0.5000000000000004441, -13.98659156302466045 ) ) ;
#24055 = CARTESIAN_POINT ( 'NONE',  ( 19.84674366389459621, 8.508931151000785675, 7.409399052514197653E-17 ) ) ;
#24056 = CARTESIAN_POINT ( 'NONE',  ( 10.00000000000000000, 61.81368534415484106, -10.88017736071110342 ) ) ;
#24057 = TOROIDAL_SURFACE ( 'NONE', #51163, 1.499999999999996669, 0.5000000000000000000 ) ;
#24058 = CARTESIAN_POINT ( 'NONE',  ( -10.09777502097869650, 0.04922511925147179945, -10.75551206493395107 ) ) ;
#24059 = EDGE_CURVE ( 'NONE', #26051, #46052, #68102, .T. ) ;
#24060 = CARTESIAN_POINT ( 'NONE',  ( -46.94000000000000483, 102.2681967859571870, 7.165875991462780092 ) ) ;
#24062 = ORIENTED_EDGE ( 'NONE', *, *, #85350, .F. ) ;
#24061 = CARTESIAN_POINT ( 'NONE',  ( 7.361572987183170547, 12.05059781766744997, 9.846743663894590881 ) ) ;
#24063 = CARTESIAN_POINT ( 'NONE',  ( 5.076628168052703671, 36.84226448433412315, 8.527530157486179263 ) ) ;
#24064 = VERTEX_POINT ( 'NONE', #17783 ) ;
#24065 = ORIENTED_EDGE ( 'NONE', *, *, #63005, .F. ) ;
#24066 = DIRECTION ( 'NONE',  ( -0.000000000000000000, -1.000000000000000000, -0.000000000000000000 ) ) ;
#24067 =( LENGTH_UNIT ( ) NAMED_UNIT ( * ) SI_UNIT ( .MILLI., .METRE. ) );
#24068 = CARTESIAN_POINT ( 'NONE',  ( 10.00000000000000000, 57.87363466993042493, -12.81628187352647608 ) ) ;
#24069 = CARTESIAN_POINT ( 'NONE',  ( 20.36894250292379382, 8.678748834913967869, 10.36894250292379205 ) ) ;
#24070 = CARTESIAN_POINT ( 'NONE',  ( 13.79529636645031943, 25.34541550158063572, -14.16423886937409904 ) ) ;
#24071 = CARTESIAN_POINT ( 'NONE',  ( 0.000000000000000000, 14.49999999999999822, 0.000000000000000000 ) ) ;
#24073 = CARTESIAN_POINT ( 'NONE',  ( -0.8801773607110991993, 57.85535201082149825, -2.915334737309923874 ) ) ;
#24072 = DIRECTION ( 'NONE',  ( 0.000000000000000000, 0.000000000000000000, 1.000000000000000000 ) ) ;
#24074 = CARTESIAN_POINT ( 'NONE',  ( 10.00000000000000178, 19.31368534415484106, 10.88017736071110342 ) ) ;
#24075 = SURFACE_STYLE_FILL_AREA ( #30561 ) ;
#24076 = ORIENTED_EDGE ( 'NONE', *, *, #16094, .F. ) ;
#24077 = CARTESIAN_POINT ( 'NONE',  ( 19.84674366389459266, 8.300597817667451750, 2.638427012816836559 ) ) ;
#24078 = CARTESIAN_POINT ( 'NONE',  ( 5.076628168052704559, 5.175597817667451750, -8.527530157486179263 ) ) ;
#24079 = CARTESIAN_POINT ( 'NONE',  ( 0.6178305044545818747, 38.49863466993042493, -9.382169495545419124 ) ) ;
#24080 = CARTESIAN_POINT ( 'NONE',  ( 14.92337183194729988, 29.34226448433411960, -8.527530157486177487 ) ) ;
#24081 = CARTESIAN_POINT ( 'NONE',  ( -16.60833333333333073, 99.74999999999998579, 8.000000000000000000 ) ) ;
#24082 = CARTESIAN_POINT ( 'NONE',  ( -1.099225684535947600, 19.54030133659708568, 6.408140936763237150 ) ) ;
#24083 = DIRECTION ( 'NONE',  ( 0.000000000000000000, 0.000000000000000000, 1.000000000000000000 ) ) ;
#24084 = VECTOR ( 'NONE', #6716, 1000.000000000000000 ) ;
#24085 = CARTESIAN_POINT ( 'NONE',  ( 10.00000000000000000, 9.758931151000785675, -9.846743663894594434 ) ) ;
#24086 = EDGE_CURVE ( 'NONE', #89063, #30064, #39308, .T. ) ;
#24087 = VERTEX_POINT ( 'NONE', #16796 ) ;
#24088 = CARTESIAN_POINT ( 'NONE',  ( 7.084665262690076126, 19.10535201082150181, 10.88017736071109987 ) ) ;
#24089 = CARTESIAN_POINT ( 'NONE',  ( 24.16423886937410614, 34.30374883491396787, 8.672049930838204340E-16 ) ) ;
#24090 = CARTESIAN_POINT ( 'NONE',  ( 0.1532563361054100626, 40.80059781766745886, -2.638427012816831230 ) ) ;
#24091 = CARTESIAN_POINT ( 'NONE',  ( 19.42250999205614193, 65.14701867748817676, 5.440088680355555262 ) ) ;
#24093 = LINE ( 'NONE', #54076, #16075 ) ;
#24092 = CARTESIAN_POINT ( 'NONE',  ( 16.40814093676323893, 55.79030133659708923, 11.09922568453595026 ) ) ;
#24094 = CARTESIAN_POINT ( 'NONE',  ( 15.44008868035555793, 26.39701867748817321, -9.422509992056140149 ) ) ;
#24095 = EDGE_CURVE ( 'NONE', #91469, #29043, #92777, .T. ) ;
#24096 = LINE ( 'NONE', #25089, #67792 ) ;
#24097 = CARTESIAN_POINT ( 'NONE',  ( 16.40814093676323893, 5.790301336597087456, 11.09922568453595026 ) ) ;
#24098 = CARTESIAN_POINT ( 'NONE',  ( 12.63842701281683034, 37.46726448433411605, 9.846743663894596210 ) ) ;
#24099 = CARTESIAN_POINT ( 'NONE',  ( 7.964842623401177768, -3.811314655845160271, -7.964842623401181321 ) ) ;
#24100 = CARTESIAN_POINT ( 'NONE',  ( 16.40814093676323893, 50.79030133659708923, 11.09922568453595026 ) ) ;
#24101 = DIRECTION ( 'NONE',  ( 0.5547001962252290364, 0.8320502943378437211, 0.000000000000000000 ) ) ;
#24103 = DIRECTION ( 'NONE',  ( 0.000000000000000000, 0.000000000000000000, 1.000000000000000000 ) ) ;
#24102 = CARTESIAN_POINT ( 'NONE',  ( 15.44008868035555260, 49.73035201082150536, 9.422509992056143702 ) ) ;
#24104 = CARTESIAN_POINT ( 'NONE',  ( -7.750000000000000000, 0.000000000000000000, -3.750000000000000000 ) ) ;
#24105 = CARTESIAN_POINT ( 'NONE',  ( -0.2849401152840977391, 14.76984969742594345, 14.93790629078302423 ) ) ;
#24106 = CARTESIAN_POINT ( 'NONE',  ( 4.559911319644449179, 57.23035201082150536, -9.422509992056141925 ) ) ;
#24107 = CIRCLE ( 'NONE', #84773, 0.7500000000000006661 ) ;
#24108 = CARTESIAN_POINT ( 'NONE',  ( 7.084665262690076126, 54.10535201082151247, 10.88017736071109987 ) ) ;
#24109 = CARTESIAN_POINT ( 'NONE',  ( 20.15039907845753930, 70.00000000000000000, -6.262539305110068177 ) ) ;
#24110 = CARTESIAN_POINT ( 'NONE',  ( 2.035157376598822676, 62.43868534415483396, -7.964842623401177768 ) ) ;
#24111 = CARTESIAN_POINT ( 'NONE',  ( 10.00000000000000178, 14.31368534415483929, 10.88017736071110342 ) ) ;
#24112 = CARTESIAN_POINT ( 'NONE',  ( 1.472469842513823179, 45.59226448433412315, -4.923371831947296329 ) ) ;
#24114 = DIRECTION ( 'NONE',  ( 0.000000000000000000, 0.000000000000000000, -1.000000000000000000 ) ) ;
#24113 = CARTESIAN_POINT ( 'NONE',  ( 7.084665262690076126, 22.02201867748817321, -10.88017736071110164 ) ) ;
#24115 = COLOUR_RGB ( '', 0.31764706, 0.68627451, 0.89019608) ;
#24116 = CARTESIAN_POINT ( 'NONE',  ( 3.591859063236761518, 19.95696800326375353, 11.09922568453594849 ) ) ;
#24117 = ORIENTED_EDGE ( 'NONE', *, *, #36990, .F. ) ;
#24118 = CARTESIAN_POINT ( 'NONE',  ( 0.5774900079438607392, 38.48035201082150536, 5.440088680355550821 ) ) ;
#24120 = DIRECTION ( 'NONE',  ( 0.000000000000000000, 0.000000000000000000, -1.000000000000000000 ) ) ;
#24119 = CARTESIAN_POINT ( 'NONE',  ( 19.38216949554541202, 10.99863466993042138, 9.382169495545424454 ) ) ;
#24121 = CARTESIAN_POINT ( 'NONE',  ( 2.035157376598822676, 17.43868534415483751, -7.964842623401177768 ) ) ;
#24122 = CIRCLE ( 'NONE', #75198, 2.999999999999997335 ) ;
#24123 = CARTESIAN_POINT ( 'NONE',  ( 0.5774900079438590739, 37.64701867748817676, -5.440088680355550821 ) ) ;
#24124 = CARTESIAN_POINT ( 'NONE',  ( 22.26659068614894466, 48.88708216824730357, 7.082119434687054849 ) ) ;
#24125 = CARTESIAN_POINT ( 'NONE',  ( 0.1532563361054082862, 26.21726448433411605, 2.638427012816831674 ) ) ;
#24126 = CARTESIAN_POINT ( 'NONE',  ( 0.5774900079438590739, 62.64701867748817676, -5.440088680355550821 ) ) ;
#24127 = DIRECTION ( 'NONE',  ( -0.000000000000000000, -1.000000000000000000, -0.000000000000000000 ) ) ;
#24128 = CARTESIAN_POINT ( 'NONE',  ( 13.79529636645031943, 20.34541550158063572, -14.16423886937409904 ) ) ;
#24129 = ADVANCED_FACE ( 'NONE', ( #31286 ), #55272, .T. ) ;
#24130 = UNCERTAINTY_MEASURE_WITH_UNIT (LENGTH_MEASURE( 1.000000000000000082E-05 ), #91066, 'distance_accuracy_value', 'NONE');
#24131 = CARTESIAN_POINT ( 'NONE',  ( 14.92337183194729988, 64.34226448433412315, -8.527530157486177487 ) ) ;
#24132 = ORIENTED_EDGE ( 'NONE', *, *, #60401, .T. ) ;
#24133 = ORIENTED_EDGE ( 'NONE', *, *, #731, .T. ) ;
#24134 = CARTESIAN_POINT ( 'NONE',  ( -2.266590686148945544, 37.22041550158063217, 7.082119434687048631 ) ) ;
#24135 = CARTESIAN_POINT ( 'NONE',  ( 24.16423886937410614, 34.30374883491396787, 8.672049930838204340E-16 ) ) ;
#24136 = CARTESIAN_POINT ( 'NONE',  ( 14.92337183194729988, 4.342264484334117824, -8.527530157486177487 ) ) ;
#24137 = CARTESIAN_POINT ( 'NONE',  ( 0.1532563361054100626, 65.80059781766745175, -2.638427012816831230 ) ) ;
#24138 = CARTESIAN_POINT ( 'NONE',  ( -8.028887233259784040, -1.053223610215041184, 3.750000000000000000 ) ) ;
#24140 = CARTESIAN_POINT ( 'NONE',  ( 13.43411237798105340, 20.58196800326374643, 12.81628187352647963 ) ) ;
#24139 = CARTESIAN_POINT ( 'NONE',  ( 4.559911319644449179, 58.89701867748817676, 9.422509992056141925 ) ) ;
#24141 = CARTESIAN_POINT ( 'NONE',  ( -0.3689425029237881626, 27.42874883491397142, 10.36894250292379027 ) ) ;
#24142 = CARTESIAN_POINT ( 'NONE',  ( 17.96484262340118221, 26.18868534415483396, -7.964842623401177768 ) ) ;
#24143 = CARTESIAN_POINT ( 'NONE',  ( -9.010802615327971665, 14.76984942314624227, 11.91753657575775271 ) ) ;
#24144 = CARTESIAN_POINT ( 'NONE',  ( 20.88017736071110875, 50.77201867748817676, -2.915334737309920765 ) ) ;
#24145 = CARTESIAN_POINT ( 'NONE',  ( 9.846743663894594434, -11.49106884899921077, -2.168404344971008868E-15 ) ) ;
#24146 = ORIENTED_EDGE ( 'NONE', *, *, #45124, .F. ) ;
#24147 = FACE_OUTER_BOUND ( 'NONE', #5234, .T. ) ;
#24148 = EDGE_LOOP ( 'NONE', ( #22464, #70646, #41249 ) ) ;
#24149 = TOROIDAL_SURFACE ( 'NONE', #1819, 0.5000000000000000000, 0.2500000000000000000 ) ;
#24150 = CARTESIAN_POINT ( 'NONE',  ( 24.16423886937410614, 9.512082168247301794, -3.795296366450302550 ) ) ;
#24152 = CARTESIAN_POINT ( 'NONE',  ( 24.16423886937410614, 59.30374883491397497, 8.672049930838204340E-16 ) ) ;
#24151 = CARTESIAN_POINT ( 'NONE',  ( -4.164238869374098151, 61.59541550158063217, -3.795296366450310543 ) ) ;
#24154 = CARTESIAN_POINT ( 'NONE',  ( 18.52753015748617571, 58.09226448433411605, 4.923371831947298993 ) ) ;
#24153 = CARTESIAN_POINT ( 'NONE',  ( 1.472469842513823179, 40.59226448433411605, -4.923371831947296329 ) ) ;
#24155 = DIRECTION ( 'NONE',  ( 0.000000000000000000, 0.000000000000000000, 1.000000000000000000 ) ) ;
#24156 = AXIS2_PLACEMENT_3D ( 'NONE', #97887, #13873, #88880 ) ;
#24157 = CARTESIAN_POINT ( 'NONE',  ( 2.120353041430647068, 15.00000000000000000, -14.34413130794945523 ) ) ;
#24158 = B_SPLINE_CURVE_WITH_KNOTS ( 'NONE', 3,
 ( #4530, #95519, #26519, #78546, #56535, #64505 ),
 .UNSPECIFIED., .F., .F.,
 ( 4, 2, 4 ),
 ( 3.409110551496113072E-05, 0.0004400426677367864632, 0.0008459942299586118092 ),
 .UNSPECIFIED. ) ;
#24159 = VECTOR ( 'NONE', #72034, 1000.000000000000000 ) ;
#24160 = CARTESIAN_POINT ( 'NONE',  ( 6.565887622018943937, 8.081968003263751754, -12.81628187352647608 ) ) ;
#24161 = ORIENTED_EDGE ( 'NONE', *, *, #35008, .F. ) ;
#24162 = CARTESIAN_POINT ( 'NONE',  ( 20.36894250292379738, 44.92874883491396787, -10.36894250292379027 ) ) ;
#24163 = CARTESIAN_POINT ( 'NONE',  ( 6.204703633549690345, 45.76208216824729647, -14.16423886937410259 ) ) ;
#24164 = ORIENTED_EDGE ( 'NONE', *, *, #70002, .F. ) ;
#24165 = CARTESIAN_POINT ( 'NONE',  ( 4.559911319644449179, 18.89701867748817321, 9.422509992056141925 ) ) ;
#24166 = FACE_OUTER_BOUND ( 'NONE', #14891, .T. ) ;
#24167 = CARTESIAN_POINT ( 'NONE',  ( 20.88017736071110164, 35.35535201082150536, 2.915334737309930979 ) ) ;
#24168 = CARTESIAN_POINT ( 'NONE',  ( 17.20831665107776587, 54.13393115100079456, -7.208316651077762316 ) ) ;
#24169 = CARTESIAN_POINT ( 'NONE',  ( 20.88017736071110519, 35.56368534415484106, 2.639326808657452039E-16 ) ) ;
#24170 =( BOUNDED_CURVE ( )  B_SPLINE_CURVE ( 3, ( #34810, #11820, #96825, #28302 ),
 .UNSPECIFIED., .F., .T. ) 
 B_SPLINE_CURVE_WITH_KNOTS ( ( 4, 4 ),
 ( 0.5528074785697332238, 0.7738571667627152095 ),
 .UNSPECIFIED. ) 
 CURVE ( )  GEOMETRIC_REPRESENTATION_ITEM ( )  RATIONAL_B_SPLINE_CURVE ( ( 1.000000000000000000, 0.9959322297119970191, 0.9959322297119970191, 1.000000000000000000 ) ) 
 REPRESENTATION_ITEM ( '' )  );
#24171 = CARTESIAN_POINT ( 'NONE',  ( 10.00000000000000178, 64.31368534415483396, 10.88017736071110342 ) ) ;
#24172 = CARTESIAN_POINT ( 'NONE',  ( -0.8801773607111008646, 33.27201867748817676, 2.915334737309923430 ) ) ;
#24173 = EDGE_CURVE ( 'NONE', #86034, #82667, #17295, .T. ) ;
#24174 =( BOUNDED_SURFACE ( )  B_SPLINE_SURFACE ( 1, 2, ( 
 ( #46256, #32707, #8735, #40717, #24735, #62712, #63203, #39254, #76740, #32210, #93211, #17241, #8256, #38756, #55212, #85728, #78214, #69744, #69257, #9725, #93707, #778, #31229, #61726, #25242, #40224, #82349, #81855, #72874, #42396, #27870, #88876, #13366, #4409, #20384, #58354, #96894, #50373, #34876, #66861, #50875, #59350, #12866, #65370, #96394, #97380, #35868, #73864, #43851, #95900, #28847, #81368, #43365, #28371, #26891, #74855, #35376, #5393, #66357, #80881, #51865, #58861, #74345, #89853, #57386, #13870, #19880, #27380, #5873, #36366, #89365, #44350, #12380, #42885, #21369, #6356, #57871, #20876, #65867, #64867, #95389, #88382, #87877, #51368, #19394, #49880, #73368, #80391, #11895, #4895, #23353, #61325, #68845, #83839, #75344, #91333, #54312, #97883, #16332, #37862, #46334, #22858, #98380, #38839, #38351, #6857, #7851, #14369, #15364, #53330, #69331, #45849, #855, #29343, #53835, #37368, #76335, #59845, #84347, #84825, #378, #91836, #90334, #30826, #44837, #30330, #14871, #98874, #67860, #90837, #31313, #29836, #60344, #76819, #15848, #45342, #60831, #22366, #46815, #8336, #61815, #77307, #92320, #21873, #23845, #83348, #36866, #67358, #52351, #52839, #82849, #75843, #7362, #68356, #86303, #48289, #93301, #33279, #17807, #55302, #18793, #10796, #71307, #92808, #2335, #10308, #2826, #78798, #87272, #79287, #49276, #25801, #1839, #8821, #63770, #39335, #40807, #85812, #25324, #56303, #70324, #17325, #40316, #32790, #86796, #94280, #24825, #77800, #69830, #78297, #33759, #63287, #47798, #18297, #93794, #48780, #55809, #1352, #31803, #9813, #41314, #70820, #71786, #32297, #64263, #3295, #94775, #62301, #9312, #39819, #26275, #24338, #56777, #54799, #85314, #16823, #47298, #62800, #4776, #96774, #19274, #35250, #42767, #12750, #65247, #49757, #81735, #65746, #74228, #27750, #80270, #12259, #66239, #97271, #20759, #28742, #73249, #5762, #79776, #26769, #42279, #28250, #34251, #96276, #58234, #20264, #51248, #13251, #59233, #43249, #88754, #11770, #19763, #72750, #50763, #57264, #95773, #4283, #58745, #43742, #64752, #27254, #73744, #34757, #81252, #11275, #5275, #89249, #36250, #57754, #88257, #66747, #89734, #50248, #35752, #21253, #87759, #80764, #41795, #72268, #3796, #95264, #23241, #53713, #44732, #61217, #44233, #74737, #90228, #30705, #60229, #69222, #76708, #29723, #22249, #8228, #7744, #68246, #38722, #747, #90724, #84232, #14251, #22742, #75727, #59732, #52725, #31200, #61693, #98266, #83231, #15740, #46223, #75229, #91720, #6250, #36754, #21759, #92209, #14755, #51751, #82235, #45229, #7242, #13750 ),
 ( #67244, #15251, #97769, #37748, #53225, #45728, #30214, #29233, #52240, #82732, #68728, #6742, #37259, #83728, #60717, #256, #67746, #98764, #91214, #76230, #38238, #84713, #33648, #93180, #2216, #17212, #9201, #10677, #47689, #2712, #18182, #16215, #71672, #77686, #54683, #40686, #71187, #78182, #41192, #70202, #39713, #56184, #48662, #24217, #9695, #24706, #64144, #23735, #62182, #54198, #25211, #40189, #70697, #92692, #86677, #32675, #63169, #10193, #48170, #55691, #93676, #85205, #86189, #3182, #46700, #77199, #55177, #33164, #17699, #16709, #25693, #78682, #47182, #63658, #1237, #94164, #79164, #8704, #39221, #69707, #31692, #1721, #32177, #62680, #85692, #43132, #43626, #27636, #50642, #56661, #58121, #72149, #88136, #72633, #87150, #12633, #34139, #50141, #18675, #73624, #74112, #88629, #81131, #49161, #20138, #3677, #19649, #4165, #57641, #64631, #49637, #28131, #95140, #26651, #35637, #5147, #34633, #80650, #57147, #5646, #12144, #66123, #36122, #42649, #79664, #96153, #42170, #51130, #94661, #73125, #87644, #4667, #58631, #96652, #89130, #35129, #65628, #80145, #20641, #81620, #65132, #26170, #13129, #11160, #41680, #19158, #11655, #95653, #27137, #46107, #38123, #8109, #83613, #59614, #68611, #37624, #75609, #15128, #6133, #140, #29598, #90601, #30095, #28627, #76591, #37133, #45102, #60100, #52122, #53592, #22128, #45603, #61094, #59114, #15622, #21636, #97647, #76101, #7632, #52609, #84106, #14132, #82616, #30589, #91604, #67122, #83110, #67628, #66630, #97159, #36639, #89624, #68120, #14639, #7120, #29111, #23120, #98646, #60602, #53103, #91097, #22624, #21136, #90111, #51637, #82116, #13626, #44108, #98137, #74619, #44617, #75113, #6619, #40077, #8594, #9577, #16098, #85580, #24597, #71074, #93066, #2599, #48052, #55062, #1112, #40577, #70578, #39101, #2105, #46585, #17094, #47576, #34397, #78072, #64885, #637, #55577, #77083, #32564, #31085, #86075, #87896, #63062, #93560, #61580, #25094, #69592, #32059, #16593, #1610, #31575, #92576, #95413, #62069, #24100, #78566, #17587, #47070, #62562, #54569, #19412, #10076, #26908, #80413, #57405, #92091, #49903, #85085, #38604, #69103, #23619, #77568, #54084, #84600, #9084, #39598, #70086, #51388, #96412, #36387, #20899, #58375, #21891, #13890, #74366, #95917, #5413, #13386, #5895, #89385, #90353, #82367, #52369, #28868, #4912, #44374, #81874, #43870, #59371, #50393, #74872, #73883, #35884, #66882, #72895, #11913, #81386, #97399, #66380, #27888, #97905, #96913, #89875, #6372, #4429, #59866, #65884, #42903, #21389, #51886, #28390, #29363, #88896, #20405, #36886 ) ),
 .UNSPECIFIED., .F., .F., .T. ) 
 B_SPLINE_SURFACE_WITH_KNOTS ( ( 2, 2 ),
 ( 3, 2, 2, 2, 2, 2, 2, 2, 2, 2, 2, 2, 2, 2, 2, 2, 2, 2, 2, 2, 2, 2, 2, 2, 2, 2, 2, 2, 2, 2, 2, 2, 2, 2, 2, 2, 2, 2, 2, 2, 2, 2, 2, 2, 2, 2, 2, 2, 2, 2, 2, 2, 2, 2, 2, 2, 2, 2, 2, 2, 2, 2, 2, 2, 2, 2, 2, 2, 2, 2, 2, 2, 2, 2, 2, 2, 2, 2, 2, 2, 2, 2, 2, 2, 2, 2, 2, 2, 2, 2, 2, 2, 2, 2, 2, 2, 2, 2, 2, 2, 2, 2, 2, 2, 2, 2, 2, 2, 2, 2, 2, 2, 2, 2, 2, 2, 2, 2, 2, 2, 2, 2, 2, 2, 2, 2, 2, 2, 2, 2, 2, 2, 2, 2, 2, 2, 2, 2, 2, 2, 2, 2, 2, 2, 2, 2, 2, 2, 2, 2, 2, 2, 2, 2, 2, 2, 2, 2, 2, 2, 2, 2, 3 ),
 ( 0.000000000000000000, 1.000000000000000000 ),
 ( 0.000000000000000000, 0.005952380952380952051, 0.01190476190476190410, 0.01785714285714285615, 0.02380952380952380820, 0.02976190476190476025, 0.03571428571428571230, 0.04166666666666666435, 0.04761904761904761640, 0.05357142857142856845, 0.05952380952380952051, 0.06547619047619047949, 0.07142857142857142461, 0.07738095238095238360, 0.08333333333333332871, 0.08928571428571428770, 0.09523809523809523281, 0.1011904761904761918, 0.1071428571428571369, 0.1130952380952380959, 0.1190476190476190410, 0.1250000000000000000, 0.1309523809523809590, 0.1369047619047619180, 0.1428571428571428492, 0.1488095238095238082, 0.1547619047619047672, 0.1607142857142857262, 0.1666666666666666574, 0.1726190476190476164, 0.1785714285714285754, 0.1845238095238095344, 0.1904761904761904656, 0.1964285714285714246, 0.2023809523809523836, 0.2083333333333333426, 0.2142857142857142738, 0.2202380952380952328, 0.2261904761904761918, 0.2321428571428571508, 0.2380952380952380820, 0.2440476190476190410, 0.2500000000000000000, 0.2559523809523809312, 0.2619047619047619180, 0.2678571428571428492, 0.2738095238095238360, 0.2797619047619047672, 0.2857142857142856984, 0.2916666666666666852, 0.2976190476190476164, 0.3035714285714285476, 0.3095238095238095344, 0.3154761904761904656, 0.3214285714285714524, 0.3273809523809523836, 0.3333333333333333148, 0.3392857142857143016, 0.3452380952380952328, 0.3511904761904761640, 0.3571428571428571508, 0.3630952380952380820, 0.3690476190476190688, 0.3750000000000000000, 0.3809523809523809312, 0.3869047619047619180, 0.3928571428571428492, 0.3988095238095238360, 0.4047619047619047672, 0.4107142857142856984, 0.4166666666666666852, 0.4226190476190476164, 0.4285714285714285476, 0.4345238095238095344, 0.4404761904761904656, 0.4464285714285714524, 0.4523809523809523836, 0.4583333333333333148, 0.4642857142857143016, 0.4702380952380952328, 0.4761904761904761640, 0.4821428571428571508, 0.4880952380952380820, 0.4940476190476190688, 0.5000000000000000000, 0.5059523809523809312, 0.5119047619047618625, 0.5178571428571429047, 0.5238095238095238360, 0.5297619047619047672, 0.5357142857142856984, 0.5416666666666666297, 0.5476190476190476719, 0.5535714285714286031, 0.5595238095238095344, 0.5654761904761904656, 0.5714285714285713969, 0.5773809523809523281, 0.5833333333333333703, 0.5892857142857143016, 0.5952380952380952328, 0.6011904761904761640, 0.6071428571428570953, 0.6130952380952381375, 0.6190476190476190688, 0.6250000000000000000, 0.6309523809523809312, 0.6369047619047618625, 0.6428571428571429047, 0.6488095238095238360, 0.6547619047619047672, 0.6607142857142856984, 0.6666666666666666297, 0.6726190476190476719, 0.6785714285714286031, 0.6845238095238095344, 0.6904761904761904656, 0.6964285714285713969, 0.7023809523809523281, 0.7083333333333333703, 0.7142857142857143016, 0.7202380952380952328, 0.7261904761904761640, 0.7321428571428570953, 0.7380952380952381375, 0.7440476190476190688, 0.7500000000000000000, 0.7559523809523809312, 0.7619047619047618625, 0.7678571428571429047, 0.7738095238095238360, 0.7797619047619047672, 0.7857142857142856984, 0.7916666666666666297, 0.7976190476190476719, 0.8035714285714286031, 0.8095238095238095344, 0.8154761904761904656, 0.8214285714285713969, 0.8273809523809523281, 0.8333333333333333703, 0.8392857142857143016, 0.8452380952380952328, 0.8511904761904761640, 0.8571428571428570953, 0.8630952380952381375, 0.8690476190476190688, 0.8750000000000000000, 0.8809523809523809312, 0.8869047619047618625, 0.8928571428571429047, 0.8988095238095238360, 0.9047619047619047672, 0.9107142857142856984, 0.9166666666666666297, 0.9226190476190476719, 0.9285714285714286031, 0.9345238095238095344, 0.9404761904761904656, 0.9464285714285713969, 0.9523809523809523281, 0.9583333333333333703, 0.9642857142857143016 ),
 .UNSPECIFIED. ) 
 GEOMETRIC_REPRESENTATION_ITEM ( )  RATIONAL_B_SPLINE_SURFACE ( (
 ( 1.000000000000000000, 0.9659258262890683122, 1.000000000000000000, 0.9659258262890683122, 1.000000000000000000, 0.9659258262890683122, 1.000000000000000000, 0.9659258262890683122, 1.000000000000000000, 0.9659258262890683122, 1.000000000000000000, 0.9659258262890683122, 1.000000000000000000, 0.9659258262890683122, 1.000000000000000000, 0.9659258262890683122, 1.000000000000000000, 0.9659258262890683122, 1.000000000000000000, 0.9659258262890683122, 1.000000000000000000, 0.9659258262890683122, 1.000000000000000000, 0.9659258262890683122, 1.000000000000000000, 0.9659258262890683122, 1.000000000000000000, 0.9659258262890683122, 1.000000000000000000, 0.9659258262890683122, 1.000000000000000000, 0.9659258262890683122, 1.000000000000000000, 0.9659258262890683122, 1.000000000000000000, 0.9659258262890683122, 1.000000000000000000, 0.9659258262890683122, 1.000000000000000000, 0.9659258262890683122, 1.000000000000000000, 0.9659258262890683122, 1.000000000000000000, 0.9659258262890683122, 1.000000000000000000, 0.9659258262890683122, 1.000000000000000000, 0.9659258262890683122, 1.000000000000000000, 0.9659258262890683122, 1.000000000000000000, 0.9659258262890683122, 1.000000000000000000, 0.9659258262890683122, 1.000000000000000000, 0.9659258262890683122, 1.000000000000000000, 0.9659258262890683122, 1.000000000000000000, 0.9659258262890683122, 1.000000000000000000, 0.9659258262890683122, 1.000000000000000000, 0.9659258262890683122, 1.000000000000000000, 0.9659258262890683122, 1.000000000000000000, 0.9659258262890683122, 1.000000000000000000, 0.9659258262890683122, 1.000000000000000000, 0.9659258262890683122, 1.000000000000000000, 0.9659258262890683122, 1.000000000000000000, 0.9659258262890683122, 1.000000000000000000, 0.9659258262890683122, 1.000000000000000000, 0.9659258262890683122, 1.000000000000000000, 0.9659258262890683122, 1.000000000000000000, 0.9659258262890683122, 1.000000000000000000, 0.9659258262890683122, 1.000000000000000000, 0.9659258262890683122, 1.000000000000000000, 0.9659258262890683122, 1.000000000000000000, 0.9659258262890683122, 1.000000000000000000, 0.9659258262890683122, 1.000000000000000000, 0.9659258262890683122, 1.000000000000000000, 0.9659258262890683122, 1.000000000000000000, 0.9659258262890683122, 1.000000000000000000, 0.9659258262890683122, 1.000000000000000000, 0.9659258262890683122, 1.000000000000000000, 0.9659258262890683122, 1.000000000000000000, 0.9659258262890683122, 1.000000000000000000, 0.9659258262890683122, 1.000000000000000000, 0.9659258262890683122, 1.000000000000000000, 0.9659258262890683122, 1.000000000000000000, 0.9659258262890683122, 1.000000000000000000, 0.9659258262890683122, 1.000000000000000000, 0.9659258262890683122, 1.000000000000000000, 0.9659258262890683122, 1.000000000000000000, 0.9659258262890683122, 1.000000000000000000, 0.9659258262890683122, 1.000000000000000000, 0.9659258262890683122, 1.000000000000000000, 0.9659258262890683122, 1.000000000000000000, 0.9659258262890683122, 1.000000000000000000, 0.9659258262890683122, 1.000000000000000000, 0.9659258262890683122, 1.000000000000000000, 0.9659258262890683122, 1.000000000000000000, 0.9659258262890683122, 1.000000000000000000, 0.9659258262890683122, 1.000000000000000000, 0.9659258262890683122, 1.000000000000000000, 0.9659258262890683122, 1.000000000000000000, 0.9659258262890683122, 1.000000000000000000, 0.9659258262890683122, 1.000000000000000000, 0.9659258262890683122, 1.000000000000000000, 0.9659258262890683122, 1.000000000000000000, 0.9659258262890683122, 1.000000000000000000, 0.9659258262890683122, 1.000000000000000000, 0.9659258262890683122, 1.000000000000000000, 0.9659258262890683122, 1.000000000000000000, 0.9659258262890683122, 1.000000000000000000, 0.9659258262890683122, 1.000000000000000000, 0.9659258262890683122, 1.000000000000000000, 0.9659258262890683122, 1.000000000000000000, 0.9659258262890683122, 1.000000000000000000, 0.9659258262890683122, 1.000000000000000000, 0.9659258262890683122, 1.000000000000000000, 0.9659258262890683122, 1.000000000000000000, 0.9659258262890683122, 1.000000000000000000, 0.9659258262890683122, 1.000000000000000000, 0.9659258262890683122, 1.000000000000000000, 0.9659258262890683122, 1.000000000000000000, 0.9659258262890683122, 1.000000000000000000, 0.9659258262890683122, 1.000000000000000000, 0.9659258262890683122, 1.000000000000000000, 0.9659258262890683122, 1.000000000000000000, 0.9659258262890683122, 1.000000000000000000, 0.9659258262890683122, 1.000000000000000000, 0.9659258262890683122, 1.000000000000000000, 0.9659258262890683122, 1.000000000000000000, 0.9659258262890683122, 1.000000000000000000, 0.9659258262890683122, 1.000000000000000000, 0.9659258262890683122, 1.000000000000000000, 0.9659258262890683122, 1.000000000000000000, 0.9659258262890683122, 1.000000000000000000, 0.9659258262890683122, 1.000000000000000000, 0.9659258262890683122, 1.000000000000000000, 0.9659258262890683122, 1.000000000000000000, 0.9659258262890683122, 1.000000000000000000, 0.9659258262890683122, 1.000000000000000000, 0.9659258262890683122, 1.000000000000000000, 0.9659258262890683122, 1.000000000000000000, 0.9659258262890683122, 1.000000000000000000, 0.9659258262890683122, 1.000000000000000000, 0.9659258262890683122, 1.000000000000000000, 0.9659258262890683122, 1.000000000000000000, 0.9659258262890683122, 1.000000000000000000, 0.9659258262890683122, 1.000000000000000000, 0.9659258262890683122, 1.000000000000000000, 0.9659258262890683122, 1.000000000000000000, 0.9659258262890683122, 1.000000000000000000, 0.9659258262890683122, 1.000000000000000000, 0.9659258262890683122, 1.000000000000000000, 0.9659258262890683122, 1.000000000000000000, 0.9659258262890683122, 1.000000000000000000, 0.9659258262890683122, 1.000000000000000000, 0.9659258262890683122, 1.000000000000000000, 0.9659258262890683122, 1.000000000000000000, 0.9659258262890683122, 1.000000000000000000, 0.9659258262890683122, 1.000000000000000000, 0.9659258262890683122, 1.000000000000000000, 0.9659258262890683122, 1.000000000000000000, 0.9659258262890683122, 1.000000000000000000, 0.9659258262890683122, 1.000000000000000000, 0.9659258262890683122, 1.000000000000000000, 0.9659258262890683122, 1.000000000000000000, 0.9659258262890683122, 1.000000000000000000, 0.9659258262890683122, 1.000000000000000000, 0.9659258262890683122, 1.000000000000000000, 0.9659258262890683122, 1.000000000000000000, 0.9659258262890683122, 1.000000000000000000, 0.9659258262890683122, 1.000000000000000000, 0.9659258262890683122, 1.000000000000000000, 0.9659258262890683122, 1.000000000000000000, 0.9659258262890683122, 1.000000000000000000, 0.9659258262890683122, 1.000000000000000000, 0.9659258262890683122, 1.000000000000000000, 0.9659258262890683122, 1.000000000000000000, 0.9659258262890683122, 1.000000000000000000, 0.9659258262890683122, 1.000000000000000000, 0.9659258262890683122, 1.000000000000000000, 0.9659258262890683122, 1.000000000000000000, 0.9659258262890683122, 1.000000000000000000, 0.9659258262890683122, 1.000000000000000000, 0.9659258262890683122, 1.000000000000000000, 0.9659258262890683122, 1.000000000000000000, 0.9659258262890683122, 1.000000000000000000, 0.9659258262890683122, 1.000000000000000000, 0.9659258262890683122, 1.000000000000000000, 0.9659258262890683122, 1.000000000000000000, 0.9659258262890683122, 1.000000000000000000),
 ( 1.000000000000000000, 0.9659258262890683122, 1.000000000000000000, 0.9659258262890683122, 1.000000000000000000, 0.9659258262890683122, 1.000000000000000000, 0.9659258262890683122, 1.000000000000000000, 0.9659258262890683122, 1.000000000000000000, 0.9659258262890683122, 1.000000000000000000, 0.9659258262890683122, 1.000000000000000000, 0.9659258262890683122, 1.000000000000000000, 0.9659258262890683122, 1.000000000000000000, 0.9659258262890683122, 1.000000000000000000, 0.9659258262890683122, 1.000000000000000000, 0.9659258262890683122, 1.000000000000000000, 0.9659258262890683122, 1.000000000000000000, 0.9659258262890683122, 1.000000000000000000, 0.9659258262890683122, 1.000000000000000000, 0.9659258262890683122, 1.000000000000000000, 0.9659258262890683122, 1.000000000000000000, 0.9659258262890683122, 1.000000000000000000, 0.9659258262890683122, 1.000000000000000000, 0.9659258262890683122, 1.000000000000000000, 0.9659258262890683122, 1.000000000000000000, 0.9659258262890683122, 1.000000000000000000, 0.9659258262890683122, 1.000000000000000000, 0.9659258262890683122, 1.000000000000000000, 0.9659258262890683122, 1.000000000000000000, 0.9659258262890683122, 1.000000000000000000, 0.9659258262890683122, 1.000000000000000000, 0.9659258262890683122, 1.000000000000000000, 0.9659258262890683122, 1.000000000000000000, 0.9659258262890683122, 1.000000000000000000, 0.9659258262890683122, 1.000000000000000000, 0.9659258262890683122, 1.000000000000000000, 0.9659258262890683122, 1.000000000000000000, 0.9659258262890683122, 1.000000000000000000, 0.9659258262890683122, 1.000000000000000000, 0.9659258262890683122, 1.000000000000000000, 0.9659258262890683122, 1.000000000000000000, 0.9659258262890683122, 1.000000000000000000, 0.9659258262890683122, 1.000000000000000000, 0.9659258262890683122, 1.000000000000000000, 0.9659258262890683122, 1.000000000000000000, 0.9659258262890683122, 1.000000000000000000, 0.9659258262890683122, 1.000000000000000000, 0.9659258262890683122, 1.000000000000000000, 0.9659258262890683122, 1.000000000000000000, 0.9659258262890683122, 1.000000000000000000, 0.9659258262890683122, 1.000000000000000000, 0.9659258262890683122, 1.000000000000000000, 0.9659258262890683122, 1.000000000000000000, 0.9659258262890683122, 1.000000000000000000, 0.9659258262890683122, 1.000000000000000000, 0.9659258262890683122, 1.000000000000000000, 0.9659258262890683122, 1.000000000000000000, 0.9659258262890683122, 1.000000000000000000, 0.9659258262890683122, 1.000000000000000000, 0.9659258262890683122, 1.000000000000000000, 0.9659258262890683122, 1.000000000000000000, 0.9659258262890683122, 1.000000000000000000, 0.9659258262890683122, 1.000000000000000000, 0.9659258262890683122, 1.000000000000000000, 0.9659258262890683122, 1.000000000000000000, 0.9659258262890683122, 1.000000000000000000, 0.9659258262890683122, 1.000000000000000000, 0.9659258262890683122, 1.000000000000000000, 0.9659258262890683122, 1.000000000000000000, 0.9659258262890683122, 1.000000000000000000, 0.9659258262890683122, 1.000000000000000000, 0.9659258262890683122, 1.000000000000000000, 0.9659258262890683122, 1.000000000000000000, 0.9659258262890683122, 1.000000000000000000, 0.9659258262890683122, 1.000000000000000000, 0.9659258262890683122, 1.000000000000000000, 0.9659258262890683122, 1.000000000000000000, 0.9659258262890683122, 1.000000000000000000, 0.9659258262890683122, 1.000000000000000000, 0.9659258262890683122, 1.000000000000000000, 0.9659258262890683122, 1.000000000000000000, 0.9659258262890683122, 1.000000000000000000, 0.9659258262890683122, 1.000000000000000000, 0.9659258262890683122, 1.000000000000000000, 0.9659258262890683122, 1.000000000000000000, 0.9659258262890683122, 1.000000000000000000, 0.9659258262890683122, 1.000000000000000000, 0.9659258262890683122, 1.000000000000000000, 0.9659258262890683122, 1.000000000000000000, 0.9659258262890683122, 1.000000000000000000, 0.9659258262890683122, 1.000000000000000000, 0.9659258262890683122, 1.000000000000000000, 0.9659258262890683122, 1.000000000000000000, 0.9659258262890683122, 1.000000000000000000, 0.9659258262890683122, 1.000000000000000000, 0.9659258262890683122, 1.000000000000000000, 0.9659258262890683122, 1.000000000000000000, 0.9659258262890683122, 1.000000000000000000, 0.9659258262890683122, 1.000000000000000000, 0.9659258262890683122, 1.000000000000000000, 0.9659258262890683122, 1.000000000000000000, 0.9659258262890683122, 1.000000000000000000, 0.9659258262890683122, 1.000000000000000000, 0.9659258262890683122, 1.000000000000000000, 0.9659258262890683122, 1.000000000000000000, 0.9659258262890683122, 1.000000000000000000, 0.9659258262890683122, 1.000000000000000000, 0.9659258262890683122, 1.000000000000000000, 0.9659258262890683122, 1.000000000000000000, 0.9659258262890683122, 1.000000000000000000, 0.9659258262890683122, 1.000000000000000000, 0.9659258262890683122, 1.000000000000000000, 0.9659258262890683122, 1.000000000000000000, 0.9659258262890683122, 1.000000000000000000, 0.9659258262890683122, 1.000000000000000000, 0.9659258262890683122, 1.000000000000000000, 0.9659258262890683122, 1.000000000000000000, 0.9659258262890683122, 1.000000000000000000, 0.9659258262890683122, 1.000000000000000000, 0.9659258262890683122, 1.000000000000000000, 0.9659258262890683122, 1.000000000000000000, 0.9659258262890683122, 1.000000000000000000, 0.9659258262890683122, 1.000000000000000000, 0.9659258262890683122, 1.000000000000000000, 0.9659258262890683122, 1.000000000000000000, 0.9659258262890683122, 1.000000000000000000, 0.9659258262890683122, 1.000000000000000000, 0.9659258262890683122, 1.000000000000000000, 0.9659258262890683122, 1.000000000000000000, 0.9659258262890683122, 1.000000000000000000, 0.9659258262890683122, 1.000000000000000000, 0.9659258262890683122, 1.000000000000000000, 0.9659258262890683122, 1.000000000000000000, 0.9659258262890683122, 1.000000000000000000, 0.9659258262890683122, 1.000000000000000000, 0.9659258262890683122, 1.000000000000000000, 0.9659258262890683122, 1.000000000000000000, 0.9659258262890683122, 1.000000000000000000, 0.9659258262890683122, 1.000000000000000000, 0.9659258262890683122, 1.000000000000000000, 0.9659258262890683122, 1.000000000000000000, 0.9659258262890683122, 1.000000000000000000, 0.9659258262890683122, 1.000000000000000000, 0.9659258262890683122, 1.000000000000000000, 0.9659258262890683122, 1.000000000000000000, 0.9659258262890683122, 1.000000000000000000, 0.9659258262890683122, 1.000000000000000000, 0.9659258262890683122, 1.000000000000000000, 0.9659258262890683122, 1.000000000000000000, 0.9659258262890683122, 1.000000000000000000, 0.9659258262890683122, 1.000000000000000000, 0.9659258262890683122, 1.000000000000000000, 0.9659258262890683122, 1.000000000000000000, 0.9659258262890683122, 1.000000000000000000, 0.9659258262890683122, 1.000000000000000000, 0.9659258262890683122, 1.000000000000000000, 0.9659258262890683122, 1.000000000000000000, 0.9659258262890683122, 1.000000000000000000, 0.9659258262890683122, 1.000000000000000000, 0.9659258262890683122, 1.000000000000000000, 0.9659258262890683122, 1.000000000000000000, 0.9659258262890683122, 1.000000000000000000, 0.9659258262890683122, 1.000000000000000000, 0.9659258262890683122, 1.000000000000000000, 0.9659258262890683122, 1.000000000000000000, 0.9659258262890683122, 1.000000000000000000) ) ) 
 REPRESENTATION_ITEM ( '' )  SURFACE ( )  );
#24177 = ORIENTED_EDGE ( 'NONE', *, *, #94487, .F. ) ;
#24176 = AXIS2_PLACEMENT_3D ( 'NONE', #84320, #75317, #83814 ) ;
#24175 = DIRECTION ( 'NONE',  ( -0.000000000000000000, 1.000000000000000000, 0.000000000000000000 ) ) ;
#24178 = CARTESIAN_POINT ( 'NONE',  ( -3.335599319945092844, -2.700684445899034447, 2.500000000000000888 ) ) ;
#24179 = ORIENTED_EDGE ( 'NONE', *, *, #97004, .T. ) ;
#24180 = CARTESIAN_POINT ( 'NONE',  ( 8.862917521832709866, -7.247543382048746707, 4.000000000000000000 ) ) ;
#24181 = CARTESIAN_POINT ( 'NONE',  ( 1.472469842513823179, 36.42559781766745175, 4.923371831947296329 ) ) ;
#24182 = EDGE_CURVE ( 'NONE', #51377, #57773, #70294, .T. ) ;
#24183 = DIRECTION ( 'NONE',  ( -0.9483236552061978797, 0.000000000000000000, -0.3173046564050965856 ) ) ;
#24184 =( GEOMETRIC_REPRESENTATION_CONTEXT ( 3 ) GLOBAL_UNCERTAINTY_ASSIGNED_CONTEXT ( ( #60375 ) ) GLOBAL_UNIT_ASSIGNED_CONTEXT ( ( #15029, #67524, #37528 ) ) REPRESENTATION_CONTEXT ( 'NONE', 'WORKASPACE' ) );
#24185 = CARTESIAN_POINT ( 'NONE',  ( 4.879999999999991900, 76.07179676972444327, -6.500000000000000888 ) ) ;
#24186 = CARTESIAN_POINT ( 'NONE',  ( 4.630000000000003446, 1.019547802438464545, 3.750000000000000000 ) ) ;
#24187 = EDGE_LOOP ( 'NONE', ( #84843, #35554, #25198, #17264 ) ) ;
#24188 = CYLINDRICAL_SURFACE ( 'NONE', #4547, 15.00000000000000000 ) ;
#24189 = CARTESIAN_POINT ( 'NONE',  ( 32.06412365047463453, 26.99999999999997868, -10.00000000000000000 ) ) ;
#24190 = CARTESIAN_POINT ( 'NONE',  ( 0.1532563361054082862, 51.21726448433412315, 2.638427012816831674 ) ) ;
#24191 = CARTESIAN_POINT ( 'NONE',  ( 10.00000000000000178, 53.05374883491396787, 14.16423886937410082 ) ) ;
#24192 = CARTESIAN_POINT ( 'NONE',  ( 10.00000000000000000, 64.75893115100078035, -9.846743663894594434 ) ) ;
#24193 = AXIS2_PLACEMENT_3D ( 'NONE', #18103, #26092, #56588 ) ;
#24194 = CARTESIAN_POINT ( 'NONE',  ( 1.472469842513823179, 20.59226448433411960, -4.923371831947296329 ) ) ;
#24195 = EDGE_CURVE ( 'NONE', #80952, #87032, #61058, .T. ) ;
#24196 = CARTESIAN_POINT ( 'NONE',  ( 19.38216949554541202, 45.99863466993041072, 9.382169495545424454 ) ) ;
#24197 = CARTESIAN_POINT ( 'NONE',  ( 14.92337183194729633, 62.67559781766745886, 8.527530157486181039 ) ) ;
#24198 = CARTESIAN_POINT ( 'NONE',  ( 15.44008868035555260, 59.73035201082151247, 9.422509992056143702 ) ) ;
#24199 = DIRECTION ( 'NONE',  ( 0.000000000000000000, 1.000000000000000000, 0.000000000000000000 ) ) ;
#24200 = ADVANCED_FACE ( 'NONE', ( #32761 ), #48748, .F. ) ;
#24201 = CARTESIAN_POINT ( 'NONE',  ( 12.91533473730992121, 54.52201867748816255, 10.88017736071110164 ) ) ;
#24202 = VERTEX_POINT ( 'NONE', #79257 ) ;
#24203 = CARTESIAN_POINT ( 'NONE',  ( -2.266590686148945544, 51.38708216824730357, -7.082119434687050408 ) ) ;
#24204 = DIRECTION ( 'NONE',  ( 1.000000000000000000, 0.000000000000000000, 0.000000000000000000 ) ) ;
#24205 = CARTESIAN_POINT ( 'NONE',  ( -0.8801773607111008646, 23.27201867748817676, 2.915334737309923430 ) ) ;
#24207 = CARTESIAN_POINT ( 'NONE',  ( 7.084665262690076126, 62.02201867748816966, -10.88017736071110164 ) ) ;
#24206 = CARTESIAN_POINT ( 'NONE',  ( -2.816281873526473856, 14.33196800326375531, 3.434112377981055619 ) ) ;
#24208 = CARTESIAN_POINT ( 'NONE',  ( 13.75801628063879711, 15.00000000000000000, -4.578972376164444746 ) ) ;
#24209 = EDGE_CURVE ( 'NONE', #13653, #61453, #55777, .T. ) ;
#24210 = CARTESIAN_POINT ( 'NONE',  ( 15.44008868035555793, 66.39701867748817676, -9.422509992056140149 ) ) ;
#24211 = DIRECTION ( 'NONE',  ( 0.3502073812594748148, 0.000000000000000000, -0.9366721892483949041 ) ) ;
#24213 = DIRECTION ( 'NONE',  ( -1.000000000000000000, 1.761140584748027129E-15, 0.000000000000000000 ) ) ;
#24212 = CARTESIAN_POINT ( 'NONE',  ( 10.00000000000000178, 54.31368534415484106, 10.88017736071110342 ) ) ;
#24214 = CARTESIAN_POINT ( 'NONE',  ( 12.63842701281683922, 44.55059781766745175, -9.846743663894590881 ) ) ;
#24215 = CARTESIAN_POINT ( 'NONE',  ( 12.63842701281683034, 7.467264484334118713, 9.846743663894596210 ) ) ;
#24216 = CARTESIAN_POINT ( 'NONE',  ( -5.440088680355547268, -36.10298132251183034, 9.422509992056143702 ) ) ;
#24217 = CARTESIAN_POINT ( 'NONE',  ( 22.81628187352648496, 6.831968003263753531, -3.434112377981050290 ) ) ;
#24219 = CARTESIAN_POINT ( 'NONE',  ( -0.05723567505238445763, 69.83236346210669865, -6.413539670616451360 ) ) ;
#24218 = CARTESIAN_POINT ( 'NONE',  ( -0.8801773607111009756, 8.063685344154837509, 1.068504757029289695E-15 ) ) ;
#24220 = CARTESIAN_POINT ( 'NONE',  ( 0.2751277870542967463, 70.00000000000000000, -6.000000000000000000 ) ) ;
#24221 = CARTESIAN_POINT ( 'NONE',  ( 24.16423886937409904, 39.09541550158062506, 3.795296366450317205 ) ) ;
#24222 = CARTESIAN_POINT ( 'NONE',  ( -0.3689425029237898834, 66.17874883491396076, -10.36894250292378850 ) ) ;
#24223 = CARTESIAN_POINT ( 'NONE',  ( 0.1532563361054083140, 36.00893115100078745, 1.131784320476157264E-15 ) ) ;
#24224 = CARTESIAN_POINT ( 'NONE',  ( 5.076628168052703671, 16.84226448433411960, 8.527530157486179263 ) ) ;
#24225 = CARTESIAN_POINT ( 'NONE',  ( 15.44008868035555793, 11.39701867748817143, -9.422509992056140149 ) ) ;
#24226 = MECHANICAL_DESIGN_GEOMETRIC_PRESENTATION_REPRESENTATION (  '', ( #64092 ), #80093 ) ;
#24227 = ORIENTED_EDGE ( 'NONE', *, *, #83791, .T. ) ;
#24228 = CARTESIAN_POINT ( 'NONE',  ( 19.84674366389459621, 43.50893115100078745, 7.409399052514197653E-17 ) ) ;
#24229 = CARTESIAN_POINT ( 'NONE',  ( 10.00000000000000000, 26.81368534415484106, -10.88017736071110342 ) ) ;
#24230 = CARTESIAN_POINT ( 'NONE',  ( 2.791683348922240793, 56.63393115100078035, 7.208316651077764092 ) ) ;
#24232 = CARTESIAN_POINT ( 'NONE',  ( 6.689969769698871360, -0.03417435944610275333, 12.58200319823975022 ) ) ;
#24231 = CARTESIAN_POINT ( 'NONE',  ( -4.164238869374098151, 11.59541550158063217, -3.795296366450310543 ) ) ;
#24233 = LINE ( 'NONE', #16725, #32826 ) ;
#24234 = UNCERTAINTY_MEASURE_WITH_UNIT (LENGTH_MEASURE( 1.000000000000000082E-05 ), #60767, 'distance_accuracy_value', 'NONE');
#24235 = CARTESIAN_POINT ( 'NONE',  ( 14.92337183194729633, 17.67559781766745175, 8.527530157486181039 ) ) ;
#24236 = CARTESIAN_POINT ( 'NONE',  ( -2.816281873526473856, 54.12363466993041783, 9.499525473075851096E-16 ) ) ;
#24237 = CARTESIAN_POINT ( 'NONE',  ( 0.1532563361054083140, 51.00893115100078745, 1.131784320476157264E-15 ) ) ;
#24238 = ORIENTED_EDGE ( 'NONE', *, *, #31687, .T. ) ;
#24239 = CARTESIAN_POINT ( 'NONE',  ( 17.20831665107776587, 19.13393115100078035, -7.208316651077762316 ) ) ;
#24240 = CARTESIAN_POINT ( 'NONE',  ( 8.705944879585906904, -3.115743166039381951, -4.000000000000000000 ) ) ;
#24241 = CARTESIAN_POINT ( 'NONE',  ( -9.000000000000000000, 75.76920769491746910, 2.900000000000000355 ) ) ;
#24242 = CARTESIAN_POINT ( 'NONE',  ( -2.266590686148945544, 57.22041550158063217, 7.082119434687048631 ) ) ;
#24243 = CARTESIAN_POINT ( 'NONE',  ( 19.42250999205614193, 55.14701867748817676, 5.440088680355555262 ) ) ;
#24244 = SURFACE_STYLE_USAGE ( .BOTH. , #98789 ) ;
#24245 = CARTESIAN_POINT ( 'NONE',  ( 7.084665262690076126, 62.02201867748816966, -10.88017736071110164 ) ) ;
#24246 = CARTESIAN_POINT ( 'NONE',  ( 17.20831665107776587, 34.13393115100078745, -7.208316651077762316 ) ) ;
#24247 = CARTESIAN_POINT ( 'NONE',  ( 2.035157376598824452, 13.68868534415483751, 7.964842623401179544 ) ) ;
#24248 = CARTESIAN_POINT ( 'NONE',  ( 18.39792806157248251, 39.52224192338641728, 6.500000000000040856 ) ) ;
#24249 = CARTESIAN_POINT ( 'NONE',  ( 1.472469842513823179, 56.42559781766745886, 4.923371831947296329 ) ) ;
#24250 = CARTESIAN_POINT ( 'NONE',  ( 20.88017736071110519, 55.56368534415484817, 2.639326808657452039E-16 ) ) ;
#24251 = EDGE_CURVE ( 'NONE', #88687, #44437, #6756, .T. ) ;
#24252 = SURFACE_STYLE_USAGE ( .BOTH. , #46733 ) ;
#24253 = CIRCLE ( 'NONE', #70560, 0.5000000000000004441 ) ;
#24254 = ORIENTED_EDGE ( 'NONE', *, *, #76203, .F. ) ;
#24255 = AXIS2_PLACEMENT_3D ( 'NONE', #14341, #44813, #45320 ) ;
#24256 = ORIENTED_EDGE ( 'NONE', *, *, #27789, .F. ) ;
#24257 = FACE_OUTER_BOUND ( 'NONE', #97602, .T. ) ;
#24258 = CARTESIAN_POINT ( 'NONE',  ( 14.92337183194729988, 49.34226448433411605, -8.527530157486177487 ) ) ;
#24259 = CARTESIAN_POINT ( 'NONE',  ( 17.20831665107776587, 22.88393115100078745, 7.208316651077764980 ) ) ;
#24260 = CARTESIAN_POINT ( 'NONE',  ( 21.09922568453594849, 61.20696800326376064, 6.408140936763242479 ) ) ;
#24262 = CARTESIAN_POINT ( 'NONE',  ( 12.63842701281683034, 42.46726448433412315, 9.846743663894596210 ) ) ;
#24261 = CARTESIAN_POINT ( 'NONE',  ( 0.5774900079438590739, 17.64701867748817321, -5.440088680355550821 ) ) ;
#24263 = CARTESIAN_POINT ( 'NONE',  ( 14.09356342482593583, 14.95077488074853456, 4.360913911515476471 ) ) ;
#24264 = CARTESIAN_POINT ( 'NONE',  ( 10.00000000000000000, 45.55374883491397497, -14.16423886937410082 ) ) ;
#24265 = CARTESIAN_POINT ( 'NONE',  ( 6.204703633549690345, 62.84541550158063927, 14.16423886937410082 ) ) ;
#24266 = CARTESIAN_POINT ( 'NONE',  ( -4.431036607602396593, 0.3639312379444145651, -14.33059365769920213 ) ) ;
#24267 = CARTESIAN_POINT ( 'NONE',  ( 17.90558034491757056, 78.11737700066547063, 4.059948642090509985 ) ) ;
#24268 = CARTESIAN_POINT ( 'NONE',  ( 4.559911319644449179, 53.89701867748817676, 9.422509992056141925 ) ) ;
#24269 = CARTESIAN_POINT ( 'NONE',  ( 7.361572987183170547, 22.05059781766745530, 9.846743663894590881 ) ) ;
#24270 = CARTESIAN_POINT ( 'NONE',  ( -7.374934931933696092, -78.83424294380051833, 4.000000000000000888 ) ) ;
#24271 = ORIENTED_EDGE ( 'NONE', *, *, #10327, .T. ) ;
#24272 = CARTESIAN_POINT ( 'NONE',  ( 0.7117905103455572924, 0.000000000000000000, -5.406585696355421966 ) ) ;
#24273 = STYLED_ITEM ( 'NONE', ( #18527 ), #75423 ) ;
#24274 = EDGE_LOOP ( 'NONE', ( #25186, #62887, #13200, #17002 ) ) ;
#24275 = CARTESIAN_POINT ( 'NONE',  ( 1.472469842513823179, 10.59226448433411782, -4.923371831947296329 ) ) ;
#24276 = ORIENTED_EDGE ( 'NONE', *, *, #4812, .F. ) ;
#24277 = CARTESIAN_POINT ( 'NONE',  ( -4.164238869374099039, 16.80374883491396787, 8.674139862899312516E-16 ) ) ;
#24278 = CARTESIAN_POINT ( 'NONE',  ( 1.472469842513823179, 16.42559781766745175, 4.923371831947296329 ) ) ;
#24279 = CARTESIAN_POINT ( 'NONE',  ( 7.084665262690076126, 47.02201867748818387, -10.88017736071110164 ) ) ;
#24280 = DIRECTION ( 'NONE',  ( -0.000000000000000000, -1.000000000000000000, -0.000000000000000000 ) ) ;
#24281 = VERTEX_POINT ( 'NONE', #48258 ) ;
#24282 = CARTESIAN_POINT ( 'NONE',  ( 0.5774900079438607392, 43.48035201082151247, 5.440088680355550821 ) ) ;
#24283 = VERTEX_POINT ( 'NONE', #78770 ) ;
#24284 = CARTESIAN_POINT ( 'NONE',  ( -0.8801773607111009756, 43.06368534415484106, 1.068504757029289695E-15 ) ) ;
#24285 = CARTESIAN_POINT ( 'NONE',  ( 2.917880565312948704, 2.637082168247300906, 12.26659068614894643 ) ) ;
#24286 = ORIENTED_EDGE ( 'NONE', *, *, #90296, .F. ) ;
#24287 = ORIENTED_EDGE ( 'NONE', *, *, #82743, .T. ) ;
#24288 = CARTESIAN_POINT ( 'NONE',  ( 6.565887622018943937, 20.16530133659708213, 12.81628187352647430 ) ) ;
#24289 = PRESENTATION_STYLE_ASSIGNMENT (( #37326 ) ) ;
#24290 = CARTESIAN_POINT ( 'NONE',  ( 1.472469842513823179, 6.425597817667451750, 4.923371831947296329 ) ) ;
#24291 = FACE_OUTER_BOUND ( 'NONE', #68423, .T. ) ;
#24292 = EDGE_CURVE ( 'NONE', #15989, #38758, #33252, .T. ) ;
#24293 = DIRECTION ( 'NONE',  ( -0.000000000000000000, 0.000000000000000000, 1.000000000000000000 ) ) ;
#24294 = CARTESIAN_POINT ( 'NONE',  ( 1.472469842513823179, 10.59226448433411782, -4.923371831947296329 ) ) ;
#24295 = CARTESIAN_POINT ( 'NONE',  ( 0.5774900079438607392, 38.48035201082150536, 5.440088680355550821 ) ) ;
#24296 = ORIENTED_EDGE ( 'NONE', *, *, #17533, .T. ) ;
#24297 = EDGE_CURVE ( 'NONE', #70269, #48471, #10768, .T. ) ;
#24298 = VECTOR ( 'NONE', #67054, 1000.000000000000000 ) ;
#24299 = ORIENTED_EDGE ( 'NONE', *, *, #80819, .T. ) ;
#24300 = B_SPLINE_CURVE_WITH_KNOTS ( 'NONE', 3,
 ( #29130, #37642, #68139, #68629 ),
 .UNSPECIFIED., .F., .F.,
 ( 4, 4 ),
 ( 1.097135458930219133E-17, 0.001060528352561998294 ),
 .UNSPECIFIED. ) ;
#24301 = LINE ( 'NONE', #76301, #21592 ) ;
#24302 = CARTESIAN_POINT ( 'NONE',  ( 17.96484262340118221, 54.93868534415484106, 7.964842623401181321 ) ) ;
#24303 = CARTESIAN_POINT ( 'NONE',  ( -14.88585913059898225, 14.76984981697404464, 1.278057234793719354 ) ) ;
#24304 = DIRECTION ( 'NONE',  ( 1.000000000000000000, 0.000000000000000000, 0.000000000000000000 ) ) ;
#24305 = CARTESIAN_POINT ( 'NONE',  ( 0.5774900079438607392, 58.48035201082151247, 5.440088680355550821 ) ) ;
#24306 = EDGE_CURVE ( 'NONE', #18620, #3959, #25629, .T. ) ;
#24307 = CARTESIAN_POINT ( 'NONE',  ( 6.565887622018943937, 8.081968003263751754, -12.81628187352647608 ) ) ;
#24308 = CARTESIAN_POINT ( 'NONE',  ( -37.92076923076924544, 94.65384615384614619, -9.500000000000000000 ) ) ;
#24309 = CARTESIAN_POINT ( 'NONE',  ( 14.92337183194729988, 29.34226448433411960, -8.527530157486177487 ) ) ;
#24310 = CARTESIAN_POINT ( 'NONE',  ( 19.38216949554541202, 50.99863466993042493, 9.382169495545424454 ) ) ;
#24311 = CARTESIAN_POINT ( 'NONE',  ( 22.26659068614894466, 8.887082168247300018, 7.082119434687054849 ) ) ;
#24312 = CARTESIAN_POINT ( 'NONE',  ( 12.63842701281683034, 17.46726448433411250, 9.846743663894596210 ) ) ;
#24313 = CARTESIAN_POINT ( 'NONE',  ( 13.43411237798105340, 25.58196800326374998, 12.81628187352647963 ) ) ;
#24315 = CARTESIAN_POINT ( 'NONE',  ( 1.114591949024928752, 4.429576435485488210E-16, 14.45709807627965304 ) ) ;
#24314 = DIRECTION ( 'NONE',  ( -1.000000000000000000, 5.782411586589362323E-17, 0.000000000000000000 ) ) ;
#24316 = CARTESIAN_POINT ( 'NONE',  ( 15.44008868035555260, 44.73035201082151247, 9.422509992056143702 ) ) ;
#24317 = CARTESIAN_POINT ( 'NONE',  ( 2.791683348922240793, 61.63393115100079456, 7.208316651077764092 ) ) ;
#24318 =( NAMED_UNIT ( * ) PLANE_ANGLE_UNIT ( ) SI_UNIT ( $, .RADIAN. ) );
#24319 = CARTESIAN_POINT ( 'NONE',  ( 12.63842701281683922, 24.55059781766745175, -9.846743663894590881 ) ) ;
#24320 = CARTESIAN_POINT ( 'NONE',  ( 12.91533473730993009, 11.60535201082150536, -10.88017736071109987 ) ) ;
#24321 = CARTESIAN_POINT ( 'NONE',  ( 22.81628187352647785, 21.41530133659708923, 3.434112377981063169 ) ) ;
#24322 = CIRCLE ( 'NONE', #84973, 0.5000000000000000000 ) ;
#24323 = CARTESIAN_POINT ( 'NONE',  ( 17.96484262340118221, 4.938685344154837509, 7.964842623401181321 ) ) ;
#24324 =( NAMED_UNIT ( * ) PLANE_ANGLE_UNIT ( ) SI_UNIT ( $, .RADIAN. ) );
#24325 = CARTESIAN_POINT ( 'NONE',  ( 11.48952521350825151, 15.00000000000000000, -8.845383562535966249 ) ) ;
#24326 = CARTESIAN_POINT ( 'NONE',  ( 17.96484262340118221, 14.93868534415484106, 7.964842623401181321 ) ) ;
#24327 = AXIS2_PLACEMENT_3D ( 'NONE', #29315, #75315, #53807 ) ;
#24328 = AXIS2_PLACEMENT_3D ( 'NONE', #44587, #43599, #37104 ) ;
#24330 = CARTESIAN_POINT ( 'NONE',  ( 20.88017736071110164, 15.35535201082150358, 2.915334737309930979 ) ) ;
#24329 = CARTESIAN_POINT ( 'NONE',  ( 17.20831665107776587, 37.88393115100078745, 7.208316651077764980 ) ) ;
#24331 = CARTESIAN_POINT ( 'NONE',  ( 5.500000000000000000, 60.50000000000000000, -5.000000000000000000 ) ) ;
#24332 = EDGE_CURVE ( 'NONE', #2137, #55638, #81819, .T. ) ;
#24333 = AXIS2_PLACEMENT_3D ( 'NONE', #49201, #79705, #11203 ) ;
#24334 = CARTESIAN_POINT ( 'NONE',  ( -0.8801773607111008646, 38.27201867748816255, 2.915334737309923430 ) ) ;
#24336 = FILL_AREA_STYLE_COLOUR ( '', #98967 ) ;
#24335 = CARTESIAN_POINT ( 'NONE',  ( -2.266590686148945544, 66.38708216824730357, -7.082119434687050408 ) ) ;
#24337 = CARTESIAN_POINT ( 'NONE',  ( 14.92337183194729633, 12.67559781766745353, 8.527530157486181039 ) ) ;
#24338 = CARTESIAN_POINT ( 'NONE',  ( 19.84674366389459266, 43.71726448433410894, -2.638427012816827677 ) ) ;
#24339 = DIRECTION ( 'NONE',  ( -1.000000000000000000, 5.818595309480552676E-17, -0.000000000000000000 ) ) ;
#24340 = CARTESIAN_POINT ( 'NONE',  ( -4.792102989642738287, 15.00000000000000000, -15.26149223938179134 ) ) ;
#24341 = CARTESIAN_POINT ( 'NONE',  ( 0.000000000000000000, 14.49999999999999822, 0.000000000000000000 ) ) ;
#24342 = ADVANCED_FACE ( 'NONE', ( #89216 ), #95743, .F. ) ;
#24343 = CARTESIAN_POINT ( 'NONE',  ( -8.107947183002034208, -3.126532598414448749, -4.000000000000000000 ) ) ;
#24344 = CARTESIAN_POINT ( 'NONE',  ( 17.08211943468705840, 20.13708216824730357, -12.26659068614894466 ) ) ;
#24345 = CARTESIAN_POINT ( 'NONE',  ( 1.472469842513823179, 40.59226448433411605, -4.923371831947296329 ) ) ;
#24346 = DIRECTION ( 'NONE',  ( 0.000000000000000000, -1.000000000000000000, 0.000000000000000000 ) ) ;
#24347 = ORIENTED_EDGE ( 'NONE', *, *, #9817, .F. ) ;
#24348 = CARTESIAN_POINT ( 'NONE',  ( 22.26659068614895176, 54.72041550158063217, -7.082119434687042414 ) ) ;
#24349 = CARTESIAN_POINT ( 'NONE',  ( 14.92337183194729633, 17.67559781766745175, 8.527530157486181039 ) ) ;
#24350 = CARTESIAN_POINT ( 'NONE',  ( 14.94699059465107105, 14.49999999999999112, 1.259949270174897329 ) ) ;
#24352 = B_SPLINE_CURVE_WITH_KNOTS ( 'NONE', 3,
 ( #79724, #32735, #11223, #39769, #70268, #63235 ),
 .UNSPECIFIED., .F., .F.,
 ( 4, 2, 4 ),
 ( 3.409110551495850831E-05, 0.0004400426677367822890, 0.0008459942299586060629 ),
 .UNSPECIFIED. ) ;
#24351 = CARTESIAN_POINT ( 'NONE',  ( -0.8801773607111008646, 43.27201867748817676, 2.915334737309923430 ) ) ;
#24353 = CARTESIAN_POINT ( 'NONE',  ( 22.81628187352647785, 56.62363466993042493, 6.195893100308588602E-16 ) ) ;
#24354 = CARTESIAN_POINT ( 'NONE',  ( 7.084665262690076126, 14.10535201082150358, 10.88017736071109987 ) ) ;
#24355 = CARTESIAN_POINT ( 'NONE',  ( 16.40814093676324603, 47.45696800326375353, -11.09922568453594671 ) ) ;
#24356 = CARTESIAN_POINT ( 'NONE',  ( 7.361572987183170547, 62.05059781766745886, 9.846743663894590881 ) ) ;
#24357 = CARTESIAN_POINT ( 'NONE',  ( 17.20831665107776587, 4.133931151000785675, -7.208316651077762316 ) ) ;
#24358 = EDGE_LOOP ( 'NONE', ( #65572, #40880, #31745, #69449 ) ) ;
#24359 = DIRECTION ( 'NONE',  ( -1.000000000000000000, 0.000000000000000000, 0.000000000000000000 ) ) ;
#24360 = CARTESIAN_POINT ( 'NONE',  ( 0.6076426042653192416, 17.37576471608601381, -6.500000000000002665 ) ) ;
#24361 = CARTESIAN_POINT ( 'NONE',  ( 24.16423886937410614, 54.51208216824730357, -3.795296366450302550 ) ) ;
#24362 = CARTESIAN_POINT ( 'NONE',  ( 13.79529636645030344, 8.262082168247300018, 14.16423886937410614 ) ) ;
#24363 = CARTESIAN_POINT ( 'NONE',  ( 12.91533473730992121, 14.52201867748817143, 10.88017736071110164 ) ) ;
#24364 = CARTESIAN_POINT ( 'NONE',  ( 2.035157376598822676, 32.43868534415483396, -7.964842623401177768 ) ) ;
#24365 = CARTESIAN_POINT ( 'NONE',  ( -12.60874940350953111, 3.965829894984375834E-16, 7.160268045226943379 ) ) ;
#24366 = DIRECTION ( 'NONE',  ( 1.000000000000000000, 0.000000000000000000, 0.000000000000000000 ) ) ;
#24367 = CARTESIAN_POINT ( 'NONE',  ( 0.1532563361054083140, 1.008931151000784787, 1.131784320476157264E-15 ) ) ;
#24368 =( NAMED_UNIT ( * ) SI_UNIT ( $, .STERADIAN. ) SOLID_ANGLE_UNIT ( ) );
#24369 = CARTESIAN_POINT ( 'NONE',  ( 10.00000000000000000, 19.75893115100078390, -9.846743663894594434 ) ) ;
#24370 = CARTESIAN_POINT ( 'NONE',  ( 19.72487221294570858, 70.00000000000000000, 6.500000000000000888 ) ) ;
#24371 = CARTESIAN_POINT ( 'NONE',  ( 10.00000000000000000, 14.75893115100078568, -9.846743663894594434 ) ) ;
#24372 = CARTESIAN_POINT ( 'NONE',  ( 18.52753015748617571, 38.09226448433412315, 4.923371831947298993 ) ) ;
#24373 = CARTESIAN_POINT ( 'NONE',  ( 4.559911319644449179, 18.89701867748817321, 9.422509992056141925 ) ) ;
#24374 = CARTESIAN_POINT ( 'NONE',  ( 16.40814093676324603, 27.45696800326375708, -11.09922568453594671 ) ) ;
#24376 = CARTESIAN_POINT ( 'NONE',  ( 18.52753015748617571, 13.09226448433411960, 4.923371831947298993 ) ) ;
#24375 = CARTESIAN_POINT ( 'NONE',  ( 10.00000000000000000, 40.55374883491397497, -14.16423886937410082 ) ) ;
#24377 = FACE_OUTER_BOUND ( 'NONE', #98835, .T. ) ;
#24378 = CARTESIAN_POINT ( 'NONE',  ( 0.1532563361054100626, 45.80059781766745886, -2.638427012816831230 ) ) ;
#24379 = CARTESIAN_POINT ( 'NONE',  ( 0.1532563361054082862, 36.21726448433410894, 2.638427012816831674 ) ) ;
#24380 = CARTESIAN_POINT ( 'NONE',  ( 6.204703633549690345, 12.84541550158063572, 14.16423886937410082 ) ) ;
#24381 = CARTESIAN_POINT ( 'NONE',  ( 15.44008868035555793, 41.39701867748817676, -9.422509992056140149 ) ) ;
#24382 = CARTESIAN_POINT ( 'NONE',  ( -0.8801773607110991993, 12.85535201082150358, -2.915334737309923874 ) ) ;
#24383 = CARTESIAN_POINT ( 'NONE',  ( 10.00000000000000178, 39.31368534415484106, 10.88017736071110342 ) ) ;
#24384 = EDGE_CURVE ( 'NONE', #11511, #83368, #84978, .T. ) ;
#24385 = CARTESIAN_POINT ( 'NONE',  ( 0.5774900079438607392, 28.48035201082150891, 5.440088680355550821 ) ) ;
#24386 = ORIENTED_EDGE ( 'NONE', *, *, #41465, .T. ) ;
#24387 = CARTESIAN_POINT ( 'NONE',  ( -1.099225684535947600, 33.70696800326375353, -6.408140936763238038 ) ) ;
#24388 = CARTESIAN_POINT ( 'NONE',  ( 0.5774900079438607392, 43.48035201082151247, 5.440088680355550821 ) ) ;
#24389 = ORIENTED_EDGE ( 'NONE', *, *, #21816, .F. ) ;
#24390 = EDGE_CURVE ( 'NONE', #35712, #28751, #89819, .T. ) ;
#24391 = CARTESIAN_POINT ( 'NONE',  ( 13.43411237798106583, 62.66530133659708923, -12.81628187352647252 ) ) ;
#24392 = CARTESIAN_POINT ( 'NONE',  ( 20.88017736071110875, 55.77201867748816966, -2.915334737309920765 ) ) ;
#24393 = VECTOR ( 'NONE', #5624, 1000.000000000000000 ) ;
#24394 = EDGE_LOOP ( 'NONE', ( #70260, #82942, #17749, #4602 ) ) ;
#24395 = CARTESIAN_POINT ( 'NONE',  ( 10.00000000000000000, 46.81368534415484106, -10.88017736071110342 ) ) ;
#24396 = CARTESIAN_POINT ( 'NONE',  ( 7.084665262690076126, 7.022018677488169658, -10.88017736071110164 ) ) ;
#24397 = CARTESIAN_POINT ( 'NONE',  ( 18.52753015748617571, 8.092264484334117824, 4.923371831947298993 ) ) ;
#24398 = CARTESIAN_POINT ( 'NONE',  ( -0.3289641300568005855, 24.27164270246084143, -5.963430220938281678 ) ) ;
#24399 = CARTESIAN_POINT ( 'NONE',  ( 22.26659068614894466, 53.88708216824731068, 7.082119434687054849 ) ) ;
#24400 = CARTESIAN_POINT ( 'NONE',  ( 7.084665262690076126, 67.02201867748817676, -10.88017736071110164 ) ) ;
#24401 = CARTESIAN_POINT ( 'NONE',  ( 22.26659068614894466, 3.887082168247300906, 7.082119434687054849 ) ) ;
#24402 = CIRCLE ( 'NONE', #32364, 0.2500000000000002220 ) ;
#24403 = AXIS2_PLACEMENT_3D ( 'NONE', #25916, #64866, #94893 ) ;
#24404 = CARTESIAN_POINT ( 'NONE',  ( 17.96484262340118221, 14.93868534415483751, 7.964842623401181321 ) ) ;
#24405 = CARTESIAN_POINT ( 'NONE',  ( 12.63842701281683034, 52.46726448433413026, 9.846743663894596210 ) ) ;
#24406 = B_SPLINE_CURVE_WITH_KNOTS ( 'NONE', 3,
 ( #16080, #32041, #71058, #84088, #78548, #2582 ),
 .UNSPECIFIED., .F., .F.,
 ( 4, 2, 4 ),
 ( 5.553824967135426632E-18, 0.0002605067024380933443, 0.0005210134048761811592 ),
 .UNSPECIFIED. ) ;
#24407 = ORIENTED_EDGE ( 'NONE', *, *, #10097, .T. ) ;
#24408 =( GEOMETRIC_REPRESENTATION_CONTEXT ( 3 ) GLOBAL_UNCERTAINTY_ASSIGNED_CONTEXT ( ( #87505 ) ) GLOBAL_UNIT_ASSIGNED_CONTEXT ( ( #40885, #24413, #85391 ) ) REPRESENTATION_CONTEXT ( 'NONE', 'WORKASPACE' ) );
#24409 = CARTESIAN_POINT ( 'NONE',  ( 2.791683348922240793, 41.63393115100078745, 7.208316651077764092 ) ) ;
#24410 = VECTOR ( 'NONE', #91346, 1000.000000000000000 ) ;
#24411 = CARTESIAN_POINT ( 'NONE',  ( 0.5774900079438590739, 37.64701867748817676, -5.440088680355550821 ) ) ;
#24412 = CARTESIAN_POINT ( 'NONE',  ( 2.791683348922237240, 35.38393115100079456, -7.208316651077763204 ) ) ;
#24414 = LINE ( 'NONE', #8411, #57441 ) ;
#24413 =( NAMED_UNIT ( * ) PLANE_ANGLE_UNIT ( ) SI_UNIT ( $, .RADIAN. ) );
#24415 = CARTESIAN_POINT ( 'NONE',  ( 20.88017736071110519, 40.56368534415484106, 2.639326808657452039E-16 ) ) ;
#24416 = CARTESIAN_POINT ( 'NONE',  ( 10.00000000000000000, 60.55374883491397497, -14.16423886937410082 ) ) ;
#24417 = EDGE_CURVE ( 'NONE', #89545, #24788, #72719, .T. ) ;
#24418 = CARTESIAN_POINT ( 'NONE',  ( 21.09922568453594849, 21.20696800326375353, 6.408140936763242479 ) ) ;
#24419 = DIRECTION ( 'NONE',  ( 0.000000000000000000, 1.000000000000000000, 0.000000000000000000 ) ) ;
#24420 = ORIENTED_EDGE ( 'NONE', *, *, #96003, .T. ) ;
#24421 = CARTESIAN_POINT ( 'NONE',  ( -2.816281873526473856, 24.12363466993042138, 9.499525473075851096E-16 ) ) ;
#24422 = CARTESIAN_POINT ( 'NONE',  ( 7.084665262690076126, 17.02201867748817676, -10.88017736071110164 ) ) ;
#24423 = EDGE_CURVE ( 'NONE', #91116, #89674, #71636, .T. ) ;
#24424 = ORIENTED_EDGE ( 'NONE', *, *, #92675, .T. ) ;
#24425 = AXIS2_PLACEMENT_3D ( 'NONE', #94423, #31939, #92943 ) ;
#24426 = CARTESIAN_POINT ( 'NONE',  ( 18.52753015748617571, 3.092264484334118269, 4.923371831947298993 ) ) ;
#24427 = CARTESIAN_POINT ( 'NONE',  ( 18.52753015748617571, 53.09226448433412315, 4.923371831947298993 ) ) ;
#24429 = CARTESIAN_POINT ( 'NONE',  ( 10.00000000000000000, 34.75893115100078745, -9.846743663894594434 ) ) ;
#24428 = CARTESIAN_POINT ( 'NONE',  ( 19.84674366389459266, 8.717264484334116048, -2.638427012816827677 ) ) ;
#24430 = CARTESIAN_POINT ( 'NONE',  ( -9.795238246328622722, -28.02849944208173127, 3.750000000000001332 ) ) ;
#24431 = CARTESIAN_POINT ( 'NONE',  ( 19.72487221294571569, 14.78217586085237656, 6.499999999999995559 ) ) ;
#24432 = CARTESIAN_POINT ( 'NONE',  ( 0.1532563361054083140, 26.00893115100078745, 1.131784320476157264E-15 ) ) ;
#24433 = CARTESIAN_POINT ( 'NONE',  ( 7.347880794884118750E-16, 17.03999999999999915, 0.000000000000000000 ) ) ;
#24434 = CARTESIAN_POINT ( 'NONE',  ( 34.56412365047464874, 29.50000000000000000, 9.500000000000000000 ) ) ;
#24435 = CARTESIAN_POINT ( 'NONE',  ( 1.472469842513823179, 16.42559781766745175, 4.923371831947296329 ) ) ;
#24437 = VERTEX_POINT ( 'NONE', #88718 ) ;
#24436 = CARTESIAN_POINT ( 'NONE',  ( 0.1532563361054083140, 46.00893115100079456, 1.131784320476157264E-15 ) ) ;
#24438 = VECTOR ( 'NONE', #22213, 1000.000000000000000 ) ;
#24439 = CARTESIAN_POINT ( 'NONE',  ( 20.24186590665278018, 17.61633188102327097, -6.114288769123028544 ) ) ;
#24440 = CARTESIAN_POINT ( 'NONE',  ( 13.43411237798105340, 30.58196800326374998, 12.81628187352647963 ) ) ;
#24441 = CARTESIAN_POINT ( 'NONE',  ( 0.2751277870542981341, 8.218334437839383000, 6.500000000000002665 ) ) ;
#24442 = CARTESIAN_POINT ( 'NONE',  ( 24.16423886937410614, 39.51208216824731068, -3.795296366450302550 ) ) ;
#24443 = CARTESIAN_POINT ( 'NONE',  ( 17.20831665107776587, 2.883931151000785231, 7.208316651077764980 ) ) ;
#24444 = CARTESIAN_POINT ( 'NONE',  ( -13.80105244023572197, 90.89655890636302615, 7.750000000000543565 ) ) ;
#24445 = CARTESIAN_POINT ( 'NONE',  ( 20.36894250292379382, 48.67874883491396076, 10.36894250292379205 ) ) ;
#24446 = ADVANCED_FACE ( 'NONE', ( #72236 ), #64720, .T. ) ;
#24447 = CARTESIAN_POINT ( 'NONE',  ( -0.3689425029237881626, 62.42874883491396787, 10.36894250292379027 ) ) ;
#24448 = CARTESIAN_POINT ( 'NONE',  ( 17.08211943468705130, 18.47041550158063572, 12.26659068614894998 ) ) ;
#24450 = DIRECTION ( 'NONE',  ( 0.000000000000000000, 0.000000000000000000, -1.000000000000000000 ) ) ;
#24449 = CARTESIAN_POINT ( 'NONE',  ( -4.164238869374099927, 32.01208216824730357, 3.795296366450308767 ) ) ;
#24451 = CARTESIAN_POINT ( 'NONE',  ( 6.673414917871782315, -55.62670566514463388, -3.750000000000000888 ) ) ;
#24453 = CARTESIAN_POINT ( 'NONE',  ( 10.00000000000000178, 47.25893115100078745, 9.846743663894594434 ) ) ;
#24452 = CARTESIAN_POINT ( 'NONE',  ( 6.757497259964397429, -58.30388498758440363, 2.500000000003219203 ) ) ;
#24454 = VERTEX_POINT ( 'NONE', #88224 ) ;
#24455 = CARTESIAN_POINT ( 'NONE',  ( 7.084665262690076126, 42.02201867748816966, -10.88017736071110164 ) ) ;
#24456 = CARTESIAN_POINT ( 'NONE',  ( 19.72487221294571214, 22.80223176428831877, -6.499999999999988454 ) ) ;
#24457 = DIRECTION ( 'NONE',  ( 0.000000000000000000, 1.000000000000000000, 0.000000000000000000 ) ) ;
#24458 = CARTESIAN_POINT ( 'NONE',  ( 10.00000000000000000, 39.75893115100078745, -9.846743663894594434 ) ) ;
#24459 = CARTESIAN_POINT ( 'NONE',  ( 21.09922568453594849, 56.20696800326375353, 6.408140936763242479 ) ) ;
#24460 = CARTESIAN_POINT ( 'NONE',  ( -14.16423886937410082, -3.196251165086032131, 4.336808689942017736E-15 ) ) ;
#24461 = STYLED_ITEM ( 'NONE', ( #32820 ), #66015 ) ;
#24462 = CARTESIAN_POINT ( 'NONE',  ( 0.1532563361054083140, 41.00893115100078745, 1.131784320476157264E-15 ) ) ;
#24463 = CARTESIAN_POINT ( 'NONE',  ( 18.52753015748618282, 63.92559781766745886, -4.923371831947291888 ) ) ;
#24464 = VERTEX_POINT ( 'NONE', #11742 ) ;
#24465 = CARTESIAN_POINT ( 'NONE',  ( 10.00000000000000178, 18.05374883491396787, 14.16423886937410082 ) ) ;
#24466 = LINE ( 'NONE', #79427, #62989 ) ;
#24468 = CARTESIAN_POINT ( 'NONE',  ( 0.8060400322139245066, 0.000000000000000000, -5.393339789881740565 ) ) ;
#24467 = CARTESIAN_POINT ( 'NONE',  ( -7.313705784284733724, 14.49999999999999112, 13.09617149020743199 ) ) ;
#24470 = AXIS2_PLACEMENT_3D ( 'NONE', #2912, #92407, #33363 ) ;
#24469 = CARTESIAN_POINT ( 'NONE',  ( 20.88017736071110519, 5.563685344154838397, 2.639326808657452039E-16 ) ) ;
#24471 = CARTESIAN_POINT ( 'NONE',  ( -1.099225684535947600, 13.70696800326375353, -6.408140936763238038 ) ) ;
#24472 = VECTOR ( 'NONE', #89262, 1000.000000000000000 ) ;
#24473 = FACE_OUTER_BOUND ( 'NONE', #76135, .T. ) ;
#24474 = CARTESIAN_POINT ( 'NONE',  ( 10.00000000000000178, 64.31368534415483396, 10.88017736071110342 ) ) ;
#24475 = CIRCLE ( 'NONE', #85132, 0.2500000000000002220 ) ;
#24476 = FACE_OUTER_BOUND ( 'NONE', #75742, .T. ) ;
#24477 = CARTESIAN_POINT ( 'NONE',  ( -46.94000000000001194, 101.2919103424992358, -7.700697297268528807 ) ) ;
#24478 = DIRECTION ( 'NONE',  ( 0.000000000000000000, 0.000000000000000000, 1.000000000000000000 ) ) ;
#24479 = CARTESIAN_POINT ( 'NONE',  ( 6.204703633549690345, 57.84541550158063927, 14.16423886937410082 ) ) ;
#24480 = CARTESIAN_POINT ( 'NONE',  ( 0.1916775849787236141, 42.25868815902070708, -6.499999999999983125 ) ) ;
#24481 = CARTESIAN_POINT ( 'NONE',  ( -0.8801773607111008646, 23.27201867748817676, 2.915334737309923430 ) ) ;
#24482 = CARTESIAN_POINT ( 'NONE',  ( 4.559911319644449179, 23.89701867748817321, 9.422509992056141925 ) ) ;
#24483 = CARTESIAN_POINT ( 'NONE',  ( 21.09922568453594849, 6.206968003263753531, 6.408140936763242479 ) ) ;
#24484 = CARTESIAN_POINT ( 'NONE',  ( 1.472469842513823179, 56.42559781766745886, 4.923371831947296329 ) ) ;
#24485 = CARTESIAN_POINT ( 'NONE',  ( 22.81628187352647785, 61.41530133659709634, 3.434112377981063169 ) ) ;
#24486 = CARTESIAN_POINT ( 'NONE',  ( 10.00000000000000178, 2.258931151000784787, 9.846743663894594434 ) ) ;
#24487 = ORIENTED_EDGE ( 'NONE', *, *, #95058, .T. ) ;
#24488 = CARTESIAN_POINT ( 'NONE',  ( 4.559911319644449179, 23.89701867748817321, 9.422509992056141925 ) ) ;
#24489 = CARTESIAN_POINT ( 'NONE',  ( -2.816281873526473856, 29.12363466993041783, 9.499525473075851096E-16 ) ) ;
#24490 = DIRECTION ( 'NONE',  ( -0.000000000000000000, -0.000000000000000000, 1.000000000000000000 ) ) ;
#24491 = CARTESIAN_POINT ( 'NONE',  ( 5.076628168052704559, 55.17559781766745175, -8.527530157486179263 ) ) ;
#24492 = CARTESIAN_POINT ( 'NONE',  ( -0.8801773607110991993, 52.85535201082151247, -2.915334737309923874 ) ) ;
#24493 = CARTESIAN_POINT ( 'NONE',  ( 14.92337183194729988, 14.34226448433411782, -8.527530157486177487 ) ) ;
#24494 = CARTESIAN_POINT ( 'NONE',  ( 3.591859063236761518, 29.95696800326375708, 11.09922568453594849 ) ) ;
#24496 = CARTESIAN_POINT ( 'NONE',  ( 13.34343830728404079, 0.5000000000000004441, -6.852200678592596184 ) ) ;
#24495 = CARTESIAN_POINT ( 'NONE',  ( 20.88017736071110875, 65.77201867748817676, -2.915334737309920765 ) ) ;
#24497 = CARTESIAN_POINT ( 'NONE',  ( -2.896551724137927497, 22.29452073070357088, 0.000000000000000000 ) ) ;
#24498 = CARTESIAN_POINT ( 'NONE',  ( 19.38216949554541202, 60.99863466993042493, 9.382169495545424454 ) ) ;
#24499 = EDGE_LOOP ( 'NONE', ( #14390, #8463, #70262, #22571 ) ) ;
#24500 = CARTESIAN_POINT ( 'NONE',  ( 3.836325488036083087, 0.3640475087720985159, 14.50112432709425470 ) ) ;
#24501 = DIRECTION ( 'NONE',  ( -0.000000000000000000, -0.000000000000000000, -1.000000000000000000 ) ) ;
#24502 = CARTESIAN_POINT ( 'NONE',  ( -0.8801773607111009756, 3.063685344154837509, 1.068504757029289695E-15 ) ) ;
#24504 = CARTESIAN_POINT ( 'NONE',  ( -4.164238869374099039, 11.80374883491396965, 8.674139862899312516E-16 ) ) ;
#24503 = CARTESIAN_POINT ( 'NONE',  ( 16.40814093676323893, 50.79030133659708923, 11.09922568453595026 ) ) ;
#24505 = CARTESIAN_POINT ( 'NONE',  ( 14.92337183194729633, 12.67559781766745353, 8.527530157486181039 ) ) ;
#24506 = CARTESIAN_POINT ( 'NONE',  ( 15.44008868035555793, 11.39701867748817143, -9.422509992056140149 ) ) ;
#24507 = CARTESIAN_POINT ( 'NONE',  ( 0.1532563361054083140, 26.00893115100078745, 1.131784320476157264E-15 ) ) ;
#24508 = DIRECTION ( 'NONE',  ( 0.000000000000000000, 0.000000000000000000, 1.000000000000000000 ) ) ;
#24509 = CARTESIAN_POINT ( 'NONE',  ( 6.204703633549690345, 62.84541550158063927, 14.16423886937410082 ) ) ;
#24510 = ORIENTED_EDGE ( 'NONE', *, *, #45945, .F. ) ;
#24511 = EDGE_CURVE ( 'NONE', #31058, #45767, #19243, .T. ) ;
#24512 =( NAMED_UNIT ( * ) PLANE_ANGLE_UNIT ( ) SI_UNIT ( $, .RADIAN. ) );
#24513 = CIRCLE ( 'NONE', #16512, 0.2500000000000002220 ) ;
#24514 = EDGE_CURVE ( 'NONE', #77456, #25656, #96241, .T. ) ;
#24515 = CARTESIAN_POINT ( 'NONE',  ( 10.00000000000000000, 1.813685344154837731, -10.88017736071110342 ) ) ;
#24516 = DIRECTION ( 'NONE',  ( -0.000000000000000000, -1.000000000000000000, -0.000000000000000000 ) ) ;
#24517 = ORIENTED_EDGE ( 'NONE', *, *, #42116, .F. ) ;
#24518 = ORIENTED_EDGE ( 'NONE', *, *, #35087, .T. ) ;
#24519 = TOROIDAL_SURFACE ( 'NONE', #42066, 14.49999999999999822, 0.5000000000000000000 ) ;
#24520 = CARTESIAN_POINT ( 'NONE',  ( 7.084665262690076126, 12.02201867748817321, -10.88017736071110164 ) ) ;
#24521 = CARTESIAN_POINT ( 'NONE',  ( 17.96484262340118221, 9.938685344154839285, 7.964842623401181321 ) ) ;
#24522 = CARTESIAN_POINT ( 'NONE',  ( 1.472469842513823179, 41.42559781766745886, 4.923371831947296329 ) ) ;
#24523 = CARTESIAN_POINT ( 'NONE',  ( -2.816281873526471635, 53.91530133659709634, -3.434112377981056508 ) ) ;
#24524 = CARTESIAN_POINT ( 'NONE',  ( -13.21382278599144300, 3.049318610115481221E-16, 6.271621331965429924 ) ) ;
#24526 = CARTESIAN_POINT ( 'NONE',  ( 6.204703633549690345, 22.84541550158062861, 14.16423886937410082 ) ) ;
#24525 = FACE_OUTER_BOUND ( 'NONE', #41264, .T. ) ;
#24527 = CARTESIAN_POINT ( 'NONE',  ( 17.96484262340118221, 19.93868534415484106, 7.964842623401181321 ) ) ;
#24528 = CARTESIAN_POINT ( 'NONE',  ( 7.084665262690076126, 9.105352010821503583, 10.88017736071109987 ) ) ;
#24529 = CARTESIAN_POINT ( 'NONE',  ( 0.1532563361054100626, 60.80059781766744464, -2.638427012816831230 ) ) ;
#24530 = DIRECTION ( 'NONE',  ( 0.000000000000000000, 0.000000000000000000, 1.000000000000000000 ) ) ;
#24531 = CARTESIAN_POINT ( 'NONE',  ( 10.00000000000000178, 32.25893115100078745, 9.846743663894594434 ) ) ;
#24532 = CARTESIAN_POINT ( 'NONE',  ( -45.94000000000000483, 92.00000000000000000, 5.000000000000000000 ) ) ;
#24533 = DIRECTION ( 'NONE',  ( 0.000000000000000000, -0.000000000000000000, -1.000000000000000000 ) ) ;
#24534 = CARTESIAN_POINT ( 'NONE',  ( -3.469446951953614189E-15, 24.75893115100079456, -9.846743663894594434 ) ) ;
#24535 = VERTEX_POINT ( 'NONE', #58715 ) ;
#24536 = FACE_OUTER_BOUND ( 'NONE', #67092, .T. ) ;
#24537 = CARTESIAN_POINT ( 'NONE',  ( -0.8801773607111008646, 68.27201867748817676, 2.915334737309923430 ) ) ;
#24538 = CARTESIAN_POINT ( 'NONE',  ( 0.1532563361054100626, 55.80059781766745175, -2.638427012816831230 ) ) ;
#24539 = CARTESIAN_POINT ( 'NONE',  ( 7.084665262690076126, 42.02201867748816966, -10.88017736071110164 ) ) ;
#24541 = CARTESIAN_POINT ( 'NONE',  ( -1.099225684535947600, 43.70696800326375353, -6.408140936763238038 ) ) ;
#24540 = CARTESIAN_POINT ( 'NONE',  ( 4.559911319644449179, 3.897018677488170990, 9.422509992056141925 ) ) ;
#24542 = CARTESIAN_POINT ( 'NONE',  ( 24.16423886937410614, 24.51208216824730002, -3.795296366450302550 ) ) ;
#24543 = B_SPLINE_CURVE_WITH_KNOTS ( 'NONE', 3,
 ( #51246, #97269, #34756, #80763 ),
 .UNSPECIFIED., .F., .F.,
 ( 4, 4 ),
 ( 0.000000000000000000, 0.0006109242138661622953 ),
 .UNSPECIFIED. ) ;
#24544 = ADVANCED_FACE ( 'NONE', ( #20229 ), #50733, .F. ) ;
#24545 = VECTOR ( 'NONE', #77821, 1000.000000000000000 ) ;
#24546 = CARTESIAN_POINT ( 'NONE',  ( 21.09922568453594849, 51.20696800326375353, 6.408140936763242479 ) ) ;
#24547 = ORIENTED_EDGE ( 'NONE', *, *, #31638, .T. ) ;
#24548 = AXIS2_PLACEMENT_3D ( 'NONE', #58090, #6098, #13594 ) ;
#24549 = CARTESIAN_POINT ( 'NONE',  ( 2.791683348922237240, 60.38393115100078745, -7.208316651077763204 ) ) ;
#24550 = EDGE_CURVE ( 'NONE', #47516, #53120, #10044, .T. ) ;
#24551 = CARTESIAN_POINT ( 'NONE',  ( 17.96484262340118221, 21.18868534415483396, -7.964842623401177768 ) ) ;
#24552 = MECHANICAL_DESIGN_GEOMETRIC_PRESENTATION_REPRESENTATION (  '', ( #26108 ), #35720 ) ;
#24553 = CARTESIAN_POINT ( 'NONE',  ( -0.8801773607110991993, 32.85535201082151247, -2.915334737309923874 ) ) ;
#24554 = ORIENTED_EDGE ( 'NONE', *, *, #16542, .T. ) ;
#24555 = CARTESIAN_POINT ( 'NONE',  ( 4.559911319644449179, 63.89701867748817676, 9.422509992056141925 ) ) ;
#24556 = CARTESIAN_POINT ( 'NONE',  ( -46.07478503777810630, 103.8690650836416722, 6.036883934524849948 ) ) ;
#24557 = CARTESIAN_POINT ( 'NONE',  ( 0.1532563361054100626, 10.80059781766745175, -2.638427012816831230 ) ) ;
#24558 = CARTESIAN_POINT ( 'NONE',  ( 19.42250999205614548, 60.98035201082151247, -5.440088680355545492 ) ) ;
#24559 = DIRECTION ( 'NONE',  ( -0.5519369853120501546, 0.000000000000000000, -0.8338858220671735433 ) ) ;
#24560 = CARTESIAN_POINT ( 'NONE',  ( 17.96484262340118221, 59.93868534415484106, 7.964842623401181321 ) ) ;
#24562 = ORIENTED_EDGE ( 'NONE', *, *, #37855, .T. ) ;
#24561 = CARTESIAN_POINT ( 'NONE',  ( 0.1532563361054082862, 1.217264484334117824, 2.638427012816831674 ) ) ;
#24563 = CARTESIAN_POINT ( 'NONE',  ( 7.361572987183169658, 44.96726448433412315, -9.846743663894592657 ) ) ;
#24564 = EDGE_LOOP ( 'NONE', ( #31463, #68136 ) ) ;
#24565 = ORIENTED_EDGE ( 'NONE', *, *, #71911, .T. ) ;
#24566 = CYLINDRICAL_SURFACE ( 'NONE', #31436, 15.00000000000000000 ) ;
#24567 = CARTESIAN_POINT ( 'NONE',  ( 10.00000000000000178, 3.053748834913967425, 14.16423886937410082 ) ) ;
#24568 =( BOUNDED_CURVE ( )  B_SPLINE_CURVE ( 2, ( #59330, #11379, #19859, #35355, #51349, #72855, #43832, #96874, #80373 ),
 .UNSPECIFIED., .F., .F. ) 
 B_SPLINE_CURVE_WITH_KNOTS ( ( 3, 2, 2, 2, 3 ),
 ( 0.4025141644748393976, 0.4047619047619047672, 0.4107142857142856984, 0.4166666666666666852, 0.4189144069537312220 ),
 .UNSPECIFIED. ) 
 CURVE ( )  GEOMETRIC_REPRESENTATION_ITEM ( )  RATIONAL_B_SPLINE_CURVE ( ( 0.9839835555609424134, 0.9871328979762477029, 1.000000000000000000, 0.9659258262890683122, 1.000000000000000000, 0.9659258262890683122, 1.000000000000000000, 0.9871328979762525879, 0.9839835555609448559 ) ) 
 REPRESENTATION_ITEM ( '' )  );
#24569 = CARTESIAN_POINT ( 'NONE',  ( 0.6178305044545818747, 63.49863466993043204, -9.382169495545419124 ) ) ;
#24570 = CARTESIAN_POINT ( 'NONE',  ( -4.164238869374099039, 6.803748834913967869, 8.674139862899312516E-16 ) ) ;
#24571 = CARTESIAN_POINT ( 'NONE',  ( -0.3689425029237898834, 21.17874883491396432, -10.36894250292378850 ) ) ;
#24572 = SURFACE_SIDE_STYLE ('',( #86047 ) ) ;
#24574 = CARTESIAN_POINT ( 'NONE',  ( 7.084665262690076126, 57.02201867748817676, -10.88017736071110164 ) ) ;
#24573 = DIRECTION ( 'NONE',  ( -0.000000000000000000, 1.000000000000000000, 0.000000000000000000 ) ) ;
#24575 = CARTESIAN_POINT ( 'NONE',  ( 17.96484262340118221, 19.93868534415484106, 7.964842623401181321 ) ) ;
#24576 = LINE ( 'NONE', #76071, #72199 ) ;
#24577 = VERTEX_POINT ( 'NONE', #59202 ) ;
#24578 = SURFACE_STYLE_FILL_AREA ( #76076 ) ;
#24579 = CARTESIAN_POINT ( 'NONE',  ( 16.40814093676323893, 25.79030133659708923, 11.09922568453595026 ) ) ;
#24581 = EDGE_CURVE ( 'NONE', #24283, #76727, #65906, .T. ) ;
#24580 = CARTESIAN_POINT ( 'NONE',  ( 19.84674366389459621, 33.50893115100078745, 7.409399052514197653E-17 ) ) ;
#24582 = CARTESIAN_POINT ( 'NONE',  ( 22.81628187352647785, 21.62363466993041783, 6.195893100308588602E-16 ) ) ;
#24583 = CARTESIAN_POINT ( 'NONE',  ( -9.898881779040587858, 15.00000000000000000, -10.25059215482589714 ) ) ;
#24584 = CARTESIAN_POINT ( 'NONE',  ( 7.361572987183169658, 19.96726448433411960, -9.846743663894592657 ) ) ;
#24585 = CARTESIAN_POINT ( 'NONE',  ( 7.361572987183170547, 12.05059781766744997, 9.846743663894590881 ) ) ;
#24586 = ORIENTED_EDGE ( 'NONE', *, *, #42772, .T. ) ;
#24587 = CARTESIAN_POINT ( 'NONE',  ( -0.8801773607110991993, 37.85535201082151247, -2.915334737309923874 ) ) ;
#24588 = CARTESIAN_POINT ( 'NONE',  ( 17.08211943468705130, 28.47041550158063572, 12.26659068614894998 ) ) ;
#24589 = CARTESIAN_POINT ( 'NONE',  ( 10.00000000000000178, 37.25893115100078745, 9.846743663894594434 ) ) ;
#24590 = CARTESIAN_POINT ( 'NONE',  ( -0.8801773607111008646, 63.27201867748817676, 2.915334737309923430 ) ) ;
#24592 = CARTESIAN_POINT ( 'NONE',  ( 9.050000000000002487, 99.99999999999998579, -8.000000000000000000 ) ) ;
#24591 = CARTESIAN_POINT ( 'NONE',  ( 22.81628187352647785, 51.62363466993042493, 6.195893100308588602E-16 ) ) ;
#24593 = CARTESIAN_POINT ( 'NONE',  ( -0.8801773607110991993, 32.85535201082151247, -2.915334737309923874 ) ) ;
#24594 = CARTESIAN_POINT ( 'NONE',  ( 19.38216949554541557, 22.24863466993041428, -9.382169495545420901 ) ) ;
#24595 = CARTESIAN_POINT ( 'NONE',  ( 19.84674366389459621, 43.50893115100078745, 7.409399052514197653E-17 ) ) ;
#24596 = CARTESIAN_POINT ( 'NONE',  ( -9.422509992056145478, -2.352981322511826789, -5.440088680355541939 ) ) ;
#24597 = CARTESIAN_POINT ( 'NONE',  ( 3.591859063236763294, 43.29030133659708923, -11.09922568453595026 ) ) ;
#24598 = DIRECTION ( 'NONE',  ( 0.000000000000000000, -0.000000000000000000, 1.000000000000000000 ) ) ;
#24600 = DIRECTION ( 'NONE',  ( -2.569960705150826877E-16, 1.000000000000000000, 0.000000000000000000 ) ) ;
#24599 = CARTESIAN_POINT ( 'NONE',  ( 20.88017736071110519, 50.56368534415484106, 2.639326808657452039E-16 ) ) ;
#24601 = CARTESIAN_POINT ( 'NONE',  ( -13.21272562211566104, -3.175103002782743638E-15, -6.271554226548334832 ) ) ;
#24602 = CARTESIAN_POINT ( 'NONE',  ( -12.34086200392831678, -0.03417435944610275333, 7.124999999999885425 ) ) ;
#24603 = CARTESIAN_POINT ( 'NONE',  ( 2.035157376598822676, 47.43868534415484817, -7.964842623401177768 ) ) ;
#24604 = CARTESIAN_POINT ( 'NONE',  ( 15.44008868035555793, 61.39701867748817676, -9.422509992056140149 ) ) ;
#24605 = DIRECTION ( 'NONE',  ( 0.000000000000000000, 1.000000000000000000, -0.000000000000000000 ) ) ;
#24606 = VECTOR ( 'NONE', #94199, 1000.000000000000000 ) ;
#24607 = CARTESIAN_POINT ( 'NONE',  ( 2.035157376598822676, 12.43868534415483751, -7.964842623401177768 ) ) ;
#24608 = CARTESIAN_POINT ( 'NONE',  ( 0.1532563361054082862, 46.21726448433411605, 2.638427012816831674 ) ) ;
#24610 = DIRECTION ( 'NONE',  ( -0.000000000000000000, 0.000000000000000000, -1.000000000000000000 ) ) ;
#24609 = CARTESIAN_POINT ( 'NONE',  ( 0.5774900079438607392, 23.48035201082150536, 5.440088680355550821 ) ) ;
#24611 = CARTESIAN_POINT ( 'NONE',  ( 16.40814093676324603, 22.45696800326375353, -11.09922568453594671 ) ) ;
#24612 = ORIENTED_EDGE ( 'NONE', *, *, #31257, .F. ) ;
#24613 = CARTESIAN_POINT ( 'NONE',  ( 15.44008868035555260, 34.73035201082151247, 9.422509992056143702 ) ) ;
#24614 = CIRCLE ( 'NONE', #15063, 1.750000000000000666 ) ;
#24616 = CARTESIAN_POINT ( 'NONE',  ( 20.03447792253739834, 47.65514106990689669, -6.401564815979719825 ) ) ;
#24615 = CARTESIAN_POINT ( 'NONE',  ( 22.81628187352648496, 6.831968003263753531, -3.434112377981050290 ) ) ;
#24617 = CARTESIAN_POINT ( 'NONE',  ( 7.084665262690076126, 14.10535201082150358, 10.88017736071109987 ) ) ;
#24618 = CARTESIAN_POINT ( 'NONE',  ( 15.44008868035555793, 36.39701867748816966, -9.422509992056140149 ) ) ;
#24619 = CARTESIAN_POINT ( 'NONE',  ( 17.08211943468705840, 45.13708216824730357, -12.26659068614894466 ) ) ;
#24620 = CARTESIAN_POINT ( 'NONE',  ( 0.1532563361054083140, 36.00893115100078745, 1.131784320476157264E-15 ) ) ;
#24621 = CARTESIAN_POINT ( 'NONE',  ( 17.96484262340118221, 56.18868534415484817, -7.964842623401177768 ) ) ;
#24622 = CARTESIAN_POINT ( 'NONE',  ( 19.72487221294570858, 70.00000000000000000, -6.000000000000000000 ) ) ;
#24623 = CARTESIAN_POINT ( 'NONE',  ( 24.16423886937410614, 19.30374883491397142, 8.672049930838204340E-16 ) ) ;
#24624 = EDGE_CURVE ( 'NONE', #57215, #34811, #44198, .T. ) ;
#24625 = FACE_OUTER_BOUND ( 'NONE', #75895, .T. ) ;
#24626 = CARTESIAN_POINT ( 'NONE',  ( 2.153642693323440493, 21.13791097397318453, -6.500000000000008882 ) ) ;
#24627 = ORIENTED_EDGE ( 'NONE', *, *, #54530, .T. ) ;
#24628 = CARTESIAN_POINT ( 'NONE',  ( -4.164238869374099039, 31.80374883491396432, 8.674139862899312516E-16 ) ) ;
#24629 = CARTESIAN_POINT ( 'NONE',  ( 2.917880565312950480, 35.97041550158063217, -12.26659068614894821 ) ) ;
#24630 = CARTESIAN_POINT ( 'NONE',  ( 14.92337183194729633, 7.675597817667451750, 8.527530157486181039 ) ) ;
#24631 = CARTESIAN_POINT ( 'NONE',  ( 14.92337183194729633, 57.67559781766745886, 8.527530157486181039 ) ) ;
#24632 = DIRECTION ( 'NONE',  ( -0.000000000000000000, -0.000000000000000000, 1.000000000000000000 ) ) ;
#24634 = CARTESIAN_POINT ( 'NONE',  ( -1.099225684535947600, 33.70696800326375353, -6.408140936763238038 ) ) ;
#24633 = CARTESIAN_POINT ( 'NONE',  ( 2.035157376598822676, 62.43868534415483396, -7.964842623401177768 ) ) ;
#24635 = CARTESIAN_POINT ( 'NONE',  ( 2.917880565312948704, 27.63708216824730357, 12.26659068614894643 ) ) ;
#24636 = CARTESIAN_POINT ( 'NONE',  ( 17.96484262340118221, 21.18868534415483396, -7.964842623401177768 ) ) ;
#24637 = CARTESIAN_POINT ( 'NONE',  ( -9.065164099344672266, 14.49999999999999112, 11.95084933600764820 ) ) ;
#24638 = CARTESIAN_POINT ( 'NONE',  ( 0.1532563361054083140, 1.008931151000784787, 1.131784320476157264E-15 ) ) ;
#24639 = CARTESIAN_POINT ( 'NONE',  ( -3.469446951953614189E-15, -10.24106884899921077, -9.846743663894594434 ) ) ;
#24640 = ORIENTED_EDGE ( 'NONE', *, *, #77270, .F. ) ;
#24641 = DIRECTION ( 'NONE',  ( -1.000000000000000000, 0.000000000000000000, 0.000000000000000000 ) ) ;
#24642 = FILL_AREA_STYLE_COLOUR ( '', #46083 ) ;
#24643 = VERTEX_POINT ( 'NONE', #6218 ) ;
#24644 = CARTESIAN_POINT ( 'NONE',  ( 20.36894250292379382, 3.678748834913967869, 10.36894250292379205 ) ) ;
#24646 = CARTESIAN_POINT ( 'NONE',  ( -0.8801773607110991993, 17.85535201082150536, -2.915334737309923874 ) ) ;
#24645 = CARTESIAN_POINT ( 'NONE',  ( -0.8801773607111009756, 8.063685344154837509, 1.068504757029289695E-15 ) ) ;
#24648 = CARTESIAN_POINT ( 'NONE',  ( 7.361572987183169658, 59.96726448433410894, -9.846743663894592657 ) ) ;
#24647 = CARTESIAN_POINT ( 'NONE',  ( 7.361572987183170547, 42.05059781766745886, 9.846743663894590881 ) ) ;
#24649 = DIRECTION ( 'NONE',  ( 1.000000000000000000, 2.569960705150834273E-16, 0.000000000000000000 ) ) ;
#24650 = DIRECTION ( 'NONE',  ( 0.000000000000000000, 0.000000000000000000, 1.000000000000000000 ) ) ;
#24651 = ADVANCED_FACE ( 'NONE', ( #22711 ), #37709, .T. ) ;
#24652 = CARTESIAN_POINT ( 'NONE',  ( 16.40814093676324603, 7.456968003263754419, -11.09922568453594671 ) ) ;
#24653 = EDGE_LOOP ( 'NONE', ( #15175, #14070, #63843 ) ) ;
#24654 = CARTESIAN_POINT ( 'NONE',  ( 22.26659068614895176, 49.72041550158063927, -7.082119434687042414 ) ) ;
#24655 = ORIENTED_EDGE ( 'NONE', *, *, #7958, .T. ) ;
#24656 = EDGE_CURVE ( 'NONE', #92022, #54254, #73906, .T. ) ;
#24657 = CARTESIAN_POINT ( 'NONE',  ( 13.79529636645031943, 50.34541550158064638, -14.16423886937409904 ) ) ;
#24658 = ORIENTED_EDGE ( 'NONE', *, *, #70514, .T. ) ;
#24659 = CARTESIAN_POINT ( 'NONE',  ( 20.88017736071110519, 20.56368534415484106, 2.639326808657452039E-16 ) ) ;
#24660 = CARTESIAN_POINT ( 'NONE',  ( 10.00000000000000178, 65.37363466993042493, 12.81628187352647608 ) ) ;
#24661 = CARTESIAN_POINT ( 'NONE',  ( 12.91533473730993009, 31.60535201082150891, -10.88017736071109987 ) ) ;
#24662 = CARTESIAN_POINT ( 'NONE',  ( 2.791683348922237240, 55.38393115100078745, -7.208316651077763204 ) ) ;
#24663 = CARTESIAN_POINT ( 'NONE',  ( 2.035157376598822676, 37.43868534415484106, -7.964842623401177768 ) ) ;
#24664 = CARTESIAN_POINT ( 'NONE',  ( 17.96484262340118221, 64.93868534415483396, 7.964842623401181321 ) ) ;
#24665 = CARTESIAN_POINT ( 'NONE',  ( 4.559911319644449179, 32.23035201082150536, -9.422509992056141925 ) ) ;
#24667 = ORIENTED_EDGE ( 'NONE', *, *, #51950, .F. ) ;
#24666 = CARTESIAN_POINT ( 'NONE',  ( -0.03932841506543420518, 33.12161441960502373, 6.397827110478944590 ) ) ;
#24668 = AXIS2_PLACEMENT_3D ( 'NONE', #47406, #79392, #32403 ) ;
#24669 = CARTESIAN_POINT ( 'NONE',  ( 2.791683348922240793, 6.633931151000785675, 7.208316651077764092 ) ) ;
#24670 = DIRECTION ( 'NONE',  ( 0.000000000000000000, 0.000000000000000000, -1.000000000000000000 ) ) ;
#24671 = ORIENTED_EDGE ( 'NONE', *, *, #5865, .F. ) ;
#24672 = CARTESIAN_POINT ( 'NONE',  ( 12.63842701281683922, 39.55059781766744464, -9.846743663894590881 ) ) ;
#24673 = CARTESIAN_POINT ( 'NONE',  ( 21.09922568453594849, 46.20696800326376064, 6.408140936763242479 ) ) ;
#24674 = CIRCLE ( 'NONE', #61410, 0.2000000000000000944 ) ;
#24675 = LINE ( 'NONE', #9168, #42727 ) ;
#24676 = VERTEX_POINT ( 'NONE', #83201 ) ;
#24677 = ADVANCED_FACE ( 'NONE', ( #89705 ), #5730, .T. ) ;
#24678 = CARTESIAN_POINT ( 'NONE',  ( 1.472469842513823179, 66.42559781766745175, 4.923371831947296329 ) ) ;
#24679 = CARTESIAN_POINT ( 'NONE',  ( 0.5774900079438590739, 52.64701867748817676, -5.440088680355550821 ) ) ;
#24680 = CARTESIAN_POINT ( 'NONE',  ( 19.84674366389459266, 48.30059781766745175, 2.638427012816836559 ) ) ;
#24681 = CARTESIAN_POINT ( 'NONE',  ( -0.3689425029237881626, 47.42874883491396787, 10.36894250292379027 ) ) ;
#24682 = CARTESIAN_POINT ( 'NONE',  ( 0.1532563361054100626, 60.80059781766744464, -2.638427012816831230 ) ) ;
#24683 = ORIENTED_EDGE ( 'NONE', *, *, #29211, .F. ) ;
#24684 = CARTESIAN_POINT ( 'NONE',  ( 6.880000000000011440, 40.74999999999999289, 4.250000000000000000 ) ) ;
#24685 = CARTESIAN_POINT ( 'NONE',  ( 5.076628168052703671, 16.84226448433411960, 8.527530157486179263 ) ) ;
#24686 = CARTESIAN_POINT ( 'NONE',  ( 10.00000000000000000, 57.87363466993042493, -12.81628187352647608 ) ) ;
#24687 = CARTESIAN_POINT ( 'NONE',  ( 19.84674366389459266, 58.71726448433411605, -2.638427012816827677 ) ) ;
#24689 = ADVANCED_FACE ( 'NONE', ( #51723 ), #46784, .T. ) ;
#24688 = CARTESIAN_POINT ( 'NONE',  ( 20.88017736071110164, 50.35535201082151247, 2.915334737309930979 ) ) ;
#24690 = CARTESIAN_POINT ( 'NONE',  ( 20.24186590665275531, 15.59014588040357374, -6.114288769123077394 ) ) ;
#24691 = ORIENTED_EDGE ( 'NONE', *, *, #64564, .T. ) ;
#24692 = CARTESIAN_POINT ( 'NONE',  ( -2.266590686148945544, 67.22041550158063217, 7.082119434687048631 ) ) ;
#24693 = DIRECTION ( 'NONE',  ( 0.000000000000000000, 0.000000000000000000, 1.000000000000000000 ) ) ;
#24694 = CARTESIAN_POINT ( 'NONE',  ( 0.5774900079438607392, 33.48035201082150536, 5.440088680355550821 ) ) ;
#24696 = CARTESIAN_POINT ( 'NONE',  ( 4.559911319644449179, 63.89701867748817676, 9.422509992056141925 ) ) ;
#24695 = CARTESIAN_POINT ( 'NONE',  ( 19.38216949554541202, 15.99863466993042138, 9.382169495545424454 ) ) ;
#24697 = CARTESIAN_POINT ( 'NONE',  ( 19.42250999205614548, 65.98035201082151957, -5.440088680355545492 ) ) ;
#24698 = EDGE_CURVE ( 'NONE', #36015, #15178, #24402, .T. ) ;
#24699 = CARTESIAN_POINT ( 'NONE',  ( 66.76470751278411342, 40.99999999999997868, -10.00000000000000000 ) ) ;
#24700 = DIRECTION ( 'NONE',  ( 0.000000000000000000, 0.000000000000000000, 1.000000000000000000 ) ) ;
#24702 = FACE_OUTER_BOUND ( 'NONE', #18733, .T. ) ;
#24701 = CARTESIAN_POINT ( 'NONE',  ( 20.88017736071110519, 55.56368534415484817, 2.639326808657452039E-16 ) ) ;
#24703 = CARTESIAN_POINT ( 'NONE',  ( 10.00000000000000000, 39.75893115100078745, -9.846743663894594434 ) ) ;
#24704 = CARTESIAN_POINT ( 'NONE',  ( 0.1532563361054083140, 6.008931151000784787, 1.131784320476157264E-15 ) ) ;
#24705 = CARTESIAN_POINT ( 'NONE',  ( 3.469446951953614189E-15, 28.05374883491396076, 14.16423886937410259 ) ) ;
#24706 = CARTESIAN_POINT ( 'NONE',  ( 19.38216949554541557, 7.248634669930421381, -9.382169495545420901 ) ) ;
#24707 = CARTESIAN_POINT ( 'NONE',  ( 10.00000000000000178, 14.31368534415483929, 10.88017736071110342 ) ) ;
#24708 = CARTESIAN_POINT ( 'NONE',  ( 3.772706337463130544E-18, 0.2999999999999981570, 0.000000000000000000 ) ) ;
#24709 = AXIS2_PLACEMENT_3D ( 'NONE', #55632, #8168, #2165 ) ;
#24710 = CARTESIAN_POINT ( 'NONE',  ( -0.3689425029237881626, 32.42874883491395366, 10.36894250292379027 ) ) ;
#24711 = CARTESIAN_POINT ( 'NONE',  ( 10.00000000000000178, 33.05374883491396787, 14.16423886937410082 ) ) ;
#24712 = CARTESIAN_POINT ( 'NONE',  ( -0.8801773607110991993, 2.855352010821504471, -2.915334737309923874 ) ) ;
#24713 = CARTESIAN_POINT ( 'NONE',  ( 17.20831665107776587, 29.13393115100078390, -7.208316651077762316 ) ) ;
#24714 = CARTESIAN_POINT ( 'NONE',  ( 19.84674366389459266, 13.71726448433411782, -2.638427012816827677 ) ) ;
#24715 = CARTESIAN_POINT ( 'NONE',  ( 10.00000000000000178, 9.313685344154839285, 10.88017736071110342 ) ) ;
#24716 = ORIENTED_EDGE ( 'NONE', *, *, #96222, .T. ) ;
#24717 = CARTESIAN_POINT ( 'NONE',  ( 0.1532563361054100626, 35.80059781766745175, -2.638427012816831230 ) ) ;
#24718 = CARTESIAN_POINT ( 'NONE',  ( 19.42250999205614548, 45.98035201082150536, -5.440088680355545492 ) ) ;
#24719 = CARTESIAN_POINT ( 'NONE',  ( 1.472469842513823179, 56.42559781766745886, 4.923371831947296329 ) ) ;
#24721 = CARTESIAN_POINT ( 'NONE',  ( 2.603489959281614308, 61.58210964143329846, 6.500000000000031086 ) ) ;
#24720 = CARTESIAN_POINT ( 'NONE',  ( 24.16423886937410614, 24.51208216824730002, -3.795296366450302550 ) ) ;
#24722 = CARTESIAN_POINT ( 'NONE',  ( -0.2838433074297238012, 13.12729635533385597, 10.00000000000000000 ) ) ;
#24723 = CARTESIAN_POINT ( 'NONE',  ( 17.20831665107776587, 14.13393115100078568, -7.208316651077762316 ) ) ;
#24724 = CARTESIAN_POINT ( 'NONE',  ( 16.40814093676323893, 50.79030133659708923, 11.09922568453595026 ) ) ;
#24725 = CARTESIAN_POINT ( 'NONE',  ( 19.84674366389459266, 58.71726448433411605, -2.638427012816827677 ) ) ;
#24726 = ORIENTED_EDGE ( 'NONE', *, *, #71380, .T. ) ;
#24727 = CARTESIAN_POINT ( 'NONE',  ( -0.8801773607110991993, 2.855352010821504471, -2.915334737309923874 ) ) ;
#24728 = CARTESIAN_POINT ( 'NONE',  ( 6.204703633549690345, 15.76208216824730179, -14.16423886937410259 ) ) ;
#24729 = CARTESIAN_POINT ( 'NONE',  ( 0.5774900079438590739, 62.64701867748817676, -5.440088680355550821 ) ) ;
#24730 = CARTESIAN_POINT ( 'NONE',  ( 18.52753015748617571, 43.09226448433412315, 4.923371831947298993 ) ) ;
#24731 = CARTESIAN_POINT ( 'NONE',  ( 10.00000000000000000, 16.81368534415483751, -10.88017736071110342 ) ) ;
#24732 = CARTESIAN_POINT ( 'NONE',  ( -7.618303901328417282, 15.00000000000000711, -12.48478900416272275 ) ) ;
#24733 = CARTESIAN_POINT ( 'NONE',  ( 2.791683348922237240, 60.38393115100078745, -7.208316651077763204 ) ) ;
#24734 = EDGE_CURVE ( 'NONE', #19346, #67870, #27581, .T. ) ;
#24735 = CARTESIAN_POINT ( 'NONE',  ( 1.472469842513823179, 0.5922644843341181575, -4.923371831947296329 ) ) ;
#24736 = CARTESIAN_POINT ( 'NONE',  ( 22.81628187352647785, 56.62363466993042493, 6.195893100308588602E-16 ) ) ;
#24737 = ORIENTED_EDGE ( 'NONE', *, *, #95076, .T. ) ;
#24738 = EDGE_LOOP ( 'NONE', ( #4412, #11525, #52571, #10358 ) ) ;
#24739 = CARTESIAN_POINT ( 'NONE',  ( -14.47650479471817242, 15.00000000000000000, -3.928206833722204028 ) ) ;
#24740 = CARTESIAN_POINT ( 'NONE',  ( 19.72487221294570858, 41.86607318730076344, 6.500000000000000888 ) ) ;
#24741 =( NAMED_UNIT ( * ) SI_UNIT ( $, .STERADIAN. ) SOLID_ANGLE_UNIT ( ) );
#24742 = CARTESIAN_POINT ( 'NONE',  ( 17.08211943468705130, 48.47041550158063927, 12.26659068614894998 ) ) ;
#24743 = CARTESIAN_POINT ( 'NONE',  ( 7.361572987183169658, 49.96726448433410894, -9.846743663894592657 ) ) ;
#24744 = CARTESIAN_POINT ( 'NONE',  ( 12.63842701281683922, 24.55059781766745175, -9.846743663894590881 ) ) ;
#24745 = CARTESIAN_POINT ( 'NONE',  ( -0.7375392941519102186, 14.49999999999999112, 14.98185688723476616 ) ) ;
#24747 = CARTESIAN_POINT ( 'NONE',  ( 19.84674366389459621, 48.50893115100078745, 7.409399052514197653E-17 ) ) ;
#24746 = CARTESIAN_POINT ( 'NONE',  ( 12.91533473730992121, 19.52201867748816611, 10.88017736071110164 ) ) ;
#24748 = PLANE ( 'NONE',  #34234 ) ;
#24749 = ADVANCED_FACE ( 'NONE', ( #45693 ), #52696, .T. ) ;
#24750 = CARTESIAN_POINT ( 'NONE',  ( 17.08211943468705130, 43.47041550158063927, 12.26659068614894998 ) ) ;
#24751 = AXIS2_PLACEMENT_3D ( 'NONE', #55736, #9736, #64674 ) ;
#24752 = CARTESIAN_POINT ( 'NONE',  ( -2.266590686148945544, 57.22041550158063217, 7.082119434687048631 ) ) ;
#24753 = CARTESIAN_POINT ( 'NONE',  ( -18.89999999999999147, 99.74999999999998579, -7.750000000000000000 ) ) ;
#24754 = CARTESIAN_POINT ( 'NONE',  ( 17.81748129626868504, 78.53842255729946942, 4.009548935143046222 ) ) ;
#24755 = CARTESIAN_POINT ( 'NONE',  ( 2.035157376598822676, 67.43868534415484817, -7.964842623401177768 ) ) ;
#24756 = CARTESIAN_POINT ( 'NONE',  ( 10.00000000000000178, 22.25893115100078745, 9.846743663894594434 ) ) ;
#24757 = CARTESIAN_POINT ( 'NONE',  ( -7.371446924914479837, -73.25787537890647627, 4.000000000000000888 ) ) ;
#24758 = ORIENTED_EDGE ( 'NONE', *, *, #67641, .F. ) ;
#24759 = CARTESIAN_POINT ( 'NONE',  ( 1.274849032794164172, 18.57228050351029935, 6.499999999999802824 ) ) ;
#24760 =( BOUNDED_CURVE ( )  B_SPLINE_CURVE ( 2, ( #29952, #68470, #58318, #53444, #10421, #25915, #71894, #56417, #48896 ),
 .UNSPECIFIED., .F., .F. ) 
 B_SPLINE_CURVE_WITH_KNOTS ( ( 3, 2, 2, 2, 3 ),
 ( 0.4739427359034107945, 0.4761904761904761640, 0.4821428571428571508, 0.4880952380952380820, 0.4903429783823025079 ),
 .UNSPECIFIED. ) 
 CURVE ( )  GEOMETRIC_REPRESENTATION_ITEM ( )  RATIONAL_B_SPLINE_CURVE ( ( 0.9839835555609424134, 0.9871328979762477029, 1.000000000000000000, 0.9659258262890683122, 1.000000000000000000, 0.9659258262890683122, 1.000000000000000000, 0.9871328979762533651, 0.9839835555609452999 ) ) 
 REPRESENTATION_ITEM ( '' )  );
#24761 = VERTEX_POINT ( 'NONE', #98733 ) ;
#24762 = CARTESIAN_POINT ( 'NONE',  ( 1.472469842513823179, 15.59226448433411960, -4.923371831947296329 ) ) ;
#24763 = EDGE_LOOP ( 'NONE', ( #29788, #38942 ) ) ;
#24764 = CARTESIAN_POINT ( 'NONE',  ( -4.164238869374099927, 17.01208216824730357, 3.795296366450308767 ) ) ;
#24765 = CARTESIAN_POINT ( 'NONE',  ( 19.84674366389459266, 23.30059781766745530, 2.638427012816836559 ) ) ;
#24766 = CARTESIAN_POINT ( 'NONE',  ( -0.8801773607110991993, 47.85535201082150536, -2.915334737309923874 ) ) ;
#24767 = DIRECTION ( 'NONE',  ( 0.000000000000000000, 0.000000000000000000, 1.000000000000000000 ) ) ;
#24768 = VERTEX_POINT ( 'NONE', #14220 ) ;
#24769 = CARTESIAN_POINT ( 'NONE',  ( 20.88017736071110875, 45.77201867748816966, -2.915334737309920765 ) ) ;
#24770 = CYLINDRICAL_SURFACE ( 'NONE', #544, 15.00000000000000000 ) ;
#24771 = CIRCLE ( 'NONE', #90187, 0.2500000000000002220 ) ;
#24772 = EDGE_CURVE ( 'NONE', #6306, #20656, #36217, .T. ) ;
#24773 = CARTESIAN_POINT ( 'NONE',  ( 9.382169495545419124, 0.9986346699304144980, 9.382169495545417348 ) ) ;
#24774 = VERTEX_POINT ( 'NONE', #91185 ) ;
#24775 = CARTESIAN_POINT ( 'NONE',  ( 12.91533473730993009, 41.60535201082149825, -10.88017736071109987 ) ) ;
#24776 = CARTESIAN_POINT ( 'NONE',  ( 24.16423886937410614, 4.303748834913967869, 8.672049930838204340E-16 ) ) ;
#24777 = EDGE_CURVE ( 'NONE', #89183, #89322, #78701, .T. ) ;
#24778 = ORIENTED_EDGE ( 'NONE', *, *, #10327, .F. ) ;
#24779 = CARTESIAN_POINT ( 'NONE',  ( 16.40814093676323893, 30.79030133659708923, 11.09922568453595026 ) ) ;
#24780 = CARTESIAN_POINT ( 'NONE',  ( -4.164238869374098151, 1.595415501580634388, -3.795296366450310543 ) ) ;
#24781 = CARTESIAN_POINT ( 'NONE',  ( 19.84674366389459621, 13.50893115100078568, 7.409399052514197653E-17 ) ) ;
#24782 = CARTESIAN_POINT ( 'NONE',  ( 14.64921366071500053, 0.04962891916449693047, -1.748670679918162163 ) ) ;
#24783 = CARTESIAN_POINT ( 'NONE',  ( -1.099225684535947600, 44.54030133659708923, 6.408140936763237150 ) ) ;
#24784 = CARTESIAN_POINT ( 'NONE',  ( -8.900000000000000355, 75.73428692542562146, -3.000000000000000000 ) ) ;
#24785 = CARTESIAN_POINT ( 'NONE',  ( 2.791683348922237240, 10.38393115100078390, -7.208316651077763204 ) ) ;
#24786 = CARTESIAN_POINT ( 'NONE',  ( 7.084665262690076126, 42.02201867748816966, -10.88017736071110164 ) ) ;
#24787 = AXIS2_PLACEMENT_3D ( 'NONE', #40801, #93296, #2330 ) ;
#24788 = VERTEX_POINT ( 'NONE', #13715 ) ;
#24789 = ORIENTED_EDGE ( 'NONE', *, *, #75730, .T. ) ;
#24790 = CARTESIAN_POINT ( 'NONE',  ( 20.32896413005680358, 64.74545670184114954, 5.963430220938287007 ) ) ;
#24791 = CARTESIAN_POINT ( 'NONE',  ( 0.5774900079438590739, 52.64701867748817676, -5.440088680355550821 ) ) ;
#24792 = CARTESIAN_POINT ( 'NONE',  ( -42.84429281707037518, 107.5921494319837706, 4.500000000000002665 ) ) ;
#24793 = CARTESIAN_POINT ( 'NONE',  ( 13.99999999999999822, 61.00000000000000711, -6.000000000000000000 ) ) ;
#24794 = CARTESIAN_POINT ( 'NONE',  ( 12.91533473730993009, 61.60535201082150536, -10.88017736071109987 ) ) ;
#24795 = CARTESIAN_POINT ( 'NONE',  ( 10.00000000000000178, 10.37363466993041961, 12.81628187352647608 ) ) ;
#24796 = CARTESIAN_POINT ( 'NONE',  ( -23.44000000000001194, 92.00000000000000000, -9.500000000000000000 ) ) ;
#24797 = CARTESIAN_POINT ( 'NONE',  ( 1.472469842513823179, 31.42559781766745530, 4.923371831947296329 ) ) ;
#24798 = FACE_OUTER_BOUND ( 'NONE', #37428, .T. ) ;
#24799 = CARTESIAN_POINT ( 'NONE',  ( -4.164238869374099039, 6.803748834913967869, 8.674139862899312516E-16 ) ) ;
#24800 = CARTESIAN_POINT ( 'NONE',  ( 5.076628168052704559, 20.17559781766745175, -8.527530157486179263 ) ) ;
#24802 = CIRCLE ( 'NONE', #19999, 0.2500000000000002220 ) ;
#24801 = CARTESIAN_POINT ( 'NONE',  ( 16.40814093676323893, 15.79030133659708746, 11.09922568453595026 ) ) ;
#24803 = CARTESIAN_POINT ( 'NONE',  ( 0.2751277870542981341, 18.21833443783937767, 6.500000000000002665 ) ) ;
#24804 = CARTESIAN_POINT ( 'NONE',  ( 2.035157376598824452, 48.68868534415483396, 7.964842623401179544 ) ) ;
#24805 = CARTESIAN_POINT ( 'NONE',  ( 10.00000000000000000, -2.126365330069579951, -12.81628187352647608 ) ) ;
#24806 = CARTESIAN_POINT ( 'NONE',  ( -0.3289641300568009741, 32.24545670184113533, -5.963430220938281678 ) ) ;
#24807 = CARTESIAN_POINT ( 'NONE',  ( 7.361572987183169658, 34.96726448433411605, -9.846743663894592657 ) ) ;
#24808 = CARTESIAN_POINT ( 'NONE',  ( 18.52753015748617571, 23.09226448433411960, 4.923371831947298993 ) ) ;
#24810 = EDGE_CURVE ( 'NONE', #59012, #26974, #67213, .T. ) ;
#24809 = CARTESIAN_POINT ( 'NONE',  ( 0.5774900079438607392, 18.48035201082150536, 5.440088680355550821 ) ) ;
#24811 = CARTESIAN_POINT ( 'NONE',  ( 6.565887622018943937, 10.16530133659708746, 12.81628187352647430 ) ) ;
#24812 = CARTESIAN_POINT ( 'NONE',  ( 12.63842701281683034, 22.46726448433411605, 9.846743663894596210 ) ) ;
#24813 = DIRECTION ( 'NONE',  ( 1.000000000000000000, 0.000000000000000000, 0.000000000000000000 ) ) ;
#24814 = CARTESIAN_POINT ( 'NONE',  ( 17.96484262340118221, 16.18868534415483396, -7.964842623401177768 ) ) ;
#24815 = VERTEX_POINT ( 'NONE', #76192 ) ;
#24816 = CARTESIAN_POINT ( 'NONE',  ( 4.559911319644449179, 67.23035201082150536, -9.422509992056141925 ) ) ;
#24817 = SURFACE_STYLE_USAGE ( .BOTH. , #84817 ) ;
#24819 = CARTESIAN_POINT ( 'NONE',  ( 15.44008868035555793, 11.39701867748817143, -9.422509992056140149 ) ) ;
#24818 = CARTESIAN_POINT ( 'NONE',  ( 10.00000000000000178, 42.25893115100078745, 9.846743663894594434 ) ) ;
#24820 = DIRECTION ( 'NONE',  ( 0.000000000000000000, 1.000000000000000000, -0.000000000000000000 ) ) ;
#24821 = CARTESIAN_POINT ( 'NONE',  ( 15.44008868035555793, 51.39701867748816966, -9.422509992056140149 ) ) ;
#24823 = FILL_AREA_STYLE_COLOUR ( '', #9572 ) ;
#24822 = CARTESIAN_POINT ( 'NONE',  ( 12.91533473730992121, 14.52201867748817143, 10.88017736071110164 ) ) ;
#24824 = CARTESIAN_POINT ( 'NONE',  ( 7.361572987183169658, 14.96726448433411960, -9.846743663894592657 ) ) ;
#24825 = CARTESIAN_POINT ( 'NONE',  ( 19.84674366389459621, 38.50893115100078745, 7.409399052514197653E-17 ) ) ;
#24826 = DIRECTION ( 'NONE',  ( 0.06975647374412512203, 0.9975640502598241977, 0.000000000000000000 ) ) ;
#24827 = PLANE ( 'NONE',  #41712 ) ;
#24828 = CARTESIAN_POINT ( 'NONE',  ( 0.6178305044545818747, -1.501365330069579951, -9.382169495545419124 ) ) ;
#24829 = CARTESIAN_POINT ( 'NONE',  ( -2.266590686148945544, 2.220415501580634388, 7.082119434687048631 ) ) ;
#24830 = CARTESIAN_POINT ( 'NONE',  ( 20.36894250292379382, 23.67874883491397142, 10.36894250292379205 ) ) ;
#24831 = CARTESIAN_POINT ( 'NONE',  ( 14.92337183194729988, 39.34226448433412315, -8.527530157486177487 ) ) ;
#24832 = VECTOR ( 'NONE', #71204, 1000.000000000000000 ) ;
#24833 = CARTESIAN_POINT ( 'NONE',  ( 2.917880565312950480, 55.97041550158063217, -12.26659068614894821 ) ) ;
#24834 = CARTESIAN_POINT ( 'NONE',  ( 5.076628168052704559, 20.17559781766745175, -8.527530157486179263 ) ) ;
#24835 = CARTESIAN_POINT ( 'NONE',  ( -8.211425130294045971, 85.75922772022539675, -4.168580035010579721 ) ) ;
#24836 = CARTESIAN_POINT ( 'NONE',  ( 20.88017736071110164, 40.35535201082150536, 2.915334737309930979 ) ) ;
#24837 = DIRECTION ( 'NONE',  ( 0.000000000000000000, 0.000000000000000000, -1.000000000000000000 ) ) ;
#24838 = CARTESIAN_POINT ( 'NONE',  ( 12.91533473730993009, 21.60535201082150536, -10.88017736071109987 ) ) ;
#24839 = CARTESIAN_POINT ( 'NONE',  ( 0.6178305044545838731, 54.74863466993042493, 9.382169495545420901 ) ) ;
#24840 = CARTESIAN_POINT ( 'NONE',  ( 10.00000000000000000, 17.87363466993041783, -12.81628187352647608 ) ) ;
#24841 = CARTESIAN_POINT ( 'NONE',  ( 19.72487221294570148, 35.71833443783938833, -6.500000000000010658 ) ) ;
#24842 = CARTESIAN_POINT ( 'NONE',  ( 2.791683348922237240, 10.38393115100078390, -7.208316651077763204 ) ) ;
#24843 = ORIENTED_EDGE ( 'NONE', *, *, #1855, .F. ) ;
#24844 = DIRECTION ( 'NONE',  ( -2.569960705150826877E-16, 1.000000000000000000, 0.000000000000000000 ) ) ;
#24845 = LINE ( 'NONE', #18813, #60389 ) ;
#24846 = CARTESIAN_POINT ( 'NONE',  ( 24.16423886937409904, 49.09541550158063217, 3.795296366450317205 ) ) ;
#24847 = CARTESIAN_POINT ( 'NONE',  ( 24.16423886937410614, 29.51208216824729647, -3.795296366450302550 ) ) ;
#24848 = CARTESIAN_POINT ( 'NONE',  ( 2.035157376598822676, 17.43868534415483751, -7.964842623401177768 ) ) ;
#24849 = CARTESIAN_POINT ( 'NONE',  ( 20.88017736071110164, 55.35535201082149825, 2.915334737309930979 ) ) ;
#24850 = DIRECTION ( 'NONE',  ( 0.000000000000000000, -1.000000000000000000, 0.000000000000000000 ) ) ;
#24851 = DIRECTION ( 'NONE',  ( -1.000000000000000000, -0.000000000000000000, -0.000000000000000000 ) ) ;
#24852 = CARTESIAN_POINT ( 'NONE',  ( 10.00000000000000178, 64.31368534415483396, 10.88017736071110342 ) ) ;
#24853 = CARTESIAN_POINT ( 'NONE',  ( 19.84674366389459266, 13.71726448433411782, -2.638427012816827677 ) ) ;
#24854 = FACE_OUTER_BOUND ( 'NONE', #26124, .T. ) ;
#24855 = CARTESIAN_POINT ( 'NONE',  ( -1.983216688680738082, 15.00000000000000000, -14.11131997956740491 ) ) ;
#24856 = CARTESIAN_POINT ( 'NONE',  ( 17.20831665107776587, 27.88393115100078390, 7.208316651077764980 ) ) ;
#24857 = CARTESIAN_POINT ( 'NONE',  ( 19.84674366389459621, 48.50893115100078745, 7.409399052514197653E-17 ) ) ;
#24858 = B_SPLINE_CURVE_WITH_KNOTS ( 'NONE', 3,
 ( #91056, #60564, #45061, #36595, #52567, #8068, #59076, #66588, #29557, #38081 ),
 .UNSPECIFIED., .F., .F.,
 ( 4, 2, 2, 2, 4 ),
 ( 0.009575373339651055415, 0.01007433173322977958, 0.01057329012680850548, 0.01157120691396595381, 0.01356704048828087997 ),
 .UNSPECIFIED. ) ;
#24859 = STYLED_ITEM ( 'NONE', ( #30696 ), #53984 ) ;
#24860 = CARTESIAN_POINT ( 'NONE',  ( 17.96484262340118221, 16.18868534415483396, -7.964842623401177768 ) ) ;
#24861 = CARTESIAN_POINT ( 'NONE',  ( 22.81628187352647785, 31.62363466993042138, 6.195893100308588602E-16 ) ) ;
#24862 = AXIS2_PLACEMENT_3D ( 'NONE', #43263, #12273, #27766 ) ;
#24863 = CARTESIAN_POINT ( 'NONE',  ( 20.88017736071110519, 55.56368534415484817, 2.639326808657452039E-16 ) ) ;
#24865 = CARTESIAN_POINT ( 'NONE',  ( 14.92337183194729633, 12.67559781766745353, 8.527530157486181039 ) ) ;
#24864 = CARTESIAN_POINT ( 'NONE',  ( 13.79529636645031943, 40.34541550158063217, -14.16423886937409904 ) ) ;
#24867 = EDGE_CURVE ( 'NONE', #49115, #95793, #97865, .T. ) ;
#24866 = PLANE ( 'NONE',  #51975 ) ;
#24868 = EDGE_CURVE ( 'NONE', #7152, #21334, #85126, .T. ) ;
#24869 = CARTESIAN_POINT ( 'NONE',  ( 18.52753015748618282, 48.92559781766745886, -4.923371831947291888 ) ) ;
#24871 = CARTESIAN_POINT ( 'NONE',  ( 10.00000000000000000, 5.553748834913967869, -14.16423886937410082 ) ) ;
#24870 = CARTESIAN_POINT ( 'NONE',  ( 10.00000000000000178, 27.25893115100078390, 9.846743663894594434 ) ) ;
#24872 = CARTESIAN_POINT ( 'NONE',  ( -0.3689425029237898834, 21.17874883491396432, -10.36894250292378850 ) ) ;
#24873 = CARTESIAN_POINT ( 'NONE',  ( 17.20831665107776587, 29.13393115100078390, -7.208316651077762316 ) ) ;
#24874 = CARTESIAN_POINT ( 'NONE',  ( -0.8801773607110991993, 42.85535201082150536, -2.915334737309923874 ) ) ;
#24875 = CARTESIAN_POINT ( 'NONE',  ( 12.91533473730993009, 16.60535201082150891, -10.88017736071109987 ) ) ;
#24876 = CARTESIAN_POINT ( 'NONE',  ( 2.035157376598822676, 42.43868534415483396, -7.964842623401177768 ) ) ;
#24877 = CARTESIAN_POINT ( 'NONE',  ( 10.00000000000000178, 24.31368534415484106, 10.88017736071110342 ) ) ;
#24878 = ORIENTED_EDGE ( 'NONE', *, *, #50729, .F. ) ;
#24879 = B_SPLINE_CURVE_WITH_KNOTS ( 'NONE', 3,
 ( #30907, #31394, #61403, #61894 ),
 .UNSPECIFIED., .F., .F.,
 ( 4, 4 ),
 ( 0.000000000000000000, 0.002657014572711312479 ),
 .UNSPECIFIED. ) ;
#24880 = CARTESIAN_POINT ( 'NONE',  ( 10.00000000000000000, 41.81368534415484106, -10.88017736071110342 ) ) ;
#24881 = ORIENTED_EDGE ( 'NONE', *, *, #7250, .F. ) ;
#24882 = CARTESIAN_POINT ( 'NONE',  ( 19.38216949554541557, 57.24863466993042493, -9.382169495545420901 ) ) ;
#24883 = LINE ( 'NONE', #55368, #68063 ) ;
#24884 = AXIS2_PLACEMENT_3D ( 'NONE', #41108, #18590, #79586 ) ;
#24885 = ORIENTED_EDGE ( 'NONE', *, *, #33522, .T. ) ;
#24886 = CARTESIAN_POINT ( 'NONE',  ( 17.96484262340118221, 46.18868534415484106, -7.964842623401177768 ) ) ;
#24887 = CARTESIAN_POINT ( 'NONE',  ( 7.084665262690076126, 4.105352010821503583, 10.88017736071109987 ) ) ;
#24888 = VECTOR ( 'NONE', #11885, 1000.000000000000000 ) ;
#24889 = B_SPLINE_CURVE_WITH_KNOTS ( 'NONE', 3,
 ( #27605, #13099, #36093, #67093, #20107, #66599, #43595, #82087, #35605, #50610, #52092, #74587, #82586, #67597, #483, #81588, #36606, #30931, #21606, #81102 ),
 .UNSPECIFIED., .F., .F.,
 ( 4, 2, 2, 2, 2, 2, 2, 2, 2, 4 ),
 ( 0.000000000000000000, 0.003408369840167499009, 0.004260462300209373436, 0.005112554760251249164, 0.006816739680334997151, 0.008520924600418745137, 0.01022510952050249486, 0.01107720198054436972, 0.01192929444058624285, 0.01363347936066999083 ),
 .UNSPECIFIED. ) ;
#24890 = DIRECTION ( 'NONE',  ( 0.7808688094430307203, -0.6246950475544238435, 0.000000000000000000 ) ) ;
#24891 = DIRECTION ( 'NONE',  ( 0.000000000000000000, 0.000000000000000000, 1.000000000000000000 ) ) ;
#24892 = CARTESIAN_POINT ( 'NONE',  ( 20.36894250292379738, 64.92874883491397497, -10.36894250292379027 ) ) ;
#24893 = CARTESIAN_POINT ( 'NONE',  ( 10.00000000000000178, 2.258931151000784787, 9.846743663894594434 ) ) ;
#24894 = MECHANICAL_DESIGN_GEOMETRIC_PRESENTATION_REPRESENTATION (  '', ( #98345 ), #32859 ) ;
#24895 = CARTESIAN_POINT ( 'NONE',  ( 0.1532563361054082862, 6.217264484334118713, 2.638427012816831674 ) ) ;
#24896 = CARTESIAN_POINT ( 'NONE',  ( 20.88017736071110164, 5.355352010821502695, 2.915334737309930979 ) ) ;
#24897 = CARTESIAN_POINT ( 'NONE',  ( 0.1532563361054083140, 46.00893115100079456, 1.131784320476157264E-15 ) ) ;
#24898 = ORIENTED_EDGE ( 'NONE', *, *, #32433, .F. ) ;
#24899 = EDGE_CURVE ( 'NONE', #53155, #78868, #90195, .T. ) ;
#24900 = CARTESIAN_POINT ( 'NONE',  ( 17.20831665107776587, 44.13393115100078745, -7.208316651077762316 ) ) ;
#24901 = DIRECTION ( 'NONE',  ( 1.000000000000000000, 0.000000000000000000, 0.000000000000000000 ) ) ;
#24902 = CARTESIAN_POINT ( 'NONE',  ( 0.5774900079438607392, 43.48035201082151247, 5.440088680355550821 ) ) ;
#24903 = CARTESIAN_POINT ( 'NONE',  ( 10.00000000000000000, 54.75893115100078745, -9.846743663894594434 ) ) ;
#24904 = CARTESIAN_POINT ( 'NONE',  ( 0.6178305044545838731, 29.74863466993042138, 9.382169495545420901 ) ) ;
#24905 = CARTESIAN_POINT ( 'NONE',  ( 10.00000000000000178, 69.31368534415484817, 10.88017736071110342 ) ) ;
#24906 = CARTESIAN_POINT ( 'NONE',  ( 2.035157376598824452, 48.68868534415483396, 7.964842623401179544 ) ) ;
#24907 = CARTESIAN_POINT ( 'NONE',  ( 22.26659068614895176, 59.72041550158063927, -7.082119434687042414 ) ) ;
#24908 = CIRCLE ( 'NONE', #71147, 14.49999999999999822 ) ;
#24909 = CARTESIAN_POINT ( 'NONE',  ( 22.81628187352648496, 21.83196800326374643, -3.434112377981050290 ) ) ;
#24910 = CARTESIAN_POINT ( 'NONE',  ( 0.4195498155886414615, 0.4999999999999994449, 9.500000000000000000 ) ) ;
#24911 = ORIENTED_EDGE ( 'NONE', *, *, #45781, .F. ) ;
#24912 = CARTESIAN_POINT ( 'NONE',  ( 19.38216949554541557, 27.24863466993041783, -9.382169495545420901 ) ) ;
#24913 = CARTESIAN_POINT ( 'NONE',  ( 2.035157376598822676, 17.43868534415483751, -7.964842623401177768 ) ) ;
#24914 = EDGE_LOOP ( 'NONE', ( #88920, #5817, #96087, #17148 ) ) ;
#24915 = VERTEX_POINT ( 'NONE', #60196 ) ;
#24916 = CARTESIAN_POINT ( 'NONE',  ( 7.361572987183169658, -0.03273551566588185635, -9.846743663894592657 ) ) ;
#24917 = CARTESIAN_POINT ( 'NONE',  ( 17.20831665107776587, 52.88393115100078035, 7.208316651077764980 ) ) ;
#24919 = CARTESIAN_POINT ( 'NONE',  ( 17.20831665107776587, 34.13393115100078745, -7.208316651077762316 ) ) ;
#24918 = CARTESIAN_POINT ( 'NONE',  ( 2.791683348922240793, 16.63393115100078745, 7.208316651077764092 ) ) ;
#24920 = CARTESIAN_POINT ( 'NONE',  ( -11.26270400852059872, -93.44583868494822809, 3.750000000000001776 ) ) ;
#24921 = FACE_OUTER_BOUND ( 'NONE', #26449, .T. ) ;
#24922 = CARTESIAN_POINT ( 'NONE',  ( 7.361572987183169658, 24.96726448433412315, -9.846743663894592657 ) ) ;
#24923 = CARTESIAN_POINT ( 'NONE',  ( 18.72515096720577787, 46.07228050351031357, -6.499999999999891642 ) ) ;
#24924 = MECHANICAL_DESIGN_GEOMETRIC_PRESENTATION_REPRESENTATION (  '', ( #98462 ), #50457 ) ;
#24925 = DIRECTION ( 'NONE',  ( 0.000000000000000000, 0.000000000000000000, -1.000000000000000000 ) ) ;
#24927 = CARTESIAN_POINT ( 'NONE',  ( 5.076628168052704559, 0.1755978176674514724, -8.527530157486179263 ) ) ;
#24926 = CARTESIAN_POINT ( 'NONE',  ( 14.92337183194729633, 22.67559781766745175, 8.527530157486181039 ) ) ;
#24928 =( NAMED_UNIT ( * ) PLANE_ANGLE_UNIT ( ) SI_UNIT ( $, .RADIAN. ) );
#24930 = ORIENTED_EDGE ( 'NONE', *, *, #37641, .T. ) ;
#24929 = CARTESIAN_POINT ( 'NONE',  ( 17.20831665107776587, 49.13393115100078745, -7.208316651077762316 ) ) ;
#24931 = CARTESIAN_POINT ( 'NONE',  ( -7.598395483715266452E-32, -2.710505431213761085E-16, 0.000000000000000000 ) ) ;
#24932 = CARTESIAN_POINT ( 'NONE',  ( 19.38216949554541202, 25.99863466993042138, 9.382169495545424454 ) ) ;
#24933 = LINE ( 'NONE', #86413, #98416 ) ;
#24934 = CARTESIAN_POINT ( 'NONE',  ( 10.00000000000000000, 45.55374883491397497, -14.16423886937410082 ) ) ;
#24935 = CARTESIAN_POINT ( 'NONE',  ( 17.20831665107776587, 14.13393115100078568, -7.208316651077762316 ) ) ;
#24936 = CARTESIAN_POINT ( 'NONE',  ( 10.00000000000000000, 4.758931151000784787, -9.846743663894594434 ) ) ;
#24937 = CARTESIAN_POINT ( 'NONE',  ( 19.64201483648647439, 93.04323334508872279, 5.303713241053674921 ) ) ;
#24938 = CARTESIAN_POINT ( 'NONE',  ( 24.16423886937410614, 49.51208216824730357, -3.795296366450302550 ) ) ;
#24939 = CARTESIAN_POINT ( 'NONE',  ( 18.52753015748618282, 53.92559781766745175, -4.923371831947291888 ) ) ;
#24940 = CARTESIAN_POINT ( 'NONE',  ( 10.00000000000000178, 63.05374883491396076, 14.16423886937410082 ) ) ;
#24941 = CARTESIAN_POINT ( 'NONE',  ( 13.79529636645031943, 25.34541550158063572, -14.16423886937409904 ) ) ;
#24942 = CARTESIAN_POINT ( 'NONE',  ( 20.36894250292379382, 38.67874883491396076, 10.36894250292379205 ) ) ;
#24943 = DIRECTION ( 'NONE',  ( -1.000000000000000000, 0.000000000000000000, 0.000000000000000000 ) ) ;
#24945 = CARTESIAN_POINT ( 'NONE',  ( 5.076628168052703671, 56.84226448433412315, 8.527530157486179263 ) ) ;
#24944 = CARTESIAN_POINT ( 'NONE',  ( 6.574584770571507697, -50.88238473864101508, 2.750000000000000444 ) ) ;
#24946 = ORIENTED_EDGE ( 'NONE', *, *, #23888, .T. ) ;
#24947 = CARTESIAN_POINT ( 'NONE',  ( 4.559911319644449179, 33.89701867748817676, 9.422509992056141925 ) ) ;
#24948 = DIRECTION ( 'NONE',  ( 0.000000000000000000, 0.000000000000000000, -1.000000000000000000 ) ) ;
#24949 = EDGE_CURVE ( 'NONE', #46764, #97225, #22219, .T. ) ;
#24950 = FACE_OUTER_BOUND ( 'NONE', #31019, .T. ) ;
#24951 = CARTESIAN_POINT ( 'NONE',  ( 7.361572987183169658, 39.96726448433411605, -9.846743663894592657 ) ) ;
#24952 = CARTESIAN_POINT ( 'NONE',  ( -1.899999999999997247, 98.49999999999998579, -8.525133428036873795 ) ) ;
#24953 = CARTESIAN_POINT ( 'NONE',  ( 14.16423886937410437, -5.904584498419365168, 3.795296366450304770 ) ) ;
#24954 = CARTESIAN_POINT ( 'NONE',  ( 18.52753015748618282, 43.92559781766745175, -4.923371831947291888 ) ) ;
#24955 = DIRECTION ( 'NONE',  ( 0.9366721892483971246, 0.000000000000000000, 0.3502073812594687086 ) ) ;
#24956 = VECTOR ( 'NONE', #13358, 1000.000000000000000 ) ;
#24957 = AXIS2_PLACEMENT_3D ( 'NONE', #90656, #14690, #30637 ) ;
#24958 = ORIENTED_EDGE ( 'NONE', *, *, #1701, .T. ) ;
#24959 = CARTESIAN_POINT ( 'NONE',  ( 13.79529636645031943, 15.34541550158063750, -14.16423886937409904 ) ) ;
#24960 = AXIS2_PLACEMENT_3D ( 'NONE', #26936, #80441, #33926 ) ;
#24961 = DIRECTION ( 'NONE',  ( -0.000000000000000000, -0.000000000000000000, 1.000000000000000000 ) ) ;
#24963 = FACE_OUTER_BOUND ( 'NONE', #90079, .T. ) ;
#24962 = SURFACE_SIDE_STYLE ('',( #83974 ) ) ;
#24964 = CARTESIAN_POINT ( 'NONE',  ( 20.88017736071110875, 5.772018677488170546, -2.915334737309920765 ) ) ;
#24965 = CARTESIAN_POINT ( 'NONE',  ( 6.565887622018943937, 25.16530133659708213, 12.81628187352647430 ) ) ;
#24966 = CARTESIAN_POINT ( 'NONE',  ( 20.15039907845753930, 2.627771745786128044, -6.262539305110069954 ) ) ;
#24967 = CARTESIAN_POINT ( 'NONE',  ( -0.8801773607111008646, 63.27201867748817676, 2.915334737309923430 ) ) ;
#24968 =( NAMED_UNIT ( * ) PLANE_ANGLE_UNIT ( ) SI_UNIT ( $, .RADIAN. ) );
#24969 = CARTESIAN_POINT ( 'NONE',  ( -46.82586484710777341, 100.5857744218339036, -9.343464521776596143 ) ) ;
#24970 = CARTESIAN_POINT ( 'NONE',  ( 14.47650479471820262, 0.3640475087720640990, 3.928206833722112989 ) ) ;
#24971 = CARTESIAN_POINT ( 'NONE',  ( -0.3689425029237898834, 56.17874883491396076, -10.36894250292378850 ) ) ;
#24972 = DIRECTION ( 'NONE',  ( -0.000000000000000000, -1.000000000000000000, -0.000000000000000000 ) ) ;
#24973 = CARTESIAN_POINT ( 'NONE',  ( 2.035157376598824452, 23.68868534415484461, 7.964842623401179544 ) ) ;
#24974 = CARTESIAN_POINT ( 'NONE',  ( 17.96484262340118221, 36.18868534415484106, -7.964842623401177768 ) ) ;
#24975 = CARTESIAN_POINT ( 'NONE',  ( 0.6178305044545818747, -1.501365330069579951, -9.382169495545419124 ) ) ;
#24976 = CARTESIAN_POINT ( 'NONE',  ( 10.00000000000000000, 49.75893115100078745, -9.846743663894594434 ) ) ;
#24977 = CARTESIAN_POINT ( 'NONE',  ( 0.6178305044545818747, 63.49863466993043204, -9.382169495545419124 ) ) ;
#24978 = CARTESIAN_POINT ( 'NONE',  ( 1.042145700049420309, 54.74216108172002748, -6.499999999999917399 ) ) ;
#24979 = ADVANCED_FACE ( 'NONE', ( #54654 ), #46193, .T. ) ;
#24980 = ORIENTED_EDGE ( 'NONE', *, *, #40812, .F. ) ;
#24981 = CARTESIAN_POINT ( 'NONE',  ( 17.96484262340118221, 26.18868534415483396, -7.964842623401177768 ) ) ;
#24982 = CARTESIAN_POINT ( 'NONE',  ( 22.81628187352648496, 36.83196800326376064, -3.434112377981050290 ) ) ;
#24983 = AXIS2_PLACEMENT_3D ( 'NONE', #68234, #14743, #62170 ) ;
#24984 = CARTESIAN_POINT ( 'NONE',  ( -0.000000000000000000, 75.65410658971823921, 6.567011432196594889 ) ) ;
#24985 = EDGE_CURVE ( 'NONE', #15093, #96102, #9167, .T. ) ;
#24986 = CARTESIAN_POINT ( 'NONE',  ( 0.6178305044545818747, -1.501365330069579951, -9.382169495545419124 ) ) ;
#24987 = CARTESIAN_POINT ( 'NONE',  ( 12.91533473730992121, 49.52201867748817676, 10.88017736071110164 ) ) ;
#24988 = ADVANCED_FACE ( 'NONE', ( #17179 ), #88244, .T. ) ;
#24989 = CARTESIAN_POINT ( 'NONE',  ( 18.52753015748618282, 8.925597817667451750, -4.923371831947291888 ) ) ;
#24990 = CARTESIAN_POINT ( 'NONE',  ( -2.816281873526473856, 39.33196800326374643, 3.434112377981055619 ) ) ;
#24992 = CARTESIAN_POINT ( 'NONE',  ( -3.499999999999998668, 1.019547802438465434, -2.750000000000000444 ) ) ;
#24991 = CARTESIAN_POINT ( 'NONE',  ( -0.8801773607111009756, 63.06368534415484106, 1.068504757029289695E-15 ) ) ;
#24993 = CARTESIAN_POINT ( 'NONE',  ( 18.06765999051789251, 53.99127512925452521, 6.499999999999959144 ) ) ;
#24994 = CARTESIAN_POINT ( 'NONE',  ( 22.81628187352647785, 61.62363466993041783, 6.195893100308588602E-16 ) ) ;
#24995 = ORIENTED_EDGE ( 'NONE', *, *, #93455, .F. ) ;
#24996 =( NAMED_UNIT ( * ) PLANE_ANGLE_UNIT ( ) SI_UNIT ( $, .RADIAN. ) );
#24997 = FACE_OUTER_BOUND ( 'NONE', #77601, .T. ) ;
#24998 = CARTESIAN_POINT ( 'NONE',  ( 10.00000000000000178, 4.313685344154837509, 10.88017736071110342 ) ) ;
#24999 = CARTESIAN_POINT ( 'NONE',  ( 13.43411237798106583, 42.66530133659707502, -12.81628187352647252 ) ) ;
#25000 = CARTESIAN_POINT ( 'NONE',  ( 19.84674366389459266, 18.30059781766745175, 2.638427012816836559 ) ) ;
#25001 = CARTESIAN_POINT ( 'NONE',  ( 12.91533473730993009, 6.605352010821504471, -10.88017736071109987 ) ) ;
#25002 = CARTESIAN_POINT ( 'NONE',  ( 2.791683348922237240, 20.38393115100078745, -7.208316651077763204 ) ) ;
#25003 = CARTESIAN_POINT ( 'NONE',  ( 2.917880565312948704, 57.63708216824731068, 12.26659068614894643 ) ) ;
#25004 = VERTEX_POINT ( 'NONE', #69676 ) ;
#25005 = CIRCLE ( 'NONE', #48954, 14.49999999999999822 ) ;
#25006 = CARTESIAN_POINT ( 'NONE',  ( 2.035157376598822676, 27.43868534415483396, -7.964842623401177768 ) ) ;
#25007 = CARTESIAN_POINT ( 'NONE',  ( 0.000000000000000000, 70.80332830338373640, 5.000000000000000000 ) ) ;
#25008 = VERTEX_POINT ( 'NONE', #46669 ) ;
#25009 = CARTESIAN_POINT ( 'NONE',  ( 7.084665262690076126, 17.02201867748817676, -10.88017736071110164 ) ) ;
#25010 = CARTESIAN_POINT ( 'NONE',  ( 7.084665262690076126, 17.02201867748817676, -10.88017736071110164 ) ) ;
#25011 = CARTESIAN_POINT ( 'NONE',  ( 10.00000000000000000, 59.75893115100078745, -9.846743663894594434 ) ) ;
#25012 = SURFACE_SIDE_STYLE ('',( #47490 ) ) ;
#25014 = CARTESIAN_POINT ( 'NONE',  ( -4.164238869374099039, 16.80374883491396787, 8.674139862899312516E-16 ) ) ;
#25013 = FACE_OUTER_BOUND ( 'NONE', #1515, .T. ) ;
#25015 = CARTESIAN_POINT ( 'NONE',  ( 20.88017736071110164, 20.35535201082150891, 2.915334737309930979 ) ) ;
#25016 = CARTESIAN_POINT ( 'NONE',  ( 0.5774900079438607392, 23.48035201082150536, 5.440088680355550821 ) ) ;
#25017 = CARTESIAN_POINT ( 'NONE',  ( 17.20831665107776587, 59.13393115100078745, -7.208316651077762316 ) ) ;
#25018 = STYLED_ITEM ( 'NONE', ( #56395 ), #30487 ) ;
#25019 = FACE_OUTER_BOUND ( 'NONE', #20317, .T. ) ;
#25020 = CARTESIAN_POINT ( 'NONE',  ( 1.472469842513823179, 31.42559781766745530, 4.923371831947296329 ) ) ;
#25021 = ADVANCED_FACE ( 'NONE', ( #84678 ), #39055, .T. ) ;
#25022 = CARTESIAN_POINT ( 'NONE',  ( 12.26500600480481040, 44.99999999999999289, 0.000000000000000000 ) ) ;
#25023 = CARTESIAN_POINT ( 'NONE',  ( 12.63842701281683922, 9.550597817667449974, -9.846743663894590881 ) ) ;
#25024 = CARTESIAN_POINT ( 'NONE',  ( 9.846743663894590881, 23.71726448433412671, -2.638427012816833894 ) ) ;
#25025 = ORIENTED_EDGE ( 'NONE', *, *, #83219, .T. ) ;
#25026 = CARTESIAN_POINT ( 'NONE',  ( 15.44008868035555793, 6.397018677488170546, -9.422509992056140149 ) ) ;
#25027 = CARTESIAN_POINT ( 'NONE',  ( 14.92337183194729633, 2.675597817667451750, 8.527530157486181039 ) ) ;
#25029 = CARTESIAN_POINT ( 'NONE',  ( 20.88017736071110875, 45.77201867748816966, -2.915334737309920765 ) ) ;
#25028 = CARTESIAN_POINT ( 'NONE',  ( 12.91533473730992121, 49.52201867748817676, 10.88017736071110164 ) ) ;
#25030 = CARTESIAN_POINT ( 'NONE',  ( 22.81628187352647785, 41.62363466993042493, 6.195893100308588602E-16 ) ) ;
#25031 = COLOUR_RGB ( '', 0.66274510, 0.83137255, 0.94901961) ;
#25032 = CARTESIAN_POINT ( 'NONE',  ( 2.917880565312950480, 15.97041550158063217, -12.26659068614894821 ) ) ;
#25033 = AXIS2_PLACEMENT_3D ( 'NONE', #97766, #22247, #61214 ) ;
#25034 = EDGE_CURVE ( 'NONE', #32525, #50081, #20208, .T. ) ;
#25035 = CIRCLE ( 'NONE', #39373, 0.4999999999999961142 ) ;
#25036 = CARTESIAN_POINT ( 'NONE',  ( 0.6178305044545818747, 63.49863466993043204, -9.382169495545419124 ) ) ;
#25037 = ORIENTED_EDGE ( 'NONE', *, *, #96097, .T. ) ;
#25038 = CARTESIAN_POINT ( 'NONE',  ( 19.84674366389459621, 58.50893115100078745, 7.409399052514197653E-17 ) ) ;
#25039 = CARTESIAN_POINT ( 'NONE',  ( 10.00000000000000000, 21.81368534415484106, -10.88017736071110342 ) ) ;
#25040 = EDGE_LOOP ( 'NONE', ( #55127, #97613, #47375, #3239 ) ) ;
#25041 = CARTESIAN_POINT ( 'NONE',  ( 14.92337183194729988, 4.342264484334117824, -8.527530157486177487 ) ) ;
#25042 = CARTESIAN_POINT ( 'NONE',  ( 10.00000000000000000, 1.813685344154837731, -10.88017736071110342 ) ) ;
#25043 =( BOUNDED_CURVE ( )  B_SPLINE_CURVE ( 2, ( #12540, #96553, #28028, #43041, #97054, #14035, #29007, #36535, #66026, #89032, #82018, #44012, #75012 ),
 .UNSPECIFIED., .F., .T. ) 
 B_SPLINE_CURVE_WITH_KNOTS ( ( 3, 2, 2, 2, 2, 2, 3 ),
 ( 0.6333333333333334147, 0.6388888888888889506, 0.6444444444444445974, 0.6500000000000001332, 0.6555555555555556690, 0.6611111111111112049, 0.6666666666666667407 ),
 .UNSPECIFIED. ) 
 CURVE ( )  GEOMETRIC_REPRESENTATION_ITEM ( )  RATIONAL_B_SPLINE_CURVE ( ( 0.9999999999999993339, 0.9659258262890688673, 1.000000000000000000, 0.9659258262890682012, 1.000000000000000000, 0.9659258262890682012, 1.000000000000000000, 0.9659258262890682012, 1.000000000000000000, 0.9659258262890682012, 1.000000000000000000, 0.9659258262890675351, 1.000000000000000666 ) ) 
 REPRESENTATION_ITEM ( '' )  );
#25044 = CARTESIAN_POINT ( 'NONE',  ( 12.63842701281683922, 14.55059781766744997, -9.846743663894590881 ) ) ;
#25045 = CARTESIAN_POINT ( 'NONE',  ( 20.88017736071110519, 65.56368534415483396, 2.639326808657452039E-16 ) ) ;
#25046 = CARTESIAN_POINT ( 'NONE',  ( -4.431036607602665711, 0.3640475087720917435, 14.33059365769909377 ) ) ;
#25049 = LINE ( 'NONE', #25537, #55138 ) ;
#25048 = AXIS2_PLACEMENT_3D ( 'NONE', #58974, #27976, #96502 ) ;
#25047 = CARTESIAN_POINT ( 'NONE',  ( -0.8801773607111009756, 58.06368534415484106, 1.068504757029289695E-15 ) ) ;
#25050 = CARTESIAN_POINT ( 'NONE',  ( 10.00000000000000178, 59.31368534415484106, 10.88017736071110342 ) ) ;
#25052 = ORIENTED_EDGE ( 'NONE', *, *, #12204, .T. ) ;
#25051 = CARTESIAN_POINT ( 'NONE',  ( 18.52753015748618282, 8.925597817667451750, -4.923371831947291888 ) ) ;
#25053 = AXIS2_PLACEMENT_3D ( 'NONE', #94382, #41419, #86406 ) ;
#25054 = CARTESIAN_POINT ( 'NONE',  ( -2.962741594153171842, -0.03417435944610275333, 13.93860331045670975 ) ) ;
#25055 = PRESENTATION_LAYER_ASSIGNMENT (  '', '', ( #13832 ) ) ;
#25056 = CARTESIAN_POINT ( 'NONE',  ( 18.52753015748618282, 48.92559781766745886, -4.923371831947291888 ) ) ;
#25057 = ORIENTED_EDGE ( 'NONE', *, *, #56791, .T. ) ;
#25058 = DIRECTION ( 'NONE',  ( -0.9997628902338809853, 0.02177529129993028070, 1.734723475976807292E-15 ) ) ;
#25059 = CARTESIAN_POINT ( 'NONE',  ( 6.204703633549690345, 0.7620821682473009062, -14.16423886937410259 ) ) ;
#25060 = CARTESIAN_POINT ( 'NONE',  ( 16.40814093676323893, 60.79030133659709634, 11.09922568453595026 ) ) ;
#25061 = CARTESIAN_POINT ( 'NONE',  ( 24.16423886937410614, 19.30374883491397142, 8.672049930838204340E-16 ) ) ;
#25062 = CARTESIAN_POINT ( 'NONE',  ( 11.81378540890936080, 0.000000000000000000, -7.968498874458115999 ) ) ;
#25063 = DIRECTION ( 'NONE',  ( 0.000000000000000000, 0.000000000000000000, 1.000000000000000000 ) ) ;
#25064 = CARTESIAN_POINT ( 'NONE',  ( 0.5774900079438590739, 22.64701867748817321, -5.440088680355550821 ) ) ;
#25065 = CARTESIAN_POINT ( 'NONE',  ( -45.94000000000001194, 99.99999999999998579, 9.500000000000000000 ) ) ;
#25066 = ORIENTED_EDGE ( 'NONE', *, *, #43468, .F. ) ;
#25067 = SURFACE_STYLE_USAGE ( .BOTH. , #47046 ) ;
#25068 = CLOSED_SHELL ( 'NONE', ( #71821, #44002, #44199, #13454, #87358, #62476, #63363, #37181, #30849, #32161, #95451, #32404, #30912, #54514, #16187, #56006, #24446, #59833, #24129, #19860, #57112, #81298, #87175, #31400, #21479, #51599, #6555, #12089, #14348, #12440, #67016, #71449, #21820, #46855, #81837, #22973, #98926, #81005, #11312, #50103, #63857, #21236, #10413, #66732, #65900, #83333, #45072, #47461, #38892, #3516, #57554, #18394, #70036, #18426, #83188, #81719, #19188, #58623, #73020, #32741, #5454, #82177, #10021, #26756, #80402, #69771, #63722, #21333, #62080, #56133, #18872, #95034, #98285, #9769, #68774, #82192, #46934, #39414, #27026, #34203, #55892, #13283, #65593, #89479, #29123, #28652, #12648, #28611, #89635, #53915, #98911, #24651, #32508, #78700, #54574, #87387, #5731, #85268, #85033, #79632, #58306, #35795, #66053, #82308, #83992, #46388, #39488, #77522, #85821, #53419, #61245, #32283, #23744, #5089, #40668, #88789, #1847, #41361, #35817, #26009, #41668, #63044, #80248, #93784, #96508, #79584, #16908, #72694, #57789, #80731, #25380, #59147, #97385, #53662, #12798, #15059, #96180, #79495, #44635, #30364, #24689, #67991, #67186, #47932, #9503, #97344, #54771, #79464, #7083, #38064, #85146, #3799, #64130, #62395, #46170, #75889, #27225, #31317, #76349, #7464, #43580, #37610, #40448, #41439, #32070, #53192, #64944, #48098, #2296, #8454, #19203, #72579, #49944, #93265, #76044, #44922, #25261, #41471, #51823, #46411, #56873, #82239, #82174, #82784, #75106, #93495, #36623, #8137, #172, #50824, #74434, #84356, #81877, #8924, #56694, #17649, #34563, #64105, #48649, #72582, #33724, #38141, #71611, #91686, #62806, #50236, #74140, #68998, #69282, #38382, #37750, #71797, #56399, #16436, #34440, #56602, #53086, #50708, #25193, #11795, #65225, #64661, #81319, #26105, #91479, #88616, #960, #31038, #49130, #86609, #6974, #87232, #41614, #48218, #14875, #72698, #74628, #46744, #84880, #44936, #44182, #94436, #83595, #88832, #74747, #61525, #39540, #28477, #20571, #97958, #83997, #14958, #38537, #59594, #51858, #11975, #10942, #92040, #60169, #68315, #17375, #5797, #25533, #38529, #31952, #62890, #7343, #38499, #42805, #27438, #96289, #62770, #54870, #47412, #26201, #53541, #91268, #88868, #87499, #8873, #73, #85759, #55096, #10857, #15727, #36593, #14723, #44691, #83433, #59522, #594, #92168, #42244, #25333, #95153, #40088, #20268, #67214, #23271, #65235, #9166, #31922, #46023, #90218, #52307, #11886, #65805, #50705, #65825, #18192, #27755, #6387, #76668, #12635, #72843, #33635, #2741, #48122, #51043, #47291, #76537, #75882, #65143, #5713, #78133, #74178, #19221, #23976, #86027, #3404, #87915, #63993, #62658, #52384, #62005, #49667, #94512, #89785, #47237, #63558, #76880, #34892, #50283, #26968, #34652, #41360, #25805, #22481, #61636, #61996, #75396, #39321, #45291, #52946, #29469, #87650, #3930, #63357, #39207, #33489, #91235, #84666, #94729, #22845, #1178, #78012, #22131, #30281, #10744, #57347, #24200, #43007, #5154, #98008, #35370, #20964, #43376, #20221, #33290, #86545, #25625, #12130, #2947, #64711, #12295, #59142, #55962, #49166, #44575, #17556, #93143, #63999, #51802, #14832, #61527, #7816, #72550, #81600, #85259, #29917, #87026, #85510, #15519, #12698, #11359, #73303, #45524, #80887, #68718, #19973, #15369, #69438, #89218, #78923, #80706, #23148, #71155, #84806, #45746, #20383, #76103, #2870, #36479, #24544, #76650, #37945, #80198, #22356, #43356, #73135, #12924, #23862, #33993, #66721, #3407, #70015, #20002, #70240, #90705, #76662, #46132, #75757, #27447, #9697, #34668, #47051, #62061, #62635, #43591, #79395, #96666, #84282, #77555, #36738, #63331, #50410, #71077, #8404, #6209, #68104, #5242, #47447, #65453, #50827, #41501, #41468, #72254, #59949, #85028, #62183 ) ) ;
#25069 = CARTESIAN_POINT ( 'NONE',  ( 0.1532563361054082862, 21.21726448433412315, 2.638427012816831674 ) ) ;
#25070 = CARTESIAN_POINT ( 'NONE',  ( 0.6178305044545838731, 34.74863466993042493, 9.382169495545420901 ) ) ;
#25071 = CARTESIAN_POINT ( 'NONE',  ( 1.472469842513823179, 40.59226448433411605, -4.923371831947296329 ) ) ;
#25072 = ADVANCED_FACE ( 'NONE', ( #75068 ), #89895, .T. ) ;
#25073 = LINE ( 'NONE', #86057, #7500 ) ;
#25074 = CARTESIAN_POINT ( 'NONE',  ( 22.81628187352647785, 11.41530133659708390, 3.434112377981063169 ) ) ;
#25075 = CARTESIAN_POINT ( 'NONE',  ( -6.732636091893173358, -88.11213685669363826, -2.500000000000000000 ) ) ;
#25076 = PRESENTATION_LAYER_ASSIGNMENT (  '', '', ( #12265 ) ) ;
#25077 = CARTESIAN_POINT ( 'NONE',  ( 17.20831665107776587, 24.13393115100078035, -7.208316651077762316 ) ) ;
#25078 = CARTESIAN_POINT ( 'NONE',  ( 17.20831665107776587, 7.883931151000784787, 7.208316651077764980 ) ) ;
#25079 = ORIENTED_EDGE ( 'NONE', *, *, #42368, .T. ) ;
#25080 = VERTEX_POINT ( 'NONE', #10029 ) ;
#25081 = PRESENTATION_LAYER_ASSIGNMENT (  '', '', ( #4300 ) ) ;
#25082 = CARTESIAN_POINT ( 'NONE',  ( 19.42250999205614193, 30.14701867748817321, 5.440088680355555262 ) ) ;
#25083 = CARTESIAN_POINT ( 'NONE',  ( 2.917880565312948704, 32.63708216824730357, 12.26659068614894643 ) ) ;
#25084 = CARTESIAN_POINT ( 'NONE',  ( 17.20831665107776587, 39.13393115100079456, -7.208316651077762316 ) ) ;
#25085 = CARTESIAN_POINT ( 'NONE',  ( 18.52753015748618282, 18.92559781766745175, -4.923371831947291888 ) ) ;
#25087 = DIRECTION ( 'NONE',  ( -0.000000000000000000, -1.000000000000000000, -0.000000000000000000 ) ) ;
#25086 = CARTESIAN_POINT ( 'NONE',  ( 13.43411237798105340, 50.58196800326375353, 12.81628187352647963 ) ) ;
#25088 = CARTESIAN_POINT ( 'NONE',  ( 15.44008868035555793, 21.39701867748817321, -9.422509992056140149 ) ) ;
#25089 = CARTESIAN_POINT ( 'NONE',  ( -3.750000000000000000, 37.00000000000000000, -4.000000000000000000 ) ) ;
#25090 = CARTESIAN_POINT ( 'NONE',  ( 19.38216949554541557, 17.24863466993041783, -9.382169495545420901 ) ) ;
#25091 = CARTESIAN_POINT ( 'NONE',  ( 21.09922568453595559, 17.04030133659708923, -6.408140936763230044 ) ) ;
#25092 = CARTESIAN_POINT ( 'NONE',  ( 5.076628168052704559, 45.17559781766745175, -8.527530157486179263 ) ) ;
#25093 = CARTESIAN_POINT ( 'NONE',  ( 2.915334737309921209, 1.605352010821511133, -10.88017736071110164 ) ) ;
#25094 = CARTESIAN_POINT ( 'NONE',  ( -2.816281873526471635, 48.91530133659708213, -3.434112377981056508 ) ) ;
#25095 = SURFACE_STYLE_FILL_AREA ( #2106 ) ;
#25097 = DIRECTION ( 'NONE',  ( -0.9848077530122086864, -0.1736481776669272503, 0.000000000000000000 ) ) ;
#25096 = CARTESIAN_POINT ( 'NONE',  ( -0.8801773607111009756, 53.06368534415484106, 1.068504757029289695E-15 ) ) ;
#25098 = CARTESIAN_POINT ( 'NONE',  ( -10.54702889484795669, -44.61188042013009891, 4.000000000000000888 ) ) ;
#25099 = DIRECTION ( 'NONE',  ( 0.000000000000000000, 0.000000000000000000, -1.000000000000000000 ) ) ;
#25100 = CARTESIAN_POINT ( 'NONE',  ( -0.8801773607111009756, 48.06368534415484817, 1.068504757029289695E-15 ) ) ;
#25101 = CARTESIAN_POINT ( 'NONE',  ( 4.559911319644449179, 53.89701867748817676, 9.422509992056141925 ) ) ;
#25102 = DIRECTION ( 'NONE',  ( 0.000000000000000000, 0.000000000000000000, 1.000000000000000000 ) ) ;
#25103 = EDGE_CURVE ( 'NONE', #45739, #70278, #85532, .T. ) ;
#25104 = DIRECTION ( 'NONE',  ( 0.000000000000000000, 0.000000000000000000, -1.000000000000000000 ) ) ;
#25105 = VECTOR ( 'NONE', #60575, 1000.000000000000000 ) ;
#25106 = CARTESIAN_POINT ( 'NONE',  ( 19.42250999205614193, 15.14701867748817143, 5.440088680355555262 ) ) ;
#25107 = EDGE_CURVE ( 'NONE', #83096, #10733, #98075, .T. ) ;
#25108 = CARTESIAN_POINT ( 'NONE',  ( 10.00000000000000000, -2.126365330069579951, -12.81628187352647608 ) ) ;
#25110 = DIRECTION ( 'NONE',  ( -0.000000000000000000, -0.000000000000000000, -1.000000000000000000 ) ) ;
#25109 = CARTESIAN_POINT ( 'NONE',  ( 20.88017736071110875, 25.77201867748816966, -2.915334737309920765 ) ) ;
#25111 = LINE ( 'NONE', #79064, #49627 ) ;
#25112 = CARTESIAN_POINT ( 'NONE',  ( 21.09922568453595559, 27.04030133659708568, -6.408140936763230044 ) ) ;
#25113 = ORIENTED_EDGE ( 'NONE', *, *, #79929, .F. ) ;
#25114 = CARTESIAN_POINT ( 'NONE',  ( 20.88017736071110875, 55.77201867748816966, -2.915334737309920765 ) ) ;
#25115 = CARTESIAN_POINT ( 'NONE',  ( 19.84674366389459266, 38.30059781766745175, 2.638427012816836559 ) ) ;
#25117 = DIRECTION ( 'NONE',  ( -0.8320502943378436100, 0.5547001962252291474, -0.000000000000000000 ) ) ;
#25116 = CARTESIAN_POINT ( 'NONE',  ( 0.6178305044545838731, 4.748634669930420493, 9.382169495545420901 ) ) ;
#25118 = CARTESIAN_POINT ( 'NONE',  ( 10.00000000000000000, 11.81368534415483751, -10.88017736071110342 ) ) ;
#25119 = CARTESIAN_POINT ( 'NONE',  ( 19.42250999205614193, 40.14701867748817676, 5.440088680355555262 ) ) ;
#25120 = CARTESIAN_POINT ( 'NONE',  ( 24.16423886937410614, 54.51208216824730357, -3.795296366450302550 ) ) ;
#25121 = VECTOR ( 'NONE', #32728, 1000.000000000000227 ) ;
#25122 = CARTESIAN_POINT ( 'NONE',  ( 19.84674366389459621, 43.50893115100078745, 7.409399052514197653E-17 ) ) ;
#25123 = CARTESIAN_POINT ( 'NONE',  ( 10.00000000000000000, 66.81368534415484817, -10.88017736071110342 ) ) ;
#25124 = CARTESIAN_POINT ( 'NONE',  ( 0.000000000000000000, 0.000000000000000000, 0.000000000000000000 ) ) ;
#25125 = CARTESIAN_POINT ( 'NONE',  ( -4.164238869374099927, 17.01208216824730357, 3.795296366450308767 ) ) ;
#25126 = APPLICATION_CONTEXT ( 'automotive_design' ) ;
#25127 = AXIS2_PLACEMENT_3D ( 'NONE', #48514, #2069, #25058 ) ;
#25128 = CARTESIAN_POINT ( 'NONE',  ( -4.000000000000000000, 36.75000000000000000, 2.500000000000000000 ) ) ;
#25129 = CARTESIAN_POINT ( 'NONE',  ( 0.1532563361054100626, 65.80059781766745175, -2.638427012816831230 ) ) ;
#25130 = TOROIDAL_SURFACE ( 'NONE', #50650, 1.750000000000000888, 0.2500000000000000000 ) ;
#25131 = VERTEX_POINT ( 'NONE', #40530 ) ;
#25132 = ORIENTED_EDGE ( 'NONE', *, *, #50128, .F. ) ;
#25133 = CARTESIAN_POINT ( 'NONE',  ( 10.00000000000000000, 50.55374883491396787, -14.16423886937410082 ) ) ;
#25134 = CARTESIAN_POINT ( 'NONE',  ( 10.00000000000000178, 38.05374883491396787, 14.16423886937410082 ) ) ;
#25135 = CARTESIAN_POINT ( 'NONE',  ( 0.1532563361054082862, 16.21726448433411960, 2.638427012816831674 ) ) ;
#25136 = CARTESIAN_POINT ( 'NONE',  ( 16.40814093676324603, 12.45696800326375353, -11.09922568453594671 ) ) ;
#25137 = CARTESIAN_POINT ( 'NONE',  ( 2.791683348922237240, 60.38393115100078745, -7.208316651077763204 ) ) ;
#25138 = CARTESIAN_POINT ( 'NONE',  ( -10.09048698379360687, 46.92328126389585208, 0.000000000000000000 ) ) ;
#25140 = CARTESIAN_POINT ( 'NONE',  ( -2.816281873526473856, 39.12363466993041783, 9.499525473075851096E-16 ) ) ;
#25139 = CARTESIAN_POINT ( 'NONE',  ( 4.559911319644449179, 57.23035201082150536, -9.422509992056141925 ) ) ;
#25141 = EDGE_CURVE ( 'NONE', #46930, #89907, #93033, .T. ) ;
#25142 = CARTESIAN_POINT ( 'NONE',  ( 24.16423886937409904, 24.09541550158063927, 3.795296366450317205 ) ) ;
#25143 = CARTESIAN_POINT ( 'NONE',  ( 10.00000000000000000, 26.81368534415484106, -10.88017736071110342 ) ) ;
#25144 = DIRECTION ( 'NONE',  ( 0.000000000000000000, 0.000000000000000000, -1.000000000000000000 ) ) ;
#25145 = CARTESIAN_POINT ( 'NONE',  ( 14.92337183194729633, 2.675597817667451750, 8.527530157486181039 ) ) ;
#25146 = CARTESIAN_POINT ( 'NONE',  ( 4.923371831947301658, -7.324402182332545586, 8.527530157486175710 ) ) ;
#25147 = VERTEX_POINT ( 'NONE', #18505 ) ;
#25148 = DIRECTION ( 'NONE',  ( 0.000000000000000000, 0.000000000000000000, -1.000000000000000000 ) ) ;
#25149 = CARTESIAN_POINT ( 'NONE',  ( 19.72487221294570858, 70.00000000000000000, -6.000000000000000000 ) ) ;
#25150 = EDGE_LOOP ( 'NONE', ( #95111, #1013, #4103, #19703 ) ) ;
#25152 = CARTESIAN_POINT ( 'NONE',  ( 2.035157376598824452, 8.688685344154839285, 7.964842623401179544 ) ) ;
#25151 = CARTESIAN_POINT ( 'NONE',  ( 2.035157376598824452, 3.688685344154837953, 7.964842623401179544 ) ) ;
#25154 = CARTESIAN_POINT ( 'NONE',  ( 19.38216949554541202, 0.9986346699304200492, 9.382169495545424454 ) ) ;
#25153 = CARTESIAN_POINT ( 'NONE',  ( 18.52753015748617571, 43.09226448433412315, 4.923371831947298993 ) ) ;
#25155 = CARTESIAN_POINT ( 'NONE',  ( 21.92686044187656691, 59.95379003517448524, 3.195792623639537755 ) ) ;
#25156 = CARTESIAN_POINT ( 'NONE',  ( -12.60874940350935169, 15.00000000000000000, -7.160268045227203615 ) ) ;
#25157 = B_SPLINE_CURVE_WITH_KNOTS ( 'NONE', 3,
 ( #71877, #48875, #79385, #33855, #65347, #78394 ),
 .UNSPECIFIED., .F., .F.,
 ( 4, 2, 4 ),
 ( 3.409110551494648722E-05, 0.0004400426677367935105, 0.0008459942299586405406 ),
 .UNSPECIFIED. ) ;
#25158 = CARTESIAN_POINT ( 'NONE',  ( 16.40814093676323893, 5.790301336597087456, 11.09922568453595026 ) ) ;
#25159 = MECHANICAL_DESIGN_GEOMETRIC_PRESENTATION_REPRESENTATION (  '', ( #21941 ), #93783 ) ;
#25160 = ORIENTED_EDGE ( 'NONE', *, *, #32527, .F. ) ;
#25161 =( BOUNDED_SURFACE ( )  B_SPLINE_SURFACE ( 1, 2, ( 
 ( #48211, #2749, #70245, #78221, #63698, #94201, #56223, #86717, #18221, #64183, #16255, #46737, #39260, #1277, #31730, #56701, #27672, #72188, #88173, #72670, #57678, #3717, #49677, #94704, #96691, #95691, #50680, #19687, #80182, #73165, #43172, #57184, #34178, #81172, #35674, #50174, #87192, #96189, #42204, #51171, #43662, #4704, #64669, #81655, #11695, #27175, #95180, #73660, #80684, #12180, #74148, #13164, #58158, #26688, #12672, #88668, #79701, #42686, #20176, #5187, #35167, #5681, #66157, #26209, #58664, #18715, #87681, #65667, #28170, #89166, #19195, #4205, #34675, #20677, #36166, #65171, #49198, #11198, #41719, #83146, #23154, #66667, #7664, #53629, #8144, #75145, #22159, #68156, #14671, #6655, #37658, #52642, #90141, #30127, #29630, #37171, #67157, #21169, #84147, #67664, #97192, #28660, #6165, #60137, #59152, #59650, #21671, #83645, #45137, #171, #52156, #82649, #98678, #14166, #75643, #15655, #29144, #38155, #68642, #44650, #98174, #7154, #22659, #36669, #60632, #51672, #97682, #91134, #53136, #46138, #90635, #15160, #45640, #76137, #76624, #30620, #89659, #61127, #82150, #91636, #13662, #44144, #74654, #1643, #47104, #39136, #92128, #56106, #9117, #79086, #38636, #77113, #32095, #69138, #31609, #62101, #55612, #17132, #71108, #92610, #54602, #40112, #24135, #47611, #86601, #1148, #78602, #40611, #85118, #70121, #24629, #93596, #8627, #93099, #23654, #69625, #32598, #2140, #18108, #16627, #25134, #77603, #39631, #48585, #62594, #94092, #17620, #666, #86109, #31116, #70614, #48090, #61611, #63096, #16131, #55095, #85615, #78106, #46617, #9612, #54115, #2636, #10112, #33089, #63583, #25613, #84628, #58048, #72076, #49086, #96074, #50561, #34553, #3116, #12066, #57074, #66045, #58545, #88058, #79589, #96572, #64557, #42090, #11089, #88555, #72557, #4089, #89052, #28049, #73053, #41607, #65548, #4586, #94581, #65048, #42569, #35048, #19570, #20563, #81056, #10599, #73544, #41113, #87082, #80571, #50068, #27555, #3602, #34061, #95065, #95574, #12560, #26571, #49557, #20058, #87570, #27061, #51049, #71603, #43063, #33572, #64066, #19082, #57560, #5069, #35556, #80070, #26097, #11576, #56592, #18593, #44033, #22546, #83531, #36554, #14054, #67546, #37547, #21057, #37048, #66550, #51550, #75529, #45022, #63, #82038, #68038, #97566, #74535, #91525, #44536, #38042, #60522, #30511, #30018, #61014, #14553, #98564, #43543, #7042, #59042, #75032, #59538, #6539, #89548, #67044, #81539, #15049, #82535, #91013, #98059, #29030, #60024, #53016, #6056, #13549, #45521, #76021, #29516, #74038, #83036, #90032, #68533, #23039, #90519 ),
 ( #21555, #13049, #22054, #52528, #7552, #52045, #5570, #36046, #97078, #28550, #31977, #39019, #69025, #85006, #46030, #84023, #8999, #92494, #85498, #39515, #23537, #47487, #32971, #70008, #1030, #39996, #16518, #8030, #15545, #54010, #84519, #77004, #31004, #85998, #54979, #61500, #78483, #62980, #24023, #24521, #54491, #46993, #77487, #9998, #76514, #38528, #40501, #92008, #17009, #69514, #16015, #55497, #77990, #559, #46505, #62483, #9495, #70995, #2518, #63477, #8517, #17509, #31491, #70501, #2023, #47974, #61994, #1532, #93980, #53512, #92987, #32486, #93484, #25010, #64930, #26451, #49949, #95457, #26948, #4468, #25978, #73427, #4951, #95956, #48472, #63948, #34935, #33939, #42945, #50434, #3482, #94950, #78970, #41490, #87454, #40992, #56474, #10480, #65432, #19456, #64443, #65926, #11458, #57449, #42456, #86961, #56952, #18969, #49447, #72937, #3968, #10968, #71489, #79952, #17989, #55988, #41976, #72439, #87939, #34436, #94460, #80454, #35432, #11952, #71959, #27437, #57932, #3004, #86490, #18475, #48960, #79470, #33453, #88441, #19941, #80943, #12437, #25502, #66922, #67418, #97443, #28907, #21429, #22425, #27927, #20444, #52898, #35926, #29403, #81917, #66423, #98440, #90395, #43426, #81427, #6415, #52413, #83409, #14930, #45396, #58926, #29897, #5938, #67919, #82913, #59409, #58419, #44413, #74916, #75902, #97945, #14431, #89915, #5453, #7428, #89426, #36430, #88934, #51926, #37924, #96455, #28428, #90897, #50933, #96956, #36927, #12930, #73927, #20939, #59905, #13427, #21932, #44900, #51428, #43910, #75403, #37430, #82410, #74410, #6921, #13936, #60400, #17385, #46876, #38407, #55371, #23415, #912, #68908, #16887, #31375, #61873, #47854, #24886, #31861, #437, #24395, #62360, #53390, #92378, #69888, #92864, #77366, #78359, #39876, #68413, #32358, #98935, #45909, #39395, #8877, #85374, #7912, #30888, #61383, #23904, #70383, #84404, #8394, #54862, #91893, #84884, #85873, #30390, #9374, #9879, #60893, #76879, #54373, #1408, #16392, #38903, #47364, #77863, #53897, #1902, #62865, #69390, #15902, #22921, #91393, #93360, #83899, #15431, #46393, #76397, #40379, #33336, #63831, #57323, #18851, #72811, #94344, #56359, #41856, #25862, #49331, #57814, #2885, #80330, #42337, #86854, #71844, #26338, #95330, #78855, #94834, #25383, #10367, #34312, #3854, #88323, #40867, #26829, #18360, #48838, #50310, #3354, #95834, #19337, #19821, #87816, #80825, #72321, #49820, #2396, #64811, #17865, #33816, #79349, #64323, #48350, #10856, #70879, #4352, #41377, #11829, #56838, #87336, #71372, #34818, #32850, #79833, #11337, #65308 ) ),
 .UNSPECIFIED., .F., .F., .F. ) 
 B_SPLINE_SURFACE_WITH_KNOTS ( ( 2, 2 ),
 ( 3, 2, 2, 2, 2, 2, 2, 2, 2, 2, 2, 2, 2, 2, 2, 2, 2, 2, 2, 2, 2, 2, 2, 2, 2, 2, 2, 2, 2, 2, 2, 2, 2, 2, 2, 2, 2, 2, 2, 2, 2, 2, 2, 2, 2, 2, 2, 2, 2, 2, 2, 2, 2, 2, 2, 2, 2, 2, 2, 2, 2, 2, 2, 2, 2, 2, 2, 2, 2, 2, 2, 2, 2, 2, 2, 2, 2, 2, 2, 2, 2, 2, 2, 2, 2, 2, 2, 2, 2, 2, 2, 2, 2, 2, 2, 2, 2, 2, 2, 2, 2, 2, 2, 2, 2, 2, 2, 2, 2, 2, 2, 2, 2, 2, 2, 2, 2, 2, 2, 2, 2, 2, 2, 2, 2, 2, 2, 2, 2, 2, 2, 2, 2, 2, 2, 2, 2, 2, 2, 2, 2, 2, 2, 2, 2, 2, 2, 2, 2, 2, 2, 2, 2, 2, 2, 2, 2, 2, 2, 2, 2, 2, 3 ),
 ( 0.000000000000000000, 1.000000000000000000 ),
 ( 0.000000000000000000, 0.005952380952380952051, 0.01190476190476190410, 0.01785714285714285615, 0.02380952380952380820, 0.02976190476190476025, 0.03571428571428571230, 0.04166666666666666435, 0.04761904761904761640, 0.05357142857142856845, 0.05952380952380952051, 0.06547619047619047949, 0.07142857142857142461, 0.07738095238095238360, 0.08333333333333332871, 0.08928571428571428770, 0.09523809523809523281, 0.1011904761904761918, 0.1071428571428571369, 0.1130952380952380959, 0.1190476190476190410, 0.1250000000000000000, 0.1309523809523809590, 0.1369047619047619180, 0.1428571428571428492, 0.1488095238095238082, 0.1547619047619047672, 0.1607142857142857262, 0.1666666666666666574, 0.1726190476190476164, 0.1785714285714285754, 0.1845238095238095344, 0.1904761904761904656, 0.1964285714285714246, 0.2023809523809523836, 0.2083333333333333426, 0.2142857142857142738, 0.2202380952380952328, 0.2261904761904761918, 0.2321428571428571508, 0.2380952380952380820, 0.2440476190476190410, 0.2500000000000000000, 0.2559523809523809312, 0.2619047619047619180, 0.2678571428571428492, 0.2738095238095238360, 0.2797619047619047672, 0.2857142857142856984, 0.2916666666666666852, 0.2976190476190476164, 0.3035714285714285476, 0.3095238095238095344, 0.3154761904761904656, 0.3214285714285714524, 0.3273809523809523836, 0.3333333333333333148, 0.3392857142857143016, 0.3452380952380952328, 0.3511904761904761640, 0.3571428571428571508, 0.3630952380952380820, 0.3690476190476190688, 0.3750000000000000000, 0.3809523809523809312, 0.3869047619047619180, 0.3928571428571428492, 0.3988095238095238360, 0.4047619047619047672, 0.4107142857142856984, 0.4166666666666666852, 0.4226190476190476164, 0.4285714285714285476, 0.4345238095238095344, 0.4404761904761904656, 0.4464285714285714524, 0.4523809523809523836, 0.4583333333333333148, 0.4642857142857143016, 0.4702380952380952328, 0.4761904761904761640, 0.4821428571428571508, 0.4880952380952380820, 0.4940476190476190688, 0.5000000000000000000, 0.5059523809523809312, 0.5119047619047618625, 0.5178571428571429047, 0.5238095238095238360, 0.5297619047619047672, 0.5357142857142856984, 0.5416666666666666297, 0.5476190476190476719, 0.5535714285714286031, 0.5595238095238095344, 0.5654761904761904656, 0.5714285714285713969, 0.5773809523809523281, 0.5833333333333333703, 0.5892857142857143016, 0.5952380952380952328, 0.6011904761904761640, 0.6071428571428570953, 0.6130952380952381375, 0.6190476190476190688, 0.6250000000000000000, 0.6309523809523809312, 0.6369047619047618625, 0.6428571428571429047, 0.6488095238095238360, 0.6547619047619047672, 0.6607142857142856984, 0.6666666666666666297, 0.6726190476190476719, 0.6785714285714286031, 0.6845238095238095344, 0.6904761904761904656, 0.6964285714285713969, 0.7023809523809523281, 0.7083333333333333703, 0.7142857142857143016, 0.7202380952380952328, 0.7261904761904761640, 0.7321428571428570953, 0.7380952380952381375, 0.7440476190476190688, 0.7500000000000000000, 0.7559523809523809312, 0.7619047619047618625, 0.7678571428571429047, 0.7738095238095238360, 0.7797619047619047672, 0.7857142857142856984, 0.7916666666666666297, 0.7976190476190476719, 0.8035714285714286031, 0.8095238095238095344, 0.8154761904761904656, 0.8214285714285713969, 0.8273809523809523281, 0.8333333333333333703, 0.8392857142857143016, 0.8452380952380952328, 0.8511904761904761640, 0.8571428571428570953, 0.8630952380952381375, 0.8690476190476190688, 0.8750000000000000000, 0.8809523809523809312, 0.8869047619047618625, 0.8928571428571429047, 0.8988095238095238360, 0.9047619047619047672, 0.9107142857142856984, 0.9166666666666666297, 0.9226190476190476719, 0.9285714285714286031, 0.9345238095238095344, 0.9404761904761904656, 0.9464285714285713969, 0.9523809523809523281, 0.9583333333333333703, 0.9642857142857143016 ),
 .UNSPECIFIED. ) 
 GEOMETRIC_REPRESENTATION_ITEM ( )  RATIONAL_B_SPLINE_SURFACE ( (
 ( 1.000000000000000000, 0.9659258262890683122, 1.000000000000000000, 0.9659258262890683122, 1.000000000000000000, 0.9659258262890683122, 1.000000000000000000, 0.9659258262890683122, 1.000000000000000000, 0.9659258262890683122, 1.000000000000000000, 0.9659258262890683122, 1.000000000000000000, 0.9659258262890683122, 1.000000000000000000, 0.9659258262890683122, 1.000000000000000000, 0.9659258262890683122, 1.000000000000000000, 0.9659258262890683122, 1.000000000000000000, 0.9659258262890683122, 1.000000000000000000, 0.9659258262890683122, 1.000000000000000000, 0.9659258262890683122, 1.000000000000000000, 0.9659258262890683122, 1.000000000000000000, 0.9659258262890683122, 1.000000000000000000, 0.9659258262890683122, 1.000000000000000000, 0.9659258262890683122, 1.000000000000000000, 0.9659258262890683122, 1.000000000000000000, 0.9659258262890683122, 1.000000000000000000, 0.9659258262890683122, 1.000000000000000000, 0.9659258262890683122, 1.000000000000000000, 0.9659258262890683122, 1.000000000000000000, 0.9659258262890683122, 1.000000000000000000, 0.9659258262890683122, 1.000000000000000000, 0.9659258262890683122, 1.000000000000000000, 0.9659258262890683122, 1.000000000000000000, 0.9659258262890683122, 1.000000000000000000, 0.9659258262890683122, 1.000000000000000000, 0.9659258262890683122, 1.000000000000000000, 0.9659258262890683122, 1.000000000000000000, 0.9659258262890683122, 1.000000000000000000, 0.9659258262890683122, 1.000000000000000000, 0.9659258262890683122, 1.000000000000000000, 0.9659258262890683122, 1.000000000000000000, 0.9659258262890683122, 1.000000000000000000, 0.9659258262890683122, 1.000000000000000000, 0.9659258262890683122, 1.000000000000000000, 0.9659258262890683122, 1.000000000000000000, 0.9659258262890683122, 1.000000000000000000, 0.9659258262890683122, 1.000000000000000000, 0.9659258262890683122, 1.000000000000000000, 0.9659258262890683122, 1.000000000000000000, 0.9659258262890683122, 1.000000000000000000, 0.9659258262890683122, 1.000000000000000000, 0.9659258262890683122, 1.000000000000000000, 0.9659258262890683122, 1.000000000000000000, 0.9659258262890683122, 1.000000000000000000, 0.9659258262890683122, 1.000000000000000000, 0.9659258262890683122, 1.000000000000000000, 0.9659258262890683122, 1.000000000000000000, 0.9659258262890683122, 1.000000000000000000, 0.9659258262890683122, 1.000000000000000000, 0.9659258262890683122, 1.000000000000000000, 0.9659258262890683122, 1.000000000000000000, 0.9659258262890683122, 1.000000000000000000, 0.9659258262890683122, 1.000000000000000000, 0.9659258262890683122, 1.000000000000000000, 0.9659258262890683122, 1.000000000000000000, 0.9659258262890683122, 1.000000000000000000, 0.9659258262890683122, 1.000000000000000000, 0.9659258262890683122, 1.000000000000000000, 0.9659258262890683122, 1.000000000000000000, 0.9659258262890683122, 1.000000000000000000, 0.9659258262890683122, 1.000000000000000000, 0.9659258262890683122, 1.000000000000000000, 0.9659258262890683122, 1.000000000000000000, 0.9659258262890683122, 1.000000000000000000, 0.9659258262890683122, 1.000000000000000000, 0.9659258262890683122, 1.000000000000000000, 0.9659258262890683122, 1.000000000000000000, 0.9659258262890683122, 1.000000000000000000, 0.9659258262890683122, 1.000000000000000000, 0.9659258262890683122, 1.000000000000000000, 0.9659258262890683122, 1.000000000000000000, 0.9659258262890683122, 1.000000000000000000, 0.9659258262890683122, 1.000000000000000000, 0.9659258262890683122, 1.000000000000000000, 0.9659258262890683122, 1.000000000000000000, 0.9659258262890683122, 1.000000000000000000, 0.9659258262890683122, 1.000000000000000000, 0.9659258262890683122, 1.000000000000000000, 0.9659258262890683122, 1.000000000000000000, 0.9659258262890683122, 1.000000000000000000, 0.9659258262890683122, 1.000000000000000000, 0.9659258262890683122, 1.000000000000000000, 0.9659258262890683122, 1.000000000000000000, 0.9659258262890683122, 1.000000000000000000, 0.9659258262890683122, 1.000000000000000000, 0.9659258262890683122, 1.000000000000000000, 0.9659258262890683122, 1.000000000000000000, 0.9659258262890683122, 1.000000000000000000, 0.9659258262890683122, 1.000000000000000000, 0.9659258262890683122, 1.000000000000000000, 0.9659258262890683122, 1.000000000000000000, 0.9659258262890683122, 1.000000000000000000, 0.9659258262890683122, 1.000000000000000000, 0.9659258262890683122, 1.000000000000000000, 0.9659258262890683122, 1.000000000000000000, 0.9659258262890683122, 1.000000000000000000, 0.9659258262890683122, 1.000000000000000000, 0.9659258262890683122, 1.000000000000000000, 0.9659258262890683122, 1.000000000000000000, 0.9659258262890683122, 1.000000000000000000, 0.9659258262890683122, 1.000000000000000000, 0.9659258262890683122, 1.000000000000000000, 0.9659258262890683122, 1.000000000000000000, 0.9659258262890683122, 1.000000000000000000, 0.9659258262890683122, 1.000000000000000000, 0.9659258262890683122, 1.000000000000000000, 0.9659258262890683122, 1.000000000000000000, 0.9659258262890683122, 1.000000000000000000, 0.9659258262890683122, 1.000000000000000000, 0.9659258262890683122, 1.000000000000000000, 0.9659258262890683122, 1.000000000000000000, 0.9659258262890683122, 1.000000000000000000, 0.9659258262890683122, 1.000000000000000000, 0.9659258262890683122, 1.000000000000000000, 0.9659258262890683122, 1.000000000000000000, 0.9659258262890683122, 1.000000000000000000, 0.9659258262890683122, 1.000000000000000000, 0.9659258262890683122, 1.000000000000000000, 0.9659258262890683122, 1.000000000000000000, 0.9659258262890683122, 1.000000000000000000, 0.9659258262890683122, 1.000000000000000000, 0.9659258262890683122, 1.000000000000000000, 0.9659258262890683122, 1.000000000000000000, 0.9659258262890683122, 1.000000000000000000, 0.9659258262890683122, 1.000000000000000000, 0.9659258262890683122, 1.000000000000000000, 0.9659258262890683122, 1.000000000000000000, 0.9659258262890683122, 1.000000000000000000, 0.9659258262890683122, 1.000000000000000000, 0.9659258262890683122, 1.000000000000000000, 0.9659258262890683122, 1.000000000000000000, 0.9659258262890683122, 1.000000000000000000, 0.9659258262890683122, 1.000000000000000000, 0.9659258262890683122, 1.000000000000000000, 0.9659258262890683122, 1.000000000000000000, 0.9659258262890683122, 1.000000000000000000, 0.9659258262890683122, 1.000000000000000000, 0.9659258262890683122, 1.000000000000000000, 0.9659258262890683122, 1.000000000000000000, 0.9659258262890683122, 1.000000000000000000, 0.9659258262890683122, 1.000000000000000000, 0.9659258262890683122, 1.000000000000000000, 0.9659258262890683122, 1.000000000000000000, 0.9659258262890683122, 1.000000000000000000, 0.9659258262890683122, 1.000000000000000000, 0.9659258262890683122, 1.000000000000000000, 0.9659258262890683122, 1.000000000000000000, 0.9659258262890683122, 1.000000000000000000, 0.9659258262890683122, 1.000000000000000000, 0.9659258262890683122, 1.000000000000000000, 0.9659258262890683122, 1.000000000000000000, 0.9659258262890683122, 1.000000000000000000, 0.9659258262890683122, 1.000000000000000000, 0.9659258262890683122, 1.000000000000000000, 0.9659258262890683122, 1.000000000000000000, 0.9659258262890683122, 1.000000000000000000, 0.9659258262890683122, 1.000000000000000000, 0.9659258262890683122, 1.000000000000000000, 0.9659258262890683122, 1.000000000000000000),
 ( 1.000000000000000000, 0.9659258262890683122, 1.000000000000000000, 0.9659258262890683122, 1.000000000000000000, 0.9659258262890683122, 1.000000000000000000, 0.9659258262890683122, 1.000000000000000000, 0.9659258262890683122, 1.000000000000000000, 0.9659258262890683122, 1.000000000000000000, 0.9659258262890683122, 1.000000000000000000, 0.9659258262890683122, 1.000000000000000000, 0.9659258262890683122, 1.000000000000000000, 0.9659258262890683122, 1.000000000000000000, 0.9659258262890683122, 1.000000000000000000, 0.9659258262890683122, 1.000000000000000000, 0.9659258262890683122, 1.000000000000000000, 0.9659258262890683122, 1.000000000000000000, 0.9659258262890683122, 1.000000000000000000, 0.9659258262890683122, 1.000000000000000000, 0.9659258262890683122, 1.000000000000000000, 0.9659258262890683122, 1.000000000000000000, 0.9659258262890683122, 1.000000000000000000, 0.9659258262890683122, 1.000000000000000000, 0.9659258262890683122, 1.000000000000000000, 0.9659258262890683122, 1.000000000000000000, 0.9659258262890683122, 1.000000000000000000, 0.9659258262890683122, 1.000000000000000000, 0.9659258262890683122, 1.000000000000000000, 0.9659258262890683122, 1.000000000000000000, 0.9659258262890683122, 1.000000000000000000, 0.9659258262890683122, 1.000000000000000000, 0.9659258262890683122, 1.000000000000000000, 0.9659258262890683122, 1.000000000000000000, 0.9659258262890683122, 1.000000000000000000, 0.9659258262890683122, 1.000000000000000000, 0.9659258262890683122, 1.000000000000000000, 0.9659258262890683122, 1.000000000000000000, 0.9659258262890683122, 1.000000000000000000, 0.9659258262890683122, 1.000000000000000000, 0.9659258262890683122, 1.000000000000000000, 0.9659258262890683122, 1.000000000000000000, 0.9659258262890683122, 1.000000000000000000, 0.9659258262890683122, 1.000000000000000000, 0.9659258262890683122, 1.000000000000000000, 0.9659258262890683122, 1.000000000000000000, 0.9659258262890683122, 1.000000000000000000, 0.9659258262890683122, 1.000000000000000000, 0.9659258262890683122, 1.000000000000000000, 0.9659258262890683122, 1.000000000000000000, 0.9659258262890683122, 1.000000000000000000, 0.9659258262890683122, 1.000000000000000000, 0.9659258262890683122, 1.000000000000000000, 0.9659258262890683122, 1.000000000000000000, 0.9659258262890683122, 1.000000000000000000, 0.9659258262890683122, 1.000000000000000000, 0.9659258262890683122, 1.000000000000000000, 0.9659258262890683122, 1.000000000000000000, 0.9659258262890683122, 1.000000000000000000, 0.9659258262890683122, 1.000000000000000000, 0.9659258262890683122, 1.000000000000000000, 0.9659258262890683122, 1.000000000000000000, 0.9659258262890683122, 1.000000000000000000, 0.9659258262890683122, 1.000000000000000000, 0.9659258262890683122, 1.000000000000000000, 0.9659258262890683122, 1.000000000000000000, 0.9659258262890683122, 1.000000000000000000, 0.9659258262890683122, 1.000000000000000000, 0.9659258262890683122, 1.000000000000000000, 0.9659258262890683122, 1.000000000000000000, 0.9659258262890683122, 1.000000000000000000, 0.9659258262890683122, 1.000000000000000000, 0.9659258262890683122, 1.000000000000000000, 0.9659258262890683122, 1.000000000000000000, 0.9659258262890683122, 1.000000000000000000, 0.9659258262890683122, 1.000000000000000000, 0.9659258262890683122, 1.000000000000000000, 0.9659258262890683122, 1.000000000000000000, 0.9659258262890683122, 1.000000000000000000, 0.9659258262890683122, 1.000000000000000000, 0.9659258262890683122, 1.000000000000000000, 0.9659258262890683122, 1.000000000000000000, 0.9659258262890683122, 1.000000000000000000, 0.9659258262890683122, 1.000000000000000000, 0.9659258262890683122, 1.000000000000000000, 0.9659258262890683122, 1.000000000000000000, 0.9659258262890683122, 1.000000000000000000, 0.9659258262890683122, 1.000000000000000000, 0.9659258262890683122, 1.000000000000000000, 0.9659258262890683122, 1.000000000000000000, 0.9659258262890683122, 1.000000000000000000, 0.9659258262890683122, 1.000000000000000000, 0.9659258262890683122, 1.000000000000000000, 0.9659258262890683122, 1.000000000000000000, 0.9659258262890683122, 1.000000000000000000, 0.9659258262890683122, 1.000000000000000000, 0.9659258262890683122, 1.000000000000000000, 0.9659258262890683122, 1.000000000000000000, 0.9659258262890683122, 1.000000000000000000, 0.9659258262890683122, 1.000000000000000000, 0.9659258262890683122, 1.000000000000000000, 0.9659258262890683122, 1.000000000000000000, 0.9659258262890683122, 1.000000000000000000, 0.9659258262890683122, 1.000000000000000000, 0.9659258262890683122, 1.000000000000000000, 0.9659258262890683122, 1.000000000000000000, 0.9659258262890683122, 1.000000000000000000, 0.9659258262890683122, 1.000000000000000000, 0.9659258262890683122, 1.000000000000000000, 0.9659258262890683122, 1.000000000000000000, 0.9659258262890683122, 1.000000000000000000, 0.9659258262890683122, 1.000000000000000000, 0.9659258262890683122, 1.000000000000000000, 0.9659258262890683122, 1.000000000000000000, 0.9659258262890683122, 1.000000000000000000, 0.9659258262890683122, 1.000000000000000000, 0.9659258262890683122, 1.000000000000000000, 0.9659258262890683122, 1.000000000000000000, 0.9659258262890683122, 1.000000000000000000, 0.9659258262890683122, 1.000000000000000000, 0.9659258262890683122, 1.000000000000000000, 0.9659258262890683122, 1.000000000000000000, 0.9659258262890683122, 1.000000000000000000, 0.9659258262890683122, 1.000000000000000000, 0.9659258262890683122, 1.000000000000000000, 0.9659258262890683122, 1.000000000000000000, 0.9659258262890683122, 1.000000000000000000, 0.9659258262890683122, 1.000000000000000000, 0.9659258262890683122, 1.000000000000000000, 0.9659258262890683122, 1.000000000000000000, 0.9659258262890683122, 1.000000000000000000, 0.9659258262890683122, 1.000000000000000000, 0.9659258262890683122, 1.000000000000000000, 0.9659258262890683122, 1.000000000000000000, 0.9659258262890683122, 1.000000000000000000, 0.9659258262890683122, 1.000000000000000000, 0.9659258262890683122, 1.000000000000000000, 0.9659258262890683122, 1.000000000000000000, 0.9659258262890683122, 1.000000000000000000, 0.9659258262890683122, 1.000000000000000000, 0.9659258262890683122, 1.000000000000000000, 0.9659258262890683122, 1.000000000000000000, 0.9659258262890683122, 1.000000000000000000, 0.9659258262890683122, 1.000000000000000000, 0.9659258262890683122, 1.000000000000000000, 0.9659258262890683122, 1.000000000000000000, 0.9659258262890683122, 1.000000000000000000, 0.9659258262890683122, 1.000000000000000000, 0.9659258262890683122, 1.000000000000000000, 0.9659258262890683122, 1.000000000000000000, 0.9659258262890683122, 1.000000000000000000, 0.9659258262890683122, 1.000000000000000000, 0.9659258262890683122, 1.000000000000000000, 0.9659258262890683122, 1.000000000000000000, 0.9659258262890683122, 1.000000000000000000, 0.9659258262890683122, 1.000000000000000000, 0.9659258262890683122, 1.000000000000000000, 0.9659258262890683122, 1.000000000000000000, 0.9659258262890683122, 1.000000000000000000, 0.9659258262890683122, 1.000000000000000000, 0.9659258262890683122, 1.000000000000000000, 0.9659258262890683122, 1.000000000000000000, 0.9659258262890683122, 1.000000000000000000, 0.9659258262890683122, 1.000000000000000000, 0.9659258262890683122, 1.000000000000000000, 0.9659258262890683122, 1.000000000000000000) ) ) 
 REPRESENTATION_ITEM ( '' )  SURFACE ( )  );
#25162 = CARTESIAN_POINT ( 'NONE',  ( 2.917880565312948704, 47.63708216824730357, 12.26659068614894643 ) ) ;
#25163 = VERTEX_POINT ( 'NONE', #48995 ) ;
#25164 = CARTESIAN_POINT ( 'NONE',  ( 10.00000000000000000, 55.55374883491396787, -14.16423886937410082 ) ) ;
#25165 = ORIENTED_EDGE ( 'NONE', *, *, #8268, .T. ) ;
#25166 = CARTESIAN_POINT ( 'NONE',  ( 12.91533473730992121, 39.52201867748817676, 10.88017736071110164 ) ) ;
#25167 = CARTESIAN_POINT ( 'NONE',  ( -0.8801773607110991993, 42.85535201082150536, -2.915334737309923874 ) ) ;
#25168 = CARTESIAN_POINT ( 'NONE',  ( 17.96484262340118221, 36.18868534415484106, -7.964842623401177768 ) ) ;
#25169 = CARTESIAN_POINT ( 'NONE',  ( 17.96484262340118221, 66.18868534415483396, -7.964842623401177768 ) ) ;
#25170 = CARTESIAN_POINT ( 'NONE',  ( 12.91533473730992121, 24.52201867748816966, 10.88017736071110164 ) ) ;
#25171 = VECTOR ( 'NONE', #26635, 1000.000000000000000 ) ;
#25173 = AXIS2_PLACEMENT_3D ( 'NONE', #82753, #68750, #98287 ) ;
#25172 = CARTESIAN_POINT ( 'NONE',  ( 0.2078280073304309694, 0.04958531807300550764, -14.75174119393810557 ) ) ;
#25174 = CARTESIAN_POINT ( 'NONE',  ( 19.84674366389459266, 18.71726448433411960, -2.638427012816827677 ) ) ;
#25175 = VERTEX_POINT ( 'NONE', #47523 ) ;
#25176 = CARTESIAN_POINT ( 'NONE',  ( 17.20831665107776587, 42.88393115100077324, 7.208316651077764980 ) ) ;
#25177 = DIRECTION ( 'NONE',  ( 0.008726535498381206638, 0.000000000000000000, -0.9999619230641713097 ) ) ;
#25178 = CARTESIAN_POINT ( 'NONE',  ( -2.816281873526473856, 44.12363466993042493, 9.499525473075851096E-16 ) ) ;
#25179 = DIRECTION ( 'NONE',  ( -0.1736481776669272503, 0.9848077530122086864, -0.000000000000000000 ) ) ;
#25180 = PRESENTATION_LAYER_ASSIGNMENT (  '', '', ( #28368 ) ) ;
#25181 = ORIENTED_EDGE ( 'NONE', *, *, #90304, .F. ) ;
#25182 = CARTESIAN_POINT ( 'NONE',  ( -46.07360246527841952, 103.8701977390176552, 6.036219926076657138 ) ) ;
#25183 = CARTESIAN_POINT ( 'NONE',  ( 5.076628168052703671, 56.84226448433412315, 8.527530157486179263 ) ) ;
#25184 = CARTESIAN_POINT ( 'NONE',  ( -2.266590686148945544, 51.38708216824730357, -7.082119434687050408 ) ) ;
#25185 = CARTESIAN_POINT ( 'NONE',  ( 0.1532563361054083140, 66.00893115100079456, 1.131784320476157264E-15 ) ) ;
#25186 = ORIENTED_EDGE ( 'NONE', *, *, #20646, .F. ) ;
#25187 = DIRECTION ( 'NONE',  ( -1.000000000000000000, -6.938893903907221278E-15, 6.938893903907221278E-15 ) ) ;
#25188 = CARTESIAN_POINT ( 'NONE',  ( 2.791683348922237240, 20.38393115100078745, -7.208316651077763204 ) ) ;
#25189 = CIRCLE ( 'NONE', #50721, 1.999999999999996669 ) ;
#25190 = CARTESIAN_POINT ( 'NONE',  ( 21.09922568453594849, 46.20696800326376064, 6.408140936763242479 ) ) ;
#25191 = CARTESIAN_POINT ( 'NONE',  ( 5.076628168052704559, 65.17559781766745175, -8.527530157486179263 ) ) ;
#25192 = CARTESIAN_POINT ( 'NONE',  ( 19.42250999205614548, 60.98035201082151247, -5.440088680355545492 ) ) ;
#25193 = ADVANCED_FACE ( 'NONE', ( #33008 ), #38887, .T. ) ;
#25194 = AXIS2_PLACEMENT_3D ( 'NONE', #24186, #25662, #70174 ) ;
#25195 = CARTESIAN_POINT ( 'NONE',  ( 5.076628168052704559, 50.17559781766745886, -8.527530157486179263 ) ) ;
#25196 = VECTOR ( 'NONE', #86843, 1000.000000000000000 ) ;
#25197 = CARTESIAN_POINT ( 'NONE',  ( 21.92686044187657401, 15.37045670184114243, -3.195792623639525765 ) ) ;
#25198 = ORIENTED_EDGE ( 'NONE', *, *, #16836, .F. ) ;
#25199 = CARTESIAN_POINT ( 'NONE',  ( -0.3689425029237898834, 66.17874883491396076, -10.36894250292378850 ) ) ;
#25200 = CARTESIAN_POINT ( 'NONE',  ( -0.1503990784575328643, 0.07447313448805115144, 6.262539305110068177 ) ) ;
#25201 = CARTESIAN_POINT ( 'NONE',  ( 7.084665262690076126, 44.10535201082151247, 10.88017736071109987 ) ) ;
#25203 = CARTESIAN_POINT ( 'NONE',  ( 20.88017736071110875, 60.77201867748817676, -2.915334737309920765 ) ) ;
#25202 = CARTESIAN_POINT ( 'NONE',  ( 10.00000000000000000, 7.873634669930421381, -12.81628187352647608 ) ) ;
#25204 = CARTESIAN_POINT ( 'NONE',  ( -0.2418659066527716062, 62.23410085661205216, -6.114288769123046308 ) ) ;
#25205 = CARTESIAN_POINT ( 'NONE',  ( 13.55255535720591986, 15.00000000000000000, 4.403492169843056914 ) ) ;
#25206 = DIRECTION ( 'NONE',  ( 0.8038568606172245001, 0.000000000000000000, -0.5948227867513318223 ) ) ;
#25207 = CARTESIAN_POINT ( 'NONE',  ( 18.72515096720568906, 36.07228050351032778, -6.500000000000007105 ) ) ;
#25208 = CARTESIAN_POINT ( 'NONE',  ( 7.361572987183170547, 47.05059781766745175, 9.846743663894590881 ) ) ;
#25209 =( NAMED_UNIT ( * ) PLANE_ANGLE_UNIT ( ) SI_UNIT ( $, .RADIAN. ) );
#25210 = CARTESIAN_POINT ( 'NONE',  ( 10.88017736071110519, -34.43631465584515894, -2.602085213965210642E-15 ) ) ;
#25211 = CARTESIAN_POINT ( 'NONE',  ( 3.591859063236763294, 8.290301336597087456, -11.09922568453595026 ) ) ;
#25212 = CARTESIAN_POINT ( 'NONE',  ( 4.559911319644449179, 7.230352010821505360, -9.422509992056141925 ) ) ;
#25213 = DIRECTION ( 'NONE',  ( 0.9483236552061956592, 0.000000000000000000, 0.3173046564051031915 ) ) ;
#25214 = CARTESIAN_POINT ( 'NONE',  ( -2.266590686148945544, 36.38708216824730357, -7.082119434687050408 ) ) ;
#25215 = CARTESIAN_POINT ( 'NONE',  ( 24.16423886937409904, 34.09541550158064638, 3.795296366450317205 ) ) ;
#25216 = CARTESIAN_POINT ( 'NONE',  ( 4.559911319644449179, 2.230352010821504916, -9.422509992056141925 ) ) ;
#25217 = CARTESIAN_POINT ( 'NONE',  ( 19.84674366389459266, 28.30059781766745886, 2.638427012816836559 ) ) ;
#25218 = CARTESIAN_POINT ( 'NONE',  ( 6.565887622018943937, 40.16530133659708923, 12.81628187352647430 ) ) ;
#25219 = CARTESIAN_POINT ( 'NONE',  ( 20.88017736071110164, 10.35535201082150714, 2.915334737309930979 ) ) ;
#25220 = EDGE_LOOP ( 'NONE', ( #63963, #16012, #70181, #22220 ) ) ;
#25221 = CARTESIAN_POINT ( 'NONE',  ( 19.84674366389459621, 38.50893115100078745, 7.409399052514197653E-17 ) ) ;
#25222 = EDGE_CURVE ( 'NONE', #79627, #46342, #33484, .T. ) ;
#25223 = CARTESIAN_POINT ( 'NONE',  ( 12.91533473730993009, 36.60535201082151247, -10.88017736071109987 ) ) ;
#25224 = CARTESIAN_POINT ( 'NONE',  ( 17.20831665107776587, 62.88393115100078745, 7.208316651077764980 ) ) ;
#25225 = CARTESIAN_POINT ( 'NONE',  ( 6.204703633549690345, 25.76208216824730712, -14.16423886937410259 ) ) ;
#25226 = CARTESIAN_POINT ( 'NONE',  ( -2.258648100792082225, 14.95077488074853456, -14.57890972981275723 ) ) ;
#25227 = EDGE_CURVE ( 'NONE', #28519, #37810, #77182, .T. ) ;
#25228 = UNCERTAINTY_MEASURE_WITH_UNIT (LENGTH_MEASURE( 1.000000000000000082E-05 ), #77653, 'distance_accuracy_value', 'NONE');
#25229 = CARTESIAN_POINT ( 'NONE',  ( 14.92337183194729633, 22.67559781766745175, 8.527530157486181039 ) ) ;
#25230 = CARTESIAN_POINT ( 'NONE',  ( 21.09922568453595559, 57.04030133659708923, -6.408140936763230044 ) ) ;
#25231 = CARTESIAN_POINT ( 'NONE',  ( 19.84674366389459266, 48.30059781766745175, 2.638427012816836559 ) ) ;
#25232 = ORIENTED_EDGE ( 'NONE', *, *, #39854, .T. ) ;
#25233 = CARTESIAN_POINT ( 'NONE',  ( 18.00000000000000000, 84.07179676972448590, -12.00000000000000000 ) ) ;
#25234 = DIRECTION ( 'NONE',  ( 0.000000000000000000, 0.000000000000000000, -1.000000000000000000 ) ) ;
#25235 = CARTESIAN_POINT ( 'NONE',  ( 4.559911319644449179, 2.230352010821504916, -9.422509992056141925 ) ) ;
#25236 = CARTESIAN_POINT ( 'NONE',  ( 2.917880565312950480, 15.97041550158063217, -12.26659068614894821 ) ) ;
#25237 = CARTESIAN_POINT ( 'NONE',  ( -0.8801773607111008646, 68.27201867748817676, 2.915334737309923430 ) ) ;
#25238 = CARTESIAN_POINT ( 'NONE',  ( 2.791683348922240793, 56.63393115100078035, 7.208316651077764092 ) ) ;
#25239 = CARTESIAN_POINT ( 'NONE',  ( 2.035157376598822676, 17.43868534415483751, -7.964842623401177768 ) ) ;
#25240 = DIRECTION ( 'NONE',  ( 0.000000000000000000, 1.000000000000000000, 0.000000000000000000 ) ) ;
#25241 = CARTESIAN_POINT ( 'NONE',  ( 0.2751277870542967463, 70.00000000000000000, 6.000000000000000000 ) ) ;
#25242 = CARTESIAN_POINT ( 'NONE',  ( 10.00000000000000000, 4.758931151000784787, -9.846743663894594434 ) ) ;
#25243 = CARTESIAN_POINT ( 'NONE',  ( -1.099225684535947600, 58.70696800326375353, -6.408140936763238038 ) ) ;
#25244 = ORIENTED_EDGE ( 'NONE', *, *, #91444, .T. ) ;
#25245 = VERTEX_POINT ( 'NONE', #55015 ) ;
#25246 = DIRECTION ( 'NONE',  ( -0.000000000000000000, -1.000000000000000000, -0.000000000000000000 ) ) ;
#25247 = CARTESIAN_POINT ( 'NONE',  ( 18.95785429995052240, 42.24216108172005590, 6.499999999999943157 ) ) ;
#25248 = FILL_AREA_STYLE_COLOUR ( '', #34929 ) ;
#25249 = CARTESIAN_POINT ( 'NONE',  ( 22.26659068614894466, 38.88708216824731068, 7.082119434687054849 ) ) ;
#25250 = CARTESIAN_POINT ( 'NONE',  ( 2.791683348922237240, 55.38393115100078745, -7.208316651077763204 ) ) ;
#25251 = CARTESIAN_POINT ( 'NONE',  ( 19.84674366389459266, 18.30059781766745175, 2.638427012816836559 ) ) ;
#25253 = CARTESIAN_POINT ( 'NONE',  ( 14.92337183194729988, 59.34226448433412315, -8.527530157486177487 ) ) ;
#25252 = CARTESIAN_POINT ( 'NONE',  ( 17.96484262340118221, 26.18868534415483396, -7.964842623401177768 ) ) ;
#25254 = CARTESIAN_POINT ( 'NONE',  ( 14.17193700899790265, 15.00000000000000000, -1.489530601564018175 ) ) ;
#25255 = CARTESIAN_POINT ( 'NONE',  ( -0.3689425029237898834, 36.17874883491396787, -10.36894250292378850 ) ) ;
#25256 = CARTESIAN_POINT ( 'NONE',  ( 7.084665262690076126, 9.105352010821503583, 10.88017736071109987 ) ) ;
#25257 = CARTESIAN_POINT ( 'NONE',  ( 13.34343830728408697, 14.49999999999999112, -6.852200678592647698 ) ) ;
#25258 = CARTESIAN_POINT ( 'NONE',  ( 2.035157376598824452, 63.68868534415484106, 7.964842623401179544 ) ) ;
#25259 = CARTESIAN_POINT ( 'NONE',  ( 19.84674366389459266, 18.71726448433411960, -2.638427012816827677 ) ) ;
#25261 = ADVANCED_FACE ( 'NONE', ( #78026 ), #8546, .T. ) ;
#25260 = AXIS2_PLACEMENT_3D ( 'NONE', #62650, #68697, #92182 ) ;
#25262 = CARTESIAN_POINT ( 'NONE',  ( -4.537879770909789556, -17.56524742836196040, 4.000000000004837908 ) ) ;
#25263 = EDGE_CURVE ( 'NONE', #52889, #64121, #78515, .T. ) ;
#25264 = ORIENTED_EDGE ( 'NONE', *, *, #6237, .F. ) ;
#25265 = CARTESIAN_POINT ( 'NONE',  ( 6.565887622018943937, 65.16530133659709634, 12.81628187352647430 ) ) ;
#25266 = VERTEX_POINT ( 'NONE', #18019 ) ;
#25267 = CARTESIAN_POINT ( 'NONE',  ( 0.1532563361054082862, 26.21726448433411605, 2.638427012816831674 ) ) ;
#25268 = ORIENTED_EDGE ( 'NONE', *, *, #86597, .F. ) ;
#25269 = CARTESIAN_POINT ( 'NONE',  ( 2.917880565312948704, 37.63708216824731068, 12.26659068614894643 ) ) ;
#25270 = CARTESIAN_POINT ( 'NONE',  ( 0.1532563361054100626, 35.80059781766745175, -2.638427012816831230 ) ) ;
#25271 = CARTESIAN_POINT ( 'NONE',  ( 2.035157376598822676, 37.43868534415484106, -7.964842623401177768 ) ) ;
#25272 = EDGE_CURVE ( 'NONE', #74162, #45188, #90722, .T. ) ;
#25273 = STYLED_ITEM ( 'NONE', ( #36999 ), #58465 ) ;
#25274 = PLANE ( 'NONE',  #32015 ) ;
#25275 = VERTEX_POINT ( 'NONE', #11489 ) ;
#25276 = AXIS2_PLACEMENT_3D ( 'NONE', #12684, #5200, #18727 ) ;
#25277 = CARTESIAN_POINT ( 'NONE',  ( 20.88017736071110164, 40.35535201082150536, 2.915334737309930979 ) ) ;
#25278 = CARTESIAN_POINT ( 'NONE',  ( -11.09922568453594316, -10.45969866340290544, 6.408140936763246920 ) ) ;
#25279 = VERTEX_POINT ( 'NONE', #87489 ) ;
#25280 = CARTESIAN_POINT ( 'NONE',  ( 2.917880565312950480, 10.97041550158063572, -12.26659068614894821 ) ) ;
#25281 = ORIENTED_EDGE ( 'NONE', *, *, #92910, .T. ) ;
#25282 = CARTESIAN_POINT ( 'NONE',  ( 21.09922568453594849, 36.20696800326375353, 6.408140936763242479 ) ) ;
#25283 = CARTESIAN_POINT ( 'NONE',  ( 14.92337183194729633, 27.67559781766745530, 8.527530157486181039 ) ) ;
#25284 = CARTESIAN_POINT ( 'NONE',  ( -0.8801773607111008646, 3.272018677488171434, 2.915334737309923430 ) ) ;
#25285 = LINE ( 'NONE', #62756, #67148 ) ;
#25286 = CARTESIAN_POINT ( 'NONE',  ( 17.20831665107776587, 34.13393115100078745, -7.208316651077762316 ) ) ;
#25287 = ORIENTED_EDGE ( 'NONE', *, *, #34413, .F. ) ;
#25288 = DIRECTION ( 'NONE',  ( 0.000000000000000000, 1.000000000000000000, 0.000000000000000000 ) ) ;
#25289 = CARTESIAN_POINT ( 'NONE',  ( 12.91533473730992121, 54.52201867748816255, 10.88017736071110164 ) ) ;
#25290 = CARTESIAN_POINT ( 'NONE',  ( 2.120353041430538266, 15.00000000000000000, 14.34413130794944635 ) ) ;
#25291 = CARTESIAN_POINT ( 'NONE',  ( 5.076628168052704559, 0.1755978176674514724, -8.527530157486179263 ) ) ;
#25292 = DIRECTION ( 'NONE',  ( -0.6755902076156641289, 0.000000000000000000, 0.7372773368101205316 ) ) ;
#25293 = CARTESIAN_POINT ( 'NONE',  ( 10.00000000000000178, 42.25893115100078745, 9.846743663894594434 ) ) ;
#25294 = CARTESIAN_POINT ( 'NONE',  ( 14.94699059465100888, 15.00000000000000000, 1.259949270174915981 ) ) ;
#25295 = CARTESIAN_POINT ( 'NONE',  ( -4.164238869374099927, 2.012082168247300906, 3.795296366450308767 ) ) ;
#25296 = CARTESIAN_POINT ( 'NONE',  ( 12.63842701281683922, 14.55059781766744997, -9.846743663894590881 ) ) ;
#25297 = CARTESIAN_POINT ( 'NONE',  ( -2.816281873526473856, 34.12363466993042493, 9.499525473075851096E-16 ) ) ;
#25299 = CARTESIAN_POINT ( 'NONE',  ( 7.618485323809187193, 2.541098841762901017E-16, 12.48587314215767741 ) ) ;
#25298 = CARTESIAN_POINT ( 'NONE',  ( 1.274849032794164172, 18.57228050351029935, 6.499999999999802824 ) ) ;
#25300 = CARTESIAN_POINT ( 'NONE',  ( 17.96484262340118221, 49.93868534415484106, 7.964842623401181321 ) ) ;
#25301 = CARTESIAN_POINT ( 'NONE',  ( 6.565887622018943937, 3.081968003263753531, -12.81628187352647608 ) ) ;
#25302 = DIRECTION ( 'NONE',  ( -0.000000000000000000, -0.000000000000000000, 1.000000000000000000 ) ) ;
#25303 = CARTESIAN_POINT ( 'NONE',  ( 10.00000000000000178, 27.25893115100078390, 9.846743663894594434 ) ) ;
#25304 = CARTESIAN_POINT ( 'NONE',  ( 5.076628168052703671, 26.84226448433411960, 8.527530157486179263 ) ) ;
#25305 = CARTESIAN_POINT ( 'NONE',  ( 15.44008868035555260, 24.73035201082150891, 9.422509992056143702 ) ) ;
#25306 = ADVANCED_FACE ( 'NONE', ( #13461 ), #51647, .T. ) ;
#25307 = CARTESIAN_POINT ( 'NONE',  ( 0.6178305044545818747, 33.49863466993042493, -9.382169495545419124 ) ) ;
#25308 = VECTOR ( 'NONE', #34442, 1000.000000000000000 ) ;
#25309 = CARTESIAN_POINT ( 'NONE',  ( 2.791683348922240793, 21.63393115100078745, 7.208316651077764092 ) ) ;
#25310 = SHAPE_REPRESENTATION_RELATIONSHIP ( 'NONE' , 'NONE' ,  #81163, #72777 ) ;
#25311 = CARTESIAN_POINT ( 'NONE',  ( 17.39651004071838969, 44.08210964143329846, -6.500000000000027534 ) ) ;
#25312 = CARTESIAN_POINT ( 'NONE',  ( 12.91533473730992121, 19.52201867748816611, 10.88017736071110164 ) ) ;
#25313 = ORIENTED_EDGE ( 'NONE', *, *, #31695, .F. ) ;
#25314 = CARTESIAN_POINT ( 'NONE',  ( 17.96484262340118221, 61.18868534415482685, -7.964842623401177768 ) ) ;
#25315 = B_SPLINE_CURVE_WITH_KNOTS ( 'NONE', 3,
 ( #23125, #39108, #37139, #60108, #69597, #52615, #76598, #30100, #75614, #16104 ),
 .UNSPECIFIED., .F., .F.,
 ( 4, 3, 3, 4 ),
 ( 7.796612332912425077E-17, 0.0006253016069560803211, 0.001250604074564920856, 0.002501455912506534394 ),
 .UNSPECIFIED. ) ;
#25317 = CARTESIAN_POINT ( 'NONE',  ( 10.00000000000000178, 19.31368534415484106, 10.88017736071110342 ) ) ;
#25316 = CARTESIAN_POINT ( 'NONE',  ( 18.52753015748617571, 38.09226448433412315, 4.923371831947298993 ) ) ;
#25318 = FILL_AREA_STYLE ('',( #85807 ) ) ;
#25319 = CARTESIAN_POINT ( 'NONE',  ( 2.035157376598822676, 52.43868534415483396, -7.964842623401177768 ) ) ;
#25320 = PRESENTATION_LAYER_ASSIGNMENT (  '', '', ( #68426 ) ) ;
#25322 = CARTESIAN_POINT ( 'NONE',  ( 19.80832241502127289, 59.75868815902069997, 6.499999999999984901 ) ) ;
#25321 = CARTESIAN_POINT ( 'NONE',  ( 0.5774900079438590739, 17.64701867748817321, -5.440088680355550821 ) ) ;
#25323 = ORIENTED_EDGE ( 'NONE', *, *, #90908, .T. ) ;
#25324 = CARTESIAN_POINT ( 'NONE',  ( 5.076628168052703671, 36.84226448433412315, 8.527530157486179263 ) ) ;
#25325 = CARTESIAN_POINT ( 'NONE',  ( -9.876730923139204421, 14.49999999999999112, -11.28938378619079863 ) ) ;
#25326 = DIRECTION ( 'NONE',  ( -0.000000000000000000, -0.000000000000000000, 1.000000000000000000 ) ) ;
#25328 = CARTESIAN_POINT ( 'NONE',  ( -0.3689425029237898834, 1.178748834913967869, -10.36894250292378850 ) ) ;
#25327 = TOROIDAL_SURFACE ( 'NONE', #82766, 3.799999999999998934, 0.2000000000000000111 ) ;
#25329 = VECTOR ( 'NONE', #16026, 1000.000000000000000 ) ;
#25330 = CARTESIAN_POINT ( 'NONE',  ( -4.164238869374099927, 22.01208216824730357, 3.795296366450308767 ) ) ;
#25331 = CARTESIAN_POINT ( 'NONE',  ( 0.000000000000000000, 14.49999999999999822, 0.000000000000000000 ) ) ;
#25332 = ORIENTED_EDGE ( 'NONE', *, *, #934, .F. ) ;
#25333 = ADVANCED_FACE ( 'NONE', ( #86394 ), #40410, .F. ) ;
#25334 = CARTESIAN_POINT ( 'NONE',  ( 7.084665262690076126, 7.022018677488170546, -10.88017736071110164 ) ) ;
#25335 = CARTESIAN_POINT ( 'NONE',  ( 12.63842701281683034, 27.46726448433411250, 9.846743663894596210 ) ) ;
#25337 = CARTESIAN_POINT ( 'NONE',  ( -7.982674952684395642, 85.82256618331770426, -4.181766378585055399 ) ) ;
#25336 = DIRECTION ( 'NONE',  ( -0.000000000000000000, -0.000000000000000000, -1.000000000000000000 ) ) ;
#25338 = CARTESIAN_POINT ( 'NONE',  ( 15.44008868035555793, 41.39701867748817676, -9.422509992056140149 ) ) ;
#25339 = CARTESIAN_POINT ( 'NONE',  ( 3.270119481323575439, 14.95077488074853456, 14.38584091150422850 ) ) ;
#25340 = CARTESIAN_POINT ( 'NONE',  ( 4.559911319644449179, 18.89701867748817321, 9.422509992056141925 ) ) ;
#25341 = CARTESIAN_POINT ( 'NONE',  ( 3.591859063236763294, 48.29030133659708923, -11.09922568453595026 ) ) ;
#25342 = CARTESIAN_POINT ( 'NONE',  ( 10.00000000000000000, 12.87363466993042138, -12.81628187352647608 ) ) ;
#25343 = CARTESIAN_POINT ( 'NONE',  ( 0.1532563361054082862, 21.21726448433412315, 2.638427012816831674 ) ) ;
#25345 = EDGE_LOOP ( 'NONE', ( #71533, #10313, #56784, #43730, #50170, #44253, #71386 ) ) ;
#25344 = EDGE_CURVE ( 'NONE', #72583, #45054, #15716, .T. ) ;
#25346 =( LENGTH_UNIT ( ) NAMED_UNIT ( * ) SI_UNIT ( .MILLI., .METRE. ) );
#25347 = LINE ( 'NONE', #47323, #49249 ) ;
#25348 = CARTESIAN_POINT ( 'NONE',  ( -0.3689425029237898834, 56.17874883491396076, -10.36894250292378850 ) ) ;
#25349 = CARTESIAN_POINT ( 'NONE',  ( 10.00000000000000178, 28.05374883491396787, 14.16423886937410082 ) ) ;
#25350 = CARTESIAN_POINT ( 'NONE',  ( 7.084665262690076126, 14.10535201082150358, 10.88017736071109987 ) ) ;
#25351 = CARTESIAN_POINT ( 'NONE',  ( 19.42250999205614193, 55.14701867748817676, 5.440088680355555262 ) ) ;
#25352 = CARTESIAN_POINT ( 'NONE',  ( 6.879999999999995453, 79.82179676972448590, 6.250000000000000000 ) ) ;
#25353 = CARTESIAN_POINT ( 'NONE',  ( 11.18665108205495962, -81.61837458712054172, -3.999999999999999112 ) ) ;
#25354 = CARTESIAN_POINT ( 'NONE',  ( 12.63842701281683922, 9.550597817667449974, -9.846743663894590881 ) ) ;
#25355 = CARTESIAN_POINT ( 'NONE',  ( 14.92337183194729633, 22.67559781766745175, 8.527530157486181039 ) ) ;
#25356 = CARTESIAN_POINT ( 'NONE',  ( 7.361572987183169658, 24.96726448433412315, -9.846743663894592657 ) ) ;
#25357 = CARTESIAN_POINT ( 'NONE',  ( 19.84674366389459266, 43.71726448433410894, -2.638427012816827677 ) ) ;
#25358 = UNCERTAINTY_MEASURE_WITH_UNIT (LENGTH_MEASURE( 1.000000000000000082E-05 ), #93751, 'distance_accuracy_value', 'NONE');
#25359 = CARTESIAN_POINT ( 'NONE',  ( 19.38216949554541202, 35.99863466993041072, 9.382169495545424454 ) ) ;
#25360 = CARTESIAN_POINT ( 'NONE',  ( 17.96484262340118221, 56.18868534415484817, -7.964842623401177768 ) ) ;
#25361 = CARTESIAN_POINT ( 'NONE',  ( 1.472469842513823179, 35.59226448433412315, -4.923371831947296329 ) ) ;
#25363 = CARTESIAN_POINT ( 'NONE',  ( 19.84674366389459266, 28.30059781766745886, 2.638427012816836559 ) ) ;
#25362 = CARTESIAN_POINT ( 'NONE',  ( 13.79529636645030344, 43.26208216824730357, 14.16423886937410614 ) ) ;
#25364 = FACE_OUTER_BOUND ( 'NONE', #30400, .T. ) ;
#25365 = CARTESIAN_POINT ( 'NONE',  ( 7.361572987183169658, 54.96726448433413026, -9.846743663894592657 ) ) ;
#25366 = B_SPLINE_CURVE_WITH_KNOTS ( 'NONE', 3,
 ( #29191, #61172, #91678, #75186, #60185, #23197 ),
 .UNSPECIFIED., .F., .F.,
 ( 4, 2, 4 ),
 ( 3.409110551496220137E-05, 0.0004400426677368005578, 0.0008459942299586389143 ),
 .UNSPECIFIED. ) ;
#25368 = CARTESIAN_POINT ( 'NONE',  ( 20.36894250292379738, 4.928748834913967869, -10.36894250292379027 ) ) ;
#25367 = CARTESIAN_POINT ( 'NONE',  ( 0.1532563361054100626, 30.80059781766744820, -2.638427012816831230 ) ) ;
#25369 = CARTESIAN_POINT ( 'NONE',  ( 20.36894250292379738, 19.92874883491396787, -10.36894250292379027 ) ) ;
#25370 = CARTESIAN_POINT ( 'NONE',  ( 5.076628168052703671, 36.84226448433412315, 8.527530157486179263 ) ) ;
#25371 = CARTESIAN_POINT ( 'NONE',  ( 19.42250999205614193, 50.14701867748817676, 5.440088680355555262 ) ) ;
#25372 = CARTESIAN_POINT ( 'NONE',  ( -0.8801773607111008646, 18.27201867748817321, 2.915334737309923430 ) ) ;
#25373 = CARTESIAN_POINT ( 'NONE',  ( 7.084665262690076126, 49.10535201082149825, 10.88017736071109987 ) ) ;
#25374 = AXIS2_PLACEMENT_3D ( 'NONE', #92715, #77709, #40215 ) ;
#25375 = CARTESIAN_POINT ( 'NONE',  ( -0.8801773607111009756, 33.06368534415484106, 1.068504757029289695E-15 ) ) ;
#25376 = ORIENTED_EDGE ( 'NONE', *, *, #70131, .T. ) ;
#25377 = CARTESIAN_POINT ( 'NONE',  ( 4.559911319644449179, 52.23035201082151247, -9.422509992056141925 ) ) ;
#25378 = ORIENTED_EDGE ( 'NONE', *, *, #38637, .T. ) ;
#25379 = CARTESIAN_POINT ( 'NONE',  ( 13.43411237798105340, 60.58196800326376064, 12.81628187352647963 ) ) ;
#25380 = ADVANCED_FACE ( 'NONE', ( #92893 ), #91550, .T. ) ;
#25381 = CARTESIAN_POINT ( 'NONE',  ( 20.88017736071110164, 60.35535201082151957, 2.915334737309930979 ) ) ;
#25382 = ORIENTED_EDGE ( 'NONE', *, *, #95950, .F. ) ;
#25383 = CARTESIAN_POINT ( 'NONE',  ( 12.91533473730993009, 61.60535201082150536, -10.88017736071109987 ) ) ;
#25384 = CARTESIAN_POINT ( 'NONE',  ( 2.035157376598824452, 3.688685344154837953, 7.964842623401179544 ) ) ;
#25385 = CARTESIAN_POINT ( 'NONE',  ( 1.492507162822227951, 27.19955587570481015, -6.499999999999968914 ) ) ;
#25386 = CARTESIAN_POINT ( 'NONE',  ( 4.873787042390699931, 15.00000000000000000, 13.39061984619922718 ) ) ;
#25387 = CARTESIAN_POINT ( 'NONE',  ( -4.164238869374098151, 61.59541550158063217, -3.795296366450310543 ) ) ;
#25388 = CARTESIAN_POINT ( 'NONE',  ( 7.361572987183169658, 4.967264484334119601, -9.846743663894592657 ) ) ;
#25389 = CARTESIAN_POINT ( 'NONE',  ( 20.36894250292379382, 8.678748834913967869, 10.36894250292379205 ) ) ;
#25390 = CARTESIAN_POINT ( 'NONE',  ( 0.1532563361054083140, 11.00893115100078568, 1.131784320476157264E-15 ) ) ;
#25391 = CARTESIAN_POINT ( 'NONE',  ( 0.5774900079438607392, 13.48035201082150358, 5.440088680355550821 ) ) ;
#25392 = CARTESIAN_POINT ( 'NONE',  ( 7.361572987183169658, 39.96726448433411605, -9.846743663894592657 ) ) ;
#25393 = CARTESIAN_POINT ( 'NONE',  ( 18.52753015748617571, 53.09226448433412315, 4.923371831947298993 ) ) ;
#25394 = ORIENTED_EDGE ( 'NONE', *, *, #79255, .F. ) ;
#25395 = CARTESIAN_POINT ( 'NONE',  ( -10.64017930668194367, 0.3639309529147286004, -10.57291749337231757 ) ) ;
#25396 = CARTESIAN_POINT ( 'NONE',  ( 10.00000000000000000, 41.81368534415484106, -10.88017736071110342 ) ) ;
#25397 = CARTESIAN_POINT ( 'NONE',  ( 2.791683348922237240, 55.38393115100078745, -7.208316651077763204 ) ) ;
#25398 = CARTESIAN_POINT ( 'NONE',  ( 22.81628187352647785, 31.41530133659709279, 3.434112377981063169 ) ) ;
#25399 = CARTESIAN_POINT ( 'NONE',  ( 19.72487221294570858, 1.866073187300754110, 6.500000000000000888 ) ) ;
#25400 = CARTESIAN_POINT ( 'NONE',  ( -0.8801773607111008646, 58.27201867748816966, 2.915334737309923430 ) ) ;
#25401 = CARTESIAN_POINT ( 'NONE',  ( 7.084665262690076126, 7.022018677488170546, -10.88017736071110164 ) ) ;
#25402 = AXIS2_PLACEMENT_3D ( 'NONE', #98694, #4838, #42829 ) ;
#25403 = VECTOR ( 'NONE', #90401, 1000.000000000000000 ) ;
#25404 = CARTESIAN_POINT ( 'NONE',  ( 6.565887622018943937, 48.08196800326375353, -12.81628187352647608 ) ) ;
#25405 = FACE_OUTER_BOUND ( 'NONE', #93237, .T. ) ;
#25406 = ORIENTED_EDGE ( 'NONE', *, *, #12093, .T. ) ;
#25407 = CARTESIAN_POINT ( 'NONE',  ( -1.099225684535947600, 24.54030133659708923, 6.408140936763237150 ) ) ;
#25408 = CARTESIAN_POINT ( 'NONE',  ( 15.44008868035555260, 34.73035201082151247, 9.422509992056143702 ) ) ;
#25409 = EDGE_CURVE ( 'NONE', #56402, #88170, #53210, .T. ) ;
#25410 = ORIENTED_EDGE ( 'NONE', *, *, #87309, .F. ) ;
#25411 = ORIENTED_EDGE ( 'NONE', *, *, #33098, .T. ) ;
#25412 = CARTESIAN_POINT ( 'NONE',  ( 3.420591144908446957, 0.5000000000000004441, 14.60477854057958425 ) ) ;
#25413 = CARTESIAN_POINT ( 'NONE',  ( 14.92337183194729988, 4.342264484334117824, -8.527530157486177487 ) ) ;
#25414 = CARTESIAN_POINT ( 'NONE',  ( 14.92337183194729988, 59.34226448433412315, -8.527530157486177487 ) ) ;
#25416 = CARTESIAN_POINT ( 'NONE',  ( 0.1532563361054082862, 36.21726448433410894, 2.638427012816831674 ) ) ;
#25415 = CARTESIAN_POINT ( 'NONE',  ( 17.20831665107776587, 12.88393115100078390, 7.208316651077764980 ) ) ;
#25417 = CARTESIAN_POINT ( 'NONE',  ( -11.51441085139681597, -65.40266849241702118, 3.750000000000001332 ) ) ;
#25418 = CARTESIAN_POINT ( 'NONE',  ( -1.796787675079396296, 0.2301501525784628854, 14.83218748772990025 ) ) ;
#25419 = CARTESIAN_POINT ( 'NONE',  ( 0.000000000000000000, 0.000000000000000000, 0.000000000000000000 ) ) ;
#25420 = CARTESIAN_POINT ( 'NONE',  ( -14.24131928502210975, -0.03417435944610275333, -0.4973178280107823923 ) ) ;
#25421 = AXIS2_PLACEMENT_3D ( 'NONE', #56375, #56851, #78869 ) ;
#25423 =( LENGTH_UNIT ( ) NAMED_UNIT ( * ) SI_UNIT ( .MILLI., .METRE. ) );
#25422 = CARTESIAN_POINT ( 'NONE',  ( 12.63842701281683034, 32.46726448433412315, 9.846743663894596210 ) ) ;
#25424 = CARTESIAN_POINT ( 'NONE',  ( -27.43587634952537968, 22.49999999999998934, -9.500000000000000000 ) ) ;
#25425 = EDGE_CURVE ( 'NONE', #46976, #2401, #87366, .T. ) ;
#25427 = ORIENTED_EDGE ( 'NONE', *, *, #22327, .F. ) ;
#25426 = CARTESIAN_POINT ( 'NONE',  ( 18.52753015748618282, 48.92559781766745886, -4.923371831947291888 ) ) ;
#25428 = CARTESIAN_POINT ( 'NONE',  ( 22.81628187352648496, 31.83196800326375353, -3.434112377981050290 ) ) ;
#25429 = CARTESIAN_POINT ( 'NONE',  ( 12.63842701281683922, 49.55059781766744464, -9.846743663894590881 ) ) ;
#25430 = DIRECTION ( 'NONE',  ( 1.000000000000000000, 0.000000000000000000, 0.000000000000000000 ) ) ;
#25432 = EDGE_CURVE ( 'NONE', #3732, #39776, #48427, .T. ) ;
#25431 = CARTESIAN_POINT ( 'NONE',  ( 6.204703633549690345, 45.76208216824729647, -14.16423886937410259 ) ) ;
#25433 = CARTESIAN_POINT ( 'NONE',  ( 7.361572987183170547, 22.05059781766745530, 9.846743663894590881 ) ) ;
#25434 = VERTEX_POINT ( 'NONE', #83198 ) ;
#25435 = CARTESIAN_POINT ( 'NONE',  ( -4.250000000000000000, 10.00000000000000000, 3.750000000000000000 ) ) ;
#25436 = CARTESIAN_POINT ( 'NONE',  ( -27.43587634952537968, 22.49999999999998934, 9.500000000000000000 ) ) ;
#25437 = CARTESIAN_POINT ( 'NONE',  ( -0.3689425029237881626, 37.42874883491396787, 10.36894250292379027 ) ) ;
#25438 = CARTESIAN_POINT ( 'NONE',  ( 0.1532563361054083140, 61.00893115100078745, 1.131784320476157264E-15 ) ) ;
#25439 = CARTESIAN_POINT ( 'NONE',  ( -4.164238869374099039, 66.80374883491396076, 8.674139862899312516E-16 ) ) ;
#25440 = CARTESIAN_POINT ( 'NONE',  ( 6.204703633549690345, 20.76208216824730357, -14.16423886937410259 ) ) ;
#25441 = CARTESIAN_POINT ( 'NONE',  ( -0.3689425029237881626, 37.42874883491396787, 10.36894250292379027 ) ) ;
#25442 = CIRCLE ( 'NONE', #82943, 2.000000000000001776 ) ;
#25444 = CARTESIAN_POINT ( 'NONE',  ( 2.791683348922237240, 55.38393115100078745, -7.208316651077763204 ) ) ;
#25443 = CARTESIAN_POINT ( 'NONE',  ( 4.655929185144718652, -8.243906417217084837, 2.500000000000000000 ) ) ;
#25445 = VERTEX_POINT ( 'NONE', #16678 ) ;
#25446 = CARTESIAN_POINT ( 'NONE',  ( 7.084665262690076126, 37.02201867748817676, -10.88017736071110164 ) ) ;
#25447 = DIRECTION ( 'NONE',  ( 1.000000000000000000, 0.000000000000000000, -0.000000000000000000 ) ) ;
#25448 = DIRECTION ( 'NONE',  ( -0.000000000000000000, -1.000000000000000000, -0.000000000000000000 ) ) ;
#25449 = CARTESIAN_POINT ( 'NONE',  ( 1.472469842513823179, 41.42559781766745886, 4.923371831947296329 ) ) ;
#25450 = CARTESIAN_POINT ( 'NONE',  ( -8.564643372776702179, 15.00000000000000000, 12.31449893000734797 ) ) ;
#25451 = CARTESIAN_POINT ( 'NONE',  ( 7.082119434687047743, 5.137082168247313341, -12.26659068614894821 ) ) ;
#25452 = CARTESIAN_POINT ( 'NONE',  ( 19.84674366389459266, 53.71726448433411605, -2.638427012816827677 ) ) ;
#25453 = LINE ( 'NONE', #9443, #78526 ) ;
#25455 = EDGE_CURVE ( 'NONE', #40665, #97363, #30180, .T. ) ;
#25454 = ORIENTED_EDGE ( 'NONE', *, *, #75562, .F. ) ;
#25456 = CARTESIAN_POINT ( 'NONE',  ( -0.3689425029237898834, 31.17874883491396787, -10.36894250292378850 ) ) ;
#25457 = CARTESIAN_POINT ( 'NONE',  ( -46.44000000000001194, 102.9999999999998863, -5.997726559847190053 ) ) ;
#25459 = CARTESIAN_POINT ( 'NONE',  ( -10.93781366033335622, 14.49999999999999112, -10.26470809774086490 ) ) ;
#25458 = CARTESIAN_POINT ( 'NONE',  ( -3.627483523066867388, -3.617667194782701934, -2.749999999999798383 ) ) ;
#25460 = CARTESIAN_POINT ( 'NONE',  ( 20.88017736071110875, 10.77201867748817143, -2.915334737309920765 ) ) ;
#25461 = CARTESIAN_POINT ( 'NONE',  ( 16.40814093676323893, 30.79030133659708923, 11.09922568453595026 ) ) ;
#25462 = FILL_AREA_STYLE ('',( #54936 ) ) ;
#25463 = CARTESIAN_POINT ( 'NONE',  ( 2.791683348922237240, 15.38393115100078212, -7.208316651077763204 ) ) ;
#25464 = EDGE_CURVE ( 'NONE', #56371, #62932, #19664, .T. ) ;
#25465 = CARTESIAN_POINT ( 'NONE',  ( 0.000000000000000000, 0.5000000000000004441, 0.000000000000000000 ) ) ;
#25466 =( GEOMETRIC_REPRESENTATION_CONTEXT ( 3 ) GLOBAL_UNCERTAINTY_ASSIGNED_CONTEXT ( ( #34154 ) ) GLOBAL_UNIT_ASSIGNED_CONTEXT ( ( #53786, #82428, #38790 ) ) REPRESENTATION_CONTEXT ( 'NONE', 'WORKASPACE' ) );
#25467 = CARTESIAN_POINT ( 'NONE',  ( 20.20021275402706706, 0.02465945891864474576, -6.181800700214930444 ) ) ;
#25468 = CARTESIAN_POINT ( 'NONE',  ( 14.15369600240090797, 1.135024149320762060E-15, 3.689340892730358146 ) ) ;
#25469 = CARTESIAN_POINT ( 'NONE',  ( 15.44008868035555260, 14.73035201082150536, 9.422509992056143702 ) ) ;
#25470 = LINE ( 'NONE', #16972, #36815 ) ;
#25471 = CARTESIAN_POINT ( 'NONE',  ( 10.00000000000000000, 21.81368534415484106, -10.88017736071110342 ) ) ;
#25472 = CARTESIAN_POINT ( 'NONE',  ( 4.559911319644449179, 32.23035201082150536, -9.422509992056141925 ) ) ;
#25473 = CARTESIAN_POINT ( 'NONE',  ( 10.00000000000000000, 64.75893115100078035, -9.846743663894594434 ) ) ;
#25474 = CARTESIAN_POINT ( 'NONE',  ( 12.63842701281683922, 64.55059781766745175, -9.846743663894590881 ) ) ;
#25475 = CARTESIAN_POINT ( 'NONE',  ( 13.43411237798105340, 60.58196800326376064, 12.81628187352647963 ) ) ;
#25476 = CARTESIAN_POINT ( 'NONE',  ( 7.361572987183169658, 14.96726448433411960, -9.846743663894592657 ) ) ;
#25477 = VERTEX_POINT ( 'NONE', #1203 ) ;
#25478 = CARTESIAN_POINT ( 'NONE',  ( 20.88017736071110875, 35.77201867748816966, -2.915334737309920765 ) ) ;
#25479 = CARTESIAN_POINT ( 'NONE',  ( 21.09922568453595559, 32.04030133659708923, -6.408140936763230044 ) ) ;
#25480 = CARTESIAN_POINT ( 'NONE',  ( -1.926860441876564023, 54.68830936912750929, 1.004413902775740781E-15 ) ) ;
#25481 = CARTESIAN_POINT ( 'NONE',  ( 7.361572987183170547, 62.05059781766745886, 9.846743663894590881 ) ) ;
#25482 = CARTESIAN_POINT ( 'NONE',  ( 10.00000000000000000, 66.81368534415484817, -10.88017736071110342 ) ) ;
#25483 = CARTESIAN_POINT ( 'NONE',  ( 17.20831665107776587, 12.88393115100078390, 7.208316651077764980 ) ) ;
#25484 = CARTESIAN_POINT ( 'NONE',  ( 0.6178305044545838731, 34.74863466993042493, 9.382169495545420901 ) ) ;
#25486 = CARTESIAN_POINT ( 'NONE',  ( 5.803070148808322948, 15.00000000000000000, -13.28812917035385510 ) ) ;
#25485 = CARTESIAN_POINT ( 'NONE',  ( 20.88017736071110519, 55.56368534415484817, 2.639326808657452039E-16 ) ) ;
#25487 = CARTESIAN_POINT ( 'NONE',  ( 3.640395162852214650, 101.0000000000000000, -9.500000000000000000 ) ) ;
#25488 = VERTEX_POINT ( 'NONE', #31661 ) ;
#25489 = CARTESIAN_POINT ( 'NONE',  ( 4.559911319644449179, 8.897018677488171434, 9.422509992056141925 ) ) ;
#25491 = CARTESIAN_POINT ( 'NONE',  ( 17.08211943468705840, 25.13708216824730357, -12.26659068614894466 ) ) ;
#25490 = CARTESIAN_POINT ( 'NONE',  ( -1.099225684535947600, 59.54030133659708923, 6.408140936763237150 ) ) ;
#25492 = CARTESIAN_POINT ( 'NONE',  ( 5.076628168052703671, 21.84226448433411960, 8.527530157486179263 ) ) ;
#25493 = CARTESIAN_POINT ( 'NONE',  ( 19.84674366389459266, 13.30059781766745353, 2.638427012816836559 ) ) ;
#25494 = CARTESIAN_POINT ( 'NONE',  ( -4.164238869374098151, 61.59541550158063217, -3.795296366450310543 ) ) ;
#25495 = ORIENTED_EDGE ( 'NONE', *, *, #97966, .F. ) ;
#25496 = DIRECTION ( 'NONE',  ( -0.000000000000000000, -0.000000000000000000, -1.000000000000000000 ) ) ;
#25497 = TOROIDAL_SURFACE ( 'NONE', #4724, 0.5000000000000000000, 0.2500000000000000000 ) ;
#25498 = CARTESIAN_POINT ( 'NONE',  ( 4.559911319644449179, 17.23035201082150536, -9.422509992056141925 ) ) ;
#25499 = CARTESIAN_POINT ( 'NONE',  ( 0.000000000000000000, 0.000000000000000000, 0.000000000000000000 ) ) ;
#25500 = ORIENTED_EDGE ( 'NONE', *, *, #70529, .F. ) ;
#25501 = ORIENTED_EDGE ( 'NONE', *, *, #53059, .T. ) ;
#25502 = CARTESIAN_POINT ( 'NONE',  ( 20.88017736071110164, 30.35535201082151247, 2.915334737309930979 ) ) ;
#25503 = CARTESIAN_POINT ( 'NONE',  ( 12.63842701281683034, 57.46726448433411605, 9.846743663894596210 ) ) ;
#25504 = CARTESIAN_POINT ( 'NONE',  ( 10.00000000000000000, 47.87363466993042493, -12.81628187352647608 ) ) ;
#25505 = CARTESIAN_POINT ( 'NONE',  ( 13.74385066382880183, 0.2306972965111846186, 5.860428621090457035 ) ) ;
#25507 = CARTESIAN_POINT ( 'NONE',  ( 6.204703633549690345, 17.84541550158063217, 14.16423886937410082 ) ) ;
#25506 = DIRECTION ( 'NONE',  ( -0.000000000000000000, -1.000000000000000000, -0.000000000000000000 ) ) ;
#25508 = CARTESIAN_POINT ( 'NONE',  ( 17.96484262340118221, 34.93868534415482685, 7.964842623401181321 ) ) ;
#25509 = CARTESIAN_POINT ( 'NONE',  ( 12.91533473730993009, 16.60535201082150891, -10.88017736071109987 ) ) ;
#25510 = CARTESIAN_POINT ( 'NONE',  ( 0.1532563361054100626, 50.80059781766745175, -2.638427012816831230 ) ) ;
#25511 =( NAMED_UNIT ( * ) PLANE_ANGLE_UNIT ( ) SI_UNIT ( $, .RADIAN. ) );
#25512 = CARTESIAN_POINT ( 'NONE',  ( 10.00000000000000000, 29.75893115100078745, -9.846743663894594434 ) ) ;
#25513 = CARTESIAN_POINT ( 'NONE',  ( -8.564643372776448160, 0.5000000000000004441, -12.31449893000752205 ) ) ;
#25514 = CARTESIAN_POINT ( 'NONE',  ( 17.20831665107776587, 14.13393115100078568, -7.208316651077762316 ) ) ;
#25515 = CARTESIAN_POINT ( 'NONE',  ( -12.81628187352647608, -25.87636533006957507, 3.903127820947815962E-15 ) ) ;
#25516 = ORIENTED_EDGE ( 'NONE', *, *, #26997, .T. ) ;
#25517 = CARTESIAN_POINT ( 'NONE',  ( 12.14357320772536575, 54.02013147999952736, -2.899999999999999467 ) ) ;
#25518 = CARTESIAN_POINT ( 'NONE',  ( 5.076628168052704559, 10.17559781766745175, -8.527530157486179263 ) ) ;
#25519 = CARTESIAN_POINT ( 'NONE',  ( 0.1532563361054082862, 66.21726448433413736, 2.638427012816831674 ) ) ;
#25521 = CARTESIAN_POINT ( 'NONE',  ( 17.96484262340118221, 46.18868534415484106, -7.964842623401177768 ) ) ;
#25520 = CARTESIAN_POINT ( 'NONE',  ( 4.559911319644449179, 48.89701867748817676, 9.422509992056141925 ) ) ;
#25523 = CARTESIAN_POINT ( 'NONE',  ( 19.38216949554541557, 42.24863466993041783, -9.382169495545420901 ) ) ;
#25522 = CARTESIAN_POINT ( 'NONE',  ( 19.42250999205614193, 10.14701867748816966, 5.440088680355555262 ) ) ;
#25524 = CARTESIAN_POINT ( 'NONE',  ( -4.164238869374098151, 26.59541550158063217, -3.795296366450310543 ) ) ;
#25525 = CARTESIAN_POINT ( 'NONE',  ( -1.099225684535947600, 53.70696800326376064, -6.408140936763238038 ) ) ;
#25526 = VERTEX_POINT ( 'NONE', #45691 ) ;
#25527 = CARTESIAN_POINT ( 'NONE',  ( 2.791683348922237240, 55.38393115100078745, -7.208316651077763204 ) ) ;
#25528 = CARTESIAN_POINT ( 'NONE',  ( 2.035157376598822676, 22.43868534415483396, -7.964842623401177768 ) ) ;
#25529 = ORIENTED_EDGE ( 'NONE', *, *, #39416, .T. ) ;
#25530 = CARTESIAN_POINT ( 'NONE',  ( 10.00000000000000000, 4.758931151000784787, -9.846743663894594434 ) ) ;
#25531 = DIRECTION ( 'NONE',  ( -0.7716245833877234395, 0.000000000000000000, 0.6360782202777597316 ) ) ;
#25532 = CARTESIAN_POINT ( 'NONE',  ( 17.20831665107776587, 14.13393115100078568, -7.208316651077762316 ) ) ;
#25533 = ADVANCED_FACE ( 'NONE', ( #98224 ), #10121, .T. ) ;
#25534 = CARTESIAN_POINT ( 'NONE',  ( 17.96484262340118221, 66.18868534415483396, -7.964842623401177768 ) ) ;
#25535 = DIRECTION ( 'NONE',  ( -1.000000000000000000, 0.000000000000000000, 0.000000000000000000 ) ) ;
#25537 = CARTESIAN_POINT ( 'NONE',  ( 4.999999999999999112, 16.50982297312470592, 10.00000000000000000 ) ) ;
#25536 = CARTESIAN_POINT ( 'NONE',  ( 10.00000000000000000, 56.81368534415484106, -10.88017736071110342 ) ) ;
#25538 = CARTESIAN_POINT ( 'NONE',  ( 2.035157376598824452, 63.68868534415484106, 7.964842623401179544 ) ) ;
#25540 = EDGE_LOOP ( 'NONE', ( #67042, #60814, #9030 ) ) ;
#25539 = CARTESIAN_POINT ( 'NONE',  ( 12.63842701281683922, 9.550597817667449974, -9.846743663894590881 ) ) ;
#25541 = ADVANCED_FACE ( 'NONE', ( #47150 ), #31167, .T. ) ;
#25542 = DIRECTION ( 'NONE',  ( -0.1822355254921381451, 0.000000000000000000, -0.9832549075639562819 ) ) ;
#25543 = CARTESIAN_POINT ( 'NONE',  ( 14.92337183194729633, 57.67559781766745886, 8.527530157486181039 ) ) ;
#25544 = ORIENTED_EDGE ( 'NONE', *, *, #75537, .F. ) ;
#25545 = CARTESIAN_POINT ( 'NONE',  ( 12.34086200392821908, 15.00000000000000000, 7.125000000000058620 ) ) ;
#25547 = EDGE_CURVE ( 'NONE', #10733, #32140, #82448, .T. ) ;
#25546 = CARTESIAN_POINT ( 'NONE',  ( 24.16423886937410614, 9.303748834913967869, 8.672049930838204340E-16 ) ) ;
#25548 = CARTESIAN_POINT ( 'NONE',  ( -2.816281873526471635, 58.91530133659707502, -3.434112377981056508 ) ) ;
#25549 = CARTESIAN_POINT ( 'NONE',  ( -4.164238869374099927, 7.012082168247302683, 3.795296366450308767 ) ) ;
#25550 = CARTESIAN_POINT ( 'NONE',  ( -2.266590686148945544, 32.22041550158063927, 7.082119434687048631 ) ) ;
#25551 = FACE_OUTER_BOUND ( 'NONE', #81371, .T. ) ;
#25552 = CARTESIAN_POINT ( 'NONE',  ( 10.00000000000000000, 5.553748834913967869, -14.16423886937410082 ) ) ;
#25553 = CARTESIAN_POINT ( 'NONE',  ( 7.084665262690076126, 22.02201867748817321, -10.88017736071110164 ) ) ;
#25554 = LINE ( 'NONE', #17561, #81899 ) ;
#25555 = VERTEX_POINT ( 'NONE', #91183 ) ;
#25556 = CARTESIAN_POINT ( 'NONE',  ( 5.076628168052704559, 0.1755978176674514724, -8.527530157486179263 ) ) ;
#25557 = CARTESIAN_POINT ( 'NONE',  ( 0.1532563361054100626, 10.80059781766745175, -2.638427012816831230 ) ) ;
#25558 = CARTESIAN_POINT ( 'NONE',  ( 22.81628187352647785, 41.41530133659708923, 3.434112377981063169 ) ) ;
#25559 = CARTESIAN_POINT ( 'NONE',  ( 0.1532563361054100626, 35.80059781766745175, -2.638427012816831230 ) ) ;
#25560 = AXIS2_PLACEMENT_3D ( 'NONE', #25022, #40511, #86007 ) ;
#25561 = CARTESIAN_POINT ( 'NONE',  ( -13.75801628063882909, 15.00000000000000000, 4.578972376164350599 ) ) ;
#25562 = CARTESIAN_POINT ( 'NONE',  ( 1.472469842513823179, 21.42559781766745175, 4.923371831947296329 ) ) ;
#25563 = CARTESIAN_POINT ( 'NONE',  ( 3.591859063236761518, 34.95696800326375353, 11.09922568453594849 ) ) ;
#25564 = CARTESIAN_POINT ( 'NONE',  ( 0.1556627343491842341, 15.00000000000000711, 14.62580308442188404 ) ) ;
#25565 = CARTESIAN_POINT ( 'NONE',  ( 17.20831665107776587, 29.13393115100078390, -7.208316651077762316 ) ) ;
#25566 = CARTESIAN_POINT ( 'NONE',  ( 20.36894250292379738, 19.92874883491396787, -10.36894250292379027 ) ) ;
#25567 = ORIENTED_EDGE ( 'NONE', *, *, #46090, .T. ) ;
#25568 = CARTESIAN_POINT ( 'NONE',  ( 4.559911319644449179, 32.23035201082150536, -9.422509992056141925 ) ) ;
#25569 = CARTESIAN_POINT ( 'NONE',  ( 24.16423886937410614, 29.51208216824729647, -3.795296366450302550 ) ) ;
#25570 = CARTESIAN_POINT ( 'NONE',  ( 10.00000000000000000, 59.75893115100078745, -9.846743663894594434 ) ) ;
#25571 = CARTESIAN_POINT ( 'NONE',  ( 0.1532563361054082862, 6.217264484334118713, 2.638427012816831674 ) ) ;
#25573 = CARTESIAN_POINT ( 'NONE',  ( -10.17570567488967725, 89.26421072723884720, 5.905278573613795601 ) ) ;
#25572 = CARTESIAN_POINT ( 'NONE',  ( 6.565887622018943937, 58.08196800326376064, -12.81628187352647608 ) ) ;
#25574 = CARTESIAN_POINT ( 'NONE',  ( 20.88017736071110875, 25.77201867748816966, -2.915334737309920765 ) ) ;
#25575 = EDGE_CURVE ( 'NONE', #69540, #97076, #88472, .T. ) ;
#25576 = DIRECTION ( 'NONE',  ( 1.000000000000000000, 0.000000000000000000, 1.224646799147350742E-16 ) ) ;
#25577 = CARTESIAN_POINT ( 'NONE',  ( 10.00000000000000178, 15.37363466993042138, 12.81628187352647608 ) ) ;
#25578 = CARTESIAN_POINT ( 'NONE',  ( 12.63842701281683034, 42.46726448433412315, 9.846743663894596210 ) ) ;
#25579 = CARTESIAN_POINT ( 'NONE',  ( -9.422509992056145478, 7.647018677488174987, -5.440088680355541939 ) ) ;
#25580 = CARTESIAN_POINT ( 'NONE',  ( 14.43100913236849614, 4.781026887021415124E-16, 1.412789942453260839 ) ) ;
#25582 = DIRECTION ( 'NONE',  ( 1.000000000000000000, 0.000000000000000000, 0.000000000000000000 ) ) ;
#25581 = CARTESIAN_POINT ( 'NONE',  ( -0.8801773607110991993, 62.85535201082150536, -2.915334737309923874 ) ) ;
#25583 = CARTESIAN_POINT ( 'NONE',  ( 0.2751277870542876425, 45.30223176428830811, 6.499999999999984901 ) ) ;
#25585 = EDGE_CURVE ( 'NONE', #14086, #98205, #22709, .T. ) ;
#25584 = CARTESIAN_POINT ( 'NONE',  ( -14.17193700899788134, -0.03417435944610275333, -1.489530601564206247 ) ) ;
#25586 = CARTESIAN_POINT ( 'NONE',  ( 19.42250999205614193, 55.14701867748817676, 5.440088680355555262 ) ) ;
#25587 = CARTESIAN_POINT ( 'NONE',  ( 20.88017736071110519, 55.56368534415484817, 2.639326808657452039E-16 ) ) ;
#25588 = CARTESIAN_POINT ( 'NONE',  ( 7.993487411949370625, 14.95037111676401587, -12.40005926694708549 ) ) ;
#25589 = CARTESIAN_POINT ( 'NONE',  ( -13.82671409943291785, -0.03417435944610275333, -3.447387012295409114 ) ) ;
#25590 = CARTESIAN_POINT ( 'NONE',  ( 15.44008868035555260, 9.730352010821505360, 9.422509992056143702 ) ) ;
#25591 = CARTESIAN_POINT ( 'NONE',  ( 14.92337183194729633, 62.67559781766745886, 8.527530157486181039 ) ) ;
#25593 = CARTESIAN_POINT ( 'NONE',  ( -7.121364490415374782, -73.24716305332424326, -3.750000000000000000 ) ) ;
#25592 = CARTESIAN_POINT ( 'NONE',  ( 0.5774900079438590739, 17.64701867748817321, -5.440088680355550821 ) ) ;
#25594 = FILL_AREA_STYLE ('',( #10093 ) ) ;
#25595 = CARTESIAN_POINT ( 'NONE',  ( 3.591859063236763294, 28.29030133659708568, -11.09922568453595026 ) ) ;
#25596 = ORIENTED_EDGE ( 'NONE', *, *, #90075, .F. ) ;
#25597 = CARTESIAN_POINT ( 'NONE',  ( 17.96484262340118221, 44.93868534415483396, 7.964842623401181321 ) ) ;
#25598 = CARTESIAN_POINT ( 'NONE',  ( 19.84674366389459266, 43.71726448433410894, -2.638427012816827677 ) ) ;
#25600 = CARTESIAN_POINT ( 'NONE',  ( -18.00000000000000355, 75.73428692542562146, -2.900000000000000799 ) ) ;
#25599 = CARTESIAN_POINT ( 'NONE',  ( 19.38216949554541202, 5.998634669930420493, 9.382169495545424454 ) ) ;
#25601 = CARTESIAN_POINT ( 'NONE',  ( 2.035157376598822676, 32.43868534415483396, -7.964842623401177768 ) ) ;
#25602 = CARTESIAN_POINT ( 'NONE',  ( 4.559911319644449179, 38.89701867748817676, 9.422509992056141925 ) ) ;
#25603 = CARTESIAN_POINT ( 'NONE',  ( 6.204703633549690345, 47.84541550158064638, 14.16423886937410082 ) ) ;
#25604 = CARTESIAN_POINT ( 'NONE',  ( 19.84674366389459621, 38.50893115100078745, 7.409399052514197653E-17 ) ) ;
#25605 = CARTESIAN_POINT ( 'NONE',  ( 17.96484262340118221, 64.93868534415483396, 7.964842623401181321 ) ) ;
#25606 = DIRECTION ( 'NONE',  ( -1.000000000000000000, 6.938893903907221278E-15, -6.938893903907221278E-15 ) ) ;
#25607 = CARTESIAN_POINT ( 'NONE',  ( 10.00000000000000000, 20.55374883491396787, -14.16423886937410082 ) ) ;
#25608 = CARTESIAN_POINT ( 'NONE',  ( -3.750000000000000000, 9.750000000000000000, 3.750000000000000000 ) ) ;
#25609 = LINE ( 'NONE', #87079, #18452 ) ;
#25610 = CIRCLE ( 'NONE', #52785, 0.2500000000000002220 ) ;
#25611 = ORIENTED_EDGE ( 'NONE', *, *, #91572, .T. ) ;
#25612 = CARTESIAN_POINT ( 'NONE',  ( 22.26659068614894466, 48.88708216824730357, 7.082119434687054849 ) ) ;
#25613 = CARTESIAN_POINT ( 'NONE',  ( 13.79529636645030344, 43.26208216824730357, 14.16423886937410614 ) ) ;
#25614 = CARTESIAN_POINT ( 'NONE',  ( 10.00000000000000178, 17.25893115100078745, 9.846743663894594434 ) ) ;
#25615 = CARTESIAN_POINT ( 'NONE',  ( 10.00000000000000178, 20.37363466993042138, 12.81628187352647608 ) ) ;
#25616 = DIRECTION ( 'NONE',  ( 0.000000000000000000, 0.5943319733993890353, 0.8042198116156974441 ) ) ;
#25617 = FACE_OUTER_BOUND ( 'NONE', #13707, .T. ) ;
#25619 = CARTESIAN_POINT ( 'NONE',  ( 16.40814093676324603, 32.45696800326375353, -11.09922568453594671 ) ) ;
#25618 = CARTESIAN_POINT ( 'NONE',  ( 4.559911319644449179, 3.897018677488170990, 9.422509992056141925 ) ) ;
#25620 = CARTESIAN_POINT ( 'NONE',  ( 24.16423886937410614, 49.30374883491396787, 8.672049930838204340E-16 ) ) ;
#25621 =( LENGTH_UNIT ( ) NAMED_UNIT ( * ) SI_UNIT ( .MILLI., .METRE. ) );
#25622 = CARTESIAN_POINT ( 'NONE',  ( 10.00000000000000178, 64.31368534415483396, 10.88017736071110342 ) ) ;
#25623 = PRESENTATION_LAYER_ASSIGNMENT (  '', '', ( #49569 ) ) ;
#25624 = CARTESIAN_POINT ( 'NONE',  ( 8.527530157486175710, -6.074402182332544697, -4.923371831947298993 ) ) ;
#25625 = ADVANCED_FACE ( 'NONE', ( #54164 ), #38690, .F. ) ;
#25626 = VERTEX_POINT ( 'NONE', #46191 ) ;
#25627 = DIRECTION ( 'NONE',  ( -1.000000000000000000, 0.000000000000000000, -0.000000000000000000 ) ) ;
#25628 = CARTESIAN_POINT ( 'NONE',  ( 2.791683348922240793, 16.63393115100078745, 7.208316651077764092 ) ) ;
#25629 =( BOUNDED_CURVE ( )  B_SPLINE_CURVE ( 2, ( #92294, #46787, #23817, #54279, #84796, #16305, #62269 ),
 .UNSPECIFIED., .F., .F. ) 
 B_SPLINE_CURVE_WITH_KNOTS ( ( 3, 2, 2, 3 ),
 ( 0.6999999999999999556, 0.7055555555555556024, 0.7111111111111111382, 0.7150761194637891283 ),
 .UNSPECIFIED. ) 
 CURVE ( )  GEOMETRIC_REPRESENTATION_ITEM ( )  RATIONAL_B_SPLINE_CURVE ( ( 1.000000000000000000, 0.9659258262890684232, 1.000000000000000000, 0.9659258262890684232, 1.000000000000000000, 0.9756812109925998566, 0.9860751345400877721 ) ) 
 REPRESENTATION_ITEM ( '' )  );
#25630 = DIRECTION ( 'NONE',  ( 0.8070303256584298035, -0.5905099943842175847, 0.000000000000000000 ) ) ;
#25631 = VECTOR ( 'NONE', #46774, 1000.000000000000000 ) ;
#25632 = ORIENTED_EDGE ( 'NONE', *, *, #84233, .F. ) ;
#25633 = CARTESIAN_POINT ( 'NONE',  ( 6.204703633549690345, 2.845415501580634388, 14.16423886937410082 ) ) ;
#25635 = CARTESIAN_POINT ( 'NONE',  ( 15.44008868035555260, 9.730352010821505360, 9.422509992056143702 ) ) ;
#25634 = CARTESIAN_POINT ( 'NONE',  ( 20.88017736071110164, 10.35535201082150714, 2.915334737309930979 ) ) ;
#25637 = CARTESIAN_POINT ( 'NONE',  ( 21.09922568453594849, 1.206968003263753531, 6.408140936763242479 ) ) ;
#25636 = CARTESIAN_POINT ( 'NONE',  ( 2.791683348922240793, 31.63393115100078745, 7.208316651077764092 ) ) ;
#25638 = EDGE_CURVE ( 'NONE', #96742, #8774, #38205, .T. ) ;
#25639 = CARTESIAN_POINT ( 'NONE',  ( 0.000000000000000000, 15.00000000000000000, 0.000000000000000000 ) ) ;
#25640 = CARTESIAN_POINT ( 'NONE',  ( -1.099225684535947600, 18.70696800326375353, -6.408140936763238038 ) ) ;
#25641 = VERTEX_POINT ( 'NONE', #75694 ) ;
#25642 = CARTESIAN_POINT ( 'NONE',  ( 10.00000000000000000, 40.55374883491397497, -14.16423886937410082 ) ) ;
#25643 = ORIENTED_EDGE ( 'NONE', *, *, #34358, .F. ) ;
#25644 = CARTESIAN_POINT ( 'NONE',  ( 6.204703633549690345, 57.84541550158063927, 14.16423886937410082 ) ) ;
#25645 = ORIENTED_EDGE ( 'NONE', *, *, #54907, .F. ) ;
#25646 = CARTESIAN_POINT ( 'NONE',  ( 4.559911319644449179, 37.23035201082150536, -9.422509992056141925 ) ) ;
#25647 = CARTESIAN_POINT ( 'NONE',  ( 10.00000000000000178, 34.31368534415484106, 10.88017736071110342 ) ) ;
#25648 = CARTESIAN_POINT ( 'NONE',  ( 15.44008868035555793, 41.39701867748817676, -9.422509992056140149 ) ) ;
#25649 = CARTESIAN_POINT ( 'NONE',  ( -0.8801773607111009756, 68.06368534415484817, 1.068504757029289695E-15 ) ) ;
#25650 = CARTESIAN_POINT ( 'NONE',  ( 12.91533473730993009, 26.60535201082150536, -10.88017736071109987 ) ) ;
#25652 = EDGE_LOOP ( 'NONE', ( #7297, #29430 ) ) ;
#25651 = CARTESIAN_POINT ( 'NONE',  ( 0.1034006766821536916, 0.000000000000000000, -14.49963131600461352 ) ) ;
#25653 = EDGE_CURVE ( 'NONE', #60197, #46560, #2148, .T. ) ;
#25654 = VECTOR ( 'NONE', #74088, 1000.000000000000114 ) ;
#25655 = CARTESIAN_POINT ( 'NONE',  ( 14.92337183194729988, 19.34226448433411960, -8.527530157486177487 ) ) ;
#25656 = VERTEX_POINT ( 'NONE', #9165 ) ;
#25657 = CARTESIAN_POINT ( 'NONE',  ( 11.10658183848185487, -52.67641232763428150, 3.750000000000000000 ) ) ;
#25658 = CARTESIAN_POINT ( 'NONE',  ( 7.361572987183169658, 49.96726448433410894, -9.846743663894592657 ) ) ;
#25660 = ADVANCED_FACE ( 'NONE', ( #30672 ), #7206, .T. ) ;
#25659 = DIRECTION ( 'NONE',  ( 0.000000000000000000, 0.000000000000000000, 1.000000000000000000 ) ) ;
#25661 = CARTESIAN_POINT ( 'NONE',  ( -2.816281873526471635, 43.91530133659708923, -3.434112377981056508 ) ) ;
#25662 = DIRECTION ( 'NONE',  ( 0.000000000000000000, -1.000000000000000000, 0.000000000000000000 ) ) ;
#25663 = ORIENTED_EDGE ( 'NONE', *, *, #47511, .F. ) ;
#25664 = CARTESIAN_POINT ( 'NONE',  ( -46.20769938831636381, 103.7415672121642274, 6.113268130406499523 ) ) ;
#25665 = CARTESIAN_POINT ( 'NONE',  ( 20.15039907845753930, 69.92552686551195507, 6.262539305110068177 ) ) ;
#25666 = PLANE ( 'NONE',  #70580 ) ;
#25667 = CARTESIAN_POINT ( 'NONE',  ( -4.164238869374099039, 41.80374883491397497, 8.674139862899312516E-16 ) ) ;
#25668 = CARTESIAN_POINT ( 'NONE',  ( 7.361572987183170547, 67.05059781766746596, 9.846743663894590881 ) ) ;
#25669 = VERTEX_POINT ( 'NONE', #84677 ) ;
#25670 = FILL_AREA_STYLE ('',( #92666 ) ) ;
#25671 = CARTESIAN_POINT ( 'NONE',  ( 10.00000000000000178, 17.25893115100078745, 9.846743663894594434 ) ) ;
#25672 = CARTESIAN_POINT ( 'NONE',  ( 13.43411237798106583, 62.66530133659708923, -12.81628187352647252 ) ) ;
#25673 = CARTESIAN_POINT ( 'NONE',  ( 18.52753015748617571, 58.09226448433411605, 4.923371831947298993 ) ) ;
#25674 = CARTESIAN_POINT ( 'NONE',  ( 12.91533473730993009, 61.60535201082150536, -10.88017736071109987 ) ) ;
#25675 = DIRECTION ( 'NONE',  ( 0.000000000000000000, 0.000000000000000000, -1.000000000000000000 ) ) ;
#25676 = CARTESIAN_POINT ( 'NONE',  ( 5.076628168052703671, 61.84226448433412315, 8.527530157486179263 ) ) ;
#25677 = CARTESIAN_POINT ( 'NONE',  ( 21.92686044187656691, 14.95379003517447458, 3.195792623639537755 ) ) ;
#25678 = AXIS2_PLACEMENT_3D ( 'NONE', #58516, #20027, #66018 ) ;
#25679 = EDGE_LOOP ( 'NONE', ( #35196, #75417, #35611, #1525 ) ) ;
#25680 = CARTESIAN_POINT ( 'NONE',  ( 10.00000000000000178, 58.05374883491397497, 14.16423886937410082 ) ) ;
#25681 = LINE ( 'NONE', #10182, #53718 ) ;
#25682 = CARTESIAN_POINT ( 'NONE',  ( 20.88017736071110519, 45.56368534415484106, 2.639326808657452039E-16 ) ) ;
#25684 = CARTESIAN_POINT ( 'NONE',  ( 4.473274078425821365, 13.14893278465882887, -11.04690489162689104 ) ) ;
#25683 = CARTESIAN_POINT ( 'NONE',  ( 22.81628187352647785, 16.62363466993042138, 6.195893100308588602E-16 ) ) ;
#25685 = CARTESIAN_POINT ( 'NONE',  ( 20.88017736071110875, 65.77201867748817676, -2.915334737309920321 ) ) ;
#25686 = EDGE_CURVE ( 'NONE', #5283, #9418, #46667, .T. ) ;
#25688 = AXIS2_PLACEMENT_3D ( 'NONE', #26078, #34041, #49066 ) ;
#25687 = CARTESIAN_POINT ( 'NONE',  ( -5.419894505350392855, 14.49999999999999822, -13.98659156302466045 ) ) ;
#25689 = CARTESIAN_POINT ( 'NONE',  ( 0.1129803114748720444, 54.29427333184091253, -6.480634945678676928 ) ) ;
#25690 = CARTESIAN_POINT ( 'NONE',  ( 7.361572987183169658, 44.96726448433412315, -9.846743663894592657 ) ) ;
#25691 = CARTESIAN_POINT ( 'NONE',  ( 1.472469842513823179, 1.425597817667451528, 4.923371831947296329 ) ) ;
#25692 = CARTESIAN_POINT ( 'NONE',  ( -5.204170427930421283E-15, -33.18631465584515894, -10.88017736071110342 ) ) ;
#25693 = CARTESIAN_POINT ( 'NONE',  ( 16.40814093676324603, 12.45696800326375353, -11.09922568453594671 ) ) ;
#25694 = CIRCLE ( 'NONE', #57576, 14.49999999999999822 ) ;
#25696 = DIRECTION ( 'NONE',  ( -0.000000000000000000, 1.000000000000000000, 0.000000000000000000 ) ) ;
#25695 = CARTESIAN_POINT ( 'NONE',  ( 15.44008868035555793, 16.39701867748817321, -9.422509992056140149 ) ) ;
#25697 = CARTESIAN_POINT ( 'NONE',  ( 0.000000000000000000, 0.000000000000000000, 4.000000000000000000 ) ) ;
#25698 = CARTESIAN_POINT ( 'NONE',  ( 2.917880565312948704, 37.63708216824731068, 12.26659068614894643 ) ) ;
#25699 = CARTESIAN_POINT ( 'NONE',  ( 10.00000000000000178, 28.05374883491396787, 14.16423886937410082 ) ) ;
#25700 = CARTESIAN_POINT ( 'NONE',  ( 6.204703633549690345, 62.84541550158063927, 14.16423886937410082 ) ) ;
#25701 = CARTESIAN_POINT ( 'NONE',  ( 0.1532563361054082862, 41.21726448433411605, 2.638427012816831674 ) ) ;
#25702 = CARTESIAN_POINT ( 'NONE',  ( 3.591859063236763294, 33.29030133659708213, -11.09922568453595026 ) ) ;
#25703 = CARTESIAN_POINT ( 'NONE',  ( 17.96484262340118221, 9.938685344154837509, 7.964842623401181321 ) ) ;
#25704 = ORIENTED_EDGE ( 'NONE', *, *, #37254, .T. ) ;
#25705 = CARTESIAN_POINT ( 'NONE',  ( 17.20831665107776587, 34.13393115100078745, -7.208316651077762316 ) ) ;
#25706 = CARTESIAN_POINT ( 'NONE',  ( 12.91533473730993009, 41.60535201082149825, -10.88017736071109987 ) ) ;
#25707 = CARTESIAN_POINT ( 'NONE',  ( -2.816281873526473856, 9.331968003263753531, 3.434112377981055619 ) ) ;
#25708 = CARTESIAN_POINT ( 'NONE',  ( -0.3689425029237881626, 17.42874883491397142, 10.36894250292379027 ) ) ;
#25709 = DIRECTION ( 'NONE',  ( -1.000000000000000000, 0.000000000000000000, 0.000000000000000000 ) ) ;
#25710 = CARTESIAN_POINT ( 'NONE',  ( 12.63842701281683922, 29.55059781766745175, -9.846743663894590881 ) ) ;
#25711 = CARTESIAN_POINT ( 'NONE',  ( 0.6178305044545838731, 44.74863466993042493, 9.382169495545420901 ) ) ;
#25712 = CARTESIAN_POINT ( 'NONE',  ( 19.84674366389459266, 58.30059781766745886, 2.638427012816836559 ) ) ;
#25713 = ORIENTED_EDGE ( 'NONE', *, *, #18543, .T. ) ;
#25714 = CARTESIAN_POINT ( 'NONE',  ( 9.112669734029088531, -7.236323975083732485, -3.750000000000000000 ) ) ;
#25715 = CARTESIAN_POINT ( 'NONE',  ( 24.16423886937409904, 64.09541550158064638, 3.795296366450317205 ) ) ;
#25716 = CARTESIAN_POINT ( 'NONE',  ( 12.91533473730993009, 61.60535201082150536, -10.88017736071109987 ) ) ;
#25717 = CARTESIAN_POINT ( 'NONE',  ( 10.00000000000000178, 13.05374883491396787, 14.16423886937410082 ) ) ;
#25718 = CARTESIAN_POINT ( 'NONE',  ( 12.63842701281683922, 4.550597817667451750, -9.846743663894590881 ) ) ;
#25719 = CARTESIAN_POINT ( 'NONE',  ( 0.1532563361054083140, 51.00893115100078745, 1.131784320476157264E-15 ) ) ;
#25720 = CARTESIAN_POINT ( 'NONE',  ( 19.42250999205614193, 15.14701867748817143, 5.440088680355555262 ) ) ;
#25721 = LINE ( 'NONE', #86709, #97487 ) ;
#25722 = CARTESIAN_POINT ( 'NONE',  ( 10.00000000000000178, 67.25893115100079456, 9.846743663894594434 ) ) ;
#25723 = VECTOR ( 'NONE', #51376, 1000.000000000000114 ) ;
#25724 = EDGE_LOOP ( 'NONE', ( #68549, #10254, #6257, #16227 ) ) ;
#25725 = DIRECTION ( 'NONE',  ( -0.000000000000000000, -1.000000000000000000, -0.000000000000000000 ) ) ;
#25726 = ORIENTED_EDGE ( 'NONE', *, *, #416, .T. ) ;
#25727 = EDGE_LOOP ( 'NONE', ( #63394, #90124, #58062, #52173 ) ) ;
#25728 = AXIS2_PLACEMENT_3D ( 'NONE', #42413, #87412, #48918 ) ;
#25729 = CARTESIAN_POINT ( 'NONE',  ( 64.56412365047462742, 26.99999999999999645, 9.500000000000000000 ) ) ;
#25730 = B_SPLINE_CURVE_WITH_KNOTS ( 'NONE', 3,
 ( #98890, #1366, #98395, #83853, #62314, #23859 ),
 .UNSPECIFIED., .F., .F.,
 ( 4, 2, 4 ),
 ( 3.409110551474236583E-05, 0.0004400426677365819827, 0.0008459942299584215317 ),
 .UNSPECIFIED. ) ;
#25731 = CARTESIAN_POINT ( 'NONE',  ( 17.08211943468705840, 10.13708216824730179, -12.26659068614894466 ) ) ;
#25732 = CARTESIAN_POINT ( 'NONE',  ( -2.266590686148945544, 47.22041550158063927, 7.082119434687048631 ) ) ;
#25733 = CARTESIAN_POINT ( 'NONE',  ( 0.1532563361054082862, 61.21726448433412315, 2.638427012816831674 ) ) ;
#25734 = CARTESIAN_POINT ( 'NONE',  ( 17.20831665107776587, 27.88393115100078390, 7.208316651077764980 ) ) ;
#25735 = CARTESIAN_POINT ( 'NONE',  ( -0.1042174387088608406, 38.10736173766201773, 6.337391062633419558 ) ) ;
#25737 = CARTESIAN_POINT ( 'NONE',  ( 6.565887622018943937, -1.918031996736246692, -12.81628187352647608 ) ) ;
#25736 = CARTESIAN_POINT ( 'NONE',  ( -0.8801773607111008646, 18.27201867748817321, 2.915334737309923430 ) ) ;
#25738 = CARTESIAN_POINT ( 'NONE',  ( 24.16423886937410614, 9.512082168247301794, -3.795296366450302550 ) ) ;
#25739 = CARTESIAN_POINT ( 'NONE',  ( 24.16423886937410614, 39.30374883491396787, 8.672049930838204340E-16 ) ) ;
#25740 = CARTESIAN_POINT ( 'NONE',  ( 0.5774900079438590739, 2.647018677488171434, -5.440088680355550821 ) ) ;
#25742 =( BOUNDED_CURVE ( )  B_SPLINE_CURVE ( 2, ( #38380, #91869, #59879, #6891, #37404, #30863, #83873, #61360, #51899, #45883, #7399, #7888, #90368 ),
 .UNSPECIFIED., .F., .F. ) 
 B_SPLINE_CURVE_WITH_KNOTS ( ( 3, 2, 2, 2, 2, 2, 3 ),
 ( 0.5388110034902238166, 0.5388888888888888618, 0.5444444444444443976, 0.5500000000000000444, 0.5555555555555556912, 0.5611111111111112271, 0.5666666666666667629 ),
 .UNSPECIFIED. ) 
 CURVE ( )  GEOMETRIC_REPRESENTATION_ITEM ( )  RATIONAL_B_SPLINE_CURVE ( ( 0.9990579970486470618, 0.9995223014913415804, 1.000000000000000000, 0.9659258262890682012, 1.000000000000000000, 0.9659258262890682012, 1.000000000000000000, 0.9659258262890682012, 1.000000000000000000, 0.9659258262890682012, 1.000000000000000000, 0.9659258262890675351, 1.000000000000000666 ) ) 
 REPRESENTATION_ITEM ( '' )  );
#25741 = CARTESIAN_POINT ( 'NONE',  ( 0.1532563361054100626, 65.80059781766745175, -2.638427012816831230 ) ) ;
#25743 = CARTESIAN_POINT ( 'NONE',  ( 18.00000000000000000, 77.62863618568174218, 4.012044701512652800 ) ) ;
#25744 = CARTESIAN_POINT ( 'NONE',  ( 10.00000000000000000, 61.81368534415484106, -10.88017736071110342 ) ) ;
#25745 = CARTESIAN_POINT ( 'NONE',  ( 7.361572987183169658, 14.96726448433411960, -9.846743663894592657 ) ) ;
#25746 = CARTESIAN_POINT ( 'NONE',  ( -7.072388532740516709, -84.40601219567591329, 3.750000000000806022 ) ) ;
#25747 = ORIENTED_EDGE ( 'NONE', *, *, #60048, .T. ) ;
#25748 = FACE_OUTER_BOUND ( 'NONE', #25890, .T. ) ;
#25749 = ORIENTED_EDGE ( 'NONE', *, *, #31079, .T. ) ;
#25750 = CARTESIAN_POINT ( 'NONE',  ( 19.84674366389459621, 18.50893115100078745, 7.409399052514197653E-17 ) ) ;
#25751 = VERTEX_POINT ( 'NONE', #85169 ) ;
#25752 = CARTESIAN_POINT ( 'NONE',  ( 6.204703633549690345, 37.84541550158063927, 14.16423886937410082 ) ) ;
#25753 = CARTESIAN_POINT ( 'NONE',  ( 14.92337183194729633, 32.67559781766745175, 8.527530157486181039 ) ) ;
#25754 = CARTESIAN_POINT ( 'NONE',  ( 7.084665262690076126, 44.10535201082151247, 10.88017736071109987 ) ) ;
#25755 = EDGE_CURVE ( 'NONE', #6552, #59059, #14910, .T. ) ;
#25756 = CIRCLE ( 'NONE', #94385, 14.49999999999999822 ) ;
#25757 = CARTESIAN_POINT ( 'NONE',  ( 17.96484262340118221, 46.18868534415484106, -7.964842623401177768 ) ) ;
#25758 = CARTESIAN_POINT ( 'NONE',  ( 20.03447792253738768, 37.65514106990689669, -6.401564815979734036 ) ) ;
#25759 = CARTESIAN_POINT ( 'NONE',  ( -6.408140936763232709, -0.04303199673624108490, 11.09922568453595026 ) ) ;
#25760 = ORIENTED_EDGE ( 'NONE', *, *, #42026, .T. ) ;
#25761 = CARTESIAN_POINT ( 'NONE',  ( 20.36894250292379382, 8.678748834913967869, 10.36894250292379205 ) ) ;
#25762 = EDGE_LOOP ( 'NONE', ( #31146, #37046, #92747, #7863 ) ) ;
#25763 = ORIENTED_EDGE ( 'NONE', *, *, #33913, .T. ) ;
#25764 = CARTESIAN_POINT ( 'NONE',  ( 5.076628168052703671, 1.842264484334118047, 8.527530157486179263 ) ) ;
#25765 = CARTESIAN_POINT ( 'NONE',  ( 10.00000000000000000, 37.87363466993041783, -12.81628187352647608 ) ) ;
#25766 = CARTESIAN_POINT ( 'NONE',  ( 0.1532563361054100626, 25.80059781766744820, -2.638427012816831230 ) ) ;
#25767 = CARTESIAN_POINT ( 'NONE',  ( -2.816281873526473856, 44.12363466993042493, 9.499525473075851096E-16 ) ) ;
#25768 = CARTESIAN_POINT ( 'NONE',  ( 6.879999999999995453, 41.24999999999999289, -6.500000000000000888 ) ) ;
#25769 = CARTESIAN_POINT ( 'NONE',  ( 1.472469842513823179, 25.59226448433412315, -4.923371831947296329 ) ) ;
#25770 = CARTESIAN_POINT ( 'NONE',  ( 20.88017736071110875, 55.77201867748816966, -2.915334737309920765 ) ) ;
#25771 = EDGE_CURVE ( 'NONE', #18519, #34814, #33616, .T. ) ;
#25772 = CARTESIAN_POINT ( 'NONE',  ( 12.91533473730992121, 64.52201867748817676, 10.88017736071110164 ) ) ;
#25773 = CARTESIAN_POINT ( 'NONE',  ( 2.361410439757232194, 14.76930270348881002, 14.75336556272938360 ) ) ;
#25774 = CARTESIAN_POINT ( 'NONE',  ( 14.49999999999999822, 75.00000000000000000, 6.500000000000000888 ) ) ;
#25775 = CARTESIAN_POINT ( 'NONE',  ( 0.1532563361054082862, 11.21726448433411605, 2.638427012816831674 ) ) ;
#25776 = EDGE_CURVE ( 'NONE', #70273, #93127, #92024, .T. ) ;
#25777 = CARTESIAN_POINT ( 'NONE',  ( -1.099225684535947600, 8.706968003263753531, -6.408140936763238038 ) ) ;
#25778 = DIRECTION ( 'NONE',  ( -0.7971177707001962931, -0.6038238647436433570, 0.000000000000000000 ) ) ;
#25779 = CARTESIAN_POINT ( 'NONE',  ( 19.84674366389459266, 48.71726448433413026, -2.638427012816827677 ) ) ;
#25780 = DIRECTION ( 'NONE',  ( -0.2503800040544323924, 0.000000000000000000, -0.9681476403781101858 ) ) ;
#25781 = CARTESIAN_POINT ( 'NONE',  ( 6.204703633549690345, 2.845415501580634388, 14.16423886937410082 ) ) ;
#25782 = CARTESIAN_POINT ( 'NONE',  ( 0.1532563361054100626, 35.80059781766745175, -2.638427012816831230 ) ) ;
#25783 = CARTESIAN_POINT ( 'NONE',  ( 0.6178305044545838731, 29.74863466993042138, 9.382169495545420901 ) ) ;
#25784 = CARTESIAN_POINT ( 'NONE',  ( -0.8801773607110990882, 22.85535201082150181, -2.915334737309924318 ) ) ;
#25785 = CARTESIAN_POINT ( 'NONE',  ( -0.8801773607111008646, 48.27201867748816966, 2.915334737309923430 ) ) ;
#25786 = CARTESIAN_POINT ( 'NONE',  ( 0.6178305044545838731, 9.748634669930416052, 9.382169495545420901 ) ) ;
#25787 = CARTESIAN_POINT ( 'NONE',  ( 4.841308736149603220, 14.76984994420195996, 14.13449535775536958 ) ) ;
#25788 = CARTESIAN_POINT ( 'NONE',  ( 7.361572987183170547, 17.05059781766745530, 9.846743663894590881 ) ) ;
#25789 = CARTESIAN_POINT ( 'NONE',  ( 0.5774900079438607392, 33.48035201082150536, 5.440088680355550821 ) ) ;
#25790 = CARTESIAN_POINT ( 'NONE',  ( 3.591859063236761518, 34.95696800326375353, 11.09922568453594849 ) ) ;
#25791 = CARTESIAN_POINT ( 'NONE',  ( -7.803778109523453743, 84.96281847254653030, 4.037836297607493741 ) ) ;
#25792 = CARTESIAN_POINT ( 'NONE',  ( 4.559911319644449179, 22.23035201082150536, -9.422509992056141925 ) ) ;
#25793 = ORIENTED_EDGE ( 'NONE', *, *, #11863, .F. ) ;
#25794 = CARTESIAN_POINT ( 'NONE',  ( 10.00000000000000000, 61.81368534415484106, -10.88017736071110342 ) ) ;
#25796 = CARTESIAN_POINT ( 'NONE',  ( 19.42250999205614548, 25.98035201082150891, -5.440088680355545492 ) ) ;
#25795 = CARTESIAN_POINT ( 'NONE',  ( 0.1532563361054083140, 41.00893115100078745, 1.131784320476157264E-15 ) ) ;
#25797 = CARTESIAN_POINT ( 'NONE',  ( 20.00000000000000000, 0.000000000000000000, -4.500000000000001776 ) ) ;
#25798 = CARTESIAN_POINT ( 'NONE',  ( 12.91533473730993009, 41.60535201082149825, -10.88017736071109987 ) ) ;
#25799 = CARTESIAN_POINT ( 'NONE',  ( -0.8801773607110991993, 7.855352010821506248, -2.915334737309923874 ) ) ;
#25800 = LINE ( 'NONE', #56301, #77066 ) ;
#25801 = CARTESIAN_POINT ( 'NONE',  ( 2.791683348922237240, 35.38393115100079456, -7.208316651077763204 ) ) ;
#25803 = DIRECTION ( 'NONE',  ( 0.1650476058606741014, -0.000000000000000000, 0.9862856015372319929 ) ) ;
#25802 = CARTESIAN_POINT ( 'NONE',  ( 2.917880565312950480, 45.97041550158063927, -12.26659068614894821 ) ) ;
#25804 = CARTESIAN_POINT ( 'NONE',  ( 6.880000000000009663, 40.99999999999999289, -6.250000000000000000 ) ) ;
#25805 = ADVANCED_FACE ( 'NONE', ( #34107 ), #10644, .F. ) ;
#25806 = CARTESIAN_POINT ( 'NONE',  ( 6.565887622018943937, 0.1653013365970866511, 12.81628187352647430 ) ) ;
#25807 = DIRECTION ( 'NONE',  ( -1.000000000000000000, 0.000000000000000000, 0.000000000000000000 ) ) ;
#25808 = CARTESIAN_POINT ( 'NONE',  ( 10.00000000000000000, 30.55374883491397142, -14.16423886937410082 ) ) ;
#25809 = TOROIDAL_SURFACE ( 'NONE', #64104, 14.49999999999999822, 0.5000000000000000000 ) ;
#25810 = STYLED_ITEM ( 'NONE', ( #7445 ), #32648 ) ;
#25811 = FACE_OUTER_BOUND ( 'NONE', #51959, .T. ) ;
#25812 = ORIENTED_EDGE ( 'NONE', *, *, #2016, .T. ) ;
#25813 = CARTESIAN_POINT ( 'NONE',  ( -0.3689425029237898834, 66.17874883491396076, -10.36894250292378850 ) ) ;
#25814 = CARTESIAN_POINT ( 'NONE',  ( 10.00000000000000000, 19.75893115100078390, -9.846743663894594434 ) ) ;
#25815 = DIRECTION ( 'NONE',  ( -0.000000000000000000, -0.000000000000000000, 1.000000000000000000 ) ) ;
#25816 = CARTESIAN_POINT ( 'NONE',  ( 2.035157376598822676, 62.43868534415483396, -7.964842623401177768 ) ) ;
#25817 = CARTESIAN_POINT ( 'NONE',  ( -2.816281873526473856, 64.33196800326376774, 3.434112377981055619 ) ) ;
#25818 = CARTESIAN_POINT ( 'NONE',  ( -0.8801773607110991993, 27.85535201082150181, -2.915334737309923874 ) ) ;
#25819 = CARTESIAN_POINT ( 'NONE',  ( 10.00000000000000178, 55.37363466993042493, 12.81628187352647608 ) ) ;
#25820 = CARTESIAN_POINT ( 'NONE',  ( 6.565887622018943937, 5.165301336597086568, 12.81628187352647430 ) ) ;
#25821 = CARTESIAN_POINT ( 'NONE',  ( 1.472469842513823179, 10.59226448433411782, -4.923371831947296329 ) ) ;
#25822 = VERTEX_POINT ( 'NONE', #40159 ) ;
#25823 = CARTESIAN_POINT ( 'NONE',  ( 0.1532563361054083140, 1.008931151000784787, 1.131784320476157264E-15 ) ) ;
#25824 = CARTESIAN_POINT ( 'NONE',  ( 0.1143410931637250938, 20.21691075486302580, 6.480892540919863443 ) ) ;
#25825 = CARTESIAN_POINT ( 'NONE',  ( -4.164238869374098151, 51.59541550158063217, -3.795296366450310543 ) ) ;
#25826 = CARTESIAN_POINT ( 'NONE',  ( -2.266590686148945544, 26.38708216824730357, -7.082119434687050408 ) ) ;
#25827 = CARTESIAN_POINT ( 'NONE',  ( 0.5774900079438607392, 33.48035201082150536, 5.440088680355550821 ) ) ;
#25828 = CARTESIAN_POINT ( 'NONE',  ( 17.96484262340118221, 46.18868534415484106, -7.964842623401177768 ) ) ;
#25829 = DIRECTION ( 'NONE',  ( 0.000000000000000000, 0.000000000000000000, -1.000000000000000000 ) ) ;
#25830 = CARTESIAN_POINT ( 'NONE',  ( 10.95672020364514054, -56.81584260457095326, -4.000000000000000000 ) ) ;
#25831 = CARTESIAN_POINT ( 'NONE',  ( 5.076628168052703671, 11.84226448433411960, 8.527530157486179263 ) ) ;
#25832 = FILL_AREA_STYLE_COLOUR ( '', #83308 ) ;
#25833 = CARTESIAN_POINT ( 'NONE',  ( 10.00000000000000000, 14.75893115100078568, -9.846743663894594434 ) ) ;
#25834 = CARTESIAN_POINT ( 'NONE',  ( 1.114591949025028450, 15.00000000000000000, -14.45709807627964416 ) ) ;
#25835 = CIRCLE ( 'NONE', #53010, 15.00000000000000000 ) ;
#25836 = LINE ( 'NONE', #95298, #86263 ) ;
#25837 = CARTESIAN_POINT ( 'NONE',  ( 17.20831665107776587, 29.13393115100078390, -7.208316651077762316 ) ) ;
#25838 = CARTESIAN_POINT ( 'NONE',  ( 2.791683348922237240, 45.38393115100079456, -7.208316651077763204 ) ) ;
#25839 = CARTESIAN_POINT ( 'NONE',  ( 12.91533473730993009, 26.60535201082150536, -10.88017736071109987 ) ) ;
#25840 = CARTESIAN_POINT ( 'NONE',  ( -2.816281873526473856, 39.12363466993041783, 9.499525473075851096E-16 ) ) ;
#25841 = CARTESIAN_POINT ( 'NONE',  ( 4.559911319644449179, 52.23035201082151247, -9.422509992056141925 ) ) ;
#25842 = CARTESIAN_POINT ( 'NONE',  ( 12.63842701281683034, 27.46726448433411250, 9.846743663894596210 ) ) ;
#25844 = CARTESIAN_POINT ( 'NONE',  ( 17.20831665107776587, 22.88393115100078745, 7.208316651077764980 ) ) ;
#25843 = CARTESIAN_POINT ( 'NONE',  ( 17.08211943468705840, 50.13708216824730357, -12.26659068614894466 ) ) ;
#25845 = DIRECTION ( 'NONE',  ( 0.000000000000000000, 0.000000000000000000, 1.000000000000000000 ) ) ;
#25846 = CARTESIAN_POINT ( 'NONE',  ( 1.472469842513823179, 51.42559781766745886, 4.923371831947296329 ) ) ;
#25848 = CARTESIAN_POINT ( 'NONE',  ( 24.16423886937410614, 4.512082168247300906, -3.795296366450302550 ) ) ;
#25847 = CARTESIAN_POINT ( 'NONE',  ( 0.1532563361054082862, 51.21726448433412315, 2.638427012816831674 ) ) ;
#25849 = CARTESIAN_POINT ( 'NONE',  ( -4.164238869374099927, 32.01208216824730357, 3.795296366450308767 ) ) ;
#25850 = CARTESIAN_POINT ( 'NONE',  ( 0.1532563361054100626, 25.80059781766744820, -2.638427012816831230 ) ) ;
#25851 = CARTESIAN_POINT ( 'NONE',  ( 10.00000000000000000, 26.81368534415484106, -10.88017736071110342 ) ) ;
#25852 = CARTESIAN_POINT ( 'NONE',  ( 15.44008868035555260, 39.73035201082150536, 9.422509992056143702 ) ) ;
#25853 = CARTESIAN_POINT ( 'NONE',  ( 17.96484262340118221, 44.93868534415483396, 7.964842623401181321 ) ) ;
#25854 = VERTEX_POINT ( 'NONE', #11131 ) ;
#25855 = CARTESIAN_POINT ( 'NONE',  ( 0.6178305044545838731, 34.74863466993042493, 9.382169495545420901 ) ) ;
#25856 = CARTESIAN_POINT ( 'NONE',  ( 15.44008868035555793, 56.39701867748817676, -9.422509992056140149 ) ) ;
#25857 = ORIENTED_EDGE ( 'NONE', *, *, #44829, .T. ) ;
#25858 = CARTESIAN_POINT ( 'NONE',  ( -28.94000000000001549, 93.50000000000000000, -10.09898361729590199 ) ) ;
#25859 = EDGE_CURVE ( 'NONE', #40989, #61441, #81966, .T. ) ;
#25860 = CARTESIAN_POINT ( 'NONE',  ( -0.8801773607111008646, 63.27201867748817676, 2.915334737309923430 ) ) ;
#25861 = EDGE_LOOP ( 'NONE', ( #97564, #77387, #20070, #92593 ) ) ;
#25862 = CARTESIAN_POINT ( 'NONE',  ( 7.084665262690076126, 59.10535201082150536, 10.88017736071109987 ) ) ;
#25863 = CARTESIAN_POINT ( 'NONE',  ( -11.35178980618980304, 0.5000000000000004441, 9.804941009311846756 ) ) ;
#25864 = CIRCLE ( 'NONE', #33818, 15.00000000000000000 ) ;
#25865 = CARTESIAN_POINT ( 'NONE',  ( 19.42250999205614193, 40.14701867748817676, 5.440088680355555262 ) ) ;
#25866 = CARTESIAN_POINT ( 'NONE',  ( -0.1503990784575328643, 70.00000000000000000, -6.262539305110068177 ) ) ;
#25867 = CARTESIAN_POINT ( 'NONE',  ( -2.266590686148945544, 67.22041550158063217, 7.082119434687048631 ) ) ;
#25868 = CARTESIAN_POINT ( 'NONE',  ( 0.1532563361054082862, 11.21726448433411605, 2.638427012816831674 ) ) ;
#25869 = CARTESIAN_POINT ( 'NONE',  ( -2.266590686148945544, 6.387082168247300906, -7.082119434687050408 ) ) ;
#25870 = CARTESIAN_POINT ( 'NONE',  ( 5.076628168052704559, 10.17559781766745175, -8.527530157486179263 ) ) ;
#25871 = CARTESIAN_POINT ( 'NONE',  ( 2.791683348922237240, 45.38393115100079456, -7.208316651077763204 ) ) ;
#25872 = VERTEX_POINT ( 'NONE', #49602 ) ;
#25873 = CARTESIAN_POINT ( 'NONE',  ( 18.52753015748618282, 53.92559781766745175, -4.923371831947291888 ) ) ;
#25874 = ORIENTED_EDGE ( 'NONE', *, *, #15606, .F. ) ;
#25875 = DIRECTION ( 'NONE',  ( -0.000000000000000000, -1.000000000000000000, -0.000000000000000000 ) ) ;
#25876 = CARTESIAN_POINT ( 'NONE',  ( 4.559911319644449179, 47.23035201082150536, -9.422509992056141925 ) ) ;
#25877 = CARTESIAN_POINT ( 'NONE',  ( 2.791683348922237240, 50.38393115100078035, -7.208316651077763204 ) ) ;
#25879 = CARTESIAN_POINT ( 'NONE',  ( 12.91533473730993009, 66.60535201082150536, -10.88017736071109987 ) ) ;
#25878 = FACE_OUTER_BOUND ( 'NONE', #53735, .T. ) ;
#25880 = CARTESIAN_POINT ( 'NONE',  ( 20.88017736071110164, 55.35535201082149825, 2.915334737309930979 ) ) ;
#25881 = CARTESIAN_POINT ( 'NONE',  ( 10.00000000000000178, 4.313685344154837509, 10.88017736071110342 ) ) ;
#25882 = CIRCLE ( 'NONE', #14761, 0.2500000000000002220 ) ;
#25883 = EDGE_CURVE ( 'NONE', #74605, #49327, #26616, .T. ) ;
#25884 = CARTESIAN_POINT ( 'NONE',  ( 10.00000000000000178, 45.37363466993041783, 12.81628187352647608 ) ) ;
#25885 = CARTESIAN_POINT ( 'NONE',  ( 0.1957200283969147692, 10.25733960839544068, 6.500000000000001776 ) ) ;
#25886 = ORIENTED_EDGE ( 'NONE', *, *, #59183, .T. ) ;
#25887 = CARTESIAN_POINT ( 'NONE',  ( 10.00000000000000000, 32.87363466993042493, -12.81628187352647608 ) ) ;
#25888 = CARTESIAN_POINT ( 'NONE',  ( 2.035157376598822676, 32.43868534415483396, -7.964842623401177768 ) ) ;
#25889 = EDGE_CURVE ( 'NONE', #80133, #11363, #96344, .T. ) ;
#25890 = EDGE_LOOP ( 'NONE', ( #32970, #59718, #37799, #34480, #8535, #23803 ) ) ;
#25891 = AXIS2_PLACEMENT_3D ( 'NONE', #82540, #30514, #91529 ) ;
#25892 = CARTESIAN_POINT ( 'NONE',  ( 19.84674366389459266, 58.71726448433411605, -2.638427012816827677 ) ) ;
#25894 = CARTESIAN_POINT ( 'NONE',  ( 2.791683348922240793, 56.63393115100078035, 7.208316651077764092 ) ) ;
#25893 = CARTESIAN_POINT ( 'NONE',  ( 14.92337183194729988, 14.34226448433411782, -8.527530157486177487 ) ) ;
#25895 = CARTESIAN_POINT ( 'NONE',  ( -10.94537820540292117, -97.33546231743453347, 3.750000000000000444 ) ) ;
#25896 = SURFACE_STYLE_FILL_AREA ( #64361 ) ;
#25897 = CARTESIAN_POINT ( 'NONE',  ( 19.84674366389459266, 38.71726448433412315, -2.638427012816827677 ) ) ;
#25898 = DIRECTION ( 'NONE',  ( 0.2503800040544389427, -0.000000000000000000, 0.9681476403781082984 ) ) ;
#25899 = CARTESIAN_POINT ( 'NONE',  ( 10.00000000000000178, 32.25893115100078745, 9.846743663894594434 ) ) ;
#25901 = ORIENTED_EDGE ( 'NONE', *, *, #624, .T. ) ;
#25900 = CARTESIAN_POINT ( 'NONE',  ( 19.84674366389459266, 58.30059781766745886, 2.638427012816836559 ) ) ;
#25902 = CARTESIAN_POINT ( 'NONE',  ( -0.8801773607111009756, 8.272018677488171434, 2.915334737309923874 ) ) ;
#25903 = CARTESIAN_POINT ( 'NONE',  ( 3.591859063236763294, 23.29030133659708568, -11.09922568453595026 ) ) ;
#25904 = CARTESIAN_POINT ( 'NONE',  ( 5.076628168052704559, 40.17559781766745175, -8.527530157486179263 ) ) ;
#25905 = CARTESIAN_POINT ( 'NONE',  ( -14.02068044289386783, 14.63606918466436113, 5.331089937175564231 ) ) ;
#25906 = CARTESIAN_POINT ( 'NONE',  ( 13.79529636645031943, 50.34541550158064638, -14.16423886937409904 ) ) ;
#25907 = CARTESIAN_POINT ( 'NONE',  ( 0.1532563361054083140, 21.00893115100078745, 1.131784320476157264E-15 ) ) ;
#25908 = ORIENTED_EDGE ( 'NONE', *, *, #12642, .T. ) ;
#25909 = CARTESIAN_POINT ( 'NONE',  ( 8.564643372776616914, 14.49999999999999822, -12.31449893000740836 ) ) ;
#25910 = CARTESIAN_POINT ( 'NONE',  ( 2.917880565312950480, 60.97041550158063927, -12.26659068614894821 ) ) ;
#25911 = CARTESIAN_POINT ( 'NONE',  ( 0.1532563361054082862, 56.21726448433411605, 2.638427012816831674 ) ) ;
#25912 = CARTESIAN_POINT ( 'NONE',  ( 2.035157376598822676, 7.438685344154837509, -7.964842623401177768 ) ) ;
#25913 = CARTESIAN_POINT ( 'NONE',  ( 13.79529636645030344, 33.26208216824730357, 14.16423886937410614 ) ) ;
#25915 = CARTESIAN_POINT ( 'NONE',  ( 19.84674366389459266, 33.71726448433410894, -2.638427012816827677 ) ) ;
#25914 = CARTESIAN_POINT ( 'NONE',  ( 22.26659068614894466, 43.88708216824729647, 7.082119434687054849 ) ) ;
#25916 = CARTESIAN_POINT ( 'NONE',  ( 6.000000000000000000, 11.50000000000000000, 6.500000000000000888 ) ) ;
#25918 = CARTESIAN_POINT ( 'NONE',  ( 2.791683348922237240, 50.38393115100078035, -7.208316651077763204 ) ) ;
#25917 = CARTESIAN_POINT ( 'NONE',  ( 6.829574850505125028, -88.00372650098201177, 2.500000000000000888 ) ) ;
#25919 = CARTESIAN_POINT ( 'NONE',  ( -0.8801773607110991993, 37.85535201082151247, -2.915334737309923874 ) ) ;
#25920 = CARTESIAN_POINT ( 'NONE',  ( -0.2838433074297238012, 13.12729635533385597, 10.00000000000000000 ) ) ;
#25921 = CARTESIAN_POINT ( 'NONE',  ( 9.730292033379889460, -19.64198355330689338, 3.750000000000001332 ) ) ;
#25922 = EDGE_CURVE ( 'NONE', #53414, #12692, #69370, .T. ) ;
#25923 = CARTESIAN_POINT ( 'NONE',  ( 0.1532563361054082862, 51.21726448433412315, 2.638427012816831674 ) ) ;
#25924 = CARTESIAN_POINT ( 'NONE',  ( -3.243710765982357636, 0.000000000000000000, 4.383623511354867830 ) ) ;
#25925 = CARTESIAN_POINT ( 'NONE',  ( 7.082119434687054849, 8.470415501580639273, 12.26659068614894288 ) ) ;
#25926 = CARTESIAN_POINT ( 'NONE',  ( 19.84674366389459266, 58.30059781766745886, 2.638427012816836559 ) ) ;
#25927 = CARTESIAN_POINT ( 'NONE',  ( 0.2751277870542967463, 70.00000000000000000, -6.500000000000000888 ) ) ;
#25928 = AXIS2_PLACEMENT_3D ( 'NONE', #65455, #6441, #52438 ) ;
#25929 = ORIENTED_EDGE ( 'NONE', *, *, #63531, .T. ) ;
#25930 = CARTESIAN_POINT ( 'NONE',  ( -2.266590686148945544, 32.22041550158063927, 7.082119434687048631 ) ) ;
#25931 = CARTESIAN_POINT ( 'NONE',  ( 0.5600000000000083800, 105.0000000000000000, 4.500000000000000888 ) ) ;
#25932 = FACE_OUTER_BOUND ( 'NONE', #24914, .T. ) ;
#25933 = CARTESIAN_POINT ( 'NONE',  ( 10.00000000000000178, 14.31368534415483929, 10.88017736071110342 ) ) ;
#25934 = CARTESIAN_POINT ( 'NONE',  ( 22.81628187352647785, 21.41530133659708923, 3.434112377981063169 ) ) ;
#25935 = CARTESIAN_POINT ( 'NONE',  ( -3.195792623639597707, 8.646642702460848540, -11.92686044187652961 ) ) ;
#25936 = CARTESIAN_POINT ( 'NONE',  ( 19.84674366389459266, 8.300597817667451750, 2.638427012816836559 ) ) ;
#25937 = CARTESIAN_POINT ( 'NONE',  ( 10.14667048435145169, 4.379817243679289018E-16, -10.35833375027041292 ) ) ;
#25938 = CARTESIAN_POINT ( 'NONE',  ( 34.56412365047464874, 29.50000000000000000, -10.00000000000000000 ) ) ;
#25939 = CARTESIAN_POINT ( 'NONE',  ( 0.000000000000000000, 0.000000000000000000, 0.000000000000000000 ) ) ;
#25940 = CARTESIAN_POINT ( 'NONE',  ( 19.42250999205614548, 10.98035201082150536, -5.440088680355545492 ) ) ;
#25941 = FACE_OUTER_BOUND ( 'NONE', #64131, .T. ) ;
#25942 = CARTESIAN_POINT ( 'NONE',  ( 10.00000000000000178, 44.31368534415484106, 10.88017736071110342 ) ) ;
#25943 = CARTESIAN_POINT ( 'NONE',  ( 12.91533473730993009, 36.60535201082151247, -10.88017736071109987 ) ) ;
#25944 = CARTESIAN_POINT ( 'NONE',  ( 18.52753015748618282, 63.92559781766745886, -4.923371831947291888 ) ) ;
#25945 = CARTESIAN_POINT ( 'NONE',  ( 1.472469842513823179, 66.42559781766745175, 4.923371831947296329 ) ) ;
#25946 = CARTESIAN_POINT ( 'NONE',  ( -1.099225684535947600, 58.70696800326375353, -6.408140936763238038 ) ) ;
#25947 = CARTESIAN_POINT ( 'NONE',  ( 1.472469842513823179, 16.42559781766745175, 4.923371831947296329 ) ) ;
#25948 = VERTEX_POINT ( 'NONE', #40658 ) ;
#25949 = CARTESIAN_POINT ( 'NONE',  ( 17.96484262340118221, 24.93868534415484461, 7.964842623401181321 ) ) ;
#25950 = CARTESIAN_POINT ( 'NONE',  ( 13.43411237798105340, 30.58196800326374998, 12.81628187352647963 ) ) ;
#25951 = VECTOR ( 'NONE', #6110, 999.9999999999998863 ) ;
#25952 = CARTESIAN_POINT ( 'NONE',  ( 12.63842701281683922, 64.55059781766745175, -9.846743663894590881 ) ) ;
#25953 = CARTESIAN_POINT ( 'NONE',  ( 2.035157376598824452, 68.68868534415484817, 7.964842623401179544 ) ) ;
#25954 = CARTESIAN_POINT ( 'NONE',  ( 14.92337183194729633, 7.675597817667451750, 8.527530157486181039 ) ) ;
#25955 = CARTESIAN_POINT ( 'NONE',  ( 21.09922568453594849, 36.20696800326375353, 6.408140936763242479 ) ) ;
#25957 = CARTESIAN_POINT ( 'NONE',  ( -5.817157072110620497, 14.49999999999999112, -13.82608706751101302 ) ) ;
#25956 = CARTESIAN_POINT ( 'NONE',  ( 7.361572987183170547, 12.05059781766744997, 9.846743663894590881 ) ) ;
#25958 = MECHANICAL_DESIGN_GEOMETRIC_PRESENTATION_REPRESENTATION (  '', ( #86627 ), #38739 ) ;
#25959 = ORIENTED_EDGE ( 'NONE', *, *, #78614, .F. ) ;
#25960 = CARTESIAN_POINT ( 'NONE',  ( 0.2751277870542967463, 70.00000000000000000, 6.000000000000000000 ) ) ;
#25961 = CARTESIAN_POINT ( 'NONE',  ( -0.8801773607110991993, 12.85535201082150358, -2.915334737309923874 ) ) ;
#25963 = CARTESIAN_POINT ( 'NONE',  ( 24.16423886937410614, 24.30374883491396787, 8.672049930838204340E-16 ) ) ;
#25962 = CARTESIAN_POINT ( 'NONE',  ( 13.43411237798105340, 60.58196800326376064, 12.81628187352647963 ) ) ;
#25964 = CARTESIAN_POINT ( 'NONE',  ( 18.52753015748618282, 13.92559781766745175, -4.923371831947291888 ) ) ;
#25965 = AXIS2_PLACEMENT_3D ( 'NONE', #9390, #2410, #62375 ) ;
#25966 = CARTESIAN_POINT ( 'NONE',  ( 15.44008868035555260, 4.730352010821504471, 9.422509992056143702 ) ) ;
#25967 = CARTESIAN_POINT ( 'NONE',  ( 7.361572987183169658, 14.96726448433411960, -9.846743663894592657 ) ) ;
#25968 = CARTESIAN_POINT ( 'NONE',  ( 24.16423886937409904, 59.09541550158063217, 3.795296366450317205 ) ) ;
#25969 = ORIENTED_EDGE ( 'NONE', *, *, #20438, .F. ) ;
#25970 = AXIS2_PLACEMENT_3D ( 'NONE', #87771, #25815, #86807 ) ;
#25971 = CARTESIAN_POINT ( 'NONE',  ( 17.96484262340118221, 19.93868534415484106, 7.964842623401181321 ) ) ;
#25972 = ADVANCED_FACE ( 'NONE', ( #2187 ), #64112, .T. ) ;
#25973 = CARTESIAN_POINT ( 'NONE',  ( 20.88017736071110875, 25.77201867748816966, -2.915334737309920765 ) ) ;
#25974 = CARTESIAN_POINT ( 'NONE',  ( -0.04068437667224622523, 7.219743609177202259, -6.396802510829698640 ) ) ;
#25975 = MECHANICAL_DESIGN_GEOMETRIC_PRESENTATION_REPRESENTATION (  '', ( #11545 ), #86639 ) ;
#25976 = ORIENTED_EDGE ( 'NONE', *, *, #9159, .T. ) ;
#25977 = CARTESIAN_POINT ( 'NONE',  ( 12.63842701281683922, 64.55059781766745175, -9.846743663894590881 ) ) ;
#25978 = CARTESIAN_POINT ( 'NONE',  ( 0.5774900079438607392, 18.48035201082150536, 5.440088680355550821 ) ) ;
#25979 = CARTESIAN_POINT ( 'NONE',  ( 5.076628168052703671, 61.84226448433412315, 8.527530157486179263 ) ) ;
#25980 = LINE ( 'NONE', #57451, #48889 ) ;
#25981 = CARTESIAN_POINT ( 'NONE',  ( 16.40814093676323893, 45.79030133659708923, 11.09922568453595026 ) ) ;
#25982 = CARTESIAN_POINT ( 'NONE',  ( 19.72487221294571924, 62.80223176428831522, -6.499999999999984901 ) ) ;
#25983 = CARTESIAN_POINT ( 'NONE',  ( 20.36894250292379738, 19.92874883491396787, -10.36894250292379027 ) ) ;
#25984 = CARTESIAN_POINT ( 'NONE',  ( -0.8801773607111008646, 43.27201867748817676, 2.915334737309923430 ) ) ;
#25985 = CARTESIAN_POINT ( 'NONE',  ( 2.035157376598824452, 18.68868534415484106, 7.964842623401179544 ) ) ;
#25986 = ADVANCED_FACE ( 'NONE', ( #63141 ), #17666, .F. ) ;
#25987 = CARTESIAN_POINT ( 'NONE',  ( 5.076628168052704559, 60.17559781766745175, -8.527530157486179263 ) ) ;
#25988 = CARTESIAN_POINT ( 'NONE',  ( -8.160079337347118766, -4.177753580735825700, -3.750000000000000444 ) ) ;
#25989 = CARTESIAN_POINT ( 'NONE',  ( 17.20831665107776587, 32.88393115100078745, 7.208316651077764980 ) ) ;
#25990 = DIRECTION ( 'NONE',  ( 0.000000000000000000, -1.000000000000000000, 0.000000000000000000 ) ) ;
#25991 = MECHANICAL_DESIGN_GEOMETRIC_PRESENTATION_REPRESENTATION (  '', ( #67533 ), #73860 ) ;
#25992 = CARTESIAN_POINT ( 'NONE',  ( 0.1532563361054100626, 5.800597817667452638, -2.638427012816831230 ) ) ;
#25993 = CARTESIAN_POINT ( 'NONE',  ( 12.81628187352647608, -33.58469866340291077, 3.434112377981052511 ) ) ;
#25994 = ORIENTED_EDGE ( 'NONE', *, *, #53507, .F. ) ;
#25995 = CARTESIAN_POINT ( 'NONE',  ( 20.88017736071110875, 10.77201867748817143, -2.915334737309920765 ) ) ;
#25996 = CARTESIAN_POINT ( 'NONE',  ( 17.20831665107776587, 17.88393115100078745, 7.208316651077764980 ) ) ;
#25997 = CARTESIAN_POINT ( 'NONE',  ( 0.1532563361054083140, 66.00893115100079456, 1.131784320476157264E-15 ) ) ;
#25998 = CARTESIAN_POINT ( 'NONE',  ( 20.88017736071110519, 40.56368534415484106, 2.639326808657452039E-16 ) ) ;
#26000 = CARTESIAN_POINT ( 'NONE',  ( 21.09922568453595559, 47.04030133659708923, -6.408140936763230044 ) ) ;
#25999 = CARTESIAN_POINT ( 'NONE',  ( 10.00000000000000000, 16.81368534415483751, -10.88017736071110342 ) ) ;
#26001 = CARTESIAN_POINT ( 'NONE',  ( -4.164238869374098151, 36.59541550158063217, -3.795296366450310543 ) ) ;
#26003 = CARTESIAN_POINT ( 'NONE',  ( 6.000000000000000000, 60.50000000000000000, -6.000000000000000000 ) ) ;
#26002 = B_SPLINE_CURVE_WITH_KNOTS ( 'NONE', 3,
 ( #10725, #26218, #9246, #86728, #24266, #17257 ),
 .UNSPECIFIED., .F., .F.,
 ( 4, 2, 4 ),
 ( 0.0002800630492131283558, 0.0006862688956284094047, 0.001092474742043690345 ),
 .UNSPECIFIED. ) ;
#26004 = AXIS2_PLACEMENT_3D ( 'NONE', #53187, #37703, #83194 ) ;
#26005 = CARTESIAN_POINT ( 'NONE',  ( -2.816281873526473856, 59.12363466993042493, 9.499525473075851096E-16 ) ) ;
#26006 = ORIENTED_EDGE ( 'NONE', *, *, #40925, .F. ) ;
#26007 = CARTESIAN_POINT ( 'NONE',  ( 12.63842701281683034, 62.46726448433410894, 9.846743663894596210 ) ) ;
#26008 = CARTESIAN_POINT ( 'NONE',  ( 10.00000000000000000, 31.81368534415483751, -10.88017736071110342 ) ) ;
#26009 = ADVANCED_FACE ( 'NONE', ( #93644 ), #97926, .T. ) ;
#26010 = B_SPLINE_CURVE_WITH_KNOTS ( 'NONE', 3,
 ( #17919, #86418, #39445, #1456, #92915, #77917 ),
 .UNSPECIFIED., .F., .F.,
 ( 4, 2, 4 ),
 ( 0.0002800715030460633101, 0.0006862774322447769745, 0.001092483361443490585 ),
 .UNSPECIFIED. ) ;
#26011 = EDGE_LOOP ( 'NONE', ( #63931, #72837 ) ) ;
#26013 = CARTESIAN_POINT ( 'NONE',  ( -45.94000000000001194, 100.9999999999999858, -9.500000000000000000 ) ) ;
#26012 = CARTESIAN_POINT ( 'NONE',  ( 0.5774900079438607392, 68.48035201082150536, 5.440088680355550821 ) ) ;
#26014 = CARTESIAN_POINT ( 'NONE',  ( 18.52753015748618282, 28.92559781766745175, -4.923371831947291888 ) ) ;
#26015 = CARTESIAN_POINT ( 'NONE',  ( 18.52753015748618282, 13.92559781766745175, -4.923371831947291888 ) ) ;
#26016 = CARTESIAN_POINT ( 'NONE',  ( 5.076628168052703671, 6.842264484334118713, 8.527530157486179263 ) ) ;
#26018 = CARTESIAN_POINT ( 'NONE',  ( -4.862001128006864903, 4.306586084822671512E-16, 13.66056166602457012 ) ) ;
#26017 = CARTESIAN_POINT ( 'NONE',  ( 2.035157376598822676, 62.43868534415483396, -7.964842623401177768 ) ) ;
#26019 = CARTESIAN_POINT ( 'NONE',  ( 17.96484262340118221, 61.18868534415482685, -7.964842623401177768 ) ) ;
#26022 = ORIENTED_EDGE ( 'NONE', *, *, #18669, .F. ) ;
#26021 =( GEOMETRIC_REPRESENTATION_CONTEXT ( 3 ) GLOBAL_UNCERTAINTY_ASSIGNED_CONTEXT ( ( #293 ) ) GLOBAL_UNIT_ASSIGNED_CONTEXT ( ( #85346, #84860, #93826 ) ) REPRESENTATION_CONTEXT ( 'NONE', 'WORKASPACE' ) );
#26020 = CARTESIAN_POINT ( 'NONE',  ( 19.84674366389459621, 18.50893115100078745, 7.409399052514197653E-17 ) ) ;
#26023 = CARTESIAN_POINT ( 'NONE',  ( -15.99538290524656503, 15.00000000000000000, -0.1584996864330918964 ) ) ;
#26024 = CARTESIAN_POINT ( 'NONE',  ( 0.1532563361054083140, 56.00893115100078745, 1.131784320476157264E-15 ) ) ;
#26025 = ORIENTED_EDGE ( 'NONE', *, *, #16399, .F. ) ;
#26026 = ORIENTED_EDGE ( 'NONE', *, *, #27106, .F. ) ;
#26027 = DIRECTION ( 'NONE',  ( 1.000000000000000000, 0.000000000000000000, 0.000000000000000000 ) ) ;
#26028 = CIRCLE ( 'NONE', #77123, 6.599999999999995204 ) ;
#26029 = CARTESIAN_POINT ( 'NONE',  ( -2.266590686148945544, 2.220415501580634388, 7.082119434687048631 ) ) ;
#26030 = MECHANICAL_DESIGN_GEOMETRIC_PRESENTATION_REPRESENTATION (  '', ( #70717 ), #64252 ) ;
#26031 = CARTESIAN_POINT ( 'NONE',  ( 3.591859063236763294, 63.29030133659708923, -11.09922568453595026 ) ) ;
#26032 = CARTESIAN_POINT ( 'NONE',  ( 24.16423886937409904, 4.095415501580634832, 3.795296366450317205 ) ) ;
#26033 = CARTESIAN_POINT ( 'NONE',  ( 6.204703633549690345, 37.84541550158063927, 14.16423886937410082 ) ) ;
#26034 = CARTESIAN_POINT ( 'NONE',  ( 0.000000000000000000, 14.49999999999999822, 0.000000000000000000 ) ) ;
#26035 =( LENGTH_UNIT ( ) NAMED_UNIT ( * ) SI_UNIT ( .MILLI., .METRE. ) );
#26036 = CARTESIAN_POINT ( 'NONE',  ( 7.084665262690076126, 29.10535201082150181, 10.88017736071109987 ) ) ;
#26037 = ORIENTED_EDGE ( 'NONE', *, *, #94333, .T. ) ;
#26039 = AXIS2_PLACEMENT_3D ( 'NONE', #90310, #23824, #75817 ) ;
#26038 = CARTESIAN_POINT ( 'NONE',  ( 1.472469842513823179, 20.59226448433411960, -4.923371831947296329 ) ) ;
#26041 = CARTESIAN_POINT ( 'NONE',  ( 5.076628168052704559, 10.17559781766745175, -8.527530157486179263 ) ) ;
#26040 = CARTESIAN_POINT ( 'NONE',  ( -0.8801773607111009756, 58.06368534415484106, 1.068504757029289695E-15 ) ) ;
#26042 = CARTESIAN_POINT ( 'NONE',  ( -2.816281873526473856, 39.33196800326374643, 3.434112377981055619 ) ) ;
#26043 = CARTESIAN_POINT ( 'NONE',  ( 12.63842701281683034, 37.46726448433411605, 9.846743663894596210 ) ) ;
#26044 = DIRECTION ( 'NONE',  ( 0.000000000000000000, -0.000000000000000000, -1.000000000000000000 ) ) ;
#26045 = EDGE_CURVE ( 'NONE', #67764, #5928, #30872, .T. ) ;
#26046 = CARTESIAN_POINT ( 'NONE',  ( 0.5774900079438590739, 57.64701867748817676, -5.440088680355550821 ) ) ;
#26047 = CARTESIAN_POINT ( 'NONE',  ( 6.565887622018943937, 23.08196800326375708, -12.81628187352647608 ) ) ;
#26048 = CARTESIAN_POINT ( 'NONE',  ( -10.36894250292378317, -37.57125116508602503, 10.36894250292379560 ) ) ;
#26049 = CARTESIAN_POINT ( 'NONE',  ( 12.63842701281683034, 27.46726448433411250, 9.846743663894596210 ) ) ;
#26050 = CARTESIAN_POINT ( 'NONE',  ( 22.26659068614895176, 9.720415501580633943, -7.082119434687042414 ) ) ;
#26051 = VERTEX_POINT ( 'NONE', #18154 ) ;
#26052 = CARTESIAN_POINT ( 'NONE',  ( 2.035157376598822676, 37.43868534415484106, -7.964842623401177768 ) ) ;
#26053 = CARTESIAN_POINT ( 'NONE',  ( 13.79529636645030344, 33.26208216824730357, 14.16423886937410614 ) ) ;
#26054 = CARTESIAN_POINT ( 'NONE',  ( 5.076628168052704559, 55.17559781766745175, -8.527530157486179263 ) ) ;
#26055 = CARTESIAN_POINT ( 'NONE',  ( 17.20831665107776587, 9.133931151000787452, -7.208316651077762316 ) ) ;
#26057 = DIRECTION ( 'NONE',  ( 0.9890158633619168249, 0.000000000000000000, 0.1478094111296113511 ) ) ;
#26056 = CARTESIAN_POINT ( 'NONE',  ( 3.591859063236761518, 64.95696800326376774, 11.09922568453594849 ) ) ;
#26058 = CARTESIAN_POINT ( 'NONE',  ( 15.44008868035555260, 44.73035201082151247, 9.422509992056143702 ) ) ;
#26059 = DIRECTION ( 'NONE',  ( -0.000000000000000000, 0.000000000000000000, 1.000000000000000000 ) ) ;
#26060 = CARTESIAN_POINT ( 'NONE',  ( 22.81628187352647785, 26.62363466993042138, 6.195893100308588602E-16 ) ) ;
#26061 = CARTESIAN_POINT ( 'NONE',  ( 19.84674366389459621, 58.50893115100078745, 7.409399052514197653E-17 ) ) ;
#26062 = CARTESIAN_POINT ( 'NONE',  ( -7.964842623401179544, 12.43868534415484639, -7.964842623401174215 ) ) ;
#26063 = SURFACE_STYLE_FILL_AREA ( #58510 ) ;
#26065 = DIRECTION ( 'NONE',  ( -0.000000000000000000, -1.000000000000000000, -0.000000000000000000 ) ) ;
#26064 = CARTESIAN_POINT ( 'NONE',  ( 0.5774900079438590739, 62.64701867748817676, -5.440088680355550821 ) ) ;
#26066 = CIRCLE ( 'NONE', #81938, 9.999999999999998224 ) ;
#26067 = CARTESIAN_POINT ( 'NONE',  ( -8.081444665946364125, -7.288330178564340400, 4.000000000000000000 ) ) ;
#26068 = DIRECTION ( 'NONE',  ( 0.6087614290087297597, 0.000000000000000000, -0.7933533402912281707 ) ) ;
#26069 = CARTESIAN_POINT ( 'NONE',  ( 0.5774900079438590739, 47.64701867748817676, -5.440088680355550821 ) ) ;
#26071 = CARTESIAN_POINT ( 'NONE',  ( 17.96484262340118221, 59.93868534415484106, 7.964842623401181321 ) ) ;
#26070 = AXIS2_PLACEMENT_3D ( 'NONE', #77401, #75939, #53426 ) ;
#26072 = DIRECTION ( 'NONE',  ( 0.000000000000000000, 1.000000000000000000, 0.000000000000000000 ) ) ;
#26073 = CARTESIAN_POINT ( 'NONE',  ( 0.2751277870542914172, 58.21833443783938833, 6.499999999999992006 ) ) ;
#26074 = CARTESIAN_POINT ( 'NONE',  ( 5.076628168052703671, 21.84226448433411960, 8.527530157486179263 ) ) ;
#26075 = CARTESIAN_POINT ( 'NONE',  ( 7.084665262690076126, 29.10535201082150181, 10.88017736071109987 ) ) ;
#26076 = CARTESIAN_POINT ( 'NONE',  ( 2.791683348922237240, 60.38393115100078745, -7.208316651077763204 ) ) ;
#26078 = CARTESIAN_POINT ( 'NONE',  ( 0.2751277870542967463, 70.00000000000000000, 6.000000000000000000 ) ) ;
#26077 = CARTESIAN_POINT ( 'NONE',  ( 19.42250999205614548, 15.98035201082150714, -5.440088680355545492 ) ) ;
#26079 = DIRECTION ( 'NONE',  ( 1.000000000000000000, 0.000000000000000000, 0.000000000000000000 ) ) ;
#26080 = CARTESIAN_POINT ( 'NONE',  ( 13.43411237798106583, 27.66530133659708568, -12.81628187352647252 ) ) ;
#26081 = ORIENTED_EDGE ( 'NONE', *, *, #88312, .T. ) ;
#26082 = CARTESIAN_POINT ( 'NONE',  ( 19.42250999205614548, 55.98035201082150536, -5.440088680355545492 ) ) ;
#26083 = CARTESIAN_POINT ( 'NONE',  ( 12.63842701281683034, 47.46726448433412315, 9.846743663894596210 ) ) ;
#26085 =( NAMED_UNIT ( * ) PLANE_ANGLE_UNIT ( ) SI_UNIT ( $, .RADIAN. ) );
#26084 = CARTESIAN_POINT ( 'NONE',  ( 22.81628187352647785, 26.62363466993042138, 6.195893100308588602E-16 ) ) ;
#26086 = CARTESIAN_POINT ( 'NONE',  ( -0.8801773607111009756, 33.06368534415484106, 1.068504757029289695E-15 ) ) ;
#26087 = CARTESIAN_POINT ( 'NONE',  ( -4.164238869374099927, 47.01208216824729647, 3.795296366450308767 ) ) ;
#26088 = CARTESIAN_POINT ( 'NONE',  ( 12.63842701281683034, 37.46726448433411605, 9.846743663894596210 ) ) ;
#26089 = CARTESIAN_POINT ( 'NONE',  ( 14.92337183194729988, 4.342264484334117824, -8.527530157486177487 ) ) ;
#26090 = CARTESIAN_POINT ( 'NONE',  ( 4.559911319644449179, 52.23035201082151247, -9.422509992056141925 ) ) ;
#26091 = CARTESIAN_POINT ( 'NONE',  ( -2.266590686148945544, 21.38708216824730357, -7.082119434687050408 ) ) ;
#26092 = DIRECTION ( 'NONE',  ( -0.000000000000000000, 0.000000000000000000, 1.000000000000000000 ) ) ;
#26093 = CARTESIAN_POINT ( 'NONE',  ( 1.383448333479231795, 22.37718327197428891, -6.499999999999977796 ) ) ;
#26095 = EDGE_LOOP ( 'NONE', ( #3148, #39189, #73184, #23903 ) ) ;
#26094 = EDGE_CURVE ( 'NONE', #91043, #91555, #87231, .T. ) ;
#26096 = CARTESIAN_POINT ( 'NONE',  ( 2.917880565312950480, 50.97041550158064638, -12.26659068614894821 ) ) ;
#26097 = CARTESIAN_POINT ( 'NONE',  ( -0.3689425029237898834, 56.17874883491396076, -10.36894250292378850 ) ) ;
#26098 = CARTESIAN_POINT ( 'NONE',  ( 1.472469842513823179, 10.59226448433411782, -4.923371831947296329 ) ) ;
#26099 = CARTESIAN_POINT ( 'NONE',  ( 3.772706337463130544E-18, 0.2999999999999981570, 0.000000000000000000 ) ) ;
#26101 = DIRECTION ( 'NONE',  ( -0.000000000000000000, 0.000000000000000000, 1.000000000000000000 ) ) ;
#26100 = AXIS2_PLACEMENT_3D ( 'NONE', #13389, #24844, #24359 ) ;
#26102 = CARTESIAN_POINT ( 'NONE',  ( 6.565887622018943937, 30.16530133659708568, 12.81628187352647430 ) ) ;
#26103 = CARTESIAN_POINT ( 'NONE',  ( 10.00000000000000178, 38.05374883491396787, 14.16423886937410082 ) ) ;
#26104 = EDGE_CURVE ( 'NONE', #31822, #83562, #78654, .T. ) ;
#26105 = ADVANCED_FACE ( 'NONE', ( #32143 ), #85187, .T. ) ;
#26106 = AXIS2_PLACEMENT_3D ( 'NONE', #80362, #91685, #23204 ) ;
#26107 = CARTESIAN_POINT ( 'NONE',  ( 7.084665262690076126, 67.02201867748817676, -10.88017736071110164 ) ) ;
#26108 = STYLED_ITEM ( 'NONE', ( #72425 ), #93637 ) ;
#26109 = CARTESIAN_POINT ( 'NONE',  ( -8.527530157486173934, 6.425597817667459744, 4.923371831947302546 ) ) ;
#26110 = VERTEX_POINT ( 'NONE', #55144 ) ;
#26111 = SURFACE_STYLE_USAGE ( .BOTH. , #680 ) ;
#26112 = CARTESIAN_POINT ( 'NONE',  ( 17.20831665107776587, 19.13393115100078035, -7.208316651077762316 ) ) ;
#26113 = SURFACE_STYLE_FILL_AREA ( #79103 ) ;
#26114 = B_SPLINE_CURVE_WITH_KNOTS ( 'NONE', 3,
 ( #65712, #50216, #79253, #71753, #58711, #11242 ),
 .UNSPECIFIED., .F., .F.,
 ( 4, 2, 4 ),
 ( 0.000000000000000000, 0.0002565770811491099672, 0.0005131541622982199345 ),
 .UNSPECIFIED. ) ;
#26115 = ORIENTED_EDGE ( 'NONE', *, *, #3962, .F. ) ;
#26117 = CARTESIAN_POINT ( 'NONE',  ( 12.91533473730993009, 16.60535201082150891, -10.88017736071109987 ) ) ;
#26116 = CARTESIAN_POINT ( 'NONE',  ( 0.5774900079438590739, 2.647018677488171434, -5.440088680355550821 ) ) ;
#26119 = CARTESIAN_POINT ( 'NONE',  ( 6.565887622018943937, 5.165301336597086568, 12.81628187352647430 ) ) ;
#26118 = CARTESIAN_POINT ( 'NONE',  ( 2.791683348922237240, 45.38393115100079456, -7.208316651077763204 ) ) ;
#26120 = EDGE_CURVE ( 'NONE', #3454, #74236, #95567, .T. ) ;
#26121 = DIRECTION ( 'NONE',  ( -0.000000000000000000, 0.000000000000000000, 1.000000000000000000 ) ) ;
#26122 = DIRECTION ( 'NONE',  ( 0.000000000000000000, 0.000000000000000000, 1.000000000000000000 ) ) ;
#26123 = CARTESIAN_POINT ( 'NONE',  ( 13.43411237798106583, 22.66530133659708923, -12.81628187352647252 ) ) ;
#26124 = EDGE_LOOP ( 'NONE', ( #70241, #36701, #32318, #88098 ) ) ;
#26125 = CARTESIAN_POINT ( 'NONE',  ( -2.266590686148945544, 61.38708216824730357, -7.082119434687050408 ) ) ;
#26126 = ORIENTED_EDGE ( 'NONE', *, *, #36189, .F. ) ;
#26127 = ADVANCED_FACE ( 'NONE', ( #81098 ), #67089, .T. ) ;
#26128 = CARTESIAN_POINT ( 'NONE',  ( 2.917880565312948704, 52.63708216824730357, 12.26659068614894643 ) ) ;
#26129 = EDGE_LOOP ( 'NONE', ( #96139, #33402, #48277, #31825 ) ) ;
#26130 = CARTESIAN_POINT ( 'NONE',  ( -0.8801773607110991993, 37.85535201082151247, -2.915334737309923874 ) ) ;
#26131 = CARTESIAN_POINT ( 'NONE',  ( 0.5774900079438607392, 33.48035201082150536, 5.440088680355550821 ) ) ;
#26132 = CARTESIAN_POINT ( 'NONE',  ( 19.72487221294570858, 5.718334437839381224, -6.500000000000000888 ) ) ;
#26133 = CARTESIAN_POINT ( 'NONE',  ( 2.035157376598822676, 22.43868534415483396, -7.964842623401177768 ) ) ;
#26134 = CYLINDRICAL_SURFACE ( 'NONE', #28074, 11.92686044187656513 ) ;
#26135 = CARTESIAN_POINT ( 'NONE',  ( 19.84674366389459266, 13.71726448433411782, -2.638427012816827677 ) ) ;
#26136 = EDGE_LOOP ( 'NONE', ( #58298, #22586, #11331, #55112 ) ) ;
#26137 = CARTESIAN_POINT ( 'NONE',  ( 11.43665280331135392, -81.62088987012758423, 4.000000000000000000 ) ) ;
#26138 = CARTESIAN_POINT ( 'NONE',  ( 1.472469842513823179, 45.59226448433412315, -4.923371831947296329 ) ) ;
#26139 = CARTESIAN_POINT ( 'NONE',  ( 18.72515096720570327, 11.07228050351031712, -6.499999999999992006 ) ) ;
#26140 = CARTESIAN_POINT ( 'NONE',  ( 21.09922568453594849, 51.20696800326375353, 6.408140936763242479 ) ) ;
#26141 = CARTESIAN_POINT ( 'NONE',  ( -7.118731320094870973, -71.92838106472885329, 3.750000000000000444 ) ) ;
#26142 = ORIENTED_EDGE ( 'NONE', *, *, #205, .F. ) ;
#26143 = CARTESIAN_POINT ( 'NONE',  ( -46.59701958359877239, 103.7651961684614577, 6.068442458532170569 ) ) ;
#26144 = CARTESIAN_POINT ( 'NONE',  ( -0.8801773607111009756, 53.27201867748818387, 2.915334737309923874 ) ) ;
#26145 = CARTESIAN_POINT ( 'NONE',  ( 19.84674366389459621, 63.50893115100078745, 7.409399052514197653E-17 ) ) ;
#26146 = CARTESIAN_POINT ( 'NONE',  ( -4.164238869374098151, 41.59541550158061796, -3.795296366450310543 ) ) ;
#26147 = CARTESIAN_POINT ( 'NONE',  ( 13.99999999999999822, 10.49999999999999822, 6.000000000000000000 ) ) ;
#26148 = VERTEX_POINT ( 'NONE', #73588 ) ;
#26149 = CARTESIAN_POINT ( 'NONE',  ( -13.14228782657329653, 15.00000000000000000, -7.230509711182418364 ) ) ;
#26150 = CARTESIAN_POINT ( 'NONE',  ( 14.92337183194729633, 37.67559781766745175, 8.527530157486181039 ) ) ;
#26151 = CARTESIAN_POINT ( 'NONE',  ( 10.00000000000000178, 60.37363466993041783, 12.81628187352647608 ) ) ;
#26152 = CARTESIAN_POINT ( 'NONE',  ( -2.816281873526471635, -1.084698663402913210, -3.434112377981056508 ) ) ;
#26153 = CARTESIAN_POINT ( 'NONE',  ( 1.472469842513823179, 0.5922644843341181575, -4.923371831947296329 ) ) ;
#26154 = CARTESIAN_POINT ( 'NONE',  ( 0.1955144967548901602, 4.327036817733407759, -6.500000000002763123 ) ) ;
#26155 = CARTESIAN_POINT ( 'NONE',  ( 7.361572987183170547, 62.05059781766745886, 9.846743663894590881 ) ) ;
#26156 = CARTESIAN_POINT ( 'NONE',  ( 7.684764310694878198, 0.5000000000000004441, -12.88194075009934991 ) ) ;
#26157 = EDGE_LOOP ( 'NONE', ( #6727, #23670, #16162, #81668 ) ) ;
#26158 = CARTESIAN_POINT ( 'NONE',  ( 20.36894250292379382, 63.67874883491396787, 10.36894250292379205 ) ) ;
#26159 = DIRECTION ( 'NONE',  ( 0.000000000000000000, -0.000000000000000000, -1.000000000000000000 ) ) ;
#26160 = CARTESIAN_POINT ( 'NONE',  ( 4.559911319644449179, 37.23035201082150536, -9.422509992056141925 ) ) ;
#26162 = CARTESIAN_POINT ( 'NONE',  ( 0.5774900079438590739, 67.64701867748817676, -5.440088680355550821 ) ) ;
#26161 = CARTESIAN_POINT ( 'NONE',  ( -1.099225684535947600, 19.54030133659708568, 6.408140936763237150 ) ) ;
#26163 = CARTESIAN_POINT ( 'NONE',  ( -0.8801773607110991993, 2.855352010821504471, -2.915334737309923874 ) ) ;
#26164 = AXIS2_PLACEMENT_3D ( 'NONE', #71182, #24211, #93174 ) ;
#26165 = CARTESIAN_POINT ( 'NONE',  ( 13.61464873478163007, 14.63595249122790598, 6.296136897217930795 ) ) ;
#26166 = CARTESIAN_POINT ( 'NONE',  ( 0.000000000000000000, 15.00000000000000000, 0.000000000000000000 ) ) ;
#26167 = CARTESIAN_POINT ( 'NONE',  ( 17.20831665107776587, 57.88393115100078745, 7.208316651077764980 ) ) ;
#26168 = PRESENTATION_STYLE_ASSIGNMENT (( #55688 ) ) ;
#26169 = CARTESIAN_POINT ( 'NONE',  ( -10.88017736071110164, -32.14464798917849464, -2.915334737309917212 ) ) ;
#26170 = CARTESIAN_POINT ( 'NONE',  ( 19.38216949554541557, 27.24863466993041783, -9.382169495545420901 ) ) ;
#26171 = CARTESIAN_POINT ( 'NONE',  ( -7.858204384621390481, -3.138042374757826991, -4.000000000000000000 ) ) ;
#26173 = CARTESIAN_POINT ( 'NONE',  ( 8.564643372776533425, 0.3640475087720987379, 12.31449893000747053 ) ) ;
#26172 = CARTESIAN_POINT ( 'NONE',  ( 19.42250999205614548, 20.98035201082150891, -5.440088680355545492 ) ) ;
#26174 = EDGE_CURVE ( 'NONE', #74650, #63206, #67575, .T. ) ;
#26175 = CARTESIAN_POINT ( 'NONE',  ( 13.79529636645031943, 40.34541550158063217, -14.16423886937409904 ) ) ;
#26176 = CARTESIAN_POINT ( 'NONE',  ( 24.16423886937409904, 24.09541550158063927, 3.795296366450317205 ) ) ;
#26177 = B_SPLINE_CURVE_WITH_KNOTS ( 'NONE', 3,
 ( #91967, #1975, #16471, #84958, #68981, #2475 ),
 .UNSPECIFIED., .F., .F.,
 ( 4, 2, 4 ),
 ( 0.000000000000000000, 0.0002701661927229442807, 0.0005403323854458885614 ),
 .UNSPECIFIED. ) ;
#26178 = CARTESIAN_POINT ( 'NONE',  ( 10.00000000000000000, 16.81368534415483751, -10.88017736071110342 ) ) ;
#26179 = CARTESIAN_POINT ( 'NONE',  ( 1.472469842513823179, 40.59226448433411605, -4.923371831947296329 ) ) ;
#26180 = CARTESIAN_POINT ( 'NONE',  ( 16.40814093676323893, 40.79030133659708923, 11.09922568453595026 ) ) ;
#26181 = CARTESIAN_POINT ( 'NONE',  ( -0.8801773607110991993, 12.85535201082150358, -2.915334737309923874 ) ) ;
#26182 = CARTESIAN_POINT ( 'NONE',  ( 17.20831665107776587, 32.88393115100078745, 7.208316651077764980 ) ) ;
#26183 = CARTESIAN_POINT ( 'NONE',  ( -0.8801773607111008646, 38.27201867748816255, 2.915334737309923430 ) ) ;
#26184 = CARTESIAN_POINT ( 'NONE',  ( -2.816281873526471635, 8.915301336597083903, -3.434112377981056508 ) ) ;
#26185 = CARTESIAN_POINT ( 'NONE',  ( 13.79529636645030344, 23.26208216824730002, 14.16423886937410614 ) ) ;
#26186 = DIRECTION ( 'NONE',  ( 0.000000000000000000, 0.000000000000000000, 1.000000000000000000 ) ) ;
#26187 = UNCERTAINTY_MEASURE_WITH_UNIT (LENGTH_MEASURE( 1.000000000000000082E-05 ), #59311, 'distance_accuracy_value', 'NONE');
#26188 = CARTESIAN_POINT ( 'NONE',  ( 10.00000000000000000, 24.75893115100078745, -9.846743663894594434 ) ) ;
#26189 = CARTESIAN_POINT ( 'NONE',  ( 21.09922568453594849, 46.20696800326376064, 6.408140936763242479 ) ) ;
#26190 = CARTESIAN_POINT ( 'NONE',  ( 2.791683348922237240, 50.38393115100078035, -7.208316651077763204 ) ) ;
#26191 = ORIENTED_EDGE ( 'NONE', *, *, #21699, .F. ) ;
#26192 = CARTESIAN_POINT ( 'NONE',  ( 10.00000000000000178, 70.00000000000000000, 0.000000000000000000 ) ) ;
#26193 = CARTESIAN_POINT ( 'NONE',  ( 6.673414917871782315, -55.62670566514463388, 2.750000000000000000 ) ) ;
#26194 = CARTESIAN_POINT ( 'NONE',  ( 10.00000000000000178, 63.05374883491396076, 14.16423886937410082 ) ) ;
#26195 = CARTESIAN_POINT ( 'NONE',  ( -4.164238869374098151, 11.59541550158063217, -3.795296366450310543 ) ) ;
#26196 = CARTESIAN_POINT ( 'NONE',  ( 0.1532563361054100626, 5.800597817667452638, -2.638427012816831230 ) ) ;
#26197 = CARTESIAN_POINT ( 'NONE',  ( 1.472469842513823179, 45.59226448433412315, -4.923371831947296329 ) ) ;
#26198 = CARTESIAN_POINT ( 'NONE',  ( 7.084665262690076126, 17.02201867748817676, -10.88017736071110164 ) ) ;
#26199 = CARTESIAN_POINT ( 'NONE',  ( 17.39651004071841456, 14.08210964143329669, -6.500000000000003553 ) ) ;
#26200 = CARTESIAN_POINT ( 'NONE',  ( 0.1532563361054100626, 60.80059781766744464, -2.638427012816831230 ) ) ;
#26201 = ADVANCED_FACE ( 'NONE', ( #73092 ), #80337, .T. ) ;
#26202 = VERTEX_POINT ( 'NONE', #12111 ) ;
#26203 = DIRECTION ( 'NONE',  ( 0.000000000000000000, 0.000000000000000000, -1.000000000000000000 ) ) ;
#26205 = ORIENTED_EDGE ( 'NONE', *, *, #67589, .T. ) ;
#26204 = EDGE_CURVE ( 'NONE', #55265, #24815, #6900, .T. ) ;
#26206 = VERTEX_POINT ( 'NONE', #97617 ) ;
#26207 = CARTESIAN_POINT ( 'NONE',  ( 5.625000000000005329, 9.588468844518212464, 9.742785792574933268 ) ) ;
#26208 = CARTESIAN_POINT ( 'NONE',  ( 6.204703633549690345, 7.845415501580634832, 14.16423886937410082 ) ) ;
#26209 = CARTESIAN_POINT ( 'NONE',  ( 20.36894250292379382, 13.67874883491396965, 10.36894250292379205 ) ) ;
#26210 = CARTESIAN_POINT ( 'NONE',  ( 17.08211943468705130, 38.47041550158063217, 12.26659068614894998 ) ) ;
#26211 = CARTESIAN_POINT ( 'NONE',  ( 2.791683348922240793, 61.63393115100079456, 7.208316651077764092 ) ) ;
#26212 = CARTESIAN_POINT ( 'NONE',  ( 0.1532563361054082862, 41.21726448433411605, 2.638427012816831674 ) ) ;
#26214 = CARTESIAN_POINT ( 'NONE',  ( 5.076628168052703671, 66.84226448433412315, 8.527530157486179263 ) ) ;
#26213 = CARTESIAN_POINT ( 'NONE',  ( -0.8801773607111008646, 38.27201867748816255, 2.915334737309923430 ) ) ;
#26215 = CARTESIAN_POINT ( 'NONE',  ( 6.204703633549690345, 0.7620821682473009062, -14.16423886937410259 ) ) ;
#26216 = EDGE_CURVE ( 'NONE', #14939, #50302, #68123, .T. ) ;
#26217 = CARTESIAN_POINT ( 'NONE',  ( 19.42250999205614193, 5.147018677488171434, 5.440088680355555262 ) ) ;
#26218 = CARTESIAN_POINT ( 'NONE',  ( -4.180366052176671232, -3.678240573451797645E-15, -14.01545757926333557 ) ) ;
#26219 = CARTESIAN_POINT ( 'NONE',  ( 0.000000000000000000, 0.5000000000000004441, 0.000000000000000000 ) ) ;
#26220 = CARTESIAN_POINT ( 'NONE',  ( 19.42250999205614193, 65.14701867748817676, 5.440088680355555262 ) ) ;
#26221 = CARTESIAN_POINT ( 'NONE',  ( 1.472469842513823179, 25.59226448433412315, -4.923371831947296329 ) ) ;
#26222 = CARTESIAN_POINT ( 'NONE',  ( 8.629999999999991900, 70.25000000000000000, -6.500000000000000888 ) ) ;
#26223 = EDGE_LOOP ( 'NONE', ( #98227, #14051, #30554, #72363 ) ) ;
#26224 = CARTESIAN_POINT ( 'NONE',  ( 64.56412365047461321, 29.50000000000000000, -10.00000000000000000 ) ) ;
#26225 = ORIENTED_EDGE ( 'NONE', *, *, #50585, .T. ) ;
#26226 = CARTESIAN_POINT ( 'NONE',  ( 5.076628168052704559, 20.17559781766745175, -8.527530157486179263 ) ) ;
#26227 = ORIENTED_EDGE ( 'NONE', *, *, #45515, .T. ) ;
#26228 = CARTESIAN_POINT ( 'NONE',  ( 22.26659068614894466, 38.88708216824731068, 7.082119434687054849 ) ) ;
#26229 = CARTESIAN_POINT ( 'NONE',  ( 14.92337183194729988, 29.34226448433411960, -8.527530157486177487 ) ) ;
#26230 = CARTESIAN_POINT ( 'NONE',  ( 15.44008868035555260, 54.73035201082150536, 9.422509992056143702 ) ) ;
#26231 = DIRECTION ( 'NONE',  ( -3.375077994860475883E-14, 0.000000000000000000, 1.000000000000000000 ) ) ;
#26232 = CARTESIAN_POINT ( 'NONE',  ( 15.44008868035555793, 46.39701867748817676, -9.422509992056140149 ) ) ;
#26233 = ADVANCED_FACE ( 'NONE', ( #42134 ), #67642, .F. ) ;
#26234 = CARTESIAN_POINT ( 'NONE',  ( -11.09922568453595382, -6.293031996736239364, -6.408140936763226492 ) ) ;
#26235 = ORIENTED_EDGE ( 'NONE', *, *, #58802, .F. ) ;
#26236 = CARTESIAN_POINT ( 'NONE',  ( -0.3689425029237881626, 7.428748834913967869, 10.36894250292379027 ) ) ;
#26237 = VERTEX_POINT ( 'NONE', #65093 ) ;
#26238 = VECTOR ( 'NONE', #20, 1000.000000000000000 ) ;
#26239 = ADVANCED_FACE ( 'NONE', ( #96118 ), #36090, .F. ) ;
#26240 = ORIENTED_EDGE ( 'NONE', *, *, #42464, .T. ) ;
#26241 = CARTESIAN_POINT ( 'NONE',  ( 16.40814093676324603, 27.45696800326375708, -11.09922568453594671 ) ) ;
#26242 = CARTESIAN_POINT ( 'NONE',  ( 19.84674366389459621, 18.50893115100078745, 7.409399052514197653E-17 ) ) ;
#26243 = CARTESIAN_POINT ( 'NONE',  ( -18.89999999999999503, 98.99999999999998579, 7.750000000000000000 ) ) ;
#26244 = CARTESIAN_POINT ( 'NONE',  ( 18.52753015748617571, 33.09226448433411605, 4.923371831947298993 ) ) ;
#26245 = CARTESIAN_POINT ( 'NONE',  ( 15.44008868035555260, 64.73035201082151957, 9.422509992056143702 ) ) ;
#26246 = SURFACE_STYLE_USAGE ( .BOTH. , #40768 ) ;
#26247 = DIRECTION ( 'NONE',  ( 1.257402221000611116E-16, -1.000000000000000000, -0.000000000000000000 ) ) ;
#26248 = CARTESIAN_POINT ( 'NONE',  ( 19.72487221294570858, 29.78217586085238366, 6.499999999999992895 ) ) ;
#26249 = DIRECTION ( 'NONE',  ( -0.000000000000000000, -1.000000000000000000, -0.000000000000000000 ) ) ;
#26250 = CARTESIAN_POINT ( 'NONE',  ( -0.8801773607110991993, 67.85535201082151957, -2.915334737309923874 ) ) ;
#26251 = CARTESIAN_POINT ( 'NONE',  ( 21.09922568453595559, 7.040301336597086568, -6.408140936763230044 ) ) ;
#26252 = CARTESIAN_POINT ( 'NONE',  ( 5.054308323419867577, 70.51564955044841554, 12.00000000000000000 ) ) ;
#26253 = CARTESIAN_POINT ( 'NONE',  ( 2.791683348922240793, 41.63393115100078745, 7.208316651077764092 ) ) ;
#26254 = CARTESIAN_POINT ( 'NONE',  ( 13.79529636645031943, 5.345415501580634832, -14.16423886937409904 ) ) ;
#26255 = CARTESIAN_POINT ( 'NONE',  ( 5.076628168052703671, 36.84226448433412315, 8.527530157486179263 ) ) ;
#26256 = CARTESIAN_POINT ( 'NONE',  ( 22.81628187352647785, 31.41530133659709279, 3.434112377981063169 ) ) ;
#26257 = CARTESIAN_POINT ( 'NONE',  ( 14.82269085861167035, 0.5000000000000004441, 2.299529454047060550 ) ) ;
#26258 = CARTESIAN_POINT ( 'NONE',  ( 17.96484262340118221, 64.93868534415483396, 7.964842623401181321 ) ) ;
#26259 = CARTESIAN_POINT ( 'NONE',  ( 19.72487221294570858, 10.71833443783938655, -6.500000000000000888 ) ) ;
#26260 = AXIS2_PLACEMENT_3D ( 'NONE', #54842, #71350, #94324 ) ;
#26261 = CARTESIAN_POINT ( 'NONE',  ( 0.1532563361054082862, 36.21726448433410894, 2.638427012816831674 ) ) ;
#26262 = CARTESIAN_POINT ( 'NONE',  ( 12.91533473730992121, 29.52201867748817321, 10.88017736071110164 ) ) ;
#26263 = CARTESIAN_POINT ( 'NONE',  ( 3.591859063236763294, 23.29030133659708568, -11.09922568453595026 ) ) ;
#26264 = CARTESIAN_POINT ( 'NONE',  ( 2.791683348922237240, 20.38393115100078745, -7.208316651077763204 ) ) ;
#26265 = CARTESIAN_POINT ( 'NONE',  ( 15.86177583122252344, -0.03417435944610275333, -2.069169861586653170 ) ) ;
#26266 = CARTESIAN_POINT ( 'NONE',  ( 7.084665262690076126, 27.02201867748817676, -10.88017736071110164 ) ) ;
#26267 = CARTESIAN_POINT ( 'NONE',  ( -0.8801773607110991993, 62.85535201082150536, -2.915334737309923874 ) ) ;
#26268 = CARTESIAN_POINT ( 'NONE',  ( 6.935117329331543345, -80.58074665962956828, 2.750000000000000888 ) ) ;
#26270 = CARTESIAN_POINT ( 'NONE',  ( 15.44008868035555260, 29.73035201082150891, 9.422509992056143702 ) ) ;
#26269 = CARTESIAN_POINT ( 'NONE',  ( 17.20831665107776587, 49.13393115100078745, -7.208316651077762316 ) ) ;
#26271 = CARTESIAN_POINT ( 'NONE',  ( -0.8801773607111009756, 48.06368534415484817, 1.068504757029289695E-15 ) ) ;
#26273 = CARTESIAN_POINT ( 'NONE',  ( -10.58981376305295008, -0.03417435944610275333, 9.535111140613638625 ) ) ;
#26272 = CARTESIAN_POINT ( 'NONE',  ( 19.42250999205614548, 15.98035201082150714, -5.440088680355545492 ) ) ;
#26274 = LINE ( 'NONE', #87271, #92053 ) ;
#26275 = CARTESIAN_POINT ( 'NONE',  ( 19.84674366389459621, 43.50893115100078745, 7.409399052514197653E-17 ) ) ;
#26277 = CARTESIAN_POINT ( 'NONE',  ( -11.48952521350030587, 4.186587853438871531E-16, 8.845383562533662314 ) ) ;
#26276 = CARTESIAN_POINT ( 'NONE',  ( 10.00000000000000000, 55.55374883491396787, -14.16423886937410082 ) ) ;
#26278 = CARTESIAN_POINT ( 'NONE',  ( 2.153642693323438717, 6.137910973973185413, -6.500000000000002665 ) ) ;
#26279 = ADVANCED_FACE ( 'NONE', ( #5111 ), #66088, .T. ) ;
#26280 = CARTESIAN_POINT ( 'NONE',  ( 64.56412365047461321, 28.99999999999999645, 10.00000000000000000 ) ) ;
#26281 = CARTESIAN_POINT ( 'NONE',  ( 13.79529636645030344, 43.26208216824730357, 14.16423886937410614 ) ) ;
#26282 = CARTESIAN_POINT ( 'NONE',  ( -3.521924834447247132, -0.8399927508087468020, 2.750000000000001776 ) ) ;
#26283 = ORIENTED_EDGE ( 'NONE', *, *, #98842, .T. ) ;
#26284 = CARTESIAN_POINT ( 'NONE',  ( -0.3689425029237898834, 61.17874883491396076, -10.36894250292378850 ) ) ;
#26285 = CARTESIAN_POINT ( 'NONE',  ( 17.20831665107776587, 29.13393115100078390, -7.208316651077762316 ) ) ;
#26287 = CARTESIAN_POINT ( 'NONE',  ( -8.443706647342963834, 87.03308080853030049, -4.556631258847860799 ) ) ;
#26286 = LINE ( 'NONE', #17338, #37191 ) ;
#26288 = CARTESIAN_POINT ( 'NONE',  ( 4.559911319644449179, 63.89701867748817676, 9.422509992056141925 ) ) ;
#26289 = CARTESIAN_POINT ( 'NONE',  ( 11.34661744925197802, 54.08985607419764818, 3.000000000000000000 ) ) ;
#26290 = TOROIDAL_SURFACE ( 'NONE', #51852, 10.09999999999999787, 0.1000000000000000056 ) ;
#26292 =( BOUNDED_SURFACE ( )  B_SPLINE_SURFACE ( 1, 2, ( 
 ( #97145, #96141, #51118, #58109, #80637, #73611, #43614, #57628, #65121, #81609, #36112, #20125, #87633, #96640, #42636, #51624, #44096, #5135, #95640, #58617, #72622, #27126, #73113, #74101, #88618, #50629, #74607, #6120, #89118, #88125, #13118, #20629, #11644, #81120, #28117, #5634, #35626, #36626, #66618, #95130, #59103, #26641, #19637, #66111, #50130, #28616, #89612, #21125, #4655, #35116, #65615, #12621, #57137, #27624, #43123, #19147, #49624, #42157, #23606, #67110, #8098, #54072, #8584, #75598, #22613, #68601, #83602, #7110, #38112, #53090, #90589, #30578, #30084, #37614, #67616, #21626, #84587, #68108, #97635, #29100, #6607, #60591, #59602, #60087, #22116, #84094, #45592, #626, #52596, #83099, #129, #14627, #76090, #16086, #29585, #38594, #69092, #45092, #98633, #15116, #23109, #37120, #7620, #52111, #98124, #61083, #91593, #46573, #91086, #53581, #15610, #46094, #77072, #76578, #90098, #31072, #82603, #44605, #61570, #14121, #92081, #75100, #71063, #16583, #32552, #17084, #2093, #47059, #93055, #39090, #41062, #40066, #94048, #63053, #24588, #17576, #86555, #1597, #77557, #25569, #79038, #93550, #31564, #40565, #85570, #94534, #87037, #48042, #9073, #2588, #39586, #70077, #55051, #18059, #25083, #55566, #18547, #26053, #33043, #32048, #56061, #63538, #24089, #86065, #48539, #10551, #78554, #49039, #71559, #69581, #3071, #1101, #47564, #62550, #62059, #33527, #64022, #78062, #79543, #10066, #56542, #92563, #9565, #70567, #54557, #85074, #28006, #88514, #95531, #26529, #42526, #3558, #41564, #65507, #50026, #43017, #96029, #80026, #5025, #89504, #27511, #57521, #96531, #73010, #64515, #72031, #11530, #42051, #34511, #87527, #43499, #12515, #19041, #36004, #20519, #80528, #81014, #12027, #4542, #35004, #66507, #34018, #95021, #97032, #49517, #73499, #27021, #72515, #13004, #35509, #57026, #4049, #20016, #66003, #28508, #59002, #21015, #65004, #73998, #19529, #81499, #58502, #58005, #88017, #50517, #89012, #51503, #51004, #5524, #11043, #89991, #68979, #74991, #90475, #43990, #37503, #513, #81997, #14010, #76471, #13508, #52005, #22501, #74492, #36508, #15005, #75977, #37997, #91965, #30464, #7986, #44491, #59981, #38485, #83975, #6494, #52972, #15500, #83484, #45475, #82991, #7506, #68489, #16, #60965, #82494, #30959, #61457, #53465, #6016, #21507, #91473, #22009, #23494, #67001, #52483, #14509, #97523, #28985, #37002, #22998, #29473, #59491, #67498, #60478, #98019, #45982, #44979, #75485, #6998, #67995, #98520, #29973, #90967, #10439, #17461, #23974, #9950, #47928, #38975, #47444, #55449, #78434, #32437, #33408 ),
 ( #54447, #40454, #63906, #39950, #1480, #70953, #85451, #8467, #15974, #84956, #16467, #77442, #31447, #86442, #85951, #61949, #78929, #63429, #24469, #24964, #54934, #16963, #77943, #40946, #84474, #76957, #71444, #92450, #2473, #39471, #46947, #55943, #32929, #987, #69466, #62937, #93935, #2958, #94417, #53965, #8954, #17941, #62433, #25460, #48426, #9449, #46464, #1972, #93439, #69961, #31933, #92937, #70453, #33895, #12881, #18927, #34394, #86922, #80408, #43380, #25933, #56908, #20401, #56433, #94909, #65386, #18433, #79429, #57885, #19896, #80898, #35880, #73382, #50888, #87410, #3924, #81382, #27884, #49404, #95913, #58371, #27393, #88399, #26904, #50389, #12394, #42900, #4908, #26408, #73879, #5409, #96408, #48916, #88892, #35389, #65880, #57401, #66376, #10925, #41451, #71915, #79904, #3436, #64400, #11413, #41934, #72395, #64881, #95408, #87891, #19408, #49899, #11909, #42411, #72891, #4425, #34890, #97395, #20894, #37879, #90850, #36881, #38363, #82870, #37385, #14886, #59367, #6368, #29359, #21887, #45355, #75360, #82363, #13383, #59862, #89381, #28387, #52365, #67371, #29853, #14384, #66878, #22381, #76353, #44854, #44370, #83363, #90349, #51383, #58879, #28863, #89870, #21385, #74362, #30342, #98396, #5890, #22875, #7380, #97901, #67875, #6874, #60356, #52855, #53346, #81870, #43866, #83854, #36383, #75860, #13886, #51882, #98891, #68372, #74869, #60849, #91348, #15378, #45862, #7868, #96910, #31329, #70834, #77321, #40330, #24836, #39349, #30843, #16840, #47313, #25338, #70337, #55318, #62315, #76834, #55822, #61829, #8835, #61341, #24351, #86316, #68861, #870, #63298, #393, #38857, #9328, #91852, #23367, #1853, #62816, #85825, #78809, #17340, #93808, #92337, #46829, #17820, #2346, #23860, #39831, #8349, #32311, #54325, #69346, #32803, #93314, #15862, #53853, #77813, #47809, #48302, #10318, #84361, #84839, #46347, #69843, #16347, #78310, #1367, #31818, #9829, #92822, #54815, #85326, #27269, #34264, #48793, #27765, #33769, #49288, #2837, #95278, #58248, #40820, #71801, #35264, #71319, #10810, #80282, #33293, #94293, #72763, #34772, #95788, #52127, #88272, #65761, #3306, #18805, #96286, #42782, #64276, #11782, #73266, #42290, #4298, #41810, #65259, #57767, #19774, #50261, #41328, #90116, #21643, #12271, #63784, #79301, #80778, #79788, #82623, #25816, #11291, #72278, #56313, #86809, #94788, #3808, #26288, #18311, #4788, #56789, #64766, #87284, #26781, #57279, #87773, #19288, #49775, #45610, #38129, #31090, #91609, #98654, #29604, #76108, #6625, #44623, #68617, #53108, #46112, #146, #83115, #8114, #92582 ) ),
 .UNSPECIFIED., .F., .F., .F. ) 
 B_SPLINE_SURFACE_WITH_KNOTS ( ( 2, 2 ),
 ( 3, 2, 2, 2, 2, 2, 2, 2, 2, 2, 2, 2, 2, 2, 2, 2, 2, 2, 2, 2, 2, 2, 2, 2, 2, 2, 2, 2, 2, 2, 2, 2, 2, 2, 2, 2, 2, 2, 2, 2, 2, 2, 2, 2, 2, 2, 2, 2, 2, 2, 2, 2, 2, 2, 2, 2, 2, 2, 2, 2, 2, 2, 2, 2, 2, 2, 2, 2, 2, 2, 2, 2, 2, 2, 2, 2, 2, 2, 2, 2, 2, 2, 2, 2, 2, 2, 2, 2, 2, 2, 2, 2, 2, 2, 2, 2, 2, 2, 2, 2, 2, 2, 2, 2, 2, 2, 2, 2, 2, 2, 2, 2, 2, 2, 2, 2, 2, 2, 2, 2, 2, 2, 2, 2, 2, 2, 2, 2, 2, 2, 2, 2, 2, 2, 2, 2, 2, 2, 2, 2, 2, 2, 2, 2, 2, 2, 2, 2, 2, 2, 2, 2, 2, 2, 2, 2, 2, 2, 2, 2, 2, 2, 3 ),
 ( 0.000000000000000000, 1.000000000000000000 ),
 ( 0.000000000000000000, 0.005952380952380952051, 0.01190476190476190410, 0.01785714285714285615, 0.02380952380952380820, 0.02976190476190476025, 0.03571428571428571230, 0.04166666666666666435, 0.04761904761904761640, 0.05357142857142856845, 0.05952380952380952051, 0.06547619047619047949, 0.07142857142857142461, 0.07738095238095238360, 0.08333333333333332871, 0.08928571428571428770, 0.09523809523809523281, 0.1011904761904761918, 0.1071428571428571369, 0.1130952380952380959, 0.1190476190476190410, 0.1250000000000000000, 0.1309523809523809590, 0.1369047619047619180, 0.1428571428571428492, 0.1488095238095238082, 0.1547619047619047672, 0.1607142857142857262, 0.1666666666666666574, 0.1726190476190476164, 0.1785714285714285754, 0.1845238095238095344, 0.1904761904761904656, 0.1964285714285714246, 0.2023809523809523836, 0.2083333333333333426, 0.2142857142857142738, 0.2202380952380952328, 0.2261904761904761918, 0.2321428571428571508, 0.2380952380952380820, 0.2440476190476190410, 0.2500000000000000000, 0.2559523809523809312, 0.2619047619047619180, 0.2678571428571428492, 0.2738095238095238360, 0.2797619047619047672, 0.2857142857142856984, 0.2916666666666666852, 0.2976190476190476164, 0.3035714285714285476, 0.3095238095238095344, 0.3154761904761904656, 0.3214285714285714524, 0.3273809523809523836, 0.3333333333333333148, 0.3392857142857143016, 0.3452380952380952328, 0.3511904761904761640, 0.3571428571428571508, 0.3630952380952380820, 0.3690476190476190688, 0.3750000000000000000, 0.3809523809523809312, 0.3869047619047619180, 0.3928571428571428492, 0.3988095238095238360, 0.4047619047619047672, 0.4107142857142856984, 0.4166666666666666852, 0.4226190476190476164, 0.4285714285714285476, 0.4345238095238095344, 0.4404761904761904656, 0.4464285714285714524, 0.4523809523809523836, 0.4583333333333333148, 0.4642857142857143016, 0.4702380952380952328, 0.4761904761904761640, 0.4821428571428571508, 0.4880952380952380820, 0.4940476190476190688, 0.5000000000000000000, 0.5059523809523809312, 0.5119047619047618625, 0.5178571428571429047, 0.5238095238095238360, 0.5297619047619047672, 0.5357142857142856984, 0.5416666666666666297, 0.5476190476190476719, 0.5535714285714286031, 0.5595238095238095344, 0.5654761904761904656, 0.5714285714285713969, 0.5773809523809523281, 0.5833333333333333703, 0.5892857142857143016, 0.5952380952380952328, 0.6011904761904761640, 0.6071428571428570953, 0.6130952380952381375, 0.6190476190476190688, 0.6250000000000000000, 0.6309523809523809312, 0.6369047619047618625, 0.6428571428571429047, 0.6488095238095238360, 0.6547619047619047672, 0.6607142857142856984, 0.6666666666666666297, 0.6726190476190476719, 0.6785714285714286031, 0.6845238095238095344, 0.6904761904761904656, 0.6964285714285713969, 0.7023809523809523281, 0.7083333333333333703, 0.7142857142857143016, 0.7202380952380952328, 0.7261904761904761640, 0.7321428571428570953, 0.7380952380952381375, 0.7440476190476190688, 0.7500000000000000000, 0.7559523809523809312, 0.7619047619047618625, 0.7678571428571429047, 0.7738095238095238360, 0.7797619047619047672, 0.7857142857142856984, 0.7916666666666666297, 0.7976190476190476719, 0.8035714285714286031, 0.8095238095238095344, 0.8154761904761904656, 0.8214285714285713969, 0.8273809523809523281, 0.8333333333333333703, 0.8392857142857143016, 0.8452380952380952328, 0.8511904761904761640, 0.8571428571428570953, 0.8630952380952381375, 0.8690476190476190688, 0.8750000000000000000, 0.8809523809523809312, 0.8869047619047618625, 0.8928571428571429047, 0.8988095238095238360, 0.9047619047619047672, 0.9107142857142856984, 0.9166666666666666297, 0.9226190476190476719, 0.9285714285714286031, 0.9345238095238095344, 0.9404761904761904656, 0.9464285714285713969, 0.9523809523809523281, 0.9583333333333333703, 0.9642857142857143016 ),
 .UNSPECIFIED. ) 
 GEOMETRIC_REPRESENTATION_ITEM ( )  RATIONAL_B_SPLINE_SURFACE ( (
 ( 1.000000000000000000, 0.9659258262890683122, 1.000000000000000000, 0.9659258262890683122, 1.000000000000000000, 0.9659258262890683122, 1.000000000000000000, 0.9659258262890683122, 1.000000000000000000, 0.9659258262890683122, 1.000000000000000000, 0.9659258262890683122, 1.000000000000000000, 0.9659258262890683122, 1.000000000000000000, 0.9659258262890683122, 1.000000000000000000, 0.9659258262890683122, 1.000000000000000000, 0.9659258262890683122, 1.000000000000000000, 0.9659258262890683122, 1.000000000000000000, 0.9659258262890683122, 1.000000000000000000, 0.9659258262890683122, 1.000000000000000000, 0.9659258262890683122, 1.000000000000000000, 0.9659258262890683122, 1.000000000000000000, 0.9659258262890683122, 1.000000000000000000, 0.9659258262890683122, 1.000000000000000000, 0.9659258262890683122, 1.000000000000000000, 0.9659258262890683122, 1.000000000000000000, 0.9659258262890683122, 1.000000000000000000, 0.9659258262890683122, 1.000000000000000000, 0.9659258262890683122, 1.000000000000000000, 0.9659258262890683122, 1.000000000000000000, 0.9659258262890683122, 1.000000000000000000, 0.9659258262890683122, 1.000000000000000000, 0.9659258262890683122, 1.000000000000000000, 0.9659258262890683122, 1.000000000000000000, 0.9659258262890683122, 1.000000000000000000, 0.9659258262890683122, 1.000000000000000000, 0.9659258262890683122, 1.000000000000000000, 0.9659258262890683122, 1.000000000000000000, 0.9659258262890683122, 1.000000000000000000, 0.9659258262890683122, 1.000000000000000000, 0.9659258262890683122, 1.000000000000000000, 0.9659258262890683122, 1.000000000000000000, 0.9659258262890683122, 1.000000000000000000, 0.9659258262890683122, 1.000000000000000000, 0.9659258262890683122, 1.000000000000000000, 0.9659258262890683122, 1.000000000000000000, 0.9659258262890683122, 1.000000000000000000, 0.9659258262890683122, 1.000000000000000000, 0.9659258262890683122, 1.000000000000000000, 0.9659258262890683122, 1.000000000000000000, 0.9659258262890683122, 1.000000000000000000, 0.9659258262890683122, 1.000000000000000000, 0.9659258262890683122, 1.000000000000000000, 0.9659258262890683122, 1.000000000000000000, 0.9659258262890683122, 1.000000000000000000, 0.9659258262890683122, 1.000000000000000000, 0.9659258262890683122, 1.000000000000000000, 0.9659258262890683122, 1.000000000000000000, 0.9659258262890683122, 1.000000000000000000, 0.9659258262890683122, 1.000000000000000000, 0.9659258262890683122, 1.000000000000000000, 0.9659258262890683122, 1.000000000000000000, 0.9659258262890683122, 1.000000000000000000, 0.9659258262890683122, 1.000000000000000000, 0.9659258262890683122, 1.000000000000000000, 0.9659258262890683122, 1.000000000000000000, 0.9659258262890683122, 1.000000000000000000, 0.9659258262890683122, 1.000000000000000000, 0.9659258262890683122, 1.000000000000000000, 0.9659258262890683122, 1.000000000000000000, 0.9659258262890683122, 1.000000000000000000, 0.9659258262890683122, 1.000000000000000000, 0.9659258262890683122, 1.000000000000000000, 0.9659258262890683122, 1.000000000000000000, 0.9659258262890683122, 1.000000000000000000, 0.9659258262890683122, 1.000000000000000000, 0.9659258262890683122, 1.000000000000000000, 0.9659258262890683122, 1.000000000000000000, 0.9659258262890683122, 1.000000000000000000, 0.9659258262890683122, 1.000000000000000000, 0.9659258262890683122, 1.000000000000000000, 0.9659258262890683122, 1.000000000000000000, 0.9659258262890683122, 1.000000000000000000, 0.9659258262890683122, 1.000000000000000000, 0.9659258262890683122, 1.000000000000000000, 0.9659258262890683122, 1.000000000000000000, 0.9659258262890683122, 1.000000000000000000, 0.9659258262890683122, 1.000000000000000000, 0.9659258262890683122, 1.000000000000000000, 0.9659258262890683122, 1.000000000000000000, 0.9659258262890683122, 1.000000000000000000, 0.9659258262890683122, 1.000000000000000000, 0.9659258262890683122, 1.000000000000000000, 0.9659258262890683122, 1.000000000000000000, 0.9659258262890683122, 1.000000000000000000, 0.9659258262890683122, 1.000000000000000000, 0.9659258262890683122, 1.000000000000000000, 0.9659258262890683122, 1.000000000000000000, 0.9659258262890683122, 1.000000000000000000, 0.9659258262890683122, 1.000000000000000000, 0.9659258262890683122, 1.000000000000000000, 0.9659258262890683122, 1.000000000000000000, 0.9659258262890683122, 1.000000000000000000, 0.9659258262890683122, 1.000000000000000000, 0.9659258262890683122, 1.000000000000000000, 0.9659258262890683122, 1.000000000000000000, 0.9659258262890683122, 1.000000000000000000, 0.9659258262890683122, 1.000000000000000000, 0.9659258262890683122, 1.000000000000000000, 0.9659258262890683122, 1.000000000000000000, 0.9659258262890683122, 1.000000000000000000, 0.9659258262890683122, 1.000000000000000000, 0.9659258262890683122, 1.000000000000000000, 0.9659258262890683122, 1.000000000000000000, 0.9659258262890683122, 1.000000000000000000, 0.9659258262890683122, 1.000000000000000000, 0.9659258262890683122, 1.000000000000000000, 0.9659258262890683122, 1.000000000000000000, 0.9659258262890683122, 1.000000000000000000, 0.9659258262890683122, 1.000000000000000000, 0.9659258262890683122, 1.000000000000000000, 0.9659258262890683122, 1.000000000000000000, 0.9659258262890683122, 1.000000000000000000, 0.9659258262890683122, 1.000000000000000000, 0.9659258262890683122, 1.000000000000000000, 0.9659258262890683122, 1.000000000000000000, 0.9659258262890683122, 1.000000000000000000, 0.9659258262890683122, 1.000000000000000000, 0.9659258262890683122, 1.000000000000000000, 0.9659258262890683122, 1.000000000000000000, 0.9659258262890683122, 1.000000000000000000, 0.9659258262890683122, 1.000000000000000000, 0.9659258262890683122, 1.000000000000000000, 0.9659258262890683122, 1.000000000000000000, 0.9659258262890683122, 1.000000000000000000, 0.9659258262890683122, 1.000000000000000000, 0.9659258262890683122, 1.000000000000000000, 0.9659258262890683122, 1.000000000000000000, 0.9659258262890683122, 1.000000000000000000, 0.9659258262890683122, 1.000000000000000000, 0.9659258262890683122, 1.000000000000000000, 0.9659258262890683122, 1.000000000000000000, 0.9659258262890683122, 1.000000000000000000, 0.9659258262890683122, 1.000000000000000000, 0.9659258262890683122, 1.000000000000000000, 0.9659258262890683122, 1.000000000000000000, 0.9659258262890683122, 1.000000000000000000, 0.9659258262890683122, 1.000000000000000000, 0.9659258262890683122, 1.000000000000000000, 0.9659258262890683122, 1.000000000000000000, 0.9659258262890683122, 1.000000000000000000, 0.9659258262890683122, 1.000000000000000000, 0.9659258262890683122, 1.000000000000000000, 0.9659258262890683122, 1.000000000000000000, 0.9659258262890683122, 1.000000000000000000, 0.9659258262890683122, 1.000000000000000000, 0.9659258262890683122, 1.000000000000000000, 0.9659258262890683122, 1.000000000000000000, 0.9659258262890683122, 1.000000000000000000, 0.9659258262890683122, 1.000000000000000000, 0.9659258262890683122, 1.000000000000000000, 0.9659258262890683122, 1.000000000000000000, 0.9659258262890683122, 1.000000000000000000, 0.9659258262890683122, 1.000000000000000000, 0.9659258262890683122, 1.000000000000000000, 0.9659258262890683122, 1.000000000000000000, 0.9659258262890683122, 1.000000000000000000, 0.9659258262890683122, 1.000000000000000000, 0.9659258262890683122, 1.000000000000000000),
 ( 1.000000000000000000, 0.9659258262890683122, 1.000000000000000000, 0.9659258262890683122, 1.000000000000000000, 0.9659258262890683122, 1.000000000000000000, 0.9659258262890683122, 1.000000000000000000, 0.9659258262890683122, 1.000000000000000000, 0.9659258262890683122, 1.000000000000000000, 0.9659258262890683122, 1.000000000000000000, 0.9659258262890683122, 1.000000000000000000, 0.9659258262890683122, 1.000000000000000000, 0.9659258262890683122, 1.000000000000000000, 0.9659258262890683122, 1.000000000000000000, 0.9659258262890683122, 1.000000000000000000, 0.9659258262890683122, 1.000000000000000000, 0.9659258262890683122, 1.000000000000000000, 0.9659258262890683122, 1.000000000000000000, 0.9659258262890683122, 1.000000000000000000, 0.9659258262890683122, 1.000000000000000000, 0.9659258262890683122, 1.000000000000000000, 0.9659258262890683122, 1.000000000000000000, 0.9659258262890683122, 1.000000000000000000, 0.9659258262890683122, 1.000000000000000000, 0.9659258262890683122, 1.000000000000000000, 0.9659258262890683122, 1.000000000000000000, 0.9659258262890683122, 1.000000000000000000, 0.9659258262890683122, 1.000000000000000000, 0.9659258262890683122, 1.000000000000000000, 0.9659258262890683122, 1.000000000000000000, 0.9659258262890683122, 1.000000000000000000, 0.9659258262890683122, 1.000000000000000000, 0.9659258262890683122, 1.000000000000000000, 0.9659258262890683122, 1.000000000000000000, 0.9659258262890683122, 1.000000000000000000, 0.9659258262890683122, 1.000000000000000000, 0.9659258262890683122, 1.000000000000000000, 0.9659258262890683122, 1.000000000000000000, 0.9659258262890683122, 1.000000000000000000, 0.9659258262890683122, 1.000000000000000000, 0.9659258262890683122, 1.000000000000000000, 0.9659258262890683122, 1.000000000000000000, 0.9659258262890683122, 1.000000000000000000, 0.9659258262890683122, 1.000000000000000000, 0.9659258262890683122, 1.000000000000000000, 0.9659258262890683122, 1.000000000000000000, 0.9659258262890683122, 1.000000000000000000, 0.9659258262890683122, 1.000000000000000000, 0.9659258262890683122, 1.000000000000000000, 0.9659258262890683122, 1.000000000000000000, 0.9659258262890683122, 1.000000000000000000, 0.9659258262890683122, 1.000000000000000000, 0.9659258262890683122, 1.000000000000000000, 0.9659258262890683122, 1.000000000000000000, 0.9659258262890683122, 1.000000000000000000, 0.9659258262890683122, 1.000000000000000000, 0.9659258262890683122, 1.000000000000000000, 0.9659258262890683122, 1.000000000000000000, 0.9659258262890683122, 1.000000000000000000, 0.9659258262890683122, 1.000000000000000000, 0.9659258262890683122, 1.000000000000000000, 0.9659258262890683122, 1.000000000000000000, 0.9659258262890683122, 1.000000000000000000, 0.9659258262890683122, 1.000000000000000000, 0.9659258262890683122, 1.000000000000000000, 0.9659258262890683122, 1.000000000000000000, 0.9659258262890683122, 1.000000000000000000, 0.9659258262890683122, 1.000000000000000000, 0.9659258262890683122, 1.000000000000000000, 0.9659258262890683122, 1.000000000000000000, 0.9659258262890683122, 1.000000000000000000, 0.9659258262890683122, 1.000000000000000000, 0.9659258262890683122, 1.000000000000000000, 0.9659258262890683122, 1.000000000000000000, 0.9659258262890683122, 1.000000000000000000, 0.9659258262890683122, 1.000000000000000000, 0.9659258262890683122, 1.000000000000000000, 0.9659258262890683122, 1.000000000000000000, 0.9659258262890683122, 1.000000000000000000, 0.9659258262890683122, 1.000000000000000000, 0.9659258262890683122, 1.000000000000000000, 0.9659258262890683122, 1.000000000000000000, 0.9659258262890683122, 1.000000000000000000, 0.9659258262890683122, 1.000000000000000000, 0.9659258262890683122, 1.000000000000000000, 0.9659258262890683122, 1.000000000000000000, 0.9659258262890683122, 1.000000000000000000, 0.9659258262890683122, 1.000000000000000000, 0.9659258262890683122, 1.000000000000000000, 0.9659258262890683122, 1.000000000000000000, 0.9659258262890683122, 1.000000000000000000, 0.9659258262890683122, 1.000000000000000000, 0.9659258262890683122, 1.000000000000000000, 0.9659258262890683122, 1.000000000000000000, 0.9659258262890683122, 1.000000000000000000, 0.9659258262890683122, 1.000000000000000000, 0.9659258262890683122, 1.000000000000000000, 0.9659258262890683122, 1.000000000000000000, 0.9659258262890683122, 1.000000000000000000, 0.9659258262890683122, 1.000000000000000000, 0.9659258262890683122, 1.000000000000000000, 0.9659258262890683122, 1.000000000000000000, 0.9659258262890683122, 1.000000000000000000, 0.9659258262890683122, 1.000000000000000000, 0.9659258262890683122, 1.000000000000000000, 0.9659258262890683122, 1.000000000000000000, 0.9659258262890683122, 1.000000000000000000, 0.9659258262890683122, 1.000000000000000000, 0.9659258262890683122, 1.000000000000000000, 0.9659258262890683122, 1.000000000000000000, 0.9659258262890683122, 1.000000000000000000, 0.9659258262890683122, 1.000000000000000000, 0.9659258262890683122, 1.000000000000000000, 0.9659258262890683122, 1.000000000000000000, 0.9659258262890683122, 1.000000000000000000, 0.9659258262890683122, 1.000000000000000000, 0.9659258262890683122, 1.000000000000000000, 0.9659258262890683122, 1.000000000000000000, 0.9659258262890683122, 1.000000000000000000, 0.9659258262890683122, 1.000000000000000000, 0.9659258262890683122, 1.000000000000000000, 0.9659258262890683122, 1.000000000000000000, 0.9659258262890683122, 1.000000000000000000, 0.9659258262890683122, 1.000000000000000000, 0.9659258262890683122, 1.000000000000000000, 0.9659258262890683122, 1.000000000000000000, 0.9659258262890683122, 1.000000000000000000, 0.9659258262890683122, 1.000000000000000000, 0.9659258262890683122, 1.000000000000000000, 0.9659258262890683122, 1.000000000000000000, 0.9659258262890683122, 1.000000000000000000, 0.9659258262890683122, 1.000000000000000000, 0.9659258262890683122, 1.000000000000000000, 0.9659258262890683122, 1.000000000000000000, 0.9659258262890683122, 1.000000000000000000, 0.9659258262890683122, 1.000000000000000000, 0.9659258262890683122, 1.000000000000000000, 0.9659258262890683122, 1.000000000000000000, 0.9659258262890683122, 1.000000000000000000, 0.9659258262890683122, 1.000000000000000000, 0.9659258262890683122, 1.000000000000000000, 0.9659258262890683122, 1.000000000000000000, 0.9659258262890683122, 1.000000000000000000, 0.9659258262890683122, 1.000000000000000000, 0.9659258262890683122, 1.000000000000000000, 0.9659258262890683122, 1.000000000000000000, 0.9659258262890683122, 1.000000000000000000, 0.9659258262890683122, 1.000000000000000000, 0.9659258262890683122, 1.000000000000000000, 0.9659258262890683122, 1.000000000000000000, 0.9659258262890683122, 1.000000000000000000, 0.9659258262890683122, 1.000000000000000000, 0.9659258262890683122, 1.000000000000000000, 0.9659258262890683122, 1.000000000000000000, 0.9659258262890683122, 1.000000000000000000, 0.9659258262890683122, 1.000000000000000000, 0.9659258262890683122, 1.000000000000000000, 0.9659258262890683122, 1.000000000000000000, 0.9659258262890683122, 1.000000000000000000, 0.9659258262890683122, 1.000000000000000000, 0.9659258262890683122, 1.000000000000000000, 0.9659258262890683122, 1.000000000000000000, 0.9659258262890683122, 1.000000000000000000, 0.9659258262890683122, 1.000000000000000000, 0.9659258262890683122, 1.000000000000000000) ) ) 
 REPRESENTATION_ITEM ( '' )  SURFACE ( )  );
#26291 = CARTESIAN_POINT ( 'NONE',  ( -0.8801773607110991993, 32.85535201082151247, -2.915334737309923874 ) ) ;
#26293 = CARTESIAN_POINT ( 'NONE',  ( 6.565887622018943937, 63.08196800326376064, -12.81628187352647608 ) ) ;
#26294 = CARTESIAN_POINT ( 'NONE',  ( 19.38216949554541557, 7.248634669930421381, -9.382169495545420901 ) ) ;
#26295 = CARTESIAN_POINT ( 'NONE',  ( 14.92337183194729988, 19.34226448433411960, -8.527530157486177487 ) ) ;
#26296 = EDGE_LOOP ( 'NONE', ( #92985, #30633, #50320, #23802 ) ) ;
#26297 = AXIS2_PLACEMENT_3D ( 'NONE', #10929, #41455, #30349 ) ;
#26298 = CARTESIAN_POINT ( 'NONE',  ( 2.888614318722440899, 15.00000000000000888, -14.33855829812821980 ) ) ;
#26299 = CARTESIAN_POINT ( 'NONE',  ( 10.00000000000000178, 68.05374883491397497, 14.16423886937410082 ) ) ;
#26300 = CARTESIAN_POINT ( 'NONE',  ( -4.164238869374099927, 32.01208216824730357, 3.795296366450308767 ) ) ;
#26301 = CARTESIAN_POINT ( 'NONE',  ( -0.8801773607111009756, 38.06368534415484106, 1.068504757029289695E-15 ) ) ;
#26302 = CARTESIAN_POINT ( 'NONE',  ( 0.5774900079438607392, 48.48035201082150536, 5.440088680355550821 ) ) ;
#26303 = CARTESIAN_POINT ( 'NONE',  ( 0.000000000000000000, 70.00000000000000000, 6.500000000000000888 ) ) ;
#26304 = CARTESIAN_POINT ( 'NONE',  ( 10.09973302574091569, -32.02492402197682253, -4.000000000000000888 ) ) ;
#26305 = CARTESIAN_POINT ( 'NONE',  ( 10.00000000000000178, 7.258931151000785675, 9.846743663894594434 ) ) ;
#26306 = CARTESIAN_POINT ( 'NONE',  ( 17.20831665107776587, 27.88393115100078390, 7.208316651077764980 ) ) ;
#26307 = FILL_AREA_STYLE_COLOUR ( '', #34685 ) ;
#26308 = MECHANICAL_DESIGN_GEOMETRIC_PRESENTATION_REPRESENTATION (  '', ( #45431 ), #82190 ) ;
#26309 = CARTESIAN_POINT ( 'NONE',  ( 14.92337183194729633, 17.67559781766745175, 8.527530157486181039 ) ) ;
#26310 = CARTESIAN_POINT ( 'NONE',  ( 17.20831665107776587, 54.13393115100079456, -7.208316651077762316 ) ) ;
#26311 = CARTESIAN_POINT ( 'NONE',  ( 7.084665262690076126, 27.02201867748817676, -10.88017736071110164 ) ) ;
#26312 = UNCERTAINTY_MEASURE_WITH_UNIT (LENGTH_MEASURE( 1.000000000000000082E-05 ), #27681, 'distance_accuracy_value', 'NONE');
#26313 = EDGE_CURVE ( 'NONE', #94118, #87018, #21099, .T. ) ;
#26314 = CARTESIAN_POINT ( 'NONE',  ( -1.099225684535947600, 44.54030133659708923, 6.408140936763237150 ) ) ;
#26315 = CIRCLE ( 'NONE', #77409, 14.49999999999999822 ) ;
#26316 = CARTESIAN_POINT ( 'NONE',  ( 17.96484262340118221, 61.18868534415482685, -7.964842623401177768 ) ) ;
#26317 = CARTESIAN_POINT ( 'NONE',  ( 17.20831665107776587, 32.88393115100078745, 7.208316651077764980 ) ) ;
#26319 = CARTESIAN_POINT ( 'NONE',  ( 0.1532563361054083140, 21.00893115100078745, 1.131784320476157264E-15 ) ) ;
#26318 = CARTESIAN_POINT ( 'NONE',  ( 6.204703633549690345, 60.76208216824730357, -14.16423886937410259 ) ) ;
#26320 = DIRECTION ( 'NONE',  ( 0.000000000000000000, 0.000000000000000000, 1.000000000000000000 ) ) ;
#26321 = CARTESIAN_POINT ( 'NONE',  ( -9.000000000000000000, 75.76920769491746910, 3.000000000000000000 ) ) ;
#26322 = CARTESIAN_POINT ( 'NONE',  ( 6.204703633549690345, 12.84541550158063572, 14.16423886937410082 ) ) ;
#26323 = EDGE_CURVE ( 'NONE', #65699, #18711, #51600, .T. ) ;
#26324 = CARTESIAN_POINT ( 'NONE',  ( 2.917880565312950480, 25.97041550158063572, -12.26659068614894821 ) ) ;
#26325 = CARTESIAN_POINT ( 'NONE',  ( 0.1532563361054100626, 30.80059781766744820, -2.638427012816831230 ) ) ;
#26326 = CARTESIAN_POINT ( 'NONE',  ( 0.000000000000000000, 12.49999999999999112, 0.000000000000000000 ) ) ;
#26327 = CARTESIAN_POINT ( 'NONE',  ( 20.88017736071110519, 20.56368534415484106, 2.639326808657452039E-16 ) ) ;
#26328 = CARTESIAN_POINT ( 'NONE',  ( 7.084665262690076126, 59.10535201082150536, 10.88017736071109987 ) ) ;
#26329 = CARTESIAN_POINT ( 'NONE',  ( 4.559911319644449179, 43.89701867748816966, 9.422509992056141925 ) ) ;
#26330 = VERTEX_POINT ( 'NONE', #82083 ) ;
#26331 = CARTESIAN_POINT ( 'NONE',  ( 21.09922568453595559, 47.04030133659708923, -6.408140936763230044 ) ) ;
#26332 = CARTESIAN_POINT ( 'NONE',  ( 19.42250999205614548, 50.98035201082151247, -5.440088680355545492 ) ) ;
#26333 = ORIENTED_EDGE ( 'NONE', *, *, #46207, .F. ) ;
#26334 = AXIS2_PLACEMENT_3D ( 'NONE', #78129, #16652, #71131 ) ;
#26335 = CARTESIAN_POINT ( 'NONE',  ( -0.1503990784575328643, 50.12777174578613426, 6.262539305110068177 ) ) ;
#26336 = CARTESIAN_POINT ( 'NONE',  ( 17.96484262340118221, 64.93868534415483396, 7.964842623401181321 ) ) ;
#26337 = VERTEX_POINT ( 'NONE', #88104 ) ;
#26338 = CARTESIAN_POINT ( 'NONE',  ( 20.88017736071110875, 60.77201867748817676, -2.915334737309920765 ) ) ;
#26339 = DIRECTION ( 'NONE',  ( 0.000000000000000000, 1.000000000000000000, 0.000000000000000000 ) ) ;
#26340 = CARTESIAN_POINT ( 'NONE',  ( 0.000000000000000000, 0.5000000000000004441, 0.000000000000000000 ) ) ;
#26341 = CARTESIAN_POINT ( 'NONE',  ( 17.96484262340118221, 4.938685344154837509, 7.964842623401181321 ) ) ;
#26342 = CARTESIAN_POINT ( 'NONE',  ( 5.076628168052704559, 10.17559781766745175, -8.527530157486179263 ) ) ;
#26343 = CARTESIAN_POINT ( 'NONE',  ( 24.16423886937410614, 9.512082168247301794, -3.795296366450302550 ) ) ;
#26344 = CARTESIAN_POINT ( 'NONE',  ( 19.84674366389459266, 3.300597817667451750, 2.638427012816836559 ) ) ;
#26345 = CARTESIAN_POINT ( 'NONE',  ( 2.035157376598822676, 12.43868534415483751, -7.964842623401177768 ) ) ;
#26346 = CARTESIAN_POINT ( 'NONE',  ( 1.472469842513823179, 51.42559781766745886, 4.923371831947296329 ) ) ;
#26347 = VERTEX_POINT ( 'NONE', #28593 ) ;
#26348 = CARTESIAN_POINT ( 'NONE',  ( 14.92337183194729633, 42.67559781766745886, 8.527530157486181039 ) ) ;
#26349 = ORIENTED_EDGE ( 'NONE', *, *, #41970, .T. ) ;
#26350 = CARTESIAN_POINT ( 'NONE',  ( 4.559911319644449179, 57.23035201082150536, -9.422509992056141925 ) ) ;
#26351 = CARTESIAN_POINT ( 'NONE',  ( 18.52753015748618282, 53.92559781766745175, -4.923371831947291888 ) ) ;
#26352 = CARTESIAN_POINT ( 'NONE',  ( -1.099225684535947600, 28.70696800326375353, -6.408140936763238038 ) ) ;
#26354 = DIRECTION ( 'NONE',  ( -0.000000000000000000, -0.000000000000000000, -1.000000000000000000 ) ) ;
#26353 = CARTESIAN_POINT ( 'NONE',  ( 20.88017736071110519, 5.563685344154837509, 2.639326808657452039E-16 ) ) ;
#26355 = CARTESIAN_POINT ( 'NONE',  ( 12.91533473730993009, 61.60535201082150536, -10.88017736071109987 ) ) ;
#26356 = CARTESIAN_POINT ( 'NONE',  ( 10.00000000000000000, 65.55374883491396076, -14.16423886937410082 ) ) ;
#26357 = AXIS2_PLACEMENT_3D ( 'NONE', #95249, #34239, #73234 ) ;
#26358 = CARTESIAN_POINT ( 'NONE',  ( 13.43411237798106583, 37.66530133659708923, -12.81628187352647252 ) ) ;
#26359 = CARTESIAN_POINT ( 'NONE',  ( 15.44008868035555260, 34.73035201082151247, 9.422509992056143702 ) ) ;
#26360 = FACE_OUTER_BOUND ( 'NONE', #53578, .T. ) ;
#26361 = VERTEX_POINT ( 'NONE', #50108 ) ;
#26362 = TOROIDAL_SURFACE ( 'NONE', #80694, 14.49999999999999822, 0.5000000000000000000 ) ;
#26363 = CARTESIAN_POINT ( 'NONE',  ( 21.09922568453595559, 47.04030133659708923, -6.408140936763230044 ) ) ;
#26364 = CARTESIAN_POINT ( 'NONE',  ( 12.91533473730992121, 39.52201867748817676, 10.88017736071110164 ) ) ;
#26365 = EDGE_LOOP ( 'NONE', ( #87678, #78358, #24076, #69259, #35841, #71868 ) ) ;
#26366 = CARTESIAN_POINT ( 'NONE',  ( 0.2751277870542913062, 49.36607318730131055, -6.499999999999992006 ) ) ;
#26367 = CARTESIAN_POINT ( 'NONE',  ( 18.52753015748617571, 63.09226448433412315, 4.923371831947298993 ) ) ;
#26369 = CARTESIAN_POINT ( 'NONE',  ( 5.076628168052703671, 46.84226448433412315, 8.527530157486179263 ) ) ;
#26368 = CARTESIAN_POINT ( 'NONE',  ( 19.84674366389459621, 13.50893115100078568, 7.409399052514197653E-17 ) ) ;
#26370 = CARTESIAN_POINT ( 'NONE',  ( -10.79673003881345217, -98.50248976943588275, 3.750000000000000888 ) ) ;
#26371 = PLANE ( 'NONE',  #77652 ) ;
#26372 = CARTESIAN_POINT ( 'NONE',  ( 7.361572987183170547, 37.05059781766744464, 9.846743663894590881 ) ) ;
#26373 = LINE ( 'NONE', #64362, #71433 ) ;
#26374 = DIRECTION ( 'NONE',  ( -0.8320502943378436100, 0.5547001962252291474, -0.000000000000000000 ) ) ;
#26376 = CARTESIAN_POINT ( 'NONE',  ( 0.1532563361054082862, 1.217264484334117824, 2.638427012816831674 ) ) ;
#26375 = CARTESIAN_POINT ( 'NONE',  ( 10.00000000000000178, 22.25893115100078745, 9.846743663894594434 ) ) ;
#26378 = ORIENTED_EDGE ( 'NONE', *, *, #38881, .T. ) ;
#26377 = CARTESIAN_POINT ( 'NONE',  ( 17.20831665107776587, 64.13393115100079456, -7.208316651077762316 ) ) ;
#26379 = FILL_AREA_STYLE_COLOUR ( '', #83764 ) ;
#26380 = CARTESIAN_POINT ( 'NONE',  ( -1.099225684535947600, 29.54030133659708923, 6.408140936763237150 ) ) ;
#26381 = CARTESIAN_POINT ( 'NONE',  ( 1.472469842513823179, 45.59226448433412315, -4.923371831947296329 ) ) ;
#26382 = CARTESIAN_POINT ( 'NONE',  ( 3.014428414850136129, 6.576366962315981723, 11.25000000000000000 ) ) ;
#26383 = CARTESIAN_POINT ( 'NONE',  ( -0.3689425029237898834, 61.17874883491396076, -10.36894250292378850 ) ) ;
#26384 = CARTESIAN_POINT ( 'NONE',  ( 17.20831665107776587, 17.88393115100078745, 7.208316651077764980 ) ) ;
#26385 = CARTESIAN_POINT ( 'NONE',  ( 19.67862543671680697, 88.20241052560767514, 5.461907810393946683 ) ) ;
#26386 = CARTESIAN_POINT ( 'NONE',  ( -0.3689425029237881626, 62.42874883491396787, 10.36894250292379027 ) ) ;
#26387 = CARTESIAN_POINT ( 'NONE',  ( 5.076628168052704559, 55.17559781766745175, -8.527530157486179263 ) ) ;
#26388 = CARTESIAN_POINT ( 'NONE',  ( 7.084665262690076126, 4.105352010821503583, 10.88017736071109987 ) ) ;
#26389 = CARTESIAN_POINT ( 'NONE',  ( 13.79529636645031943, 35.34541550158063927, -14.16423886937409904 ) ) ;
#26390 = CARTESIAN_POINT ( 'NONE',  ( 24.16423886937409904, 44.09541550158063927, 3.795296366450317205 ) ) ;
#26391 = CARTESIAN_POINT ( 'NONE',  ( 12.54342190210046759, 14.76984988503095764, -8.116945096741293497 ) ) ;
#26393 = CARTESIAN_POINT ( 'NONE',  ( 5.076628168052704559, 55.17559781766745175, -8.527530157486179263 ) ) ;
#26392 = CARTESIAN_POINT ( 'NONE',  ( -7.993487411949188548, 0.04962888323599694979, -12.40005926694717786 ) ) ;
#26394 = CARTESIAN_POINT ( 'NONE',  ( 4.559911319644449179, 37.23035201082150536, -9.422509992056141925 ) ) ;
#26395 = PRESENTATION_LAYER_ASSIGNMENT (  '', '', ( #890 ) ) ;
#26396 = CARTESIAN_POINT ( 'NONE',  ( 20.00000000000000711, 96.99164844389140683, -4.500000004094268036 ) ) ;
#26397 = EDGE_CURVE ( 'NONE', #87849, #77456, #62846, .T. ) ;
#26398 = CARTESIAN_POINT ( 'NONE',  ( 3.591859063236763294, 63.29030133659708923, -11.09922568453595026 ) ) ;
#26399 = CARTESIAN_POINT ( 'NONE',  ( -3.795296366450300773, 2.845415501580633499, 14.16423886937410437 ) ) ;
#26400 = CARTESIAN_POINT ( 'NONE',  ( 18.52753015748618282, 58.92559781766745886, -4.923371831947291888 ) ) ;
#26401 = DIRECTION ( 'NONE',  ( -0.000000000000000000, -0.000000000000000000, 1.000000000000000000 ) ) ;
#26402 = ORIENTED_EDGE ( 'NONE', *, *, #93509, .T. ) ;
#26403 = AXIS2_PLACEMENT_3D ( 'NONE', #36138, #66645, #34153 ) ;
#26404 = CARTESIAN_POINT ( 'NONE',  ( -2.266590686148945544, 22.22041550158063572, 7.082119434687048631 ) ) ;
#26405 = LINE ( 'NONE', #3921, #5545 ) ;
#26407 = CARTESIAN_POINT ( 'NONE',  ( 18.72515096720577787, 46.07228050351031357, -6.499999999999891642 ) ) ;
#26406 = CARTESIAN_POINT ( 'NONE',  ( -3.521047174886991815, -6.414748048905294375, -2.500000000000000000 ) ) ;
#26408 = CARTESIAN_POINT ( 'NONE',  ( 19.42250999205614193, 20.14701867748817321, 5.440088680355555262 ) ) ;
#26409 = CARTESIAN_POINT ( 'NONE',  ( -2.816281873526471635, 18.91530133659708213, -3.434112377981056508 ) ) ;
#26410 = CARTESIAN_POINT ( 'NONE',  ( -46.94000000000001194, 92.00000000000000000, -8.999999999999998224 ) ) ;
#26411 = CARTESIAN_POINT ( 'NONE',  ( 10.00000000000000178, 7.258931151000785675, 9.846743663894594434 ) ) ;
#26412 = CARTESIAN_POINT ( 'NONE',  ( 6.910361961229144256, -84.29457034759302303, -3.999999999998390177 ) ) ;
#26413 = CARTESIAN_POINT ( 'NONE',  ( -2.266590686148945544, 32.22041550158063927, 7.082119434687048631 ) ) ;
#26414 = DIRECTION ( 'NONE',  ( 0.000000000000000000, 0.000000000000000000, -1.000000000000000000 ) ) ;
#26415 = CARTESIAN_POINT ( 'NONE',  ( -0.1503990784575407469, 17.22266099184918531, -6.262539305110056631 ) ) ;
#26416 = CARTESIAN_POINT ( 'NONE',  ( 19.42250999205614193, 10.14701867748816966, 5.440088680355555262 ) ) ;
#26417 = CARTESIAN_POINT ( 'NONE',  ( 12.79413655343697265, 0.2301508429231309272, -7.715718893782876897 ) ) ;
#26418 = CARTESIAN_POINT ( 'NONE',  ( 2.035157376598824452, 38.68868534415483396, 7.964842623401179544 ) ) ;
#26419 = CARTESIAN_POINT ( 'NONE',  ( 0.5774900079438607392, 38.48035201082150536, 5.440088680355550821 ) ) ;
#26420 = CARTESIAN_POINT ( 'NONE',  ( -1.099225684535947600, -1.293031996736246469, -6.408140936763238038 ) ) ;
#26421 = CARTESIAN_POINT ( 'NONE',  ( 0.1532563361054083140, 61.00893115100078745, 1.131784320476157264E-15 ) ) ;
#26422 = CARTESIAN_POINT ( 'NONE',  ( 0.000000000000000000, -97.00000000000000000, -4.000000000000000000 ) ) ;
#26423 = CARTESIAN_POINT ( 'NONE',  ( 2.791683348922240793, 11.63393115100078568, 7.208316651077764092 ) ) ;
#26424 = CARTESIAN_POINT ( 'NONE',  ( 18.72515096720571037, 50.05509018479936856, 6.499999999999982236 ) ) ;
#26425 = CARTESIAN_POINT ( 'NONE',  ( -0.8801773607111009756, 48.06368534415484817, 1.068504757029289695E-15 ) ) ;
#26426 = AXIS2_PLACEMENT_3D ( 'NONE', #35650, #42665, #81146 ) ;
#26427 = UNCERTAINTY_MEASURE_WITH_UNIT (LENGTH_MEASURE( 1.000000000000000082E-05 ), #64001, 'distance_accuracy_value', 'NONE');
#26428 = AXIS2_PLACEMENT_3D ( 'NONE', #81968, #76446, #97992 ) ;
#26429 = EDGE_CURVE ( 'NONE', #31758, #34270, #40951, .T. ) ;
#26430 = CARTESIAN_POINT ( 'NONE',  ( -2.816281873526473856, -0.6680319967362464695, 3.434112377981055619 ) ) ;
#26431 = CARTESIAN_POINT ( 'NONE',  ( 15.44008868035555260, 59.73035201082151247, 9.422509992056143702 ) ) ;
#26432 = B_SPLINE_CURVE_WITH_KNOTS ( 'NONE', 3,
 ( #59255, #89756, #74760, #6268, #53738, #46244, #768, #70725, #69733, #10217, #48194, #31714 ),
 .UNSPECIFIED., .F., .F.,
 ( 4, 2, 2, 2, 2, 4 ),
 ( 0.0003200197625851165816, 0.0008213128228309329870, 0.001322605883076749230, 0.002325192003568404050, 0.003327778124060059087, 0.004330364244551714557 ),
 .UNSPECIFIED. ) ;
#26433 = CIRCLE ( 'NONE', #96701, 0.2500000000000002220 ) ;
#26434 = CARTESIAN_POINT ( 'NONE',  ( 19.84674366389459266, 28.30059781766745886, 2.638427012816836559 ) ) ;
#26435 = CARTESIAN_POINT ( 'NONE',  ( 6.565887622018943937, 38.08196800326376064, -12.81628187352647608 ) ) ;
#26437 = CARTESIAN_POINT ( 'NONE',  ( -5.810213597521615370, 14.95037102642602278, -13.56092647078879310 ) ) ;
#26436 = CARTESIAN_POINT ( 'NONE',  ( 1.472469842513823179, 5.592264484334118713, -4.923371831947296329 ) ) ;
#26438 = EDGE_LOOP ( 'NONE', ( #35652, #40177, #2564, #2271, #1245, #98170 ) ) ;
#26439 = CARTESIAN_POINT ( 'NONE',  ( 1.821708436314924962, 16.66792564121896802, -6.500000000000007105 ) ) ;
#26440 = CARTESIAN_POINT ( 'NONE',  ( 12.91533473730993009, 11.60535201082150536, -10.88017736071109987 ) ) ;
#26441 = CARTESIAN_POINT ( 'NONE',  ( -3.541595367958713769, 0.000000000000000000, 4.146675399920569660 ) ) ;
#26442 = CARTESIAN_POINT ( 'NONE',  ( 17.20831665107776587, 34.13393115100078745, -7.208316651077762316 ) ) ;
#26443 =( NAMED_UNIT ( * ) PLANE_ANGLE_UNIT ( ) SI_UNIT ( $, .RADIAN. ) );
#26444 = CARTESIAN_POINT ( 'NONE',  ( -0.3689425029237898834, 66.17874883491396076, -10.36894250292378850 ) ) ;
#26445 = ORIENTED_EDGE ( 'NONE', *, *, #30927, .F. ) ;
#26446 = CARTESIAN_POINT ( 'NONE',  ( 2.035157376598824452, 18.68868534415484106, 7.964842623401179544 ) ) ;
#26447 = CARTESIAN_POINT ( 'NONE',  ( 20.88017736071110519, 15.56368534415483751, 2.639326808657452039E-16 ) ) ;
#26448 = FACE_OUTER_BOUND ( 'NONE', #64651, .T. ) ;
#26449 = EDGE_LOOP ( 'NONE', ( #46027, #98859, #74050, #30760, #9487, #98155 ) ) ;
#26450 = CARTESIAN_POINT ( 'NONE',  ( 1.472469842513823179, 61.42559781766745175, 4.923371831947296329 ) ) ;
#26451 = CARTESIAN_POINT ( 'NONE',  ( 2.035157376598822676, 17.43868534415483751, -7.964842623401177768 ) ) ;
#26452 = CARTESIAN_POINT ( 'NONE',  ( 19.84674366389459621, 58.50893115100078745, 7.409399052514197653E-17 ) ) ;
#26453 = VECTOR ( 'NONE', #92449, 999.9999999999998863 ) ;
#26454 = CARTESIAN_POINT ( 'NONE',  ( 4.879999999999991900, 76.07179676972444327, -4.250000000000000000 ) ) ;
#26455 = CARTESIAN_POINT ( 'NONE',  ( 19.38216949554541557, 52.24863466993041072, -9.382169495545420901 ) ) ;
#26456 = DIRECTION ( 'NONE',  ( 5.818595309480553908E-17, 1.000000000000000000, -0.000000000000000000 ) ) ;
#26457 = CARTESIAN_POINT ( 'NONE',  ( -2.266590686148945544, 36.38708216824730357, -7.082119434687050408 ) ) ;
#26458 = CARTESIAN_POINT ( 'NONE',  ( 0.5774900079438590739, 37.64701867748817676, -5.440088680355550821 ) ) ;
#26459 = CARTESIAN_POINT ( 'NONE',  ( -0.8801773607111009756, 18.06368534415484106, 1.068504757029289695E-15 ) ) ;
#26460 = CARTESIAN_POINT ( 'NONE',  ( 12.63842701281683034, 57.46726448433411605, 9.846743663894596210 ) ) ;
#26461 = CARTESIAN_POINT ( 'NONE',  ( 5.500000000000000000, 60.50000000000000711, 6.500000000000000888 ) ) ;
#26462 = CARTESIAN_POINT ( 'NONE',  ( 7.361572987183169658, 49.96726448433410894, -9.846743663894592657 ) ) ;
#26463 = FACE_OUTER_BOUND ( 'NONE', #5722, .T. ) ;
#26464 = CARTESIAN_POINT ( 'NONE',  ( 10.00000000000000178, 2.258931151000784787, 9.846743663894594434 ) ) ;
#26465 = CARTESIAN_POINT ( 'NONE',  ( -6.408140936763246032, -26.70969866340291077, -11.09922568453594316 ) ) ;
#26466 = VERTEX_POINT ( 'NONE', #69561 ) ;
#26467 = EDGE_CURVE ( 'NONE', #54753, #91690, #75620, .T. ) ;
#26468 = CARTESIAN_POINT ( 'NONE',  ( 4.559911319644449179, 18.89701867748817321, 9.422509992056141925 ) ) ;
#26469 = CARTESIAN_POINT ( 'NONE',  ( 7.361572987183170547, 17.05059781766745530, 9.846743663894590881 ) ) ;
#26470 = CARTESIAN_POINT ( 'NONE',  ( 22.81628187352648496, 1.831968003263753753, -3.434112377981050290 ) ) ;
#26472 = CARTESIAN_POINT ( 'NONE',  ( -0.8801773607110991993, 52.85535201082151247, -2.915334737309923874 ) ) ;
#26471 = CARTESIAN_POINT ( 'NONE',  ( 2.035157376598822676, 47.43868534415484817, -7.964842623401177768 ) ) ;
#26474 = CARTESIAN_POINT ( 'NONE',  ( 16.40814093676324603, 47.45696800326375353, -11.09922568453594671 ) ) ;
#26473 = CARTESIAN_POINT ( 'NONE',  ( 2.035157376598822676, 17.43868534415483751, -7.964842623401177768 ) ) ;
#26475 = CARTESIAN_POINT ( 'NONE',  ( 22.26659068614895176, 34.72041550158063927, -7.082119434687042414 ) ) ;
#26476 = AXIS2_PLACEMENT_3D ( 'NONE', #5266, #11765, #58225 ) ;
#26477 = EDGE_CURVE ( 'NONE', #27464, #66913, #79191, .T. ) ;
#26478 = CARTESIAN_POINT ( 'NONE',  ( 9.879999999999988347, 26.99999999999999645, -2.900000000000000799 ) ) ;
#26479 = CARTESIAN_POINT ( 'NONE',  ( 21.09922568453595559, 52.04030133659708923, -6.408140936763230044 ) ) ;
#26480 = ORIENTED_EDGE ( 'NONE', *, *, #27801, .F. ) ;
#26481 = CARTESIAN_POINT ( 'NONE',  ( 10.00000000000000178, 62.25893115100078745, 9.846743663894594434 ) ) ;
#26482 = CARTESIAN_POINT ( 'NONE',  ( -1.926860441876562025, 14.47997603579417536, -3.195792623639529761 ) ) ;
#26483 = CARTESIAN_POINT ( 'NONE',  ( 20.88017736071110519, 35.56368534415484106, 2.639326808657452039E-16 ) ) ;
#26484 = LINE ( 'NONE', #72472, #47360 ) ;
#26485 = EDGE_CURVE ( 'NONE', #70379, #79717, #58949, .T. ) ;
#26486 = VERTEX_POINT ( 'NONE', #52575 ) ;
#26488 = CARTESIAN_POINT ( 'NONE',  ( -5.078940136053647691, -28.66985681914853501, 2.499999999999999556 ) ) ;
#26487 = CARTESIAN_POINT ( 'NONE',  ( 7.361572987183170547, 7.050597817667451750, 9.846743663894590881 ) ) ;
#26489 = CARTESIAN_POINT ( 'NONE',  ( 1.472469842513823179, 11.42559781766745175, 4.923371831947296329 ) ) ;
#26490 = CARTESIAN_POINT ( 'NONE',  ( 17.20831665107776587, 27.88393115100078390, 7.208316651077764980 ) ) ;
#26491 = CARTESIAN_POINT ( 'NONE',  ( 18.52753015748617571, 8.092264484334117824, 4.923371831947298993 ) ) ;
#26492 = CARTESIAN_POINT ( 'NONE',  ( 0.1532563361054100626, 5.800597817667452638, -2.638427012816831230 ) ) ;
#26493 = CARTESIAN_POINT ( 'NONE',  ( 4.559911319644449179, 63.89701867748817676, 9.422509992056141925 ) ) ;
#26494 = CARTESIAN_POINT ( 'NONE',  ( -0.8801773607110991993, 57.85535201082149825, -2.915334737309923874 ) ) ;
#26495 = AXIS2_PLACEMENT_3D ( 'NONE', #78404, #18403, #25430 ) ;
#26497 = ORIENTED_EDGE ( 'NONE', *, *, #94550, .T. ) ;
#26496 = CARTESIAN_POINT ( 'NONE',  ( 1.472469842513823179, 20.59226448433411960, -4.923371831947296329 ) ) ;
#26498 = CIRCLE ( 'NONE', #82386, 4.190000000000001279 ) ;
#26499 = CARTESIAN_POINT ( 'NONE',  ( 5.817157072110707539, 14.63606918420059877, 13.82608706751094907 ) ) ;
#26500 = CARTESIAN_POINT ( 'NONE',  ( 10.00000000000000000, 59.75893115100078745, -9.846743663894594434 ) ) ;
#26501 = EDGE_LOOP ( 'NONE', ( #40752, #10524, #98098, #35603, #5438, #73377 ) ) ;
#26502 = VERTEX_POINT ( 'NONE', #92537 ) ;
#26503 = CARTESIAN_POINT ( 'NONE',  ( -12.03829478939432462, 15.00000000000000888, 8.307695547791295709 ) ) ;
#26504 = VECTOR ( 'NONE', #21211, 1000.000000000000000 ) ;
#26505 = CARTESIAN_POINT ( 'NONE',  ( 22.26659068614895176, 4.720415501580633943, -7.082119434687042414 ) ) ;
#26506 = UNCERTAINTY_MEASURE_WITH_UNIT (LENGTH_MEASURE( 1.000000000000000082E-05 ), #91207, 'distance_accuracy_value', 'NONE');
#26507 = CARTESIAN_POINT ( 'NONE',  ( -3.999999999999994671, 43.00000000000000711, -4.250000000000000000 ) ) ;
#26508 = CARTESIAN_POINT ( 'NONE',  ( 2.917880565312948704, 17.63708216824730357, 12.26659068614894643 ) ) ;
#26509 = CARTESIAN_POINT ( 'NONE',  ( -2.266590686148945544, 26.38708216824730357, -7.082119434687050408 ) ) ;
#26510 = CARTESIAN_POINT ( 'NONE',  ( 6.880000000000009663, 40.99999999999999289, -6.250000000000000000 ) ) ;
#26511 = CARTESIAN_POINT ( 'NONE',  ( -0.1503990784575242878, 59.24884699246888431, -6.262539305110083276 ) ) ;
#26512 = CARTESIAN_POINT ( 'NONE',  ( 2.035157376598822676, 32.43868534415483396, -7.964842623401177768 ) ) ;
#26513 = ORIENTED_EDGE ( 'NONE', *, *, #92438, .F. ) ;
#26514 = CARTESIAN_POINT ( 'NONE',  ( 5.076628168052704559, 20.17559781766745175, -8.527530157486179263 ) ) ;
#26516 = CARTESIAN_POINT ( 'NONE',  ( 19.84674366389459621, 13.50893115100078568, 7.409399052514197653E-17 ) ) ;
#26515 = CARTESIAN_POINT ( 'NONE',  ( 20.88017736071110519, 55.56368534415484817, 2.639326808657452039E-16 ) ) ;
#26517 = CARTESIAN_POINT ( 'NONE',  ( 6.565887622018943937, 48.08196800326375353, -12.81628187352647608 ) ) ;
#26518 = CARTESIAN_POINT ( 'NONE',  ( 0.1532563361054100626, 40.80059781766745886, -2.638427012816831230 ) ) ;
#26519 = CARTESIAN_POINT ( 'NONE',  ( 11.94720539484412569, 0.2306972965111893092, -8.972309510150163092 ) ) ;
#26520 = EDGE_CURVE ( 'NONE', #55863, #92145, #14604, .T. ) ;
#26521 = CARTESIAN_POINT ( 'NONE',  ( 10.00000000000000000, 27.87363466993042138, -12.81628187352647608 ) ) ;
#26522 = CARTESIAN_POINT ( 'NONE',  ( -7.082119434687044190, -32.36291783175269643, 12.26659068614894998 ) ) ;
#26523 = CARTESIAN_POINT ( 'NONE',  ( 1.472469842513823179, 30.59226448433411960, -4.923371831947296329 ) ) ;
#26524 = CARTESIAN_POINT ( 'NONE',  ( 13.79529636645031943, 10.34541550158063394, -14.16423886937409904 ) ) ;
#26525 = EDGE_LOOP ( 'NONE', ( #78739, #66967, #18864, #91131 ) ) ;
#26526 = ADVANCED_FACE ( 'NONE', ( #31050 ), #90840, .T. ) ;
#26527 = CARTESIAN_POINT ( 'NONE',  ( 12.91533473730992121, 44.52201867748816966, 10.88017736071110164 ) ) ;
#26528 = CARTESIAN_POINT ( 'NONE',  ( 7.084665262690076126, 54.10535201082151247, 10.88017736071109987 ) ) ;
#26529 = CARTESIAN_POINT ( 'NONE',  ( 20.36894250292379738, 39.92874883491396787, -10.36894250292379027 ) ) ;
#26530 = CARTESIAN_POINT ( 'NONE',  ( 19.84674366389459621, 58.50893115100078745, 7.409399052514197653E-17 ) ) ;
#26531 = CARTESIAN_POINT ( 'NONE',  ( 10.00000000000000000, 9.758931151000785675, -9.846743663894594434 ) ) ;
#26532 = B_SPLINE_CURVE_WITH_KNOTS ( 'NONE', 3,
 ( #79, #82053, #74553, #31992, #85514, #55512 ),
 .UNSPECIFIED., .F., .F.,
 ( 4, 2, 4 ),
 ( 0.0002800011564896231716, 0.0006862063972211615310, 0.001092411637952699728 ),
 .UNSPECIFIED. ) ;
#26534 = DIRECTION ( 'NONE',  ( 0.000000000000000000, 1.000000000000000000, 0.000000000000000000 ) ) ;
#26533 = CARTESIAN_POINT ( 'NONE',  ( 22.81628187352647785, 61.62363466993041783, 6.195893100308588602E-16 ) ) ;
#26535 = CARTESIAN_POINT ( 'NONE',  ( 10.00000000000000000, 46.81368534415484106, -10.88017736071110342 ) ) ;
#26536 = DIRECTION ( 'NONE',  ( -1.000000000000000000, 0.000000000000000000, 0.000000000000000000 ) ) ;
#26537 = CARTESIAN_POINT ( 'NONE',  ( 22.81628187352647785, 26.41530133659708923, 3.434112377981063169 ) ) ;
#26538 = CARTESIAN_POINT ( 'NONE',  ( 17.20831665107776587, 54.13393115100079456, -7.208316651077762316 ) ) ;
#26539 = CARTESIAN_POINT ( 'NONE',  ( -5.440088680355558814, 17.23035201082151602, -9.422509992056136596 ) ) ;
#26540 = CARTESIAN_POINT ( 'NONE',  ( 7.084665262690076126, 2.022018677488170990, -10.88017736071110164 ) ) ;
#26541 = CARTESIAN_POINT ( 'NONE',  ( 15.44008868035555793, 66.39701867748817676, -9.422509992056140149 ) ) ;
#26542 = AXIS2_PLACEMENT_3D ( 'NONE', #34036, #43034, #65019 ) ;
#26543 = CARTESIAN_POINT ( 'NONE',  ( -8.647950603703787209, -15.58161425315404180, 4.000000000000000000 ) ) ;
#26544 = CARTESIAN_POINT ( 'NONE',  ( 1.274849032794305170, 12.55509018479935968, -6.499999999999995559 ) ) ;
#26545 = CARTESIAN_POINT ( 'NONE',  ( 17.96484262340118221, 64.93868534415483396, 7.964842623401181321 ) ) ;
#26546 = CARTESIAN_POINT ( 'NONE',  ( -0.8801773607110991993, 67.85535201082151957, -2.915334737309923874 ) ) ;
#26547 = DIRECTION ( 'NONE',  ( 0.000000000000000000, 1.000000000000000000, 0.000000000000000000 ) ) ;
#26548 = EDGE_CURVE ( 'NONE', #79151, #22706, #63723, .T. ) ;
#26549 = CARTESIAN_POINT ( 'NONE',  ( 2.791683348922240793, 36.63393115100078035, 7.208316651077764092 ) ) ;
#26550 = CARTESIAN_POINT ( 'NONE',  ( 17.96484262340118221, 24.93868534415484461, 7.964842623401181321 ) ) ;
#26551 = CARTESIAN_POINT ( 'NONE',  ( 19.38216949554541202, 0.9986346699304200492, 9.382169495545424454 ) ) ;
#26553 = CARTESIAN_POINT ( 'NONE',  ( 18.72515096720583827, 56.07228050351029225, -6.499999999999802824 ) ) ;
#26552 = CARTESIAN_POINT ( 'NONE',  ( 17.96484262340118221, 31.18868534415483751, -7.964842623401177768 ) ) ;
#26554 = CARTESIAN_POINT ( 'NONE',  ( 0.6178305044545818747, 33.49863466993042493, -9.382169495545419124 ) ) ;
#26555 = VERTEX_POINT ( 'NONE', #54535 ) ;
#26556 = CARTESIAN_POINT ( 'NONE',  ( -0.8801773607111008646, 53.27201867748816966, 2.915334737309923430 ) ) ;
#26557 = EDGE_CURVE ( 'NONE', #77887, #27971, #44580, .T. ) ;
#26559 = DIRECTION ( 'NONE',  ( -0.09584575252022722869, 0.000000000000000000, 0.9953961983671785196 ) ) ;
#26558 = CARTESIAN_POINT ( 'NONE',  ( 6.565887622018943937, 23.08196800326375708, -12.81628187352647608 ) ) ;
#26560 = CARTESIAN_POINT ( 'NONE',  ( 7.084665262690076126, 22.02201867748817321, -10.88017736071110164 ) ) ;
#26561 = CARTESIAN_POINT ( 'NONE',  ( 13.79529636645031943, 60.34541550158063927, -14.16423886937409904 ) ) ;
#26562 = CARTESIAN_POINT ( 'NONE',  ( 5.076628168052703671, 46.84226448433412315, 8.527530157486179263 ) ) ;
#26563 = CARTESIAN_POINT ( 'NONE',  ( 12.63842701281683922, 4.550597817667451750, -9.846743663894590881 ) ) ;
#26564 = CARTESIAN_POINT ( 'NONE',  ( 4.559911319644449179, 57.23035201082150536, -9.422509992056141925 ) ) ;
#26565 = DIRECTION ( 'NONE',  ( -1.000000000000000000, 3.035766082959409891E-14, 0.000000000000000000 ) ) ;
#26566 = CARTESIAN_POINT ( 'NONE',  ( 22.26659068614894466, 33.88708216824730357, 7.082119434687054849 ) ) ;
#26567 = PRESENTATION_LAYER_ASSIGNMENT (  '', '', ( #34547 ) ) ;
#26568 =( BOUNDED_SURFACE ( )  B_SPLINE_SURFACE ( 3, 2, ( 
 ( #16942, #77421, #31427 ),
 ( #17445, #92921, #38955 ),
 ( #84939, #61931, #92432 ),
 ( #23956, #78417, #93916 ),
 ( #54430, #69447, #1956 ),
 ( #967, #54918, #62921 ),
 ( #8935, #25443, #70938 ),
 ( #39452, #32420, #77925 ),
 ( #69944, #93422, #76455 ),
 ( #23476, #7970, #15482 ),
 ( #493, #91945, #85433 ),
 ( #24944, #1464, #31916 ),
 ( #62417, #24452, #9934 ),
 ( #63411, #32911, #55926 ),
 ( #71896, #72382, #29225 ),
 ( #87878, #57872, #79412 ),
 ( #4410, #42397, #26892 ),
 ( #56419, #25917, #80393 ) ),
 .UNSPECIFIED., .F., .F., .T. ) 
 B_SPLINE_SURFACE_WITH_KNOTS ( ( 4, 2, 2, 2, 2, 2, 2, 2, 4 ),
 ( 3, 3 ),
 ( 0.000000000000000000, 0.002783459421197213672, 0.005566918842394427344, 0.01113383768478885469, 0.02226767536957770938, 0.04453535073915541875, 0.06680302610873312119, 0.07793686379352197935, 0.08907070147831083751 ),
 ( 0.000000000000000000, 1.000000000000000000 ),
 .UNSPECIFIED. ) 
 GEOMETRIC_REPRESENTATION_ITEM ( )  RATIONAL_B_SPLINE_SURFACE ( (
 ( 1.000000000000000000, 0.7071067811865482389, 1.000000000000000000),
 ( 1.000000000000000000, 0.7071067811865482389, 1.000000000000000000),
 ( 1.000000000000000000, 0.7071067811865482389, 1.000000000000000000),
 ( 1.000000000000000000, 0.7071067811865482389, 1.000000000000000000),
 ( 1.000000000000000000, 0.7071067811865482389, 1.000000000000000000),
 ( 1.000000000000000000, 0.7071067811865482389, 1.000000000000000000),
 ( 1.000000000000000000, 0.7071067811865482389, 1.000000000000000000),
 ( 1.000000000000000000, 0.7071067811865482389, 1.000000000000000000),
 ( 1.000000000000000000, 0.7071067811865482389, 1.000000000000000000),
 ( 1.000000000000000000, 0.7071067811865482389, 1.000000000000000000),
 ( 1.000000000000000000, 0.7071067811865465735, 1.000000000000000000),
 ( 1.000000000000000000, 0.7071067811865465735, 1.000000000000000000),
 ( 1.000000000000000000, 0.7071067811865482389, 1.000000000000000000),
 ( 1.000000000000000000, 0.7071067811865482389, 1.000000000000000000),
 ( 1.000000000000000000, 0.7071067811865482389, 1.000000000000000000),
 ( 1.000000000000000000, 0.7071067811865482389, 1.000000000000000000),
 ( 1.000000000000000000, 0.7071067811865476838, 1.000000000000000000),
 ( 1.000000000000000000, 0.7071067811865476838, 1.000000000000000000) ) ) 
 REPRESENTATION_ITEM ( '' )  SURFACE ( )  );
#26569 = ORIENTED_EDGE ( 'NONE', *, *, #88174, .F. ) ;
#26570 = CARTESIAN_POINT ( 'NONE',  ( 6.204703633549690345, 47.84541550158064638, 14.16423886937410082 ) ) ;
#26571 = CARTESIAN_POINT ( 'NONE',  ( 10.00000000000000178, 53.05374883491396787, 14.16423886937410082 ) ) ;
#26572 = CARTESIAN_POINT ( 'NONE',  ( 0.1532563361054083140, 16.00893115100078390, 1.131784320476157264E-15 ) ) ;
#26573 = CARTESIAN_POINT ( 'NONE',  ( 22.81628187352648496, 16.83196800326374998, -3.434112377981050290 ) ) ;
#26574 = DIRECTION ( 'NONE',  ( -1.000000000000000000, 0.000000000000000000, 0.000000000000000000 ) ) ;
#26575 = LINE ( 'NONE', #11094, #3566 ) ;
#26577 = CARTESIAN_POINT ( 'NONE',  ( 0.6178305044545818747, 33.49863466993042493, -9.382169495545419124 ) ) ;
#26576 = CARTESIAN_POINT ( 'NONE',  ( 15.44008868035555793, 66.39701867748817676, -9.422509992056140149 ) ) ;
#26578 = CARTESIAN_POINT ( 'NONE',  ( 22.26659068614894466, 38.88708216824731068, 7.082119434687054849 ) ) ;
#26579 = VECTOR ( 'NONE', #86149, 1000.000000000000000 ) ;
#26580 = B_SPLINE_CURVE_WITH_KNOTS ( 'NONE', 3,
 ( #59194, #11732, #26731, #3758, #66710, #34216 ),
 .UNSPECIFIED., .F., .F.,
 ( 4, 2, 4 ),
 ( 3.409110551495777647E-05, 0.0004400426677367824516, 0.0008459942299586071471 ),
 .UNSPECIFIED. ) ;
#26581 =( BOUNDED_SURFACE ( )  B_SPLINE_SURFACE ( 1, 2, ( 
 ( #74364, #91350, #52857, #68374, #67373, #45357, #5893, #58881, #83365, #6876, #51884, #53348, #97903, #52367, #90852, #36385, #21387, #59864, #66880, #14888, #98893, #81872, #89383, #90351, #5411, #43382, #21889, #13888, #44856, #82872, #97397, #37387, #22877, #14386, #98398, #59369, #22383, #12885, #73881, #75862, #7383, #30344, #20896, #60851, #51386, #61343, #69845, #32805, #32313, #63301, #62818, #31820, #84841, #15380, #45865, #7870, #9831, #23369, #62318, #24354, #16842, #54817, #77816, #30845, #68863, #92824, #39833, #70836, #40333, #93810, #83856, #16349, #395, #70339, #46831, #77323, #92339, #17342, #8351, #23863, #91854, #85328, #25340, #78312, #76355, #47316, #9331, #8837, #39351, #1369, #1856, #93316, #46349, #76836, #2349, #24838, #47812, #38365, #55321, #85827, #69348, #53855, #84365, #15864, #38859, #54327, #872, #31331, #61831, #57281, #3308, #63786, #74626, #19290, #86811, #80284, #56792, #56315, #95282, #5655, #18807, #49290, #36643, #13633, #49777, #25818, #11784, #42292, #40822, #79790, #87775, #17822, #44117, #94295, #48304, #55824, #21142, #86318, #33295, #26783, #64768, #74119, #18315, #48795, #79304, #11293, #59122, #6140, #41330, #26291, #41812, #72280, #67128, #78812, #97165, #97655, #10320, #64278, #3810, #28633, #10812, #51642, #36133, #66641, #89631, #71322, #82123, #94790, #71803, #2840, #33771, #87287, #34266, #37142, #44625, #22632, #29119, #22135, #52617, #46114, #7641, #61587, #83118, #21645, #31092, #8117, #91105, #38131, #16106, #98145, #69600, #37631, #52129, #59620, #98656, #60110, #69110, #82626, #6628, #23127, #91611, #46592, #67636, #14140, #14647, #84605, #75120, #15136, #53112, #53601, #83620, #29606, #76110, #77091, #84115, #15631, #8600, #90611, #45110, #75616, #39110, #7126, #45612, #68619, #76600, #149, #68128, #30596, #90118, #38612, #60610, #61102, #643, #92098, #23629, #30102, #54090, #94553, #17593, #64040, #92584, #71081, #63068, #85588, #78575, #48555, #70095, #86082, #70586, #17101, #25101, #24108, #2607, #47586, #9091, #18566, #63556, #32067, #25587, #2113, #1618, #40584, #79056, #93568, #55586, #79562, #56561, #94065, #62570, #56079, #86573, #85093, #48061, #33061, #62076, #87055, #39607, #54578, #1121, #26071, #31583, #77576, #18078, #10085, #10571, #93075, #24604, #55070, #41079, #3087, #49058, #78080, #32571, #71577, #33544, #11061, #16602, #41581, #47078, #9584, #40085, #73023, #96544, #72527, #58518, #43033, #5043, #28020, #34035, #58020, #57534, #80041, #95037, #81513, #35526, #19543, #19056, #26546, #12039, #72049, #4061, #34524, #66020, #96045, #89027 ),
 ( #64530, #3578, #4557, #27035, #51021, #11547, #65018, #50039, #13020, #5541, #95547, #42067, #35021, #49534, #87545, #88528, #65522, #20537, #20030, #88031, #43518, #57042, #74013, #80542, #50532, #42539, #27529, #12533, #81027, #73514, #85904, #39909, #94867, #63860, #70412, #48382, #11370, #10885, #41892, #41409, #10395, #63383, #92897, #24428, #85407, #87368, #1932, #40899, #2916, #94374, #33366, #56392, #9407, #47393, #71400, #18389, #49364, #18883, #72352, #62389, #93887, #77895, #48868, #25415, #55899, #70907, #26368, #17418, #2427, #32389, #25893, #3884, #56867, #54892, #86879, #32884, #16917, #17899, #79866, #62894, #93393, #24918, #79380, #86396, #55403, #71873, #47887, #3385, #33850, #64358, #78389, #78884, #9910, #40412, #98048, #34504, #72023, #24584, #10546, #57019, #85564, #64017, #56056, #78550, #71555, #41559, #63048, #79033, #63535, #10061, #18055, #17076, #94530, #40559, #2087, #11522, #56539, #25077, #18541, #94042, #93544, #33521, #3553, #86550, #48533, #72509, #49512, #87029, #55559, #49033, #79538, #78057, #41057, #26049, #55045, #3068, #42045, #34013, #4042, #64510, #11037, #25565, #47559, #9559, #40060, #19036, #32547, #95014, #26523, #87521, #80019, #93050, #70561, #86060, #17571, #48038, #71059, #2583, #33038, #64996, #65997, #80522, #51496, #96525, #27997, #73492, #97517, #88506, #5019, #12020, #35997, #14005, #59484, #27015, #66499, #35503, #57514, #20513, #82488, #51998, #65501, #27505, #97025, #58496, #28980, #12996, #96023, #28502, #58996, #21009, #74985, #50998, #4535, #74485, #81493, #58000, #43982, #89984, #42520, #20009, #89006, #43493, #89498, #81991, #13502, #6007, #36502, #73003, #50511, #19523, #43010, #88010, #34998, #66994, #73993, #50018, #81008, #12509, #44483, #21501, #6488, #5519, #95523, #37497, #59974, #76950, #30952, #75970, #77433, #22992, #76465, #53960, #98513, #45469, #68483, #90961, #8461, #61942, #6993, #52478, #10, #29467, #67492, #91467, #7498, #68972, #53458, #67986, #61451, #16460, #83966, #30458, #29966, #60957, #46940, #98013, #60472, #22493, #52966, #14503, #69459, #38479, #44973, #37991, #504, #15493, #83478, #91958, #36995, #45975, #7980, #14999, #23488, #90468, #22003, #84467, #15965, #46457, #75479, #978, #38966, #31441, #92443, #84949, #23966, #82983, #54440, #55936, #9944, #39464, #69954, #31927, #33888, #47437, #86436, #48420, #40940, #78922, #2952, #54928, #92930, #17935, #63899, #94904, #64393, #56901, #8946, #40447, #24463, #94412, #70948, #2466, #17455, #41445, #32430, #47922, #85444, #10432, #87406, #3429, #1473, #71438, #78427, #62427, #63424 ) ),
 .UNSPECIFIED., .F., .F., .F. ) 
 B_SPLINE_SURFACE_WITH_KNOTS ( ( 2, 2 ),
 ( 3, 2, 2, 2, 2, 2, 2, 2, 2, 2, 2, 2, 2, 2, 2, 2, 2, 2, 2, 2, 2, 2, 2, 2, 2, 2, 2, 2, 2, 2, 2, 2, 2, 2, 2, 2, 2, 2, 2, 2, 2, 2, 2, 2, 2, 2, 2, 2, 2, 2, 2, 2, 2, 2, 2, 2, 2, 2, 2, 2, 2, 2, 2, 2, 2, 2, 2, 2, 2, 2, 2, 2, 2, 2, 2, 2, 2, 2, 2, 2, 2, 2, 2, 2, 2, 2, 2, 2, 2, 2, 2, 2, 2, 2, 2, 2, 2, 2, 2, 2, 2, 2, 2, 2, 2, 2, 2, 2, 2, 2, 2, 2, 2, 2, 2, 2, 2, 2, 2, 2, 2, 2, 2, 2, 2, 2, 2, 2, 2, 2, 2, 2, 2, 2, 2, 2, 2, 2, 2, 2, 2, 2, 2, 2, 2, 2, 2, 2, 2, 2, 2, 2, 2, 2, 2, 2, 2, 2, 2, 2, 2, 2, 3 ),
 ( 0.000000000000000000, 1.000000000000000000 ),
 ( 0.000000000000000000, 0.005952380952380952051, 0.01190476190476190410, 0.01785714285714285615, 0.02380952380952380820, 0.02976190476190476025, 0.03571428571428571230, 0.04166666666666666435, 0.04761904761904761640, 0.05357142857142856845, 0.05952380952380952051, 0.06547619047619047949, 0.07142857142857142461, 0.07738095238095238360, 0.08333333333333332871, 0.08928571428571428770, 0.09523809523809523281, 0.1011904761904761918, 0.1071428571428571369, 0.1130952380952380959, 0.1190476190476190410, 0.1250000000000000000, 0.1309523809523809590, 0.1369047619047619180, 0.1428571428571428492, 0.1488095238095238082, 0.1547619047619047672, 0.1607142857142857262, 0.1666666666666666574, 0.1726190476190476164, 0.1785714285714285754, 0.1845238095238095344, 0.1904761904761904656, 0.1964285714285714246, 0.2023809523809523836, 0.2083333333333333426, 0.2142857142857142738, 0.2202380952380952328, 0.2261904761904761918, 0.2321428571428571508, 0.2380952380952380820, 0.2440476190476190410, 0.2500000000000000000, 0.2559523809523809312, 0.2619047619047619180, 0.2678571428571428492, 0.2738095238095238360, 0.2797619047619047672, 0.2857142857142856984, 0.2916666666666666852, 0.2976190476190476164, 0.3035714285714285476, 0.3095238095238095344, 0.3154761904761904656, 0.3214285714285714524, 0.3273809523809523836, 0.3333333333333333148, 0.3392857142857143016, 0.3452380952380952328, 0.3511904761904761640, 0.3571428571428571508, 0.3630952380952380820, 0.3690476190476190688, 0.3750000000000000000, 0.3809523809523809312, 0.3869047619047619180, 0.3928571428571428492, 0.3988095238095238360, 0.4047619047619047672, 0.4107142857142856984, 0.4166666666666666852, 0.4226190476190476164, 0.4285714285714285476, 0.4345238095238095344, 0.4404761904761904656, 0.4464285714285714524, 0.4523809523809523836, 0.4583333333333333148, 0.4642857142857143016, 0.4702380952380952328, 0.4761904761904761640, 0.4821428571428571508, 0.4880952380952380820, 0.4940476190476190688, 0.5000000000000000000, 0.5059523809523809312, 0.5119047619047618625, 0.5178571428571429047, 0.5238095238095238360, 0.5297619047619047672, 0.5357142857142856984, 0.5416666666666666297, 0.5476190476190476719, 0.5535714285714286031, 0.5595238095238095344, 0.5654761904761904656, 0.5714285714285713969, 0.5773809523809523281, 0.5833333333333333703, 0.5892857142857143016, 0.5952380952380952328, 0.6011904761904761640, 0.6071428571428570953, 0.6130952380952381375, 0.6190476190476190688, 0.6250000000000000000, 0.6309523809523809312, 0.6369047619047618625, 0.6428571428571429047, 0.6488095238095238360, 0.6547619047619047672, 0.6607142857142856984, 0.6666666666666666297, 0.6726190476190476719, 0.6785714285714286031, 0.6845238095238095344, 0.6904761904761904656, 0.6964285714285713969, 0.7023809523809523281, 0.7083333333333333703, 0.7142857142857143016, 0.7202380952380952328, 0.7261904761904761640, 0.7321428571428570953, 0.7380952380952381375, 0.7440476190476190688, 0.7500000000000000000, 0.7559523809523809312, 0.7619047619047618625, 0.7678571428571429047, 0.7738095238095238360, 0.7797619047619047672, 0.7857142857142856984, 0.7916666666666666297, 0.7976190476190476719, 0.8035714285714286031, 0.8095238095238095344, 0.8154761904761904656, 0.8214285714285713969, 0.8273809523809523281, 0.8333333333333333703, 0.8392857142857143016, 0.8452380952380952328, 0.8511904761904761640, 0.8571428571428570953, 0.8630952380952381375, 0.8690476190476190688, 0.8750000000000000000, 0.8809523809523809312, 0.8869047619047618625, 0.8928571428571429047, 0.8988095238095238360, 0.9047619047619047672, 0.9107142857142856984, 0.9166666666666666297, 0.9226190476190476719, 0.9285714285714286031, 0.9345238095238095344, 0.9404761904761904656, 0.9464285714285713969, 0.9523809523809523281, 0.9583333333333333703, 0.9642857142857143016 ),
 .UNSPECIFIED. ) 
 GEOMETRIC_REPRESENTATION_ITEM ( )  RATIONAL_B_SPLINE_SURFACE ( (
 ( 1.000000000000000000, 0.9659258262890683122, 1.000000000000000000, 0.9659258262890683122, 1.000000000000000000, 0.9659258262890683122, 1.000000000000000000, 0.9659258262890683122, 1.000000000000000000, 0.9659258262890683122, 1.000000000000000000, 0.9659258262890683122, 1.000000000000000000, 0.9659258262890683122, 1.000000000000000000, 0.9659258262890683122, 1.000000000000000000, 0.9659258262890683122, 1.000000000000000000, 0.9659258262890683122, 1.000000000000000000, 0.9659258262890683122, 1.000000000000000000, 0.9659258262890683122, 1.000000000000000000, 0.9659258262890683122, 1.000000000000000000, 0.9659258262890683122, 1.000000000000000000, 0.9659258262890683122, 1.000000000000000000, 0.9659258262890683122, 1.000000000000000000, 0.9659258262890683122, 1.000000000000000000, 0.9659258262890683122, 1.000000000000000000, 0.9659258262890683122, 1.000000000000000000, 0.9659258262890683122, 1.000000000000000000, 0.9659258262890683122, 1.000000000000000000, 0.9659258262890683122, 1.000000000000000000, 0.9659258262890683122, 1.000000000000000000, 0.9659258262890683122, 1.000000000000000000, 0.9659258262890683122, 1.000000000000000000, 0.9659258262890683122, 1.000000000000000000, 0.9659258262890683122, 1.000000000000000000, 0.9659258262890683122, 1.000000000000000000, 0.9659258262890683122, 1.000000000000000000, 0.9659258262890683122, 1.000000000000000000, 0.9659258262890683122, 1.000000000000000000, 0.9659258262890683122, 1.000000000000000000, 0.9659258262890683122, 1.000000000000000000, 0.9659258262890683122, 1.000000000000000000, 0.9659258262890683122, 1.000000000000000000, 0.9659258262890683122, 1.000000000000000000, 0.9659258262890683122, 1.000000000000000000, 0.9659258262890683122, 1.000000000000000000, 0.9659258262890683122, 1.000000000000000000, 0.9659258262890683122, 1.000000000000000000, 0.9659258262890683122, 1.000000000000000000, 0.9659258262890683122, 1.000000000000000000, 0.9659258262890683122, 1.000000000000000000, 0.9659258262890683122, 1.000000000000000000, 0.9659258262890683122, 1.000000000000000000, 0.9659258262890683122, 1.000000000000000000, 0.9659258262890683122, 1.000000000000000000, 0.9659258262890683122, 1.000000000000000000, 0.9659258262890683122, 1.000000000000000000, 0.9659258262890683122, 1.000000000000000000, 0.9659258262890683122, 1.000000000000000000, 0.9659258262890683122, 1.000000000000000000, 0.9659258262890683122, 1.000000000000000000, 0.9659258262890683122, 1.000000000000000000, 0.9659258262890683122, 1.000000000000000000, 0.9659258262890683122, 1.000000000000000000, 0.9659258262890683122, 1.000000000000000000, 0.9659258262890683122, 1.000000000000000000, 0.9659258262890683122, 1.000000000000000000, 0.9659258262890683122, 1.000000000000000000, 0.9659258262890683122, 1.000000000000000000, 0.9659258262890683122, 1.000000000000000000, 0.9659258262890683122, 1.000000000000000000, 0.9659258262890683122, 1.000000000000000000, 0.9659258262890683122, 1.000000000000000000, 0.9659258262890683122, 1.000000000000000000, 0.9659258262890683122, 1.000000000000000000, 0.9659258262890683122, 1.000000000000000000, 0.9659258262890683122, 1.000000000000000000, 0.9659258262890683122, 1.000000000000000000, 0.9659258262890683122, 1.000000000000000000, 0.9659258262890683122, 1.000000000000000000, 0.9659258262890683122, 1.000000000000000000, 0.9659258262890683122, 1.000000000000000000, 0.9659258262890683122, 1.000000000000000000, 0.9659258262890683122, 1.000000000000000000, 0.9659258262890683122, 1.000000000000000000, 0.9659258262890683122, 1.000000000000000000, 0.9659258262890683122, 1.000000000000000000, 0.9659258262890683122, 1.000000000000000000, 0.9659258262890683122, 1.000000000000000000, 0.9659258262890683122, 1.000000000000000000, 0.9659258262890683122, 1.000000000000000000, 0.9659258262890683122, 1.000000000000000000, 0.9659258262890683122, 1.000000000000000000, 0.9659258262890683122, 1.000000000000000000, 0.9659258262890683122, 1.000000000000000000, 0.9659258262890683122, 1.000000000000000000, 0.9659258262890683122, 1.000000000000000000, 0.9659258262890683122, 1.000000000000000000, 0.9659258262890683122, 1.000000000000000000, 0.9659258262890683122, 1.000000000000000000, 0.9659258262890683122, 1.000000000000000000, 0.9659258262890683122, 1.000000000000000000, 0.9659258262890683122, 1.000000000000000000, 0.9659258262890683122, 1.000000000000000000, 0.9659258262890683122, 1.000000000000000000, 0.9659258262890683122, 1.000000000000000000, 0.9659258262890683122, 1.000000000000000000, 0.9659258262890683122, 1.000000000000000000, 0.9659258262890683122, 1.000000000000000000, 0.9659258262890683122, 1.000000000000000000, 0.9659258262890683122, 1.000000000000000000, 0.9659258262890683122, 1.000000000000000000, 0.9659258262890683122, 1.000000000000000000, 0.9659258262890683122, 1.000000000000000000, 0.9659258262890683122, 1.000000000000000000, 0.9659258262890683122, 1.000000000000000000, 0.9659258262890683122, 1.000000000000000000, 0.9659258262890683122, 1.000000000000000000, 0.9659258262890683122, 1.000000000000000000, 0.9659258262890683122, 1.000000000000000000, 0.9659258262890683122, 1.000000000000000000, 0.9659258262890683122, 1.000000000000000000, 0.9659258262890683122, 1.000000000000000000, 0.9659258262890683122, 1.000000000000000000, 0.9659258262890683122, 1.000000000000000000, 0.9659258262890683122, 1.000000000000000000, 0.9659258262890683122, 1.000000000000000000, 0.9659258262890683122, 1.000000000000000000, 0.9659258262890683122, 1.000000000000000000, 0.9659258262890683122, 1.000000000000000000, 0.9659258262890683122, 1.000000000000000000, 0.9659258262890683122, 1.000000000000000000, 0.9659258262890683122, 1.000000000000000000, 0.9659258262890683122, 1.000000000000000000, 0.9659258262890683122, 1.000000000000000000, 0.9659258262890683122, 1.000000000000000000, 0.9659258262890683122, 1.000000000000000000, 0.9659258262890683122, 1.000000000000000000, 0.9659258262890683122, 1.000000000000000000, 0.9659258262890683122, 1.000000000000000000, 0.9659258262890683122, 1.000000000000000000, 0.9659258262890683122, 1.000000000000000000, 0.9659258262890683122, 1.000000000000000000, 0.9659258262890683122, 1.000000000000000000, 0.9659258262890683122, 1.000000000000000000, 0.9659258262890683122, 1.000000000000000000, 0.9659258262890683122, 1.000000000000000000, 0.9659258262890683122, 1.000000000000000000, 0.9659258262890683122, 1.000000000000000000, 0.9659258262890683122, 1.000000000000000000, 0.9659258262890683122, 1.000000000000000000, 0.9659258262890683122, 1.000000000000000000, 0.9659258262890683122, 1.000000000000000000, 0.9659258262890683122, 1.000000000000000000, 0.9659258262890683122, 1.000000000000000000, 0.9659258262890683122, 1.000000000000000000, 0.9659258262890683122, 1.000000000000000000, 0.9659258262890683122, 1.000000000000000000, 0.9659258262890683122, 1.000000000000000000, 0.9659258262890683122, 1.000000000000000000, 0.9659258262890683122, 1.000000000000000000, 0.9659258262890683122, 1.000000000000000000, 0.9659258262890683122, 1.000000000000000000, 0.9659258262890683122, 1.000000000000000000, 0.9659258262890683122, 1.000000000000000000, 0.9659258262890683122, 1.000000000000000000, 0.9659258262890683122, 1.000000000000000000, 0.9659258262890683122, 1.000000000000000000, 0.9659258262890683122, 1.000000000000000000, 0.9659258262890683122, 1.000000000000000000),
 ( 1.000000000000000000, 0.9659258262890683122, 1.000000000000000000, 0.9659258262890683122, 1.000000000000000000, 0.9659258262890683122, 1.000000000000000000, 0.9659258262890683122, 1.000000000000000000, 0.9659258262890683122, 1.000000000000000000, 0.9659258262890683122, 1.000000000000000000, 0.9659258262890683122, 1.000000000000000000, 0.9659258262890683122, 1.000000000000000000, 0.9659258262890683122, 1.000000000000000000, 0.9659258262890683122, 1.000000000000000000, 0.9659258262890683122, 1.000000000000000000, 0.9659258262890683122, 1.000000000000000000, 0.9659258262890683122, 1.000000000000000000, 0.9659258262890683122, 1.000000000000000000, 0.9659258262890683122, 1.000000000000000000, 0.9659258262890683122, 1.000000000000000000, 0.9659258262890683122, 1.000000000000000000, 0.9659258262890683122, 1.000000000000000000, 0.9659258262890683122, 1.000000000000000000, 0.9659258262890683122, 1.000000000000000000, 0.9659258262890683122, 1.000000000000000000, 0.9659258262890683122, 1.000000000000000000, 0.9659258262890683122, 1.000000000000000000, 0.9659258262890683122, 1.000000000000000000, 0.9659258262890683122, 1.000000000000000000, 0.9659258262890683122, 1.000000000000000000, 0.9659258262890683122, 1.000000000000000000, 0.9659258262890683122, 1.000000000000000000, 0.9659258262890683122, 1.000000000000000000, 0.9659258262890683122, 1.000000000000000000, 0.9659258262890683122, 1.000000000000000000, 0.9659258262890683122, 1.000000000000000000, 0.9659258262890683122, 1.000000000000000000, 0.9659258262890683122, 1.000000000000000000, 0.9659258262890683122, 1.000000000000000000, 0.9659258262890683122, 1.000000000000000000, 0.9659258262890683122, 1.000000000000000000, 0.9659258262890683122, 1.000000000000000000, 0.9659258262890683122, 1.000000000000000000, 0.9659258262890683122, 1.000000000000000000, 0.9659258262890683122, 1.000000000000000000, 0.9659258262890683122, 1.000000000000000000, 0.9659258262890683122, 1.000000000000000000, 0.9659258262890683122, 1.000000000000000000, 0.9659258262890683122, 1.000000000000000000, 0.9659258262890683122, 1.000000000000000000, 0.9659258262890683122, 1.000000000000000000, 0.9659258262890683122, 1.000000000000000000, 0.9659258262890683122, 1.000000000000000000, 0.9659258262890683122, 1.000000000000000000, 0.9659258262890683122, 1.000000000000000000, 0.9659258262890683122, 1.000000000000000000, 0.9659258262890683122, 1.000000000000000000, 0.9659258262890683122, 1.000000000000000000, 0.9659258262890683122, 1.000000000000000000, 0.9659258262890683122, 1.000000000000000000, 0.9659258262890683122, 1.000000000000000000, 0.9659258262890683122, 1.000000000000000000, 0.9659258262890683122, 1.000000000000000000, 0.9659258262890683122, 1.000000000000000000, 0.9659258262890683122, 1.000000000000000000, 0.9659258262890683122, 1.000000000000000000, 0.9659258262890683122, 1.000000000000000000, 0.9659258262890683122, 1.000000000000000000, 0.9659258262890683122, 1.000000000000000000, 0.9659258262890683122, 1.000000000000000000, 0.9659258262890683122, 1.000000000000000000, 0.9659258262890683122, 1.000000000000000000, 0.9659258262890683122, 1.000000000000000000, 0.9659258262890683122, 1.000000000000000000, 0.9659258262890683122, 1.000000000000000000, 0.9659258262890683122, 1.000000000000000000, 0.9659258262890683122, 1.000000000000000000, 0.9659258262890683122, 1.000000000000000000, 0.9659258262890683122, 1.000000000000000000, 0.9659258262890683122, 1.000000000000000000, 0.9659258262890683122, 1.000000000000000000, 0.9659258262890683122, 1.000000000000000000, 0.9659258262890683122, 1.000000000000000000, 0.9659258262890683122, 1.000000000000000000, 0.9659258262890683122, 1.000000000000000000, 0.9659258262890683122, 1.000000000000000000, 0.9659258262890683122, 1.000000000000000000, 0.9659258262890683122, 1.000000000000000000, 0.9659258262890683122, 1.000000000000000000, 0.9659258262890683122, 1.000000000000000000, 0.9659258262890683122, 1.000000000000000000, 0.9659258262890683122, 1.000000000000000000, 0.9659258262890683122, 1.000000000000000000, 0.9659258262890683122, 1.000000000000000000, 0.9659258262890683122, 1.000000000000000000, 0.9659258262890683122, 1.000000000000000000, 0.9659258262890683122, 1.000000000000000000, 0.9659258262890683122, 1.000000000000000000, 0.9659258262890683122, 1.000000000000000000, 0.9659258262890683122, 1.000000000000000000, 0.9659258262890683122, 1.000000000000000000, 0.9659258262890683122, 1.000000000000000000, 0.9659258262890683122, 1.000000000000000000, 0.9659258262890683122, 1.000000000000000000, 0.9659258262890683122, 1.000000000000000000, 0.9659258262890683122, 1.000000000000000000, 0.9659258262890683122, 1.000000000000000000, 0.9659258262890683122, 1.000000000000000000, 0.9659258262890683122, 1.000000000000000000, 0.9659258262890683122, 1.000000000000000000, 0.9659258262890683122, 1.000000000000000000, 0.9659258262890683122, 1.000000000000000000, 0.9659258262890683122, 1.000000000000000000, 0.9659258262890683122, 1.000000000000000000, 0.9659258262890683122, 1.000000000000000000, 0.9659258262890683122, 1.000000000000000000, 0.9659258262890683122, 1.000000000000000000, 0.9659258262890683122, 1.000000000000000000, 0.9659258262890683122, 1.000000000000000000, 0.9659258262890683122, 1.000000000000000000, 0.9659258262890683122, 1.000000000000000000, 0.9659258262890683122, 1.000000000000000000, 0.9659258262890683122, 1.000000000000000000, 0.9659258262890683122, 1.000000000000000000, 0.9659258262890683122, 1.000000000000000000, 0.9659258262890683122, 1.000000000000000000, 0.9659258262890683122, 1.000000000000000000, 0.9659258262890683122, 1.000000000000000000, 0.9659258262890683122, 1.000000000000000000, 0.9659258262890683122, 1.000000000000000000, 0.9659258262890683122, 1.000000000000000000, 0.9659258262890683122, 1.000000000000000000, 0.9659258262890683122, 1.000000000000000000, 0.9659258262890683122, 1.000000000000000000, 0.9659258262890683122, 1.000000000000000000, 0.9659258262890683122, 1.000000000000000000, 0.9659258262890683122, 1.000000000000000000, 0.9659258262890683122, 1.000000000000000000, 0.9659258262890683122, 1.000000000000000000, 0.9659258262890683122, 1.000000000000000000, 0.9659258262890683122, 1.000000000000000000, 0.9659258262890683122, 1.000000000000000000, 0.9659258262890683122, 1.000000000000000000, 0.9659258262890683122, 1.000000000000000000, 0.9659258262890683122, 1.000000000000000000, 0.9659258262890683122, 1.000000000000000000, 0.9659258262890683122, 1.000000000000000000, 0.9659258262890683122, 1.000000000000000000, 0.9659258262890683122, 1.000000000000000000, 0.9659258262890683122, 1.000000000000000000, 0.9659258262890683122, 1.000000000000000000, 0.9659258262890683122, 1.000000000000000000, 0.9659258262890683122, 1.000000000000000000, 0.9659258262890683122, 1.000000000000000000, 0.9659258262890683122, 1.000000000000000000, 0.9659258262890683122, 1.000000000000000000, 0.9659258262890683122, 1.000000000000000000, 0.9659258262890683122, 1.000000000000000000, 0.9659258262890683122, 1.000000000000000000, 0.9659258262890683122, 1.000000000000000000, 0.9659258262890683122, 1.000000000000000000, 0.9659258262890683122, 1.000000000000000000, 0.9659258262890683122, 1.000000000000000000, 0.9659258262890683122, 1.000000000000000000, 0.9659258262890683122, 1.000000000000000000, 0.9659258262890683122, 1.000000000000000000) ) ) 
 REPRESENTATION_ITEM ( '' )  SURFACE ( )  );
#26582 = FILL_AREA_STYLE ('',( #10608 ) ) ;
#26583 = CARTESIAN_POINT ( 'NONE',  ( 2.638427012816835227, 7.467264484334121377, 9.846743663894590881 ) ) ;
#26584 = VERTEX_POINT ( 'NONE', #60572 ) ;
#26585 = CARTESIAN_POINT ( 'NONE',  ( 18.52753015748618282, 18.92559781766745175, -4.923371831947291888 ) ) ;
#26586 = DIRECTION ( 'NONE',  ( 0.000000000000000000, 0.000000000000000000, 1.000000000000000000 ) ) ;
#26587 = EDGE_LOOP ( 'NONE', ( #94848, #28938, #40719, #72100 ) ) ;
#26589 = CARTESIAN_POINT ( 'NONE',  ( 4.559911319644449179, 7.230352010821505360, -9.422509992056141925 ) ) ;
#26588 = CARTESIAN_POINT ( 'NONE',  ( 12.91533473730992121, 4.522018677488170546, 10.88017736071110164 ) ) ;
#26591 = CARTESIAN_POINT ( 'NONE',  ( 10.00000000000000000, 2.873634669930420049, -12.81628187352647608 ) ) ;
#26590 = CARTESIAN_POINT ( 'NONE',  ( 10.00000000000000000, 54.75893115100078745, -9.846743663894594434 ) ) ;
#26592 = CARTESIAN_POINT ( 'NONE',  ( 0.3329122712636403691, 0.000000000000000000, -5.443067521379384210 ) ) ;
#26593 = CARTESIAN_POINT ( 'NONE',  ( 9.879999999999968807, 26.99999999999954170, -2.958578643762691307 ) ) ;
#26594 = ADVANCED_FACE ( 'NONE', ( #45571 ), #77285, .T. ) ;
#26595 = MECHANICAL_DESIGN_GEOMETRIC_PRESENTATION_REPRESENTATION (  '', ( #28587 ), #76060 ) ;
#26596 = AXIS2_PLACEMENT_3D ( 'NONE', #23943, #14970, #14468 ) ;
#26597 = VECTOR ( 'NONE', #23101, 1000.000000000000000 ) ;
#26598 = CARTESIAN_POINT ( 'NONE',  ( 21.09922568453594849, 16.20696800326375353, 6.408140936763242479 ) ) ;
#26599 = ORIENTED_EDGE ( 'NONE', *, *, #64961, .F. ) ;
#26600 = CARTESIAN_POINT ( 'NONE',  ( 6.204703633549690345, 62.84541550158063927, 14.16423886937410082 ) ) ;
#26601 = EDGE_LOOP ( 'NONE', ( #28898, #36538, #38070, #24179 ) ) ;
#26602 = CARTESIAN_POINT ( 'NONE',  ( 2.917880565312950480, 60.97041550158063927, -12.26659068614894821 ) ) ;
#26603 = ORIENTED_EDGE ( 'NONE', *, *, #80162, .F. ) ;
#26604 = CARTESIAN_POINT ( 'NONE',  ( 7.084665262690076126, 39.10535201082150536, 10.88017736071109987 ) ) ;
#26605 = CARTESIAN_POINT ( 'NONE',  ( 4.559911319644449179, 48.89701867748817676, 9.422509992056141925 ) ) ;
#26606 = CARTESIAN_POINT ( 'NONE',  ( 7.084665262690076126, 57.02201867748817676, -10.88017736071110164 ) ) ;
#26607 = CARTESIAN_POINT ( 'NONE',  ( 4.559911319644449179, 47.23035201082150536, -9.422509992056141925 ) ) ;
#26608 =( GEOMETRIC_REPRESENTATION_CONTEXT ( 3 ) GLOBAL_UNCERTAINTY_ASSIGNED_CONTEXT ( ( #79324 ) ) GLOBAL_UNIT_ASSIGNED_CONTEXT ( ( #79597, #41616, #95075 ) ) REPRESENTATION_CONTEXT ( 'NONE', 'WORKASPACE' ) );
#26610 = EDGE_LOOP ( 'NONE', ( #65461, #56717, #53352, #61 ) ) ;
#26609 = FILL_AREA_STYLE ('',( #58085 ) ) ;
#26611 = CIRCLE ( 'NONE', #55392, 14.49999999999999822 ) ;
#26612 = CARTESIAN_POINT ( 'NONE',  ( 18.52753015748618282, 8.925597817667451750, -4.923371831947291888 ) ) ;
#26613 = ORIENTED_EDGE ( 'NONE', *, *, #10850, .F. ) ;
#26614 = CARTESIAN_POINT ( 'NONE',  ( 19.84674366389459621, 43.50893115100078745, 7.409399052514197653E-17 ) ) ;
#26615 = B_SPLINE_CURVE_WITH_KNOTS ( 'NONE', 3,
 ( #35771, #57287, #51270, #12282, #42789, #81272 ),
 .UNSPECIFIED., .F., .F.,
 ( 4, 2, 4 ),
 ( 0.0002800138956522149549, 0.0006862192609926520345, 0.001092424626333089168 ),
 .UNSPECIFIED. ) ;
#26616 = LINE ( 'NONE', #87610, #59625 ) ;
#26617 = VECTOR ( 'NONE', #2486, 1000.000000000000000 ) ;
#26618 = CARTESIAN_POINT ( 'NONE',  ( 19.38216949554541557, 52.24863466993041072, -9.382169495545420901 ) ) ;
#26619 = EDGE_CURVE ( 'NONE', #80133, #70674, #14210, .T. ) ;
#26620 = CARTESIAN_POINT ( 'NONE',  ( -6.757332319902496387, -55.97232334539076959, 2.750000000000000000 ) ) ;
#26621 = FACE_OUTER_BOUND ( 'NONE', #43435, .T. ) ;
#26622 = CARTESIAN_POINT ( 'NONE',  ( 18.52753015748617571, 63.09226448433412315, 4.923371831947298993 ) ) ;
#26623 = CARTESIAN_POINT ( 'NONE',  ( 2.917880565312950480, 65.97041550158063217, -12.26659068614894821 ) ) ;
#26624 = CARTESIAN_POINT ( 'NONE',  ( 10.00000000000000178, 67.25893115100079456, 9.846743663894594434 ) ) ;
#26625 = ORIENTED_EDGE ( 'NONE', *, *, #35481, .F. ) ;
#26626 = PLANE ( 'NONE',  #89521 ) ;
#26627 = CARTESIAN_POINT ( 'NONE',  ( 18.52753015748617571, 38.09226448433412315, 4.923371831947298993 ) ) ;
#26628 = CARTESIAN_POINT ( 'NONE',  ( 6.565887622018943937, 65.16530133659709634, 12.81628187352647430 ) ) ;
#26629 = CARTESIAN_POINT ( 'NONE',  ( 21.09922568453594849, 11.20696800326375531, 6.408140936763242479 ) ) ;
#26630 = CARTESIAN_POINT ( 'NONE',  ( 19.84674366389459266, 3.717264484334118713, -2.638427012816827677 ) ) ;
#26631 = CARTESIAN_POINT ( 'NONE',  ( -10.64017930668197209, 14.49999999999999112, -10.57291749337233000 ) ) ;
#26632 = EDGE_CURVE ( 'NONE', #71139, #20387, #7856, .T. ) ;
#26633 = CARTESIAN_POINT ( 'NONE',  ( 0.1532563361054100626, 15.80059781766745353, -2.638427012816831230 ) ) ;
#26634 = CARTESIAN_POINT ( 'NONE',  ( 18.52753015748617571, 53.09226448433412315, 4.923371831947298993 ) ) ;
#26635 = DIRECTION ( 'NONE',  ( 0.3826834323650877834, -0.000000000000000000, -0.9238795325112876267 ) ) ;
#26636 = EDGE_CURVE ( 'NONE', #8161, #75142, #85885, .T. ) ;
#26637 = AXIS2_PLACEMENT_3D ( 'NONE', #8200, #230, #6711 ) ;
#26638 = EDGE_CURVE ( 'NONE', #66014, #68558, #34328, .T. ) ;
#26639 = EDGE_LOOP ( 'NONE', ( #83580, #79698, #39770, #63779 ) ) ;
#26640 = CARTESIAN_POINT ( 'NONE',  ( -0.3689425029237881626, 62.42874883491396787, 10.36894250292379027 ) ) ;
#26641 = CARTESIAN_POINT ( 'NONE',  ( 24.16423886937409904, 9.095415501580633943, 3.795296366450317205 ) ) ;
#26642 = CARTESIAN_POINT ( 'NONE',  ( 5.076628168052704559, 10.17559781766745175, -8.527530157486179263 ) ) ;
#26643 = CARTESIAN_POINT ( 'NONE',  ( -0.8801773607111009756, 38.06368534415484106, 1.068504757029289695E-15 ) ) ;
#26645 = CARTESIAN_POINT ( 'NONE',  ( 11.32252723389645510, 12.55781760004707692, 0.3396460154096309636 ) ) ;
#26644 = CARTESIAN_POINT ( 'NONE',  ( 0.6178305044545838731, 29.74863466993042138, 9.382169495545420901 ) ) ;
#26646 = CYLINDRICAL_SURFACE ( 'NONE', #19810, 0.5000000000000004441 ) ;
#26647 = CARTESIAN_POINT ( 'NONE',  ( -18.00000000000000355, 75.73428692542562146, 2.900000000000000355 ) ) ;
#26648 = CARTESIAN_POINT ( 'NONE',  ( 0.1532563361054083140, 56.00893115100078745, 1.131784320476157264E-15 ) ) ;
#26649 = CARTESIAN_POINT ( 'NONE',  ( 14.92337183194729988, 14.34226448433411782, -8.527530157486177487 ) ) ;
#26650 = CARTESIAN_POINT ( 'NONE',  ( 2.915334737309928315, -30.47798132251182324, 10.88017736071109987 ) ) ;
#26651 = CARTESIAN_POINT ( 'NONE',  ( 22.81628187352647785, 21.41530133659708923, 3.434112377981063169 ) ) ;
#26652 = CARTESIAN_POINT ( 'NONE',  ( 14.99847009497944583, 0.5000000000000004441, -0.2142307401080305596 ) ) ;
#26654 = CARTESIAN_POINT ( 'NONE',  ( 12.60874940350947959, 15.00000000000000000, -7.160268045227033973 ) ) ;
#26653 = CARTESIAN_POINT ( 'NONE',  ( 19.42250999205614548, 25.98035201082150891, -5.440088680355545492 ) ) ;
#26655 = CARTESIAN_POINT ( 'NONE',  ( -10.19513985507819598, 14.63606907090794351, -11.00268709613235174 ) ) ;
#26656 = CARTESIAN_POINT ( 'NONE',  ( 17.08211943468705840, 55.13708216824731068, -12.26659068614894466 ) ) ;
#26657 = AXIS2_PLACEMENT_3D ( 'NONE', #94997, #9540, #16562 ) ;
#26658 = CARTESIAN_POINT ( 'NONE',  ( 17.08211943468705130, 23.47041550158063572, 12.26659068614894998 ) ) ;
#26659 = CARTESIAN_POINT ( 'NONE',  ( 10.00000000000000178, 42.25893115100078745, 9.846743663894594434 ) ) ;
#26660 = VECTOR ( 'NONE', #41102, 1000.000000000000000 ) ;
#26661 = CARTESIAN_POINT ( 'NONE',  ( 19.38216949554541557, 32.24863466993041783, -9.382169495545420901 ) ) ;
#26662 = CARTESIAN_POINT ( 'NONE',  ( 19.42250999205614548, 25.98035201082150891, -5.440088680355545492 ) ) ;
#26663 = CARTESIAN_POINT ( 'NONE',  ( 5.076628168052703671, 56.84226448433412315, 8.527530157486179263 ) ) ;
#26664 = CARTESIAN_POINT ( 'NONE',  ( 15.44008868035555260, 44.73035201082151247, 9.422509992056143702 ) ) ;
#26665 = CARTESIAN_POINT ( 'NONE',  ( 3.591859063236761518, -0.04303199673624671928, 11.09922568453594849 ) ) ;
#26666 = CARTESIAN_POINT ( 'NONE',  ( 10.00000000000000178, 23.05374883491397142, 14.16423886937410082 ) ) ;
#26667 = FACE_OUTER_BOUND ( 'NONE', #26682, .T. ) ;
#26668 = CARTESIAN_POINT ( 'NONE',  ( 18.52753015748617571, 23.09226448433411960, 4.923371831947298993 ) ) ;
#26669 = CARTESIAN_POINT ( 'NONE',  ( 0.1532563361054083140, 66.00893115100079456, 1.131784320476157264E-15 ) ) ;
#26670 = ORIENTED_EDGE ( 'NONE', *, *, #1740, .T. ) ;
#26671 = EDGE_CURVE ( 'NONE', #81788, #23479, #33372, .T. ) ;
#26672 = CARTESIAN_POINT ( 'NONE',  ( 0.000000000000000000, 14.49999999999999822, 0.000000000000000000 ) ) ;
#26673 = CARTESIAN_POINT ( 'NONE',  ( 6.930493939446634499, -71.55570417525920845, 3.750000000000001776 ) ) ;
#26674 = CARTESIAN_POINT ( 'NONE',  ( 10.00000000000000000, 16.81368534415483751, -10.88017736071110342 ) ) ;
#26675 = CARTESIAN_POINT ( 'NONE',  ( -2.266590686148945544, 16.38708216824730357, -7.082119434687050408 ) ) ;
#26676 = CARTESIAN_POINT ( 'NONE',  ( 7.361572987183169658, 4.967264484334119601, -9.846743663894592657 ) ) ;
#26677 = CARTESIAN_POINT ( 'NONE',  ( 0.1532563361054100626, 50.80059781766745175, -2.638427012816831230 ) ) ;
#26678 = CARTESIAN_POINT ( 'NONE',  ( 20.88017736071110519, 35.56368534415484106, 2.639326808657452039E-16 ) ) ;
#26679 = FACE_OUTER_BOUND ( 'NONE', #12220, .T. ) ;
#26680 = CARTESIAN_POINT ( 'NONE',  ( 5.076628168052703671, 61.84226448433412315, 8.527530157486179263 ) ) ;
#26681 = MECHANICAL_DESIGN_GEOMETRIC_PRESENTATION_REPRESENTATION (  '', ( #69809 ), #18707 ) ;
#26682 = EDGE_LOOP ( 'NONE', ( #127, #95373, #39065, #55893, #54635, #37545 ) ) ;
#26683 = CYLINDRICAL_SURFACE ( 'NONE', #92842, 0.5000000000000004441 ) ;
#26684 = EDGE_LOOP ( 'NONE', ( #62951, #75029, #24612, #66339 ) ) ;
#26685 = ORIENTED_EDGE ( 'NONE', *, *, #65751, .T. ) ;
#26686 = CARTESIAN_POINT ( 'NONE',  ( 5.991992585808537441, 4.355491999677157623E-16, 13.20401548210299048 ) ) ;
#26687 = CARTESIAN_POINT ( 'NONE',  ( -2.266590686148945544, 12.22041550158063394, 7.082119434687048631 ) ) ;
#26688 = CARTESIAN_POINT ( 'NONE',  ( -4.164238869374098151, 11.59541550158063217, -3.795296366450310543 ) ) ;
#26689 = CARTESIAN_POINT ( 'NONE',  ( 24.16423886937410614, 59.30374883491397497, 8.672049930838204340E-16 ) ) ;
#26690 = CARTESIAN_POINT ( 'NONE',  ( 19.84674366389459621, 63.50893115100078745, 7.409399052514197653E-17 ) ) ;
#26691 = CARTESIAN_POINT ( 'NONE',  ( 12.63842701281683922, 29.55059781766745175, -9.846743663894590881 ) ) ;
#26692 = FILL_AREA_STYLE ('',( #85738 ) ) ;
#26694 = CARTESIAN_POINT ( 'NONE',  ( 10.00000000000000000, 64.75893115100078035, -9.846743663894594434 ) ) ;
#26693 = CARTESIAN_POINT ( 'NONE',  ( 2.035157376598822676, 37.43868534415484106, -7.964842623401177768 ) ) ;
#26695 = CARTESIAN_POINT ( 'NONE',  ( 13.79529636645030344, 3.262082168247301350, 14.16423886937410614 ) ) ;
#26696 = CARTESIAN_POINT ( 'NONE',  ( 13.79529636645030344, 48.26208216824728936, 14.16423886937410614 ) ) ;
#26697 = CARTESIAN_POINT ( 'NONE',  ( -2.266590686148945544, 67.22041550158063217, 7.082119434687048631 ) ) ;
#26698 = CARTESIAN_POINT ( 'NONE',  ( -2.863845842055730895, 0.04922511925147109862, -14.47219703936417545 ) ) ;
#26699 = DIRECTION ( 'NONE',  ( -5.818595309480553908E-17, -1.000000000000000000, -0.000000000000000000 ) ) ;
#26700 = CARTESIAN_POINT ( 'NONE',  ( 0.5774900079438590739, 67.64701867748817676, -5.440088680355550821 ) ) ;
#26701 = DIRECTION ( 'NONE',  ( 0.000000000000000000, 0.000000000000000000, 1.000000000000000000 ) ) ;
#26702 = VERTEX_POINT ( 'NONE', #11350 ) ;
#26703 = SURFACE_STYLE_FILL_AREA ( #80200 ) ;
#26704 = ORIENTED_EDGE ( 'NONE', *, *, #80880, .F. ) ;
#26705 = CARTESIAN_POINT ( 'NONE',  ( 7.361572987183169658, 19.96726448433411960, -9.846743663894592657 ) ) ;
#26706 = VERTEX_POINT ( 'NONE', #10869 ) ;
#26707 = CARTESIAN_POINT ( 'NONE',  ( -4.164238869374099927, 27.01208216824730357, 3.795296366450308767 ) ) ;
#26708 = CARTESIAN_POINT ( 'NONE',  ( 18.52753015748617571, 38.09226448433412315, 4.923371831947298993 ) ) ;
#26709 = CARTESIAN_POINT ( 'NONE',  ( -0.8801773607111008646, 58.27201867748816966, 2.915334737309923430 ) ) ;
#26710 = EDGE_CURVE ( 'NONE', #33681, #11587, #14749, .T. ) ;
#26711 = CARTESIAN_POINT ( 'NONE',  ( 19.42250999205614548, 60.98035201082151247, -5.440088680355545492 ) ) ;
#26712 = CARTESIAN_POINT ( 'NONE',  ( 1.472469842513823179, 51.42559781766745886, 4.923371831947296329 ) ) ;
#26713 = AXIS2_PLACEMENT_3D ( 'NONE', #69564, #3051, #85055 ) ;
#26714 = CARTESIAN_POINT ( 'NONE',  ( 10.00000000000000178, 55.37363466993042493, 12.81628187352647608 ) ) ;
#26715 = CARTESIAN_POINT ( 'NONE',  ( -9.382169495545422677, 13.49863466993042316, -9.382169495545417348 ) ) ;
#26716 = ORIENTED_EDGE ( 'NONE', *, *, #86681, .F. ) ;
#26717 = CARTESIAN_POINT ( 'NONE',  ( 2.917880565312950480, 15.97041550158063217, -12.26659068614894821 ) ) ;
#26718 = VERTEX_POINT ( 'NONE', #49832 ) ;
#26719 = EDGE_LOOP ( 'NONE', ( #17160, #50676, #79502, #40738, #52927, #37379 ) ) ;
#26720 = CARTESIAN_POINT ( 'NONE',  ( 13.43411237798105340, 25.58196800326374998, 12.81628187352647963 ) ) ;
#26721 = VECTOR ( 'NONE', #27595, 1000.000000000000000 ) ;
#26722 = FACE_OUTER_BOUND ( 'NONE', #7570, .T. ) ;
#26723 = CARTESIAN_POINT ( 'NONE',  ( 18.52753015748618282, 18.92559781766745175, -4.923371831947291888 ) ) ;
#26724 = SURFACE_STYLE_USAGE ( .BOTH. , #3754 ) ;
#26725 = CARTESIAN_POINT ( 'NONE',  ( -1.099225684535947600, 54.54030133659708923, 6.408140936763237150 ) ) ;
#26726 = CARTESIAN_POINT ( 'NONE',  ( -46.56032334906440440, 103.8061263278352016, -5.692785474544873381 ) ) ;
#26727 = CARTESIAN_POINT ( 'NONE',  ( 2.791683348922237240, 35.38393115100079456, -7.208316651077763204 ) ) ;
#26728 = ADVANCED_FACE ( 'NONE', ( #55880 ), #72333, .T. ) ;
#26729 = AXIS2_PLACEMENT_3D ( 'NONE', #86649, #65594, #20105 ) ;
#26730 = CIRCLE ( 'NONE', #76209, 0.5000000000000004441 ) ;
#26732 = EDGE_LOOP ( 'NONE', ( #49622, #83528, #80584, #58308 ) ) ;
#26731 = CARTESIAN_POINT ( 'NONE',  ( 10.17198128013136227, 0.2306972965111899476, 10.94389562857672438 ) ) ;
#26733 = CYLINDRICAL_SURFACE ( 'NONE', #22346, 10.90000000000000036 ) ;
#26734 = CYLINDRICAL_SURFACE ( 'NONE', #46640, 0.5000000000000004441 ) ;
#26735 = CARTESIAN_POINT ( 'NONE',  ( 1.274849032794102888, 3.572280503510291361, 6.499999999999721112 ) ) ;
#26736 = CARTESIAN_POINT ( 'NONE',  ( 14.92337183194729988, 4.342264484334117824, -8.527530157486177487 ) ) ;
#26737 = CARTESIAN_POINT ( 'NONE',  ( 10.00000000000000178, 30.37363466993042138, 12.81628187352647608 ) ) ;
#26738 = DIRECTION ( 'NONE',  ( -0.000000000000000000, -1.000000000000000000, -0.000000000000000000 ) ) ;
#26739 = CARTESIAN_POINT ( 'NONE',  ( 18.52753015748617571, 38.09226448433412315, 4.923371831947298993 ) ) ;
#26740 = CARTESIAN_POINT ( 'NONE',  ( -1.983216688681034068, 15.00000000000000000, 14.11131997956736406 ) ) ;
#26741 = CARTESIAN_POINT ( 'NONE',  ( -0.3689425029237898834, 26.17874883491396432, -10.36894250292378850 ) ) ;
#26742 = CARTESIAN_POINT ( 'NONE',  ( 14.92337183194729633, 32.67559781766745175, 8.527530157486181039 ) ) ;
#26743 = CARTESIAN_POINT ( 'NONE',  ( 13.43411237798106583, 32.66530133659708213, -12.81628187352647252 ) ) ;
#26745 = CARTESIAN_POINT ( 'NONE',  ( 14.48718990079892066, 4.852832169489322230E-16, 0.6093675230841453239 ) ) ;
#26744 = CARTESIAN_POINT ( 'NONE',  ( 20.00000000000000711, 97.71973001530635372, 4.500000000000000888 ) ) ;
#26746 = CARTESIAN_POINT ( 'NONE',  ( 12.91533473730993009, 66.60535201082150536, -10.88017736071109987 ) ) ;
#26747 = EDGE_CURVE ( 'NONE', #65300, #89307, #6402, .T. ) ;
#26748 = CARTESIAN_POINT ( 'NONE',  ( -1.099225684535947600, 4.540301336597087456, 6.408140936763237150 ) ) ;
#26749 = CARTESIAN_POINT ( 'NONE',  ( 1.959929470562272291, 40.51528370094807485, -5.767676674365837641 ) ) ;
#26750 = CARTESIAN_POINT ( 'NONE',  ( 10.00000000000000178, 32.25893115100078745, 9.846743663894594434 ) ) ;
#26751 = CARTESIAN_POINT ( 'NONE',  ( -0.8801773607111009756, 23.06368534415484106, 1.068504757029289695E-15 ) ) ;
#26752 = CARTESIAN_POINT ( 'NONE',  ( 21.09922568453594849, 31.20696800326375353, 6.408140936763242479 ) ) ;
#26753 = CARTESIAN_POINT ( 'NONE',  ( 19.84674366389459266, 33.71726448433410894, -2.638427012816827677 ) ) ;
#26754 = SHAPE_DEFINITION_REPRESENTATION ( #6738, #81163 ) ;
#26755 = CARTESIAN_POINT ( 'NONE',  ( -12.87930560075679942, 14.95037102969557452, 7.195887444332292660 ) ) ;
#26756 = ADVANCED_FACE ( 'NONE', ( #95342 ), #42350, .T. ) ;
#26757 = CARTESIAN_POINT ( 'NONE',  ( -0.8801773607110991993, 32.85535201082151247, -2.915334737309923874 ) ) ;
#26758 = EDGE_CURVE ( 'NONE', #94992, #20984, #65280, .T. ) ;
#26759 = VERTEX_POINT ( 'NONE', #40394 ) ;
#26760 = CARTESIAN_POINT ( 'NONE',  ( 15.44008868035555793, 66.39701867748817676, -9.422509992056140149 ) ) ;
#26761 =( NAMED_UNIT ( * ) SI_UNIT ( $, .STERADIAN. ) SOLID_ANGLE_UNIT ( ) );
#26763 = CARTESIAN_POINT ( 'NONE',  ( -0.8801773607110991993, 32.85535201082151247, -2.915334737309923874 ) ) ;
#26762 = CARTESIAN_POINT ( 'NONE',  ( 5.076628168052704559, 55.17559781766745175, -8.527530157486179263 ) ) ;
#26764 = CARTESIAN_POINT ( 'NONE',  ( -3.999999999999999112, 78.07179676972445748, -6.500000000000000888 ) ) ;
#26765 = CARTESIAN_POINT ( 'NONE',  ( 20.88017736071110875, 50.77201867748817676, -2.915334737309920765 ) ) ;
#26767 = CARTESIAN_POINT ( 'NONE',  ( 20.00000000000000711, 79.40087001978915282, -4.500000000000000000 ) ) ;
#26766 = CARTESIAN_POINT ( 'NONE',  ( 10.00000000000000178, 14.31368534415483929, 10.88017736071110342 ) ) ;
#26768 = DIRECTION ( 'NONE',  ( 0.000000000000000000, 0.000000000000000000, 1.000000000000000000 ) ) ;
#26769 = CARTESIAN_POINT ( 'NONE',  ( 12.63842701281683922, 49.55059781766744464, -9.846743663894590881 ) ) ;
#26770 = CARTESIAN_POINT ( 'NONE',  ( 2.917880565312948704, 52.63708216824730357, 12.26659068614894643 ) ) ;
#26771 = FACE_OUTER_BOUND ( 'NONE', #21068, .T. ) ;
#26772 = CARTESIAN_POINT ( 'NONE',  ( 10.00000000000000178, 33.05374883491396787, 14.16423886937410082 ) ) ;
#26773 = AXIS2_PLACEMENT_3D ( 'NONE', #42093, #11579, #57077 ) ;
#26774 = CARTESIAN_POINT ( 'NONE',  ( 22.81628187352647785, 1.415301336597087012, 3.434112377981063169 ) ) ;
#26775 = CARTESIAN_POINT ( 'NONE',  ( -4.536162600130072775, -17.54167793721155633, 2.750000000000002220 ) ) ;
#26776 = VERTEX_POINT ( 'NONE', #17399 ) ;
#26777 = CARTESIAN_POINT ( 'NONE',  ( -2.266590686148945544, 67.22041550158063217, 7.082119434687048631 ) ) ;
#26778 = CARTESIAN_POINT ( 'NONE',  ( 7.361572987183170547, 37.05059781766744464, 9.846743663894590881 ) ) ;
#26780 = CARTESIAN_POINT ( 'NONE',  ( -9.297374403301716939, 88.08016496434417775, -4.860721439949188039 ) ) ;
#26779 = DIRECTION ( 'NONE',  ( 0.7933533402912409382, 0.000000000000000000, -0.6087614290087131064 ) ) ;
#26781 = CARTESIAN_POINT ( 'NONE',  ( 19.42250999205614193, 65.14701867748817676, 5.440088680355555262 ) ) ;
#26782 = CARTESIAN_POINT ( 'NONE',  ( -1.099225684535947600, 64.54030133659709634, 6.408140936763237150 ) ) ;
#26783 = CARTESIAN_POINT ( 'NONE',  ( 20.88017736071110875, 30.77201867748816966, -2.915334737309920765 ) ) ;
#26784 = CARTESIAN_POINT ( 'NONE',  ( -1.099225684535947600, 63.70696800326376774, -6.408140936763238038 ) ) ;
#26785 = CARTESIAN_POINT ( 'NONE',  ( 21.09922568453595559, 7.040301336597086568, -6.408140936763230044 ) ) ;
#26786 = CARTESIAN_POINT ( 'NONE',  ( 5.076628168052704559, 30.17559781766745175, -8.527530157486179263 ) ) ;
#26787 = VERTEX_POINT ( 'NONE', #78372 ) ;
#26788 = FILL_AREA_STYLE_COLOUR ( '', #88461 ) ;
#26789 = EDGE_CURVE ( 'NONE', #43815, #67057, #95633, .T. ) ;
#26790 = DIRECTION ( 'NONE',  ( 0.000000000000000000, 0.000000000000000000, 1.000000000000000000 ) ) ;
#26791 = CARTESIAN_POINT ( 'NONE',  ( 2.035157376598822676, 2.438685344154838397, -7.964842623401177768 ) ) ;
#26792 = CARTESIAN_POINT ( 'NONE',  ( -4.164238869374099039, 26.80374883491397142, 8.674139862899312516E-16 ) ) ;
#26793 = CARTESIAN_POINT ( 'NONE',  ( 20.88017736071110875, 30.77201867748816966, -2.915334737309920765 ) ) ;
#26794 = AXIS2_PLACEMENT_3D ( 'NONE', #7677, #44665, #83659 ) ;
#26795 = CARTESIAN_POINT ( 'NONE',  ( 0.5774900079438590739, 52.64701867748817676, -5.440088680355550821 ) ) ;
#26796 = DIRECTION ( 'NONE',  ( 0.9681476403781101858, 0.000000000000000000, -0.2503800040544323924 ) ) ;
#26797 = CARTESIAN_POINT ( 'NONE',  ( 14.97687855664608314, 0.5000000000000004441, -0.8325315005900512100 ) ) ;
#26798 = B_SPLINE_CURVE_WITH_KNOTS ( 'NONE', 3,
 ( #33427, #92467, #1992, #32458, #93458, #24984, #55468, #46790, #92297, #52812, #61298, #23821, #91807, #30798, #91303, #15821 ),
 .UNSPECIFIED., .F., .F.,
 ( 4, 2, 2, 2, 2, 2, 2, 4 ),
 ( 0.000000000000000000, 0.002379327621847403523, 0.004758655243694807045, 0.005948319054618508156, 0.007137982865542210134, 0.008327646676465913847, 0.008922478581927750091, 0.009517310487389588070 ),
 .UNSPECIFIED. ) ;
#26799 = CARTESIAN_POINT ( 'NONE',  ( 18.52753015748617571, 8.092264484334117824, 4.923371831947298993 ) ) ;
#26800 = DIRECTION ( 'NONE',  ( -0.000000000000000000, 0.000000000000000000, 1.000000000000000000 ) ) ;
#26801 = DIRECTION ( 'NONE',  ( 0.5519369853120676961, 0.000000000000000000, -0.8338858220671618859 ) ) ;
#26802 = CARTESIAN_POINT ( 'NONE',  ( 19.84674366389459266, 28.30059781766745886, 2.638427012816836559 ) ) ;
#26803 = CARTESIAN_POINT ( 'NONE',  ( 19.84674366389459266, 53.30059781766744464, 2.638427012816836559 ) ) ;
#26804 = AXIS2_PLACEMENT_3D ( 'NONE', #42892, #89371, #66363 ) ;
#26805 = CARTESIAN_POINT ( 'NONE',  ( 7.084665262690076126, 29.10535201082150181, 10.88017736071109987 ) ) ;
#26806 = AXIS2_PLACEMENT_3D ( 'NONE', #55621, #46626, #48101 ) ;
#26807 = CARTESIAN_POINT ( 'NONE',  ( -2.816281873526473856, 44.12363466993042493, 9.499525473075851096E-16 ) ) ;
#26808 = CARTESIAN_POINT ( 'NONE',  ( -2.174473938468956646, 0.000000000000000000, 5.000947681547202706 ) ) ;
#26809 = CARTESIAN_POINT ( 'NONE',  ( 20.88017736071110164, 65.35535201082150536, 2.915334737309930979 ) ) ;
#26810 = CARTESIAN_POINT ( 'NONE',  ( 19.84674366389459266, 33.30059781766744464, 2.638427012816836559 ) ) ;
#26812 = CARTESIAN_POINT ( 'NONE',  ( 17.20831665107776587, 27.88393115100078390, 7.208316651077764980 ) ) ;
#26811 = CARTESIAN_POINT ( 'NONE',  ( 2.917880565312950480, 55.97041550158063217, -12.26659068614894821 ) ) ;
#26813 = CARTESIAN_POINT ( 'NONE',  ( 2.603489959281614308, 51.58210964143330557, 6.500000000000031086 ) ) ;
#26814 = DIRECTION ( 'NONE',  ( -0.000000000000000000, -1.000000000000000000, -0.000000000000000000 ) ) ;
#26815 = CARTESIAN_POINT ( 'NONE',  ( -4.164238869374099039, 11.80374883491396965, 8.674139862899312516E-16 ) ) ;
#26816 = CARTESIAN_POINT ( 'NONE',  ( -4.164238869374098151, 36.59541550158063217, -3.795296366450310543 ) ) ;
#26817 = CARTESIAN_POINT ( 'NONE',  ( 2.791683348922237240, 35.38393115100079456, -7.208316651077763204 ) ) ;
#26818 = CARTESIAN_POINT ( 'NONE',  ( 17.62281668512002852, 8.285933195168226462, 6.500000000000004441 ) ) ;
#26819 = CARTESIAN_POINT ( 'NONE',  ( 15.44008868035555793, 26.39701867748817321, -9.422509992056140149 ) ) ;
#26820 = CARTESIAN_POINT ( 'NONE',  ( 20.88017736071110519, 55.56368534415484817, 2.639326808657452039E-16 ) ) ;
#26821 = CARTESIAN_POINT ( 'NONE',  ( 20.88017736071110164, 50.35535201082151247, 2.915334737309930979 ) ) ;
#26822 = ORIENTED_EDGE ( 'NONE', *, *, #40124, .F. ) ;
#26823 = CARTESIAN_POINT ( 'NONE',  ( 0.6178305044545818747, 38.49863466993042493, -9.382169495545419124 ) ) ;
#26824 = CARTESIAN_POINT ( 'NONE',  ( 17.96484262340118221, 49.93868534415484106, 7.964842623401181321 ) ) ;
#26825 = EDGE_LOOP ( 'NONE', ( #38930, #17272, #55163, #12598, #39967, #91011 ) ) ;
#26826 =( NAMED_UNIT ( * ) PLANE_ANGLE_UNIT ( ) SI_UNIT ( $, .RADIAN. ) );
#26827 = CARTESIAN_POINT ( 'NONE',  ( 17.96484262340118221, 66.18868534415483396, -7.964842623401177768 ) ) ;
#26828 = ORIENTED_EDGE ( 'NONE', *, *, #88988, .F. ) ;
#26829 = CARTESIAN_POINT ( 'NONE',  ( -0.8801773607110991993, 62.85535201082150536, -2.915334737309923874 ) ) ;
#26830 = CARTESIAN_POINT ( 'NONE',  ( 20.88017736071110875, 20.77201867748816611, -2.915334737309920765 ) ) ;
#26831 = LINE ( 'NONE', #95332, #5296 ) ;
#26832 = DIRECTION ( 'NONE',  ( 0.000000000000000000, 1.000000000000000000, 0.000000000000000000 ) ) ;
#26833 = CARTESIAN_POINT ( 'NONE',  ( -0.8801773607110991993, 7.855352010821506248, -2.915334737309923874 ) ) ;
#26834 = CARTESIAN_POINT ( 'NONE',  ( 0.1532563361054100626, 15.80059781766745353, -2.638427012816831230 ) ) ;
#26835 = CARTESIAN_POINT ( 'NONE',  ( 10.00000000000000178, 23.05374883491397142, 14.16423886937410082 ) ) ;
#26836 = CARTESIAN_POINT ( 'NONE',  ( 10.00000000000000178, 24.31368534415484106, 10.88017736071110342 ) ) ;
#26837 = CARTESIAN_POINT ( 'NONE',  ( 19.84674366389459266, 63.30059781766745886, 2.638427012816836559 ) ) ;
#26838 = ORIENTED_EDGE ( 'NONE', *, *, #96884, .F. ) ;
#26839 = CARTESIAN_POINT ( 'NONE',  ( 19.84674366389459621, 63.50893115100078745, 7.409399052514197653E-17 ) ) ;
#26840 = ORIENTED_EDGE ( 'NONE', *, *, #40456, .F. ) ;
#26841 = ADVANCED_FACE ( 'NONE', ( #93868 ), #48363, .T. ) ;
#26842 = CARTESIAN_POINT ( 'NONE',  ( -0.8801773607111008646, 58.27201867748816966, 2.915334737309923430 ) ) ;
#26843 = CARTESIAN_POINT ( 'NONE',  ( 2.791683348922240793, 46.63393115100077324, 7.208316651077764092 ) ) ;
#26844 = CARTESIAN_POINT ( 'NONE',  ( 13.43411237798106583, 32.66530133659708213, -12.81628187352647252 ) ) ;
#26846 = CARTESIAN_POINT ( 'NONE',  ( -13.95749458852073133, 14.76930270348882068, -5.331641351773216186 ) ) ;
#26845 = CARTESIAN_POINT ( 'NONE',  ( -0.8801773607110991993, 2.855352010821504471, -2.915334737309923874 ) ) ;
#26847 = CARTESIAN_POINT ( 'NONE',  ( 10.00000000000000000, 61.81368534415484106, -10.88017736071110342 ) ) ;
#26848 = CARTESIAN_POINT ( 'NONE',  ( -0.8801773607110991993, 2.855352010821504471, -2.915334737309923874 ) ) ;
#26849 = EDGE_CURVE ( 'NONE', #19080, #14105, #55273, .T. ) ;
#26850 = VECTOR ( 'NONE', #56955, 1000.000000000000000 ) ;
#26851 = CARTESIAN_POINT ( 'NONE',  ( 0.6178305044545838731, 39.74863466993041072, 9.382169495545420901 ) ) ;
#26852 = CARTESIAN_POINT ( 'NONE',  ( 19.42250999205614548, 35.98035201082151247, -5.440088680355545492 ) ) ;
#26853 = DIRECTION ( 'NONE',  ( 0.000000000000000000, 0.000000000000000000, 1.000000000000000000 ) ) ;
#26854 = ORIENTED_EDGE ( 'NONE', *, *, #37493, .F. ) ;
#26855 = CARTESIAN_POINT ( 'NONE',  ( 0.6178305044545838731, 44.74863466993042493, 9.382169495545420901 ) ) ;
#26856 = CARTESIAN_POINT ( 'NONE',  ( 20.88017736071110164, 35.35535201082150536, 2.915334737309930979 ) ) ;
#26857 = CARTESIAN_POINT ( 'NONE',  ( 10.00000000000000000, 54.75893115100078745, -9.846743663894594434 ) ) ;
#26858 = EDGE_LOOP ( 'NONE', ( #37639, #94198, #38779, #73064 ) ) ;
#26859 = AXIS2_PLACEMENT_3D ( 'NONE', #56637, #71647, #63629 ) ;
#26860 = CARTESIAN_POINT ( 'NONE',  ( 1.472469842513823179, 60.59226448433412315, -4.923371831947296329 ) ) ;
#26862 = CARTESIAN_POINT ( 'NONE',  ( 18.52753015748617571, 53.09226448433412315, 4.923371831947298993 ) ) ;
#26861 = CYLINDRICAL_SURFACE ( 'NONE', #18126, 0.5000000000000004441 ) ;
#26863 = CARTESIAN_POINT ( 'NONE',  ( 10.00000000000000000, 21.81368534415484106, -10.88017736071110342 ) ) ;
#26864 = CARTESIAN_POINT ( 'NONE',  ( 1.472469842513823179, 41.42559781766745886, 4.923371831947296329 ) ) ;
#26865 = CARTESIAN_POINT ( 'NONE',  ( -14.49154782522698071, 14.95037109980891543, -2.766288502467150412 ) ) ;
#26866 = LINE ( 'NONE', #40907, #83597 ) ;
#26869 = CARTESIAN_POINT ( 'NONE',  ( 10.00000000000000000, 14.75893115100078568, -9.846743663894594434 ) ) ;
#26868 = VECTOR ( 'NONE', #33546, 1000.000000000000000 ) ;
#26867 = CARTESIAN_POINT ( 'NONE',  ( 5.076628168052704559, 45.17559781766745175, -8.527530157486179263 ) ) ;
#26870 = DIRECTION ( 'NONE',  ( 1.000000000000000000, 1.257402221000611116E-16, -0.000000000000000000 ) ) ;
#26872 = VERTEX_POINT ( 'NONE', #75795 ) ;
#26871 = CARTESIAN_POINT ( 'NONE',  ( 0.1532563361054083140, 61.00893115100078745, 1.131784320476157264E-15 ) ) ;
#26873 = CIRCLE ( 'NONE', #93977, 14.49999999999999822 ) ;
#26874 = CARTESIAN_POINT ( 'NONE',  ( -2.816281873526473856, 64.33196800326376774, 3.434112377981055619 ) ) ;
#26875 = CARTESIAN_POINT ( 'NONE',  ( 20.03447792253739124, 7.655141069906896689, -6.401564815979731371 ) ) ;
#26876 = EDGE_CURVE ( 'NONE', #53155, #44802, #30776, .T. ) ;
#26877 = CARTESIAN_POINT ( 'NONE',  ( 10.00000000000000178, 45.37363466993041783, 12.81628187352647608 ) ) ;
#26878 = CARTESIAN_POINT ( 'NONE',  ( 18.52753015748617571, 48.09226448433412315, 4.923371831947298993 ) ) ;
#26879 = CARTESIAN_POINT ( 'NONE',  ( 9.742785792574936821, 7.201366962315986164, 5.624999999999996447 ) ) ;
#26880 = CARTESIAN_POINT ( 'NONE',  ( 20.36894250292379382, 63.67874883491396787, 10.36894250292379205 ) ) ;
#26881 = CARTESIAN_POINT ( 'NONE',  ( 12.63842701281683922, 19.55059781766745175, -9.846743663894590881 ) ) ;
#26882 = EDGE_CURVE ( 'NONE', #97286, #24048, #71745, .T. ) ;
#26883 = FACE_OUTER_BOUND ( 'NONE', #76035, .T. ) ;
#26884 = CARTESIAN_POINT ( 'NONE',  ( 22.26659068614895176, 54.72041550158063217, -7.082119434687042414 ) ) ;
#26885 = CARTESIAN_POINT ( 'NONE',  ( 5.076628168052703671, 66.84226448433412315, 8.527530157486179263 ) ) ;
#26886 = CARTESIAN_POINT ( 'NONE',  ( 12.91533473730993009, 6.605352010821504471, -10.88017736071109987 ) ) ;
#26887 = CARTESIAN_POINT ( 'NONE',  ( -4.164238869374098151, 31.59541550158063927, -3.795296366450310543 ) ) ;
#26889 = LINE ( 'NONE', #50371, #6298 ) ;
#26888 = CARTESIAN_POINT ( 'NONE',  ( 2.917880565312950480, 45.97041550158063927, -12.26659068614894821 ) ) ;
#26890 = FACE_OUTER_BOUND ( 'NONE', #50394, .T. ) ;
#26891 = CARTESIAN_POINT ( 'NONE',  ( 0.1532563361054083140, 11.00893115100078568, 1.131784320476157264E-15 ) ) ;
#26893 = CARTESIAN_POINT ( 'NONE',  ( 10.00000000000000178, 57.25893115100078745, 9.846743663894594434 ) ) ;
#26892 = CARTESIAN_POINT ( 'NONE',  ( 6.660444548071449589, -84.28805632662712810, 2.500000000000001332 ) ) ;
#26894 = VERTEX_POINT ( 'NONE', #2291 ) ;
#26895 = CARTESIAN_POINT ( 'NONE',  ( 7.084665262690076126, 44.10535201082151247, 10.88017736071109987 ) ) ;
#26896 = CARTESIAN_POINT ( 'NONE',  ( 19.67858290521088804, 89.00000000000000000, -5.461713021790605360 ) ) ;
#26897 = CARTESIAN_POINT ( 'NONE',  ( 19.84674366389459266, 48.71726448433413026, -2.638427012816827677 ) ) ;
#26898 = CARTESIAN_POINT ( 'NONE',  ( -1.099225684535947600, 64.54030133659709634, 6.408140936763237150 ) ) ;
#26899 = CARTESIAN_POINT ( 'NONE',  ( 19.84674366389459621, 58.50893115100078745, 7.409399052514197653E-17 ) ) ;
#26900 = CARTESIAN_POINT ( 'NONE',  ( -4.164238869374099039, 21.80374883491396787, 8.674139862899312516E-16 ) ) ;
#26901 = EDGE_CURVE ( 'NONE', #10866, #54718, #78757, .T. ) ;
#26902 = CARTESIAN_POINT ( 'NONE',  ( 7.361572987183170547, 2.050597817667451750, 9.846743663894590881 ) ) ;
#26903 = CARTESIAN_POINT ( 'NONE',  ( -5.328486666255608739, -28.65465727419771724, -2.750000000000806466 ) ) ;
#26904 = CARTESIAN_POINT ( 'NONE',  ( 7.084665262690076126, 19.10535201082150181, 10.88017736071109987 ) ) ;
#26905 = CARTESIAN_POINT ( 'NONE',  ( -2.816281873526473856, 29.12363466993041783, 9.499525473075851096E-16 ) ) ;
#26906 = LINE ( 'NONE', #95915, #51257 ) ;
#26907 = CARTESIAN_POINT ( 'NONE',  ( 5.076628168052703671, 6.842264484334118713, 8.527530157486179263 ) ) ;
#26908 = CARTESIAN_POINT ( 'NONE',  ( 16.40814093676324603, 52.45696800326375353, -11.09922568453594671 ) ) ;
#26909 = ORIENTED_EDGE ( 'NONE', *, *, #97966, .T. ) ;
#26910 = CARTESIAN_POINT ( 'NONE',  ( 7.160361147697994255, -84.29732993326337009, -4.000000000000000000 ) ) ;
#26911 = ADVANCED_FACE ( 'NONE', ( #26722 ), #49254, .T. ) ;
#26912 = CARTESIAN_POINT ( 'NONE',  ( -2.266590686148945544, 22.22041550158063572, 7.082119434687048631 ) ) ;
#26913 = CARTESIAN_POINT ( 'NONE',  ( 6.000000000000000000, 11.50000000000000000, 6.000000000000000000 ) ) ;
#26914 = CARTESIAN_POINT ( 'NONE',  ( -0.8801773607111008646, 13.27201867748817321, 2.915334737309923430 ) ) ;
#26915 = CARTESIAN_POINT ( 'NONE',  ( 14.24131928502211331, -0.03417435944610275333, 0.4973178280106892446 ) ) ;
#26916 = DIRECTION ( 'NONE',  ( 1.000000000000000000, 0.000000000000000000, 0.000000000000000000 ) ) ;
#26917 = CARTESIAN_POINT ( 'NONE',  ( 15.44008868035555260, 44.73035201082151247, 9.422509992056143702 ) ) ;
#26918 = CARTESIAN_POINT ( 'NONE',  ( 0.5774900079438607392, 53.48035201082151247, 5.440088680355550821 ) ) ;
#26919 = CARTESIAN_POINT ( 'NONE',  ( 0.6178305044545818747, 18.49863466993041428, -9.382169495545419124 ) ) ;
#26920 = CARTESIAN_POINT ( 'NONE',  ( 0.000000000000000000, 14.49999999999999822, 0.000000000000000000 ) ) ;
#26921 = DIRECTION ( 'NONE',  ( 1.000000000000000000, -0.000000000000000000, -0.000000000000000000 ) ) ;
#26922 = CARTESIAN_POINT ( 'NONE',  ( 0.1532563361054082862, 16.21726448433411960, 2.638427012816831674 ) ) ;
#26923 = CARTESIAN_POINT ( 'NONE',  ( -10.84451454130513426, 4.265732461173792237E-16, 9.625305416630759225 ) ) ;
#26924 = CARTESIAN_POINT ( 'NONE',  ( -0.8801773607111008646, 48.27201867748816966, 2.915334737309923430 ) ) ;
#26925 = VECTOR ( 'NONE', #33820, 1000.000000000000000 ) ;
#26926 = CARTESIAN_POINT ( 'NONE',  ( 22.81628187352648496, 1.831968003263753753, -3.434112377981050290 ) ) ;
#26927 = CARTESIAN_POINT ( 'NONE',  ( 19.42250999205614193, 65.14701867748817676, 5.440088680355555262 ) ) ;
#26928 = CARTESIAN_POINT ( 'NONE',  ( 14.92337183194729988, 24.34226448433411960, -8.527530157486177487 ) ) ;
#26929 = CARTESIAN_POINT ( 'NONE',  ( 10.00000000000000000, 47.87363466993042493, -12.81628187352647608 ) ) ;
#26931 = FACE_OUTER_BOUND ( 'NONE', #10132, .T. ) ;
#26930 = CARTESIAN_POINT ( 'NONE',  ( 0.1532563361054100626, 0.8005978176674514168, -2.638427012816831230 ) ) ;
#26932 = ORIENTED_EDGE ( 'NONE', *, *, #39658, .T. ) ;
#26933 = CARTESIAN_POINT ( 'NONE',  ( 2.153642693323453816, 56.13791097397319163, -6.500000000000043521 ) ) ;
#26934 = DIRECTION ( 'NONE',  ( 0.000000000000000000, 0.000000000000000000, 1.000000000000000000 ) ) ;
#26935 = CARTESIAN_POINT ( 'NONE',  ( 12.91533473730992121, 24.52201867748816966, 10.88017736071110164 ) ) ;
#26936 = CARTESIAN_POINT ( 'NONE',  ( 0.000000000000000000, 61.50000000000000711, -6.000000000000000000 ) ) ;
#26937 = CARTESIAN_POINT ( 'NONE',  ( 1.472469842513823179, 35.59226448433412315, -4.923371831947296329 ) ) ;
#26938 = CARTESIAN_POINT ( 'NONE',  ( 0.5774900079438607392, 13.48035201082150358, 5.440088680355550821 ) ) ;
#26939 = CARTESIAN_POINT ( 'NONE',  ( 12.91533473730992121, 4.522018677488170546, 10.88017736071110164 ) ) ;
#26940 = EDGE_LOOP ( 'NONE', ( #33116, #86123, #17198, #12691 ) ) ;
#26941 = CARTESIAN_POINT ( 'NONE',  ( 19.42250999205614548, 10.98035201082150358, -5.440088680355545492 ) ) ;
#26942 = AXIS2_PLACEMENT_3D ( 'NONE', #78620, #31626, #69642 ) ;
#26943 = CARTESIAN_POINT ( 'NONE',  ( 0.5774900079438590739, 17.64701867748817321, -5.440088680355550821 ) ) ;
#26945 = CARTESIAN_POINT ( 'NONE',  ( -0.8801773607110991993, 22.85535201082150181, -2.915334737309923874 ) ) ;
#26944 = CARTESIAN_POINT ( 'NONE',  ( -14.24131928502210975, 0.000000000000000000, -0.4973178280107823923 ) ) ;
#26946 = VERTEX_POINT ( 'NONE', #59521 ) ;
#26947 = CARTESIAN_POINT ( 'NONE',  ( 21.92686044187656336, 26.97997603579417714, 3.195792623639536423 ) ) ;
#26948 = CARTESIAN_POINT ( 'NONE',  ( -0.8801773607111009756, 18.06368534415484106, 1.068504757029289695E-15 ) ) ;
#26949 = CARTESIAN_POINT ( 'NONE',  ( 19.84674366389459266, 58.71726448433411605, -2.638427012816827677 ) ) ;
#26950 = FACE_OUTER_BOUND ( 'NONE', #85639, .T. ) ;
#26951 = CARTESIAN_POINT ( 'NONE',  ( 0.6178305044545818747, 58.49863466993042493, -9.382169495545419124 ) ) ;
#26952 = DIRECTION ( 'NONE',  ( -1.000000000000000000, -1.927470528863119542E-16, 0.000000000000000000 ) ) ;
#26953 = CARTESIAN_POINT ( 'NONE',  ( 6.204703633549690345, 35.76208216824729647, -14.16423886937410259 ) ) ;
#26954 = CARTESIAN_POINT ( 'NONE',  ( 19.42250999205614548, 45.98035201082150536, -5.440088680355545492 ) ) ;
#26955 = CARTESIAN_POINT ( 'NONE',  ( 17.96484262340118221, 21.18868534415483396, -7.964842623401177768 ) ) ;
#26956 = CARTESIAN_POINT ( 'NONE',  ( 19.88565890683628368, 42.71691075486305067, -6.480892540919849232 ) ) ;
#26957 = CARTESIAN_POINT ( 'NONE',  ( -5.991992585808451288, 3.888230080364882544E-16, -13.20401548210303311 ) ) ;
#26958 = CARTESIAN_POINT ( 'NONE',  ( 14.92337183194729988, 44.34226448433412315, -8.527530157486177487 ) ) ;
#26959 = DIRECTION ( 'NONE',  ( -0.000000000000000000, 1.000000000000000000, -0.000000000000000000 ) ) ;
#26960 = CARTESIAN_POINT ( 'NONE',  ( 14.92337183194729633, 12.67559781766745353, 8.527530157486181039 ) ) ;
#26961 = CARTESIAN_POINT ( 'NONE',  ( 3.434112377981054287, -27.33469866340291077, -12.81628187352647608 ) ) ;
#26962 = CARTESIAN_POINT ( 'NONE',  ( 19.42250999205614193, 15.14701867748817143, 5.440088680355555262 ) ) ;
#26963 = CARTESIAN_POINT ( 'NONE',  ( 17.20831665107776587, 14.13393115100078568, -7.208316651077762316 ) ) ;
#26964 = CARTESIAN_POINT ( 'NONE',  ( 15.44008868035555793, 66.39701867748817676, -9.422509992056140149 ) ) ;
#26966 = CARTESIAN_POINT ( 'NONE',  ( 22.81628187352647785, 51.41530133659708923, 3.434112377981063169 ) ) ;
#26965 = CARTESIAN_POINT ( 'NONE',  ( 20.88017736071110875, 25.77201867748816966, -2.915334737309920765 ) ) ;
#26968 = ADVANCED_FACE ( 'NONE', ( #82521 ), #90502, .F. ) ;
#26967 = CARTESIAN_POINT ( 'NONE',  ( -4.164238869374098151, 31.59541550158063927, -3.795296366450310543 ) ) ;
#26969 = ADVANCED_FACE ( 'NONE', ( #12049 ), #73034, .T. ) ;
#26970 = AXIS2_PLACEMENT_3D ( 'NONE', #46553, #31541, #62037 ) ;
#26971 = DIRECTION ( 'NONE',  ( 0.000000000000000000, 1.000000000000000000, 0.000000000000000000 ) ) ;
#26972 = EDGE_CURVE ( 'NONE', #35670, #8560, #55813, .T. ) ;
#26973 = CARTESIAN_POINT ( 'NONE',  ( -2.816281873526473856, 59.33196800326374643, 3.434112377981055619 ) ) ;
#26974 = VERTEX_POINT ( 'NONE', #22527 ) ;
#26975 = CARTESIAN_POINT ( 'NONE',  ( 13.43411237798106583, 7.665301336597086568, -12.81628187352647252 ) ) ;
#26976 = CARTESIAN_POINT ( 'NONE',  ( -5.999999999999994671, 43.00000000000000000, 4.250000000000000000 ) ) ;
#26977 = CARTESIAN_POINT ( 'NONE',  ( 20.88017736071110164, 35.35535201082150536, 2.915334737309930979 ) ) ;
#26978 = CARTESIAN_POINT ( 'NONE',  ( 2.791683348922237240, 65.38393115100078035, -7.208316651077763204 ) ) ;
#26979 = ORIENTED_EDGE ( 'NONE', *, *, #71412, .F. ) ;
#26981 = CARTESIAN_POINT ( 'NONE',  ( -14.04391541078760675, 15.00000000000000000, -3.608107528143027043 ) ) ;
#26980 = CARTESIAN_POINT ( 'NONE',  ( 1.472469842513823179, 11.42559781766745175, 4.923371831947296329 ) ) ;
#26982 = CARTESIAN_POINT ( 'NONE',  ( 7.361572987183170547, 12.05059781766744997, 9.846743663894590881 ) ) ;
#26983 = APPLICATION_CONTEXT ( 'automotive_design' ) ;
#26984 = CARTESIAN_POINT ( 'NONE',  ( 19.84674366389459266, 18.30059781766745175, 2.638427012816836559 ) ) ;
#26985 = CARTESIAN_POINT ( 'NONE',  ( 14.92337183194729988, 9.342264484334119601, -8.527530157486177487 ) ) ;
#26987 = LINE ( 'NONE', #4991, #54735 ) ;
#26986 = CARTESIAN_POINT ( 'NONE',  ( 4.559911319644449179, 52.23035201082151247, -9.422509992056141925 ) ) ;
#26988 = CARTESIAN_POINT ( 'NONE',  ( 19.84674366389459266, 3.717264484334118713, -2.638427012816827677 ) ) ;
#26990 = ORIENTED_EDGE ( 'NONE', *, *, #89741, .F. ) ;
#26989 = CARTESIAN_POINT ( 'NONE',  ( 0.1532563361054100626, 15.80059781766745353, -2.638427012816831230 ) ) ;
#26991 = CARTESIAN_POINT ( 'NONE',  ( -8.606322355891443010, 3.794835101497137347E-16, 11.66967075398801335 ) ) ;
#26992 = EDGE_CURVE ( 'NONE', #63612, #80095, #77472, .T. ) ;
#26993 = CARTESIAN_POINT ( 'NONE',  ( 0.1532563361054100626, 60.80059781766744464, -2.638427012816831230 ) ) ;
#26994 = ORIENTED_EDGE ( 'NONE', *, *, #28772, .F. ) ;
#26995 = CARTESIAN_POINT ( 'NONE',  ( -3.699999999999999289, -2.245204982926630245E-16, 4.714890176717308529E-16 ) ) ;
#26996 = CARTESIAN_POINT ( 'NONE',  ( 24.16423886937410614, 14.30374883491396787, 8.672049930838204340E-16 ) ) ;
#26997 = EDGE_CURVE ( 'NONE', #14094, #16059, #540, .T. ) ;
#26998 = DIRECTION ( 'NONE',  ( 0.000000000000000000, 1.000000000000000000, 0.000000000000000000 ) ) ;
#26999 = CARTESIAN_POINT ( 'NONE',  ( -0.3689425029237881626, 17.42874883491397142, 10.36894250292379027 ) ) ;
#27000 = CARTESIAN_POINT ( 'NONE',  ( 17.08211943468705840, 35.13708216824730357, -12.26659068614894466 ) ) ;
#27001 = AXIS2_PLACEMENT_3D ( 'NONE', #56239, #78736, #10244 ) ;
#27002 = FACE_OUTER_BOUND ( 'NONE', #13387, .T. ) ;
#27003 = FILL_AREA_STYLE ('',( #11509 ) ) ;
#27004 = CARTESIAN_POINT ( 'NONE',  ( 19.42250999205614193, 30.14701867748817321, 5.440088680355555262 ) ) ;
#27005 = DIRECTION ( 'NONE',  ( 0.000000000000000000, 0.000000000000000000, 1.000000000000000000 ) ) ;
#27006 = CARTESIAN_POINT ( 'NONE',  ( 1.472469842513823179, 15.59226448433411960, -4.923371831947296329 ) ) ;
#27008 = CARTESIAN_POINT ( 'NONE',  ( 0.1532563361054100626, 20.80059781766744464, -2.638427012816831230 ) ) ;
#27007 = CARTESIAN_POINT ( 'NONE',  ( 10.00000000000000178, 59.31368534415484106, 10.88017736071110342 ) ) ;
#27009 = CARTESIAN_POINT ( 'NONE',  ( 4.559911319644449179, 17.23035201082150536, -9.422509992056141925 ) ) ;
#27010 = CARTESIAN_POINT ( 'NONE',  ( -1.099225684535947600, 43.70696800326375353, -6.408140936763238038 ) ) ;
#27011 = CARTESIAN_POINT ( 'NONE',  ( 18.52753015748617571, 48.09226448433412315, 4.923371831947298993 ) ) ;
#27012 = CARTESIAN_POINT ( 'NONE',  ( 18.52753015748618282, 58.92559781766745886, -4.923371831947291888 ) ) ;
#27013 = CARTESIAN_POINT ( 'NONE',  ( -2.816281873526471635, 23.91530133659708568, -3.434112377981056508 ) ) ;
#27014 = CARTESIAN_POINT ( 'NONE',  ( 3.795296366450306547, -29.65458449841936428, -14.16423886937410259 ) ) ;
#27015 = CARTESIAN_POINT ( 'NONE',  ( 0.1532563361054100626, 35.80059781766745175, -2.638427012816831230 ) ) ;
#27016 = CARTESIAN_POINT ( 'NONE',  ( 10.00000000000000178, 8.053748834913967869, 14.16423886937410082 ) ) ;
#27017 = ORIENTED_EDGE ( 'NONE', *, *, #28711, .F. ) ;
#27018 = DIRECTION ( 'NONE',  ( 1.000000000000000000, -0.000000000000000000, -0.000000000000000000 ) ) ;
#27019 = CARTESIAN_POINT ( 'NONE',  ( -0.8801773607111009756, 53.06368534415484106, 1.068504757029289695E-15 ) ) ;
#27020 = CARTESIAN_POINT ( 'NONE',  ( 17.96484262340118221, 51.18868534415483396, -7.964842623401177768 ) ) ;
#27021 = CARTESIAN_POINT ( 'NONE',  ( 2.917880565312948704, 47.63708216824730357, 12.26659068614894643 ) ) ;
#27022 = CARTESIAN_POINT ( 'NONE',  ( 14.92337183194729988, 49.34226448433411605, -8.527530157486177487 ) ) ;
#27023 = CARTESIAN_POINT ( 'NONE',  ( -14.82629065241402699, 14.76984952912780003, -1.844815641836186293 ) ) ;
#27024 = CARTESIAN_POINT ( 'NONE',  ( 7.084665262690076126, 42.02201867748816966, -10.88017736071110164 ) ) ;
#27025 = CARTESIAN_POINT ( 'NONE',  ( -6.617298650316658204, -58.37178459782693096, -2.500000000000000000 ) ) ;
#27026 = ADVANCED_FACE ( 'NONE', ( #30987 ), #46489, .T. ) ;
#27027 = CARTESIAN_POINT ( 'NONE',  ( 21.09922568453595559, 22.04030133659708923, -6.408140936763230044 ) ) ;
#27028 = CARTESIAN_POINT ( 'NONE',  ( 2.791683348922237240, 50.38393115100078035, -7.208316651077763204 ) ) ;
#27029 = CARTESIAN_POINT ( 'NONE',  ( 10.88017736071110164, 15.35535201082150891, 2.915334737309921209 ) ) ;
#27030 = CARTESIAN_POINT ( 'NONE',  ( 4.559911319644449179, 3.897018677488170990, 9.422509992056141925 ) ) ;
#27031 = CARTESIAN_POINT ( 'NONE',  ( -11.94665733272764463, 0.2301501672491015338, -8.972157519073791221 ) ) ;
#27032 = EDGE_CURVE ( 'NONE', #97225, #92281, #16501, .T. ) ;
#27033 = CARTESIAN_POINT ( 'NONE',  ( 12.91533473730993009, 6.605352010821504471, -10.88017736071109987 ) ) ;
#27034 = CARTESIAN_POINT ( 'NONE',  ( 19.42250999205614548, 60.98035201082151247, -5.440088680355545492 ) ) ;
#27035 = CARTESIAN_POINT ( 'NONE',  ( 2.791683348922237240, 0.3839311510007847872, -7.208316651077763204 ) ) ;
#27036 = CARTESIAN_POINT ( 'NONE',  ( 17.75000000000000355, 78.80384757729335377, -4.000000000000000000 ) ) ;
#27037 = CARTESIAN_POINT ( 'NONE',  ( 18.52753015748618282, 38.92559781766745175, -4.923371831947291888 ) ) ;
#27038 = CARTESIAN_POINT ( 'NONE',  ( 20.88017736071110164, 25.35535201082150891, 2.915334737309930979 ) ) ;
#27039 = CARTESIAN_POINT ( 'NONE',  ( 18.52753015748618282, 63.92559781766745886, -4.923371831947291888 ) ) ;
#27041 = CARTESIAN_POINT ( 'NONE',  ( 2.781662917646512463E-16, 22.11937003968011695, 0.000000000000000000 ) ) ;
#27040 = CARTESIAN_POINT ( 'NONE',  ( 4.559911319644449179, 38.89701867748817676, 9.422509992056141925 ) ) ;
#27042 = LINE ( 'NONE', #5050, #9832 ) ;
#27043 = CARTESIAN_POINT ( 'NONE',  ( 22.81628187352647785, 36.62363466993041783, 6.195893100308588602E-16 ) ) ;
#27044 = ORIENTED_EDGE ( 'NONE', *, *, #80497, .T. ) ;
#27045 = CARTESIAN_POINT ( 'NONE',  ( 20.88017736071110164, 45.35535201082149115, 2.915334737309930979 ) ) ;
#27047 = FACE_OUTER_BOUND ( 'NONE', #73306, .T. ) ;
#27046 = CARTESIAN_POINT ( 'NONE',  ( 10.00000000000000000, 17.87363466993041783, -12.81628187352647608 ) ) ;
#27048 = CARTESIAN_POINT ( 'NONE',  ( 18.52753015748617571, 3.092264484334118269, 4.923371831947298993 ) ) ;
#27049 = CARTESIAN_POINT ( 'NONE',  ( -0.8801773607111009756, 23.06368534415484106, 1.068504757029289695E-15 ) ) ;
#27050 = CARTESIAN_POINT ( 'NONE',  ( 24.16423886937409904, 64.09541550158064638, 3.795296366450317205 ) ) ;
#27051 = CARTESIAN_POINT ( 'NONE',  ( 5.076628168052704559, 55.17559781766745175, -8.527530157486179263 ) ) ;
#27052 = CARTESIAN_POINT ( 'NONE',  ( 12.63842701281683034, 2.467264484334118269, 9.846743663894596210 ) ) ;
#27053 = CARTESIAN_POINT ( 'NONE',  ( 17.96484262340118221, 59.93868534415484106, 7.964842623401181321 ) ) ;
#27054 = FACE_OUTER_BOUND ( 'NONE', #35910, .T. ) ;
#27055 = CARTESIAN_POINT ( 'NONE',  ( 6.204703633549690345, 35.76208216824729647, -14.16423886937410259 ) ) ;
#27056 = CIRCLE ( 'NONE', #19075, 0.09999999999999982514 ) ;
#27057 = DIRECTION ( 'NONE',  ( 0.000000000000000000, 0.000000000000000000, 1.000000000000000000 ) ) ;
#27058 = FACE_OUTER_BOUND ( 'NONE', #87006, .T. ) ;
#27059 = ORIENTED_EDGE ( 'NONE', *, *, #77550, .T. ) ;
#27060 = CARTESIAN_POINT ( 'NONE',  ( -2.266590686148945544, 51.38708216824730357, -7.082119434687050408 ) ) ;
#27061 = CARTESIAN_POINT ( 'NONE',  ( 22.26659068614894466, 53.88708216824731068, 7.082119434687054849 ) ) ;
#27062 = CARTESIAN_POINT ( 'NONE',  ( 17.20831665107776587, 19.13393115100078035, -7.208316651077762316 ) ) ;
#27063 = CARTESIAN_POINT ( 'NONE',  ( 0.6178305044545838731, 29.74863466993042138, 9.382169495545420901 ) ) ;
#27064 = CARTESIAN_POINT ( 'NONE',  ( -8.900000000000002132, 83.99999999999994316, -2.900000000000000799 ) ) ;
#27065 = CARTESIAN_POINT ( 'NONE',  ( -0.2418659066527659718, 42.23410085661204505, -6.114288769123055189 ) ) ;
#27067 = CARTESIAN_POINT ( 'NONE',  ( 0.6178305044545838731, 44.74863466993042493, 9.382169495545420901 ) ) ;
#27066 = DIRECTION ( 'NONE',  ( 1.000000000000000000, 4.683753385137374737E-14, 0.000000000000000000 ) ) ;
#27068 = CARTESIAN_POINT ( 'NONE',  ( 22.26659068614895176, 44.72041550158063927, -7.082119434687042414 ) ) ;
#27069 = FACE_OUTER_BOUND ( 'NONE', #21320, .T. ) ;
#27070 = CARTESIAN_POINT ( 'NONE',  ( 10.00000000000000000, 14.75893115100078568, -9.846743663894594434 ) ) ;
#27071 = CARTESIAN_POINT ( 'NONE',  ( -7.208316651077756099, 6.633931151000788340, 7.208316651077766757 ) ) ;
#27072 = VERTEX_POINT ( 'NONE', #52511 ) ;
#27073 = CARTESIAN_POINT ( 'NONE',  ( 5.076628168052703671, 21.84226448433411960, 8.527530157486179263 ) ) ;
#27074 = ORIENTED_EDGE ( 'NONE', *, *, #57176, .F. ) ;
#27075 = DIRECTION ( 'NONE',  ( 1.000000000000000000, 0.000000000000000000, 0.000000000000000000 ) ) ;
#27076 = ORIENTED_EDGE ( 'NONE', *, *, #17316, .T. ) ;
#27078 = CARTESIAN_POINT ( 'NONE',  ( 12.91533473730992121, 19.52201867748816611, 10.88017736071110164 ) ) ;
#27077 = CARTESIAN_POINT ( 'NONE',  ( 7.084665262690076126, 19.10535201082150181, 10.88017736071109987 ) ) ;
#27080 = CARTESIAN_POINT ( 'NONE',  ( 22.81628187352647785, 6.623634669930420493, 6.195893100308588602E-16 ) ) ;
#27079 = CARTESIAN_POINT ( 'NONE',  ( 12.63842701281683922, 49.55059781766744464, -9.846743663894590881 ) ) ;
#27081 = DIRECTION ( 'NONE',  ( 0.000000000000000000, 0.000000000000000000, 1.000000000000000000 ) ) ;
#27082 = EDGE_CURVE ( 'NONE', #41530, #30913, #39004, .T. ) ;
#27083 = CARTESIAN_POINT ( 'NONE',  ( 13.43411237798105340, 15.58196800326374998, 12.81628187352647963 ) ) ;
#27084 = ORIENTED_EDGE ( 'NONE', *, *, #29003, .T. ) ;
#27085 = CARTESIAN_POINT ( 'NONE',  ( 2.791683348922240793, 31.63393115100078745, 7.208316651077764092 ) ) ;
#27086 = CARTESIAN_POINT ( 'NONE',  ( 13.79529636645030344, 58.26208216824728936, 14.16423886937410614 ) ) ;
#27087 = CARTESIAN_POINT ( 'NONE',  ( 4.559911319644449179, 8.897018677488173211, 9.422509992056141925 ) ) ;
#27088 = ORIENTED_EDGE ( 'NONE', *, *, #70808, .T. ) ;
#27089 = CARTESIAN_POINT ( 'NONE',  ( 7.084665262690076126, 34.10535201082151247, 10.88017736071109987 ) ) ;
#27090 = CARTESIAN_POINT ( 'NONE',  ( 19.42250999205614548, 45.98035201082150536, -5.440088680355545492 ) ) ;
#27091 = CARTESIAN_POINT ( 'NONE',  ( -0.8801773607111008646, 53.27201867748816966, 2.915334737309923430 ) ) ;
#27092 = CARTESIAN_POINT ( 'NONE',  ( 0.000000000000000000, -97.00000000000000000, -4.000000000000000000 ) ) ;
#27093 = CARTESIAN_POINT ( 'NONE',  ( 2.035157376598824452, 43.68868534415484106, 7.964842623401179544 ) ) ;
#27094 = PRESENTATION_LAYER_ASSIGNMENT (  '', '', ( #70236 ) ) ;
#27095 = CARTESIAN_POINT ( 'NONE',  ( 1.274849032794292736, 47.55509018479936856, -6.499999999999977796 ) ) ;
#27096 = AXIS2_PLACEMENT_3D ( 'NONE', #24532, #55999, #68660 ) ;
#27098 = ORIENTED_EDGE ( 'NONE', *, *, #82331, .F. ) ;
#27097 = DIRECTION ( 'NONE',  ( -0.000000000000000000, -0.000000000000000000, -1.000000000000000000 ) ) ;
#27099 = EDGE_CURVE ( 'NONE', #31960, #85529, #57749, .T. ) ;
#27100 = CARTESIAN_POINT ( 'NONE',  ( 2.791683348922240793, 11.63393115100078568, 7.208316651077764092 ) ) ;
#27101 = VERTEX_POINT ( 'NONE', #1015 ) ;
#27102 = CARTESIAN_POINT ( 'NONE',  ( 11.29389914963937969, -89.89072489379410058, 4.000000000000002665 ) ) ;
#27103 = CARTESIAN_POINT ( 'NONE',  ( 1.472469842513823179, 60.59226448433412315, -4.923371831947296329 ) ) ;
#27104 = DIRECTION ( 'NONE',  ( -0.000000000000000000, -0.000000000000000000, -1.000000000000000000 ) ) ;
#27105 = CARTESIAN_POINT ( 'NONE',  ( 3.591859063236763294, 53.29030133659708923, -11.09922568453595026 ) ) ;
#27106 = EDGE_CURVE ( 'NONE', #55108, #91827, #11125, .T. ) ;
#27107 = CARTESIAN_POINT ( 'NONE',  ( 7.313705784284593392, 15.00000000000000000, -13.09617149020743732 ) ) ;
#27108 = ORIENTED_EDGE ( 'NONE', *, *, #46885, .F. ) ;
#27109 = CARTESIAN_POINT ( 'NONE',  ( -46.21538524526006597, 104.1852450480875660, 5.851526435683386040 ) ) ;
#27110 = CARTESIAN_POINT ( 'NONE',  ( -1.326515405095929800, 14.76930270348882068, -14.88215077106016970 ) ) ;
#27112 = CARTESIAN_POINT ( 'NONE',  ( 17.20831665107776587, 29.13393115100078390, -7.208316651077762316 ) ) ;
#27111 = SURFACE_SIDE_STYLE ('',( #64606 ) ) ;
#27113 = CARTESIAN_POINT ( 'NONE',  ( 6.204703633549690345, 62.84541550158063927, 14.16423886937410082 ) ) ;
#27114 = DIRECTION ( 'NONE',  ( 1.000000000000000000, 0.000000000000000000, 0.000000000000000000 ) ) ;
#27115 = ORIENTED_EDGE ( 'NONE', *, *, #53334, .F. ) ;
#27116 = CARTESIAN_POINT ( 'NONE',  ( -12.00809552683946357, 0.5000000000000004441, -8.989195838243713155 ) ) ;
#27117 = CARTESIAN_POINT ( 'NONE',  ( 7.361572987183169658, 29.96726448433411960, -9.846743663894592657 ) ) ;
#27118 = CARTESIAN_POINT ( 'NONE',  ( 10.00000000000000178, 65.37363466993042493, 12.81628187352647608 ) ) ;
#27119 = CARTESIAN_POINT ( 'NONE',  ( 21.09922568453595559, 2.040301336597086568, -6.408140936763230044 ) ) ;
#27120 = CARTESIAN_POINT ( 'NONE',  ( 0.1532563361054083140, 1.008931151000784787, 1.131784320476157264E-15 ) ) ;
#27121 = CARTESIAN_POINT ( 'NONE',  ( 0.1532563361054083140, 6.008931151000784787, 1.131784320476157264E-15 ) ) ;
#27122 = CARTESIAN_POINT ( 'NONE',  ( 18.52753015748617571, 63.09226448433412315, 4.923371831947298993 ) ) ;
#27123 = CARTESIAN_POINT ( 'NONE',  ( 9.779999999999990479, 20.99999999999999645, 2.900000000000000355 ) ) ;
#27124 = EDGE_LOOP ( 'NONE', ( #88297, #3629, #96856, #19610, #13285, #4731 ) ) ;
#27125 = CARTESIAN_POINT ( 'NONE',  ( 19.42250999205614193, 5.147018677488171434, 5.440088680355555262 ) ) ;
#27126 = CARTESIAN_POINT ( 'NONE',  ( 20.36894250292379738, 4.928748834913967869, -10.36894250292379027 ) ) ;
#27127 = CARTESIAN_POINT ( 'NONE',  ( 0.1532563361054083140, 11.00893115100078568, 1.131784320476157264E-15 ) ) ;
#27128 = CARTESIAN_POINT ( 'NONE',  ( 17.96484262340118221, 46.18868534415484106, -7.964842623401177768 ) ) ;
#27130 = CARTESIAN_POINT ( 'NONE',  ( 2.035157376598822676, 67.43868534415484817, -7.964842623401177768 ) ) ;
#27129 = CARTESIAN_POINT ( 'NONE',  ( 19.38216949554541557, 32.24863466993041783, -9.382169495545420901 ) ) ;
#27131 = FILL_AREA_STYLE_COLOUR ( '', #20052 ) ;
#27132 = CARTESIAN_POINT ( 'NONE',  ( 19.72487221294571569, 17.80223176428831522, -6.499999999999990230 ) ) ;
#27133 = CARTESIAN_POINT ( 'NONE',  ( 0.000000000000000000, 0.000000000000000000, 0.000000000000000000 ) ) ;
#27134 = CARTESIAN_POINT ( 'NONE',  ( -1.099225684535947600, -1.293031996736246469, -6.408140936763238038 ) ) ;
#27135 = CARTESIAN_POINT ( 'NONE',  ( 2.791683348922240793, 16.63393115100078745, 7.208316651077764092 ) ) ;
#27136 = CARTESIAN_POINT ( 'NONE',  ( -10.88017736071110164, -22.14464798917849109, -2.915334737309917212 ) ) ;
#27137 = CARTESIAN_POINT ( 'NONE',  ( -1.099225684535947600, 28.70696800326375353, -6.408140936763238038 ) ) ;
#27138 = DIRECTION ( 'NONE',  ( 1.000000000000000000, 6.938893903907221278E-15, 0.000000000000000000 ) ) ;
#27140 = CARTESIAN_POINT ( 'NONE',  ( 3.772706337463130544E-18, 0.2999999999999981570, 0.000000000000000000 ) ) ;
#27139 = CARTESIAN_POINT ( 'NONE',  ( 2.035157376598822676, 22.43868534415483396, -7.964842623401177768 ) ) ;
#27141 = CARTESIAN_POINT ( 'NONE',  ( -10.19513985507820486, 14.49999999999999112, -11.00268709613237306 ) ) ;
#27142 = CARTESIAN_POINT ( 'NONE',  ( 20.36894250292379738, 44.92874883491396787, -10.36894250292379027 ) ) ;
#27143 = EDGE_CURVE ( 'NONE', #23604, #53783, #93531, .T. ) ;
#27144 = DIRECTION ( 'NONE',  ( 0.000000000000000000, 0.000000000000000000, -1.000000000000000000 ) ) ;
#27145 = CARTESIAN_POINT ( 'NONE',  ( 0.1532563361054083140, 46.00893115100079456, 1.131784320476157264E-15 ) ) ;
#27146 = CARTESIAN_POINT ( 'NONE',  ( 10.00000000000000000, 37.87363466993041783, -12.81628187352647608 ) ) ;
#27147 = CARTESIAN_POINT ( 'NONE',  ( 0.5774900079438607392, 23.48035201082150536, 5.440088680355550821 ) ) ;
#27148 = CARTESIAN_POINT ( 'NONE',  ( 18.52753015748617571, 58.09226448433411605, 4.923371831947298993 ) ) ;
#27149 = CARTESIAN_POINT ( 'NONE',  ( 0.5774900079438590739, 47.64701867748817676, -5.440088680355550821 ) ) ;
#27150 = CARTESIAN_POINT ( 'NONE',  ( 0.6178305044545838731, 4.748634669930420493, 9.382169495545420901 ) ) ;
#27151 = CARTESIAN_POINT ( 'NONE',  ( 22.26659068614895176, 34.72041550158063927, -7.082119434687042414 ) ) ;
#27152 = CARTESIAN_POINT ( 'NONE',  ( -14.69227023463708726, 14.95077488074851502, -1.335400878252729573 ) ) ;
#27153 = UNCERTAINTY_MEASURE_WITH_UNIT (LENGTH_MEASURE( 1.000000000000000082E-05 ), #5641, 'distance_accuracy_value', 'NONE');
#27154 = CARTESIAN_POINT ( 'NONE',  ( 0.1532563361054083140, 21.00893115100078745, 1.131784320476157264E-15 ) ) ;
#27155 = CARTESIAN_POINT ( 'NONE',  ( 22.81628187352647785, 61.62363466993041783, 6.195893100308588602E-16 ) ) ;
#27156 = CARTESIAN_POINT ( 'NONE',  ( 10.00000000000000000, 2.873634669930420049, -12.81628187352647608 ) ) ;
#27157 = ORIENTED_EDGE ( 'NONE', *, *, #60667, .F. ) ;
#27158 = CARTESIAN_POINT ( 'NONE',  ( 19.80448550324508616, 11.82703681773342907, 6.500000000002751577 ) ) ;
#27159 = CARTESIAN_POINT ( 'NONE',  ( 6.004190426492125532, -34.81345361117713111, 2.750000000000000000 ) ) ;
#27160 = CARTESIAN_POINT ( 'NONE',  ( 19.42250999205614548, 10.98035201082150536, -5.440088680355545492 ) ) ;
#27162 = DIRECTION ( 'NONE',  ( 0.000000000000000000, 1.000000000000000000, 0.000000000000000000 ) ) ;
#27161 = CARTESIAN_POINT ( 'NONE',  ( -0.3689425029237881626, 22.42874883491397142, 10.36894250292379027 ) ) ;
#27163 = CARTESIAN_POINT ( 'NONE',  ( 19.42250999205614193, 65.14701867748817676, 5.440088680355555262 ) ) ;
#27164 = CARTESIAN_POINT ( 'NONE',  ( 14.92337183194729988, 54.34226448433412315, -8.527530157486177487 ) ) ;
#27165 = CARTESIAN_POINT ( 'NONE',  ( 17.96484262340118221, 29.93868534415484106, 7.964842623401181321 ) ) ;
#27166 = DIRECTION ( 'NONE',  ( -0.000000000000000000, -0.000000000000000000, -1.000000000000000000 ) ) ;
#27167 = DIRECTION ( 'NONE',  ( 0.8070303256584298035, -0.5905099943842175847, 0.000000000000000000 ) ) ;
#27168 = VECTOR ( 'NONE', #67702, 1000.000000000000000 ) ;
#27169 = ORIENTED_EDGE ( 'NONE', *, *, #62861, .F. ) ;
#27170 = CARTESIAN_POINT ( 'NONE',  ( 6.685141491970859384, -80.57575624202263498, 2.500000000000000444 ) ) ;
#27171 = ORIENTED_EDGE ( 'NONE', *, *, #80594, .T. ) ;
#27172 = ORIENTED_EDGE ( 'NONE', *, *, #94988, .T. ) ;
#27173 = DIRECTION ( 'NONE',  ( 1.000000000000000000, -0.000000000000000000, -0.000000000000000000 ) ) ;
#27174 = CARTESIAN_POINT ( 'NONE',  ( -0.3689425029237898834, 6.178748834913968757, -10.36894250292378850 ) ) ;
#27175 = CARTESIAN_POINT ( 'NONE',  ( 20.36894250292379738, 9.928748834913966093, -10.36894250292379027 ) ) ;
#27176 = CARTESIAN_POINT ( 'NONE',  ( 17.96484262340118221, 41.18868534415484106, -7.964842623401177768 ) ) ;
#27177 = CARTESIAN_POINT ( 'NONE',  ( 24.16423886937410614, 49.51208216824730357, -3.795296366450302550 ) ) ;
#27178 = CARTESIAN_POINT ( 'NONE',  ( 7.361572987183170547, 62.05059781766745886, 9.846743663894590881 ) ) ;
#27179 = CARTESIAN_POINT ( 'NONE',  ( 17.20831665107776587, 29.13393115100078390, -7.208316651077762316 ) ) ;
#27180 = DIRECTION ( 'NONE',  ( 0.000000000000000000, -1.000000000000000000, 0.000000000000000000 ) ) ;
#27182 = CARTESIAN_POINT ( 'NONE',  ( 21.09922568453594849, 11.20696800326375531, 6.408140936763242479 ) ) ;
#27181 = CARTESIAN_POINT ( 'NONE',  ( 15.44008868035555260, 34.73035201082151247, 9.422509992056143702 ) ) ;
#27183 = CARTESIAN_POINT ( 'NONE',  ( 2.917880565312948704, 2.637082168247300906, 12.26659068614894643 ) ) ;
#27184 = CARTESIAN_POINT ( 'NONE',  ( 17.08211943468705840, 50.13708216824730357, -12.26659068614894466 ) ) ;
#27185 = CARTESIAN_POINT ( 'NONE',  ( 15.44008868035555793, 6.397018677488171434, -9.422509992056140149 ) ) ;
#27186 = CARTESIAN_POINT ( 'NONE',  ( 18.04007052943772038, 39.00257860105349295, -5.767676674365850076 ) ) ;
#27187 = CARTESIAN_POINT ( 'NONE',  ( -0.1503990784575328643, 15.12777174578612538, 6.262539305110068177 ) ) ;
#27188 = CARTESIAN_POINT ( 'NONE',  ( 2.638427012816829897, -35.44940218233254114, -9.846743663894592657 ) ) ;
#27189 = ORIENTED_EDGE ( 'NONE', *, *, #54530, .F. ) ;
#27190 =( NAMED_UNIT ( * ) SI_UNIT ( $, .STERADIAN. ) SOLID_ANGLE_UNIT ( ) );
#27191 = EDGE_LOOP ( 'NONE', ( #98122, #87094, #10157, #17112, #16238, #62590 ) ) ;
#27192 = CARTESIAN_POINT ( 'NONE',  ( 18.52753015748617571, 18.09226448433411960, 4.923371831947298993 ) ) ;
#27193 = VERTEX_POINT ( 'NONE', #93470 ) ;
#27194 = CARTESIAN_POINT ( 'NONE',  ( 13.79529636645030344, 33.26208216824730357, 14.16423886937410614 ) ) ;
#27195 = CARTESIAN_POINT ( 'NONE',  ( 19.84674366389459266, 38.30059781766745175, 2.638427012816836559 ) ) ;
#27196 = CARTESIAN_POINT ( 'NONE',  ( 7.084665262690076126, 52.02201867748816255, -10.88017736071110164 ) ) ;
#27197 = CARTESIAN_POINT ( 'NONE',  ( 0.000000000000000000, 15.00000000000000000, 0.000000000000000000 ) ) ;
#27198 = ADVANCED_FACE ( 'NONE', ( #24997 ), #72426, .T. ) ;
#27199 = CARTESIAN_POINT ( 'NONE',  ( 17.96484262340118221, 59.93868534415484106, 7.964842623401181321 ) ) ;
#27200 = B_SPLINE_CURVE_WITH_KNOTS ( 'NONE', 3,
 ( #73316, #20330, #18854, #66807, #19823, #35315 ),
 .UNSPECIFIED., .F., .F.,
 ( 4, 2, 4 ),
 ( 0.0002800808511812542118, 0.0006862868719359076263, 0.001092492892690561041 ),
 .UNSPECIFIED. ) ;
#27201 = EDGE_CURVE ( 'NONE', #81929, #60398, #62220, .T. ) ;
#27202 = CARTESIAN_POINT ( 'NONE',  ( 3.591859063236761518, 54.95696800326376064, 11.09922568453594849 ) ) ;
#27203 = CARTESIAN_POINT ( 'NONE',  ( 3.434112377981054287, 2.665301336597088788, -12.81628187352647608 ) ) ;
#27204 = ORIENTED_EDGE ( 'NONE', *, *, #90290, .F. ) ;
#27205 = CARTESIAN_POINT ( 'NONE',  ( -2.266590686148945544, 16.38708216824730357, -7.082119434687050408 ) ) ;
#27206 = ORIENTED_EDGE ( 'NONE', *, *, #61925, .F. ) ;
#27207 = CARTESIAN_POINT ( 'NONE',  ( 0.6178305044545838731, 49.74863466993041072, 9.382169495545420901 ) ) ;
#27208 = CARTESIAN_POINT ( 'NONE',  ( 19.42250999205614548, 20.98035201082150891, -5.440088680355545492 ) ) ;
#27209 = CARTESIAN_POINT ( 'NONE',  ( 14.92337183194729988, 29.34226448433411960, -8.527530157486177487 ) ) ;
#27210 = CARTESIAN_POINT ( 'NONE',  ( 15.44008868035555793, 16.39701867748817321, -9.422509992056140149 ) ) ;
#27211 = CARTESIAN_POINT ( 'NONE',  ( 22.81628187352648496, 51.83196800326376064, -3.434112377981050290 ) ) ;
#27212 = EDGE_CURVE ( 'NONE', #25948, #67069, #3952, .T. ) ;
#27213 = CARTESIAN_POINT ( 'NONE',  ( 70.68973184038034674, 41.77083333333331439, 10.00000000000000000 ) ) ;
#27214 = CARTESIAN_POINT ( 'NONE',  ( 1.472469842513823179, 26.42559781766745175, 4.923371831947296329 ) ) ;
#27216 = AXIS2_PLACEMENT_3D ( 'NONE', #16246, #63200, #70234 ) ;
#27215 = CARTESIAN_POINT ( 'NONE',  ( 21.92686044187656336, 21.97997603579417358, 3.195792623639536423 ) ) ;
#27217 = EDGE_CURVE ( 'NONE', #8762, #9509, #63775, .T. ) ;
#27218 = CARTESIAN_POINT ( 'NONE',  ( 14.37657372141816126, 15.00000000000000888, -2.693041920167344117 ) ) ;
#27219 = CARTESIAN_POINT ( 'NONE',  ( 4.559911319644449179, 67.23035201082150536, -9.422509992056141925 ) ) ;
#27220 = CARTESIAN_POINT ( 'NONE',  ( 0.7166339456633684657, 0.000000000000000000, -15.98010739087745868 ) ) ;
#27221 = CARTESIAN_POINT ( 'NONE',  ( 4.879999999999994564, 43.00000000000000711, 6.250000000000000000 ) ) ;
#27222 = CARTESIAN_POINT ( 'NONE',  ( 18.52753015748617571, 18.09226448433411960, 4.923371831947298993 ) ) ;
#27223 = CARTESIAN_POINT ( 'NONE',  ( 22.81628187352647785, 21.41530133659708923, 3.434112377981063169 ) ) ;
#27224 = VECTOR ( 'NONE', #54943, 1000.000000000000000 ) ;
#27225 = ADVANCED_FACE ( 'NONE', ( #41478 ), #31882, .T. ) ;
#27226 = DIRECTION ( 'NONE',  ( 0.4305110968082926370, 0.000000000000000000, 0.9025852843498617384 ) ) ;
#27227 = AXIS2_PLACEMENT_3D ( 'NONE', #22033, #61482, #68511 ) ;
#27228 = CARTESIAN_POINT ( 'NONE',  ( 1.472469842513823179, 41.42559781766745886, 4.923371831947296329 ) ) ;
#27229 = CARTESIAN_POINT ( 'NONE',  ( -9.641087339108999288, 0.04922511925147086270, 11.16671550067042418 ) ) ;
#27230 = CARTESIAN_POINT ( 'NONE',  ( 20.36894250292379738, 14.92874883491396432, -10.36894250292379027 ) ) ;
#27231 = CARTESIAN_POINT ( 'NONE',  ( 14.92337183194729633, 37.67559781766745175, 8.527530157486181039 ) ) ;
#27232 = CARTESIAN_POINT ( 'NONE',  ( 21.09922568453595559, 27.04030133659708568, -6.408140936763230044 ) ) ;
#27234 = CARTESIAN_POINT ( 'NONE',  ( 7.684764310694791156, 0.3640475087720984049, 12.88194075009940853 ) ) ;
#27233 = CARTESIAN_POINT ( 'NONE',  ( -4.023424921641842289, 15.00000000000000000, 15.48190712851503648 ) ) ;
#27235 = CARTESIAN_POINT ( 'NONE',  ( 7.084665262690076126, 59.10535201082150536, 10.88017736071109987 ) ) ;
#27236 = CARTESIAN_POINT ( 'NONE',  ( 22.81628187352648496, 11.83196800326375531, -3.434112377981050290 ) ) ;
#27237 = DIRECTION ( 'NONE',  ( 0.9961946980917462113, -0.08715574274765140739, 0.000000000000000000 ) ) ;
#27238 = CARTESIAN_POINT ( 'NONE',  ( 5.076628168052703671, 31.84226448433412315, 8.527530157486179263 ) ) ;
#27239 = CARTESIAN_POINT ( 'NONE',  ( 20.88017736071110875, 25.77201867748816966, -2.915334737309920765 ) ) ;
#27240 = CARTESIAN_POINT ( 'NONE',  ( 6.565887622018943937, 33.08196800326374643, -12.81628187352647608 ) ) ;
#27241 = CARTESIAN_POINT ( 'NONE',  ( 2.791683348922237240, 30.38393115100078390, -7.208316651077763204 ) ) ;
#27242 =( NAMED_UNIT ( * ) PLANE_ANGLE_UNIT ( ) SI_UNIT ( $, .RADIAN. ) );
#27243 = DIRECTION ( 'NONE',  ( 0.000000000000000000, 0.000000000000000000, 1.000000000000000000 ) ) ;
#27244 = CARTESIAN_POINT ( 'NONE',  ( 4.559911319644449179, 32.23035201082150536, -9.422509992056141925 ) ) ;
#27245 = ORIENTED_EDGE ( 'NONE', *, *, #23632, .T. ) ;
#27246 = CARTESIAN_POINT ( 'NONE',  ( -5.624999999999997335, 3.755135511184878538, 9.742785792574938597 ) ) ;
#27248 = CARTESIAN_POINT ( 'NONE',  ( 20.88017736071110875, 35.77201867748816966, -2.915334737309920765 ) ) ;
#27247 = CARTESIAN_POINT ( 'NONE',  ( 7.361572987183169658, 49.96726448433410894, -9.846743663894592657 ) ) ;
#27249 = FACE_OUTER_BOUND ( 'NONE', #95612, .T. ) ;
#27250 = CARTESIAN_POINT ( 'NONE',  ( 20.88017736071110875, 65.77201867748817676, -2.915334737309920765 ) ) ;
#27252 = DIRECTION ( 'NONE',  ( 2.478176394252579169E-16, -1.000000000000000000, 0.000000000000000000 ) ) ;
#27251 = CARTESIAN_POINT ( 'NONE',  ( -0.8801773607111009756, 23.06368534415484106, 1.068504757029289695E-15 ) ) ;
#27253 = CARTESIAN_POINT ( 'NONE',  ( -2.614810775378867191, 35.00346125376525919, -7.000000000000000888 ) ) ;
#27254 = CARTESIAN_POINT ( 'NONE',  ( 17.20831665107776587, 54.13393115100079456, -7.208316651077762316 ) ) ;
#27256 = CARTESIAN_POINT ( 'NONE',  ( 6.934008441971972303, -73.15902683813038720, 3.750000000000000888 ) ) ;
#27255 = CARTESIAN_POINT ( 'NONE',  ( 6.204703633549690345, 52.84541550158062506, 14.16423886937410082 ) ) ;
#27257 = CARTESIAN_POINT ( 'NONE',  ( 12.00809552683965364, 14.49999999999999112, -8.989195838243565717 ) ) ;
#27258 = CARTESIAN_POINT ( 'NONE',  ( 24.16423886937410614, 4.303748834913967869, 8.672049930838204340E-16 ) ) ;
#27259 = EDGE_CURVE ( 'NONE', #14459, #80097, #32957, .T. ) ;
#27260 = CARTESIAN_POINT ( 'NONE',  ( -4.164238869374099039, 41.80374883491397497, 8.674139862899312516E-16 ) ) ;
#27261 = CARTESIAN_POINT ( 'NONE',  ( 16.40814093676323893, 0.7903013365970867898, 11.09922568453595026 ) ) ;
#27263 = CARTESIAN_POINT ( 'NONE',  ( -7.037775659072364576, -86.26045094518553924, 2.750000000000000444 ) ) ;
#27262 = AXIS2_PLACEMENT_3D ( 'NONE', #67221, #52215, #61669 ) ;
#27264 = ORIENTED_EDGE ( 'NONE', *, *, #16116, .T. ) ;
#27265 = CARTESIAN_POINT ( 'NONE',  ( -0.3689425029237881626, 67.42874883491396076, 10.36894250292379027 ) ) ;
#27266 = CARTESIAN_POINT ( 'NONE',  ( 14.92337183194729988, 34.34226448433411605, -8.527530157486177487 ) ) ;
#27268 = CARTESIAN_POINT ( 'NONE',  ( 9.898881779040660689, 0.000000000000000000, 10.25059215482582786 ) ) ;
#27267 = DIRECTION ( 'NONE',  ( 0.9304175679820282374, 0.000000000000000000, -0.3665012267242880872 ) ) ;
#27269 = CARTESIAN_POINT ( 'NONE',  ( -0.8801773607110991993, 52.85535201082151247, -2.915334737309923874 ) ) ;
#27270 = FACE_OUTER_BOUND ( 'NONE', #70382, .T. ) ;
#27271 = CARTESIAN_POINT ( 'NONE',  ( 6.565887622018943937, 60.16530133659707502, 12.81628187352647430 ) ) ;
#27272 = CARTESIAN_POINT ( 'NONE',  ( 19.38216949554541202, 30.99863466993042138, 9.382169495545424454 ) ) ;
#27273 = CARTESIAN_POINT ( 'NONE',  ( 17.20831665107776587, 29.13393115100078390, -7.208316651077762316 ) ) ;
#27274 = EDGE_LOOP ( 'NONE', ( #85761, #42296, #21686, #7278 ) ) ;
#27275 = CARTESIAN_POINT ( 'NONE',  ( 1.472469842513823179, 1.425597817667451528, 4.923371831947296329 ) ) ;
#27276 = CARTESIAN_POINT ( 'NONE',  ( -8.000000000000000000, 80.32179676972448590, 4.250000000000000000 ) ) ;
#27277 = CARTESIAN_POINT ( 'NONE',  ( 10.00000000000000000, 65.55374883491396076, -14.16423886937410082 ) ) ;
#27278 = CARTESIAN_POINT ( 'NONE',  ( 7.084665262690076126, 19.10535201082150181, 10.88017736071109987 ) ) ;
#27279 = CARTESIAN_POINT ( 'NONE',  ( 22.26659068614895176, 44.72041550158063927, -7.082119434687042414 ) ) ;
#27280 = CARTESIAN_POINT ( 'NONE',  ( 20.88017736071110519, 30.56368534415484106, 2.639326808657452039E-16 ) ) ;
#27281 = CARTESIAN_POINT ( 'NONE',  ( 10.00000000000000178, 69.31368534415484817, 10.88017736071110342 ) ) ;
#27282 = CARTESIAN_POINT ( 'NONE',  ( 2.618367889266248100E-15, 44.99999999999999289, 7.000000000000000000 ) ) ;
#27283 = CARTESIAN_POINT ( 'NONE',  ( 19.84674366389459621, 48.50893115100078745, 7.409399052514197653E-17 ) ) ;
#27284 = CARTESIAN_POINT ( 'NONE',  ( 1.472469842513823179, 10.59226448433411782, -4.923371831947296329 ) ) ;
#27285 =( NAMED_UNIT ( * ) SI_UNIT ( $, .STERADIAN. ) SOLID_ANGLE_UNIT ( ) );
#27286 = CARTESIAN_POINT ( 'NONE',  ( 5.076628168052703671, 36.84226448433412315, 8.527530157486179263 ) ) ;
#27287 = CARTESIAN_POINT ( 'NONE',  ( 19.84674366389459266, 58.71726448433411605, -2.638427012816827677 ) ) ;
#27288 = CARTESIAN_POINT ( 'NONE',  ( 17.96484262340118221, 21.18868534415483396, -7.964842623401177768 ) ) ;
#27289 = UNCERTAINTY_MEASURE_WITH_UNIT (LENGTH_MEASURE( 1.000000000000000082E-05 ), #80642, 'distance_accuracy_value', 'NONE');
#27290 = STYLED_ITEM ( 'NONE', ( #54576 ), #61971 ) ;
#27291 = VERTEX_POINT ( 'NONE', #54963 ) ;
#27292 = CARTESIAN_POINT ( 'NONE',  ( -2.816281873526473856, 39.33196800326374643, 3.434112377981055619 ) ) ;
#27293 = DIRECTION ( 'NONE',  ( 1.000000000000000000, -0.000000000000000000, -0.000000000000000000 ) ) ;
#27294 = CARTESIAN_POINT ( 'NONE',  ( 17.96484262340118221, 59.93868534415484106, 7.964842623401181321 ) ) ;
#27295 = CARTESIAN_POINT ( 'NONE',  ( 2.791683348922237240, 30.38393115100078390, -7.208316651077763204 ) ) ;
#27297 = CARTESIAN_POINT ( 'NONE',  ( 12.63842701281683922, 24.55059781766745175, -9.846743663894590881 ) ) ;
#27296 = CARTESIAN_POINT ( 'NONE',  ( 10.00000000000000000, 65.55374883491396076, -14.16423886937410082 ) ) ;
#27298 = CARTESIAN_POINT ( 'NONE',  ( 8.439016546559823695, 15.00000000000000000, 11.79122553964979048 ) ) ;
#27299 = CARTESIAN_POINT ( 'NONE',  ( 2.791683348922237240, 65.38393115100078035, -7.208316651077763204 ) ) ;
#27300 = CARTESIAN_POINT ( 'NONE',  ( -4.164238869374099039, 31.80374883491396432, 8.674139862899312516E-16 ) ) ;
#27301 = CARTESIAN_POINT ( 'NONE',  ( 1.472469842513823179, 40.59226448433411605, -4.923371831947296329 ) ) ;
#27302 = VECTOR ( 'NONE', #84377, 1000.000000000000000 ) ;
#27303 = CARTESIAN_POINT ( 'NONE',  ( 4.130000000000000782, 0.09092508112526098696, -2.499999999999999556 ) ) ;
#27304 = CARTESIAN_POINT ( 'NONE',  ( 15.44008868035555793, 31.39701867748817676, -9.422509992056140149 ) ) ;
#27305 = CARTESIAN_POINT ( 'NONE',  ( -0.8801773607111009756, 58.06368534415484106, 1.068504757029289695E-15 ) ) ;
#27306 = DIRECTION ( 'NONE',  ( -1.000000000000000000, 0.000000000000000000, 0.000000000000000000 ) ) ;
#27307 = ORIENTED_EDGE ( 'NONE', *, *, #57997, .F. ) ;
#27308 = CARTESIAN_POINT ( 'NONE',  ( -2.816281873526473856, 39.33196800326374643, 3.434112377981055619 ) ) ;
#27309 = ADVANCED_FACE ( 'NONE', ( #3468 ), #25497, .T. ) ;
#27310 = ORIENTED_EDGE ( 'NONE', *, *, #70682, .F. ) ;
#27311 = CARTESIAN_POINT ( 'NONE',  ( 7.084665262690076126, 52.02201867748816255, -10.88017736071110164 ) ) ;
#27312 = ORIENTED_EDGE ( 'NONE', *, *, #93766, .T. ) ;
#27313 = PRESENTATION_STYLE_ASSIGNMENT (( #10002 ) ) ;
#27314 = DIRECTION ( 'NONE',  ( 0.000000000000000000, 1.000000000000000000, 0.000000000000000000 ) ) ;
#27315 = ORIENTED_EDGE ( 'NONE', *, *, #85593, .F. ) ;
#27317 = EDGE_CURVE ( 'NONE', #98193, #84532, #3145, .T. ) ;
#27316 = CARTESIAN_POINT ( 'NONE',  ( -12.98685442714190508, 4.246409518909109890E-16, -6.449155920601135072 ) ) ;
#27318 = CARTESIAN_POINT ( 'NONE',  ( 12.91533473730992121, 14.52201867748817143, 10.88017736071110164 ) ) ;
#27319 = CARTESIAN_POINT ( 'NONE',  ( -3.195792623639597263, 11.62045670184115664, -11.92686044187653494 ) ) ;
#27320 = FACE_OUTER_BOUND ( 'NONE', #96071, .T. ) ;
#27321 = CARTESIAN_POINT ( 'NONE',  ( 2.035157376598824452, 3.688685344154837953, 7.964842623401179544 ) ) ;
#27322 = CARTESIAN_POINT ( 'NONE',  ( 2.791683348922240793, 26.63393115100078745, 7.208316651077764092 ) ) ;
#27323 = CARTESIAN_POINT ( 'NONE',  ( 6.204703633549690345, 12.84541550158063572, 14.16423886937410082 ) ) ;
#27324 = EDGE_CURVE ( 'NONE', #15285, #26110, #16994, .T. ) ;
#27325 = ADVANCED_FACE ( 'NONE', ( #77973 ), #18460, .F. ) ;
#27326 = CARTESIAN_POINT ( 'NONE',  ( 10.00000000000000178, 29.31368534415483751, 10.88017736071110342 ) ) ;
#27327 = CARTESIAN_POINT ( 'NONE',  ( 14.92337183194729988, 64.34226448433412315, -8.527530157486177487 ) ) ;
#27328 = ORIENTED_EDGE ( 'NONE', *, *, #22702, .T. ) ;
#27329 = CARTESIAN_POINT ( 'NONE',  ( 10.00000000000000000, -2.126365330069579951, -12.81628187352647608 ) ) ;
#27330 = ORIENTED_EDGE ( 'NONE', *, *, #19518, .F. ) ;
#27331 = CARTESIAN_POINT ( 'NONE',  ( 0.5774900079438590739, 47.64701867748817676, -5.440088680355550821 ) ) ;
#27332 = CARTESIAN_POINT ( 'NONE',  ( 5.076628168052703671, 61.84226448433412315, 8.527530157486179263 ) ) ;
#27333 = CARTESIAN_POINT ( 'NONE',  ( 16.40814093676324603, 42.45696800326375353, -11.09922568453594671 ) ) ;
#27335 = DIRECTION ( 'NONE',  ( -1.000000000000000000, 0.000000000000000000, 0.000000000000000000 ) ) ;
#27334 = CARTESIAN_POINT ( 'NONE',  ( 20.88017736071110875, 5.772018677488170546, -2.915334737309920765 ) ) ;
#27336 = CARTESIAN_POINT ( 'NONE',  ( 19.42250999205614548, 65.98035201082151957, -5.440088680355545492 ) ) ;
#27337 = CARTESIAN_POINT ( 'NONE',  ( 17.08211943468705840, 65.13708216824730357, -12.26659068614894466 ) ) ;
#27338 = B_SPLINE_CURVE_WITH_KNOTS ( 'NONE', 3,
 ( #20225, #94744, #34220, #26735 ),
 .UNSPECIFIED., .F., .F.,
 ( 4, 4 ),
 ( 3.127317220692750759E-18, 0.002392975128318519749 ),
 .UNSPECIFIED. ) ;
#27339 = ADVANCED_FACE ( 'NONE', ( #73409 ), #54230, .F. ) ;
#27340 = VECTOR ( 'NONE', #58361, 1000.000000000000000 ) ;
#27341 = AXIS2_PLACEMENT_3D ( 'NONE', #89993, #89506, #60967 ) ;
#27342 = CARTESIAN_POINT ( 'NONE',  ( 3.591859063236761518, 39.95696800326375353, 11.09922568453594849 ) ) ;
#27343 = CARTESIAN_POINT ( 'NONE',  ( 0.5774900079438590739, 27.64701867748817676, -5.440088680355550821 ) ) ;
#27344 = CARTESIAN_POINT ( 'NONE',  ( -8.000000000000000000, 40.74999999999999289, 3.750000000000000000 ) ) ;
#27345 = CARTESIAN_POINT ( 'NONE',  ( 6.565887622018943937, 40.16530133659708923, 12.81628187352647430 ) ) ;
#27346 = CARTESIAN_POINT ( 'NONE',  ( 7.084665262690076126, 34.10535201082151247, 10.88017736071109987 ) ) ;
#27347 = CARTESIAN_POINT ( 'NONE',  ( 17.20831665107776587, 54.13393115100079456, -7.208316651077762316 ) ) ;
#27349 = VERTEX_POINT ( 'NONE', #82395 ) ;
#27348 = EDGE_CURVE ( 'NONE', #50944, #90628, #35825, .T. ) ;
#27350 = CARTESIAN_POINT ( 'NONE',  ( -7.595945211628411187, 15.00000000000000000, 12.35117874301633734 ) ) ;
#27351 = CARTESIAN_POINT ( 'NONE',  ( 10.00000000000000178, 57.25893115100078745, 9.846743663894594434 ) ) ;
#27353 = CARTESIAN_POINT ( 'NONE',  ( 2.791683348922237240, 50.38393115100078035, -7.208316651077763204 ) ) ;
#27352 = DIRECTION ( 'NONE',  ( 0.000000000000000000, -1.000000000000000000, 0.000000000000000000 ) ) ;
#27354 = CARTESIAN_POINT ( 'NONE',  ( 20.88017736071110164, 25.35535201082150891, 2.915334737309930979 ) ) ;
#27355 = CARTESIAN_POINT ( 'NONE',  ( 18.52753015748617571, 38.09226448433412315, 4.923371831947298993 ) ) ;
#27356 = CARTESIAN_POINT ( 'NONE',  ( 6.880000000000009663, 40.99999999999999289, -6.500000000000000888 ) ) ;
#27357 = CARTESIAN_POINT ( 'NONE',  ( -26.69000000000001194, 92.00000000000000000, -9.500000000000000000 ) ) ;
#27359 = CARTESIAN_POINT ( 'NONE',  ( 0.1532563361054082862, 6.217264484334118713, 2.638427012816831674 ) ) ;
#27358 = CARTESIAN_POINT ( 'NONE',  ( 10.00000000000000000, 34.75893115100078745, -9.846743663894594434 ) ) ;
#27360 = CARTESIAN_POINT ( 'NONE',  ( 1.472469842513823179, 1.425597817667451528, 4.923371831947296329 ) ) ;
#27362 = ORIENTED_EDGE ( 'NONE', *, *, #942, .F. ) ;
#27361 = CARTESIAN_POINT ( 'NONE',  ( 19.84674366389459266, 63.30059781766745886, 2.638427012816836559 ) ) ;
#27363 = EDGE_CURVE ( 'NONE', #50168, #30576, #35912, .T. ) ;
#27364 = AXIS2_PLACEMENT_3D ( 'NONE', #43137, #5155, #42656 ) ;
#27365 = CARTESIAN_POINT ( 'NONE',  ( 6.565887622018943937, 38.08196800326376064, -12.81628187352647608 ) ) ;
#27366 = CARTESIAN_POINT ( 'NONE',  ( 19.84674366389459266, 48.30059781766745175, 2.638427012816836559 ) ) ;
#27367 = CARTESIAN_POINT ( 'NONE',  ( -0.8801773607110990882, 57.85535201082150536, -2.915334737309924318 ) ) ;
#27368 = CARTESIAN_POINT ( 'NONE',  ( 24.16423886937410614, 54.51208216824730357, -3.795296366450302550 ) ) ;
#27369 = CARTESIAN_POINT ( 'NONE',  ( 19.84674366389459266, 33.71726448433410894, -2.638427012816827677 ) ) ;
#27370 = CIRCLE ( 'NONE', #12957, 0.5000000000000004441 ) ;
#27371 = DIRECTION ( 'NONE',  ( 0.000000000000000000, 0.000000000000000000, 1.000000000000000000 ) ) ;
#27372 = CARTESIAN_POINT ( 'NONE',  ( 24.16423886937410614, 59.51208216824728936, -3.795296366450302550 ) ) ;
#27373 = CARTESIAN_POINT ( 'NONE',  ( 12.83294900548064099, 14.63595249122789177, -7.766300266068371982 ) ) ;
#27374 = CARTESIAN_POINT ( 'NONE',  ( 15.44008868035555260, 9.730352010821505360, 9.422509992056143702 ) ) ;
#27375 = CARTESIAN_POINT ( 'NONE',  ( 22.26659068614894466, 33.88708216824730357, 7.082119434687054849 ) ) ;
#27377 = CARTESIAN_POINT ( 'NONE',  ( 34.56412365047464874, 11.99999999999999645, -7.000000000000000888 ) ) ;
#27376 = CARTESIAN_POINT ( 'NONE',  ( 17.08211943468705130, 58.47041550158063927, 12.26659068614894998 ) ) ;
#27378 = CARTESIAN_POINT ( 'NONE',  ( 7.684764310694801814, 14.49999999999999112, 12.88194075009947248 ) ) ;
#27379 = VECTOR ( 'NONE', #52637, 1000.000000000000000 ) ;
#27380 = CARTESIAN_POINT ( 'NONE',  ( 19.84674366389459266, 13.71726448433411782, -2.638427012816827677 ) ) ;
#27382 = CARTESIAN_POINT ( 'NONE',  ( 6.565887622018943937, 5.165301336597086568, 12.81628187352647430 ) ) ;
#27381 = CARTESIAN_POINT ( 'NONE',  ( -7.771322705631335204, 4.741813304736951008E-16, -12.24159072199927678 ) ) ;
#27383 = ORIENTED_EDGE ( 'NONE', *, *, #26174, .F. ) ;
#27384 = CARTESIAN_POINT ( 'NONE',  ( 17.96484262340118221, 49.93868534415484106, 7.964842623401181321 ) ) ;
#27385 = CARTESIAN_POINT ( 'NONE',  ( 5.076628168052704559, 50.17559781766745886, -8.527530157486179263 ) ) ;
#27386 = CARTESIAN_POINT ( 'NONE',  ( 14.26139399674457309, 4.693468746458063789E-16, -2.619664342929806988 ) ) ;
#27387 = CARTESIAN_POINT ( 'NONE',  ( 7.361572987183169658, 59.96726448433410894, -9.846743663894592657 ) ) ;
#27388 = CARTESIAN_POINT ( 'NONE',  ( -0.3689425029237881626, 2.428748834913967869, 10.36894250292379027 ) ) ;
#27389 = CARTESIAN_POINT ( 'NONE',  ( 20.36894250292379738, 29.92874883491396432, -10.36894250292379027 ) ) ;
#27390 = CARTESIAN_POINT ( 'NONE',  ( -14.62617646268084926, 14.63595249122789177, -3.327906561567075983 ) ) ;
#27392 = CARTESIAN_POINT ( 'NONE',  ( -11.24999999999999822, 8.130135511184871433, 3.014428414850141458 ) ) ;
#27391 = SURFACE_SIDE_STYLE ('',( #87889 ) ) ;
#27393 = CARTESIAN_POINT ( 'NONE',  ( 2.035157376598824452, 18.68868534415484106, 7.964842623401179544 ) ) ;
#27394 = CARTESIAN_POINT ( 'NONE',  ( 22.81628187352648496, 36.83196800326376064, -3.434112377981050290 ) ) ;
#27395 = CARTESIAN_POINT ( 'NONE',  ( -14.09356342482591451, 14.95077488074853456, -4.360913911515565289 ) ) ;
#27396 = CARTESIAN_POINT ( 'NONE',  ( 0.1532563361054083140, 6.008931151000784787, 1.131784320476157264E-15 ) ) ;
#27397 = DIRECTION ( 'NONE',  ( 0.000000000000000000, 0.000000000000000000, 1.000000000000000000 ) ) ;
#27398 = VERTEX_POINT ( 'NONE', #12914 ) ;
#27399 = CARTESIAN_POINT ( 'NONE',  ( 6.825238882348372726, -50.90120388559804354, -4.000000000000000000 ) ) ;
#27400 = CARTESIAN_POINT ( 'NONE',  ( 13.79529636645030344, 28.26208216824729647, 14.16423886937410614 ) ) ;
#27401 =( NAMED_UNIT ( * ) PLANE_ANGLE_UNIT ( ) SI_UNIT ( $, .RADIAN. ) );
#27402 = EDGE_CURVE ( 'NONE', #87105, #31762, #59767, .T. ) ;
#27403 = CARTESIAN_POINT ( 'NONE',  ( -5.320211218918609930, -24.96484130673367474, 4.000000000000000888 ) ) ;
#27404 = CARTESIAN_POINT ( 'NONE',  ( 12.91533473730992121, 9.522018677488171434, 10.88017736071110164 ) ) ;
#27405 = DIRECTION ( 'NONE',  ( 5.818595309480553908E-17, 1.000000000000000000, -0.000000000000000000 ) ) ;
#27406 = CARTESIAN_POINT ( 'NONE',  ( 17.96484262340118221, 39.93868534415484106, 7.964842623401181321 ) ) ;
#27407 = CARTESIAN_POINT ( 'NONE',  ( 12.91533473730993009, 46.60535201082150536, -10.88017736071109987 ) ) ;
#27408 = CARTESIAN_POINT ( 'NONE',  ( -1.099225684535947600, 18.70696800326375353, -6.408140936763238038 ) ) ;
#27409 = FILL_AREA_STYLE_COLOUR ( '', #50607 ) ;
#27410 = CARTESIAN_POINT ( 'NONE',  ( 1.611620712799448185, 1.046791834471127114, 6.500000000000002665 ) ) ;
#27411 = CARTESIAN_POINT ( 'NONE',  ( 2.791683348922237240, 10.38393115100078390, -7.208316651077763204 ) ) ;
#27412 = DIRECTION ( 'NONE',  ( 1.000000000000000000, 0.000000000000000000, 0.000000000000000000 ) ) ;
#27413 = EDGE_CURVE ( 'NONE', #71943, #13653, #81412, .T. ) ;
#27414 = CARTESIAN_POINT ( 'NONE',  ( 2.035157376598822676, 47.43868534415484817, -7.964842623401177768 ) ) ;
#27415 = VECTOR ( 'NONE', #89277, 1000.000000000000000 ) ;
#27416 = CARTESIAN_POINT ( 'NONE',  ( 22.81628187352648496, 6.831968003263753531, -3.434112377981050290 ) ) ;
#27417 = CARTESIAN_POINT ( 'NONE',  ( 2.035157376598822676, 57.43868534415484106, -7.964842623401177768 ) ) ;
#27418 = CARTESIAN_POINT ( 'NONE',  ( 5.076628168052703671, 21.84226448433411960, 8.527530157486179263 ) ) ;
#27419 = CARTESIAN_POINT ( 'NONE',  ( 22.81628187352647785, 46.62363466993041783, 6.195893100308588602E-16 ) ) ;
#27421 = PRESENTATION_STYLE_ASSIGNMENT (( #96938 ) ) ;
#27420 = CARTESIAN_POINT ( 'NONE',  ( 18.52753015748617571, 3.092264484334118269, 4.923371831947298993 ) ) ;
#27422 = ORIENTED_EDGE ( 'NONE', *, *, #47570, .T. ) ;
#27423 = DIRECTION ( 'NONE',  ( -0.000000000000000000, -0.000000000000000000, -1.000000000000000000 ) ) ;
#27424 = DIRECTION ( 'NONE',  ( 0.000000000000000000, 0.000000000000000000, 1.000000000000000000 ) ) ;
#27425 = CARTESIAN_POINT ( 'NONE',  ( 10.00000000000000178, 14.31368534415483751, 10.88017736071110342 ) ) ;
#27426 = CARTESIAN_POINT ( 'NONE',  ( 22.81628187352647785, 61.41530133659709634, 3.434112377981063169 ) ) ;
#27427 = CARTESIAN_POINT ( 'NONE',  ( 10.00000000000000178, 37.25893115100078745, 9.846743663894594434 ) ) ;
#27428 = CARTESIAN_POINT ( 'NONE',  ( -0.8801773607111009756, 13.06368534415483929, 1.068504757029289695E-15 ) ) ;
#27429 = CARTESIAN_POINT ( 'NONE',  ( 2.035157376598822676, 7.438685344154837509, -7.964842623401177768 ) ) ;
#27430 = ORIENTED_EDGE ( 'NONE', *, *, #90385, .T. ) ;
#27431 = CARTESIAN_POINT ( 'NONE',  ( 10.00000000000000178, 9.313685344154839285, 10.88017736071110342 ) ) ;
#27432 = CARTESIAN_POINT ( 'NONE',  ( 20.88017736071110519, 35.56368534415484106, 2.639326808657452039E-16 ) ) ;
#27434 = CARTESIAN_POINT ( 'NONE',  ( 12.91533473730993009, 26.60535201082150536, -10.88017736071109987 ) ) ;
#27433 = CARTESIAN_POINT ( 'NONE',  ( 0.000000000000000000, 35.00000000000000000, 0.000000000000000000 ) ) ;
#27435 = ORIENTED_EDGE ( 'NONE', *, *, #93798, .F. ) ;
#27436 = CARTESIAN_POINT ( 'NONE',  ( 21.92686044187656691, 9.953790035174472806, 3.195792623639537755 ) ) ;
#27438 = ADVANCED_FACE ( 'NONE', ( #36413 ), #70166, .T. ) ;
#27437 = CARTESIAN_POINT ( 'NONE',  ( -0.8801773607110991993, 27.85535201082150181, -2.915334737309923874 ) ) ;
#27439 = CARTESIAN_POINT ( 'NONE',  ( 4.441537491767904022, -2.700695904837609351, 3.750000000000000000 ) ) ;
#27440 = CARTESIAN_POINT ( 'NONE',  ( 20.15039907845753930, 5.601585745166425490, -6.262539305110069954 ) ) ;
#27441 = CARTESIAN_POINT ( 'NONE',  ( -1.099225684535947600, 64.54030133659709634, 6.408140936763237150 ) ) ;
#27442 = CARTESIAN_POINT ( 'NONE',  ( -1.354709868695722852, 0.5000000000000004441, 14.93870011653150698 ) ) ;
#27443 = CARTESIAN_POINT ( 'NONE',  ( 22.26659068614895176, 29.72041550158063572, -7.082119434687042414 ) ) ;
#27444 = CARTESIAN_POINT ( 'NONE',  ( 7.084665262690076126, 44.10535201082151247, 10.88017736071109987 ) ) ;
#27445 = CARTESIAN_POINT ( 'NONE',  ( -0.8801773607111008646, 33.27201867748817676, 2.915334737309923430 ) ) ;
#27446 = CARTESIAN_POINT ( 'NONE',  ( 0.1532563361054082862, 66.21726448433413736, 2.638427012816831674 ) ) ;
#27447 = ADVANCED_FACE ( 'NONE', ( #57432 ), #27911, .F. ) ;
#27448 = DIRECTION ( 'NONE',  ( 0.000000000000000000, 1.000000000000000000, 0.000000000000000000 ) ) ;
#27449 = CARTESIAN_POINT ( 'NONE',  ( 19.84674366389459266, 48.30059781766745175, 2.638427012816836559 ) ) ;
#27450 = CIRCLE ( 'NONE', #30650, 15.00000000000000000 ) ;
#27451 = DIRECTION ( 'NONE',  ( 0.000000000000000000, -0.000000000000000000, -1.000000000000000000 ) ) ;
#27452 = CARTESIAN_POINT ( 'NONE',  ( 17.20831665107776587, 22.88393115100078745, 7.208316651077764980 ) ) ;
#27453 = CARTESIAN_POINT ( 'NONE',  ( -6.408140936763232709, -35.04303199673624647, 11.09922568453595026 ) ) ;
#27454 = VECTOR ( 'NONE', #11025, 1000.000000000000000 ) ;
#27455 = CARTESIAN_POINT ( 'NONE',  ( 17.96484262340118221, 16.18868534415483396, -7.964842623401177768 ) ) ;
#27456 = CARTESIAN_POINT ( 'NONE',  ( 7.361572987183170547, 22.05059781766745530, 9.846743663894590881 ) ) ;
#27457 = CARTESIAN_POINT ( 'NONE',  ( 17.96484262340118221, 56.18868534415484817, -7.964842623401177768 ) ) ;
#27459 = CARTESIAN_POINT ( 'NONE',  ( -1.099225684535947600, 63.70696800326376774, -6.408140936763238038 ) ) ;
#27458 = CARTESIAN_POINT ( 'NONE',  ( 20.88017736071110519, 15.56368534415483751, 2.639326808657452039E-16 ) ) ;
#27460 = CARTESIAN_POINT ( 'NONE',  ( 17.08211943468705130, 28.47041550158063572, 12.26659068614894998 ) ) ;
#27461 = SURFACE_STYLE_USAGE ( .BOTH. , #34955 ) ;
#27462 = ADVANCED_FACE ( 'NONE', ( #81902 ), #66906, .T. ) ;
#27463 = CARTESIAN_POINT ( 'NONE',  ( -14.26139399674456776, 15.00000000000000000, 2.619664342929695966 ) ) ;
#27464 = VERTEX_POINT ( 'NONE', #74396 ) ;
#27465 = CARTESIAN_POINT ( 'NONE',  ( 3.591859063236763294, 8.290301336597087456, -11.09922568453595026 ) ) ;
#27466 = CARTESIAN_POINT ( 'NONE',  ( -0.3289641300568005855, 15.10497603579417181, 5.963430220938281678 ) ) ;
#27467 = CARTESIAN_POINT ( 'NONE',  ( 7.084665262690076126, 29.10535201082150181, 10.88017736071109987 ) ) ;
#27468 = DIRECTION ( 'NONE',  ( 0.000000000000000000, -1.000000000000000000, 0.000000000000000000 ) ) ;
#27470 = ORIENTED_EDGE ( 'NONE', *, *, #45376, .F. ) ;
#27469 = EDGE_CURVE ( 'NONE', #94718, #13092, #82934, .T. ) ;
#27471 = CARTESIAN_POINT ( 'NONE',  ( 17.20831665107776587, 17.88393115100078745, 7.208316651077764980 ) ) ;
#27472 = CARTESIAN_POINT ( 'NONE',  ( 10.00000000000000000, 9.758931151000785675, -9.846743663894594434 ) ) ;
#27473 = CARTESIAN_POINT ( 'NONE',  ( 12.63842701281683034, 17.46726448433411250, 9.846743663894596210 ) ) ;
#27474 = CARTESIAN_POINT ( 'NONE',  ( 1.472469842513823179, 16.42559781766745175, 4.923371831947296329 ) ) ;
#27475 = CARTESIAN_POINT ( 'NONE',  ( 1.472469842513823179, 0.5922644843341181575, -4.923371831947296329 ) ) ;
#27476 = CARTESIAN_POINT ( 'NONE',  ( -4.285674571761296292, -17.54407107685944212, 2.500000000000000888 ) ) ;
#27478 = DIRECTION ( 'NONE',  ( -1.000000000000000000, 0.000000000000000000, 0.000000000000000000 ) ) ;
#27477 = CARTESIAN_POINT ( 'NONE',  ( 17.96484262340118221, 66.18868534415483396, -7.964842623401177768 ) ) ;
#27479 = CARTESIAN_POINT ( 'NONE',  ( 0.1532563361054100626, 0.8005978176674514168, -2.638427012816831230 ) ) ;
#27481 = VERTEX_POINT ( 'NONE', #57917 ) ;
#27480 = CARTESIAN_POINT ( 'NONE',  ( 7.361572987183170547, 17.05059781766745530, 9.846743663894590881 ) ) ;
#27482 = PRESENTATION_LAYER_ASSIGNMENT (  '', '', ( #9945 ) ) ;
#27483 = CARTESIAN_POINT ( 'NONE',  ( 4.630000000000003446, 1.019547802438464545, 4.000000000000000000 ) ) ;
#27484 = CARTESIAN_POINT ( 'NONE',  ( 18.52753015748617571, 63.09226448433412315, 4.923371831947298993 ) ) ;
#27485 = ORIENTED_EDGE ( 'NONE', *, *, #48131, .F. ) ;
#27486 = CARTESIAN_POINT ( 'NONE',  ( -4.164238869374098151, 21.59541550158063217, -3.795296366450310543 ) ) ;
#27487 = PRODUCT_DEFINITION_CONTEXT ( 'detailed design', #47424, 'design' ) ;
#27488 = CARTESIAN_POINT ( 'NONE',  ( 4.023424921641736596, -0.03417435944610275333, -15.48190712851506667 ) ) ;
#27489 = CARTESIAN_POINT ( 'NONE',  ( 6.204703633549690345, 20.76208216824730357, -14.16423886937410259 ) ) ;
#27490 = CARTESIAN_POINT ( 'NONE',  ( 10.00000000000000000, 35.55374883491396787, -14.16423886937410082 ) ) ;
#27491 =( NAMED_UNIT ( * ) PLANE_ANGLE_UNIT ( ) SI_UNIT ( $, .RADIAN. ) );
#27493 = CARTESIAN_POINT ( 'NONE',  ( 12.91533473730993009, 66.60535201082150536, -10.88017736071109987 ) ) ;
#27492 = CARTESIAN_POINT ( 'NONE',  ( 20.36894250292379382, 3.678748834913967869, 10.36894250292379205 ) ) ;
#27494 = CARTESIAN_POINT ( 'NONE',  ( 10.00000000000000178, 29.31368534415483751, 10.88017736071110342 ) ) ;
#27495 = CARTESIAN_POINT ( 'NONE',  ( 6.930493939446634499, -71.55570417525920845, -2.750000000000000000 ) ) ;
#27496 = CARTESIAN_POINT ( 'NONE',  ( 14.92337183194729988, 19.34226448433411960, -8.527530157486177487 ) ) ;
#27498 = CARTESIAN_POINT ( 'NONE',  ( 12.63842701281683034, 32.46726448433412315, 9.846743663894596210 ) ) ;
#27497 = CARTESIAN_POINT ( 'NONE',  ( 2.035157376598822676, 57.43868534415484106, -7.964842623401177768 ) ) ;
#27499 = CARTESIAN_POINT ( 'NONE',  ( 20.88017736071110519, 15.56368534415483751, 2.639326808657452039E-16 ) ) ;
#27500 = CARTESIAN_POINT ( 'NONE',  ( 10.00000000000000000, 47.87363466993042493, -12.81628187352647608 ) ) ;
#27501 = CARTESIAN_POINT ( 'NONE',  ( 5.076628168052703671, 51.84226448433412315, 8.527530157486179263 ) ) ;
#27502 = CARTESIAN_POINT ( 'NONE',  ( 13.43411237798106583, 27.66530133659708568, -12.81628187352647252 ) ) ;
#27503 = CARTESIAN_POINT ( 'NONE',  ( -3.795296366450300773, -32.15458449841936073, 14.16423886937410437 ) ) ;
#27504 =( GEOMETRIC_REPRESENTATION_CONTEXT ( 3 ) GLOBAL_UNCERTAINTY_ASSIGNED_CONTEXT ( ( #64176 ) ) GLOBAL_UNIT_ASSIGNED_CONTEXT ( ( #83414, #2402, #17872 ) ) REPRESENTATION_CONTEXT ( 'NONE', 'WORKASPACE' ) );
#27505 = CARTESIAN_POINT ( 'NONE',  ( 12.63842701281683034, 37.46726448433411605, 9.846743663894596210 ) ) ;
#27506 = CARTESIAN_POINT ( 'NONE',  ( 20.36894250292379738, 9.928748834913966093, -10.36894250292379027 ) ) ;
#27507 = ORIENTED_EDGE ( 'NONE', *, *, #83340, .F. ) ;
#27508 = FACE_OUTER_BOUND ( 'NONE', #3137, .T. ) ;
#27509 = CARTESIAN_POINT ( 'NONE',  ( 10.00000000000000178, 54.31368534415484106, 10.88017736071110342 ) ) ;
#27510 = CARTESIAN_POINT ( 'NONE',  ( 7.084665262690076126, 57.02201867748817676, -10.88017736071110164 ) ) ;
#27512 = COLOUR_RGB ( '', 0.09019608, 0.27058824, 0.51372549) ;
#27511 = CARTESIAN_POINT ( 'NONE',  ( -2.266590686148945544, 42.22041550158063217, 7.082119434687048631 ) ) ;
#27513 = CARTESIAN_POINT ( 'NONE',  ( 2.791683348922237240, 50.38393115100078035, -7.208316651077763204 ) ) ;
#27514 = COLOUR_RGB ( '', 0.40784314, 0.44705882, 0.49803922) ;
#27515 = CARTESIAN_POINT ( 'NONE',  ( 14.22901244993681757, 15.00000000000000888, 3.387263120971414576 ) ) ;
#27516 = CARTESIAN_POINT ( 'NONE',  ( -0.8801773607111009756, 43.06368534415484106, 1.068504757029289695E-15 ) ) ;
#27517 = VECTOR ( 'NONE', #12677, 1000.000000000000114 ) ;
#27518 = CARTESIAN_POINT ( 'NONE',  ( -6.742022620658322474, 0.04962897188439633483, 13.12259272460500092 ) ) ;
#27519 = CARTESIAN_POINT ( 'NONE',  ( 1.472469842513823179, 51.42559781766745886, 4.923371831947296329 ) ) ;
#27520 = CARTESIAN_POINT ( 'NONE',  ( 10.88017736071109987, 10.77201867748817321, -2.915334737309928315 ) ) ;
#27521 = CIRCLE ( 'NONE', #92980, 0.2500000000000000000 ) ;
#27522 = CARTESIAN_POINT ( 'NONE',  ( 2.035157376598824452, 68.68868534415484817, 7.964842623401179544 ) ) ;
#27523 = VERTEX_POINT ( 'NONE', #87925 ) ;
#27524 = EDGE_CURVE ( 'NONE', #45856, #13800, #65911, .T. ) ;
#27525 = CARTESIAN_POINT ( 'NONE',  ( 2.035157376598824452, 8.688685344154839285, 7.964842623401179544 ) ) ;
#27526 = CARTESIAN_POINT ( 'NONE',  ( 19.89103541497710737, 65.66234555792573246, -6.479102184480822757 ) ) ;
#27527 = VECTOR ( 'NONE', #33758, 999.9999999999998863 ) ;
#27528 = CARTESIAN_POINT ( 'NONE',  ( 19.42250999205614193, 65.14701867748817676, 5.440088680355555262 ) ) ;
#27529 = CARTESIAN_POINT ( 'NONE',  ( 5.076628168052704559, 5.175597817667451750, -8.527530157486179263 ) ) ;
#27530 = CARTESIAN_POINT ( 'NONE',  ( 0.000000000000000000, 0.5000000000000004441, 0.000000000000000000 ) ) ;
#27531 = CARTESIAN_POINT ( 'NONE',  ( 19.84674366389459621, 33.50893115100078745, 7.409399052514197653E-17 ) ) ;
#27532 = CARTESIAN_POINT ( 'NONE',  ( 17.96484262340118221, 21.18868534415483396, -7.964842623401177768 ) ) ;
#27533 = CARTESIAN_POINT ( 'NONE',  ( 19.38216949554541557, 12.24863466993041961, -9.382169495545420901 ) ) ;
#27535 = CARTESIAN_POINT ( 'NONE',  ( 2.599899806584774264, 0.4361964623231012195, -6.495912400107028084 ) ) ;
#27534 = CARTESIAN_POINT ( 'NONE',  ( 17.96484262340118221, 39.93868534415484106, 7.964842623401181321 ) ) ;
#27536 = CARTESIAN_POINT ( 'NONE',  ( 0.000000000000000000, 14.49999999999999822, 0.000000000000000000 ) ) ;
#27537 = CARTESIAN_POINT ( 'NONE',  ( -1.099225684535947600, 34.54030133659708923, 6.408140936763237150 ) ) ;
#27538 = ORIENTED_EDGE ( 'NONE', *, *, #90990, .T. ) ;
#27539 = CARTESIAN_POINT ( 'NONE',  ( -0.8801773607110991993, 67.85535201082151957, -2.915334737309923874 ) ) ;
#27541 = DIRECTION ( 'NONE',  ( -0.000000000000000000, -0.000000000000000000, -1.000000000000000000 ) ) ;
#27540 = CARTESIAN_POINT ( 'NONE',  ( 22.81628187352647785, 21.41530133659708923, 3.434112377981063169 ) ) ;
#27542 = CARTESIAN_POINT ( 'NONE',  ( 19.42250999205614193, 30.14701867748817321, 5.440088680355555262 ) ) ;
#27543 = CARTESIAN_POINT ( 'NONE',  ( -0.3689425029237898834, 61.17874883491396076, -10.36894250292378850 ) ) ;
#27544 = CARTESIAN_POINT ( 'NONE',  ( 19.84674366389459621, 53.50893115100078745, 7.409399052514197653E-17 ) ) ;
#27545 = CARTESIAN_POINT ( 'NONE',  ( 7.361572987183170547, 2.050597817667451750, 9.846743663894590881 ) ) ;
#27546 = CARTESIAN_POINT ( 'NONE',  ( 4.559911319644449179, 63.89701867748817676, 9.422509992056141925 ) ) ;
#27547 = CARTESIAN_POINT ( 'NONE',  ( 13.61464873478166737, 0.5000000000000004441, -6.296136897217838424 ) ) ;
#27548 = CARTESIAN_POINT ( 'NONE',  ( 10.00000000000000178, 28.05374883491396787, 14.16423886937410082 ) ) ;
#27549 = CARTESIAN_POINT ( 'NONE',  ( 10.35038117927457968, -32.03264712071879927, -3.750000000000000888 ) ) ;
#27550 = CARTESIAN_POINT ( 'NONE',  ( -3.772435417270373570, -6.430908609833668521, -3.750000000000000000 ) ) ;
#27551 = ORIENTED_EDGE ( 'NONE', *, *, #64906, .T. ) ;
#27552 = VERTEX_POINT ( 'NONE', #89899 ) ;
#27553 = AXIS2_PLACEMENT_3D ( 'NONE', #79372, #56860, #49846 ) ;
#27554 = CARTESIAN_POINT ( 'NONE',  ( 2.917880565312948704, 67.63708216824730357, 12.26659068614894643 ) ) ;
#27556 = EDGE_CURVE ( 'NONE', #56519, #70269, #44397, .T. ) ;
#27555 = CARTESIAN_POINT ( 'NONE',  ( -4.164238869374099039, 51.80374883491396787, 8.674139862899312516E-16 ) ) ;
#27557 = CARTESIAN_POINT ( 'NONE',  ( 0.1532563361054082862, 31.21726448433412315, 2.638427012816831674 ) ) ;
#27558 = DIRECTION ( 'NONE',  ( -1.000000000000000000, 0.000000000000000000, 0.000000000000000000 ) ) ;
#27559 = CARTESIAN_POINT ( 'NONE',  ( 0.000000000000000000, 14.49999999999999822, 0.000000000000000000 ) ) ;
#27560 = CARTESIAN_POINT ( 'NONE',  ( -0.8801773607111008646, 68.27201867748817676, 2.915334737309923430 ) ) ;
#27561 = CARTESIAN_POINT ( 'NONE',  ( 6.204703633549690345, 42.84541550158063217, 14.16423886937410082 ) ) ;
#27562 = EDGE_CURVE ( 'NONE', #29895, #76186, #31068, .T. ) ;
#27563 = DIRECTION ( 'NONE',  ( -0.000000000000000000, 0.000000000000000000, 1.000000000000000000 ) ) ;
#27564 = CARTESIAN_POINT ( 'NONE',  ( 17.20831665107776587, 4.133931151000785675, -7.208316651077762316 ) ) ;
#27565 = CARTESIAN_POINT ( 'NONE',  ( -32.19000000000001194, 93.50000000000000000, 9.500000000000000000 ) ) ;
#27566 = CARTESIAN_POINT ( 'NONE',  ( -7.208316651077756099, 1.633931151000786341, 7.208316651077766757 ) ) ;
#27567 = ORIENTED_EDGE ( 'NONE', *, *, #55005, .T. ) ;
#27568 = CARTESIAN_POINT ( 'NONE',  ( -7.771322705631335204, 4.741813304736951008E-16, -12.24159072199927678 ) ) ;
#27569 = VERTEX_POINT ( 'NONE', #95441 ) ;
#27570 = CARTESIAN_POINT ( 'NONE',  ( 13.61464873478173843, 14.49999999999999112, -6.296136897217843753 ) ) ;
#27571 = ORIENTED_EDGE ( 'NONE', *, *, #48371, .T. ) ;
#27573 = CARTESIAN_POINT ( 'NONE',  ( 17.96484262340118221, 19.93868534415484106, 7.964842623401181321 ) ) ;
#27572 = CARTESIAN_POINT ( 'NONE',  ( 15.44008868035555793, 21.39701867748817321, -9.422509992056140149 ) ) ;
#27575 = CARTESIAN_POINT ( 'NONE',  ( 6.565887622018943937, 13.08196800326374998, -12.81628187352647608 ) ) ;
#27574 = CARTESIAN_POINT ( 'NONE',  ( 18.52753015748618282, 48.92559781766745886, -4.923371831947291888 ) ) ;
#27576 = CARTESIAN_POINT ( 'NONE',  ( 12.07856007377822394, 4.551077920620485022E-16, 8.022367888854921247 ) ) ;
#27577 = CARTESIAN_POINT ( 'NONE',  ( 19.84674366389459621, 43.50893115100078745, 7.409399052514197653E-17 ) ) ;
#27578 = AXIS2_PLACEMENT_3D ( 'NONE', #41949, #49419, #65897 ) ;
#27579 = CARTESIAN_POINT ( 'NONE',  ( 10.00000000000000178, 15.37363466993042138, 12.81628187352647608 ) ) ;
#27580 = VERTEX_POINT ( 'NONE', #42442 ) ;
#27581 = CIRCLE ( 'NONE', #22823, 0.2500000000000002220 ) ;
#27582 = CARTESIAN_POINT ( 'NONE',  ( 5.076628168052703671, 36.84226448433412315, 8.527530157486179263 ) ) ;
#27583 = CIRCLE ( 'NONE', #56368, 0.2500000000000002220 ) ;
#27584 = CARTESIAN_POINT ( 'NONE',  ( -2.266590686148945544, 56.38708216824731068, -7.082119434687050408 ) ) ;
#27585 = ORIENTED_EDGE ( 'NONE', *, *, #262, .T. ) ;
#27586 = AXIS2_PLACEMENT_3D ( 'NONE', #31876, #16412, #23918 ) ;
#27587 = CARTESIAN_POINT ( 'NONE',  ( -4.164238869374099927, 67.01208216824728936, 3.795296366450308767 ) ) ;
#27588 = ORIENTED_EDGE ( 'NONE', *, *, #83791, .F. ) ;
#27589 = CARTESIAN_POINT ( 'NONE',  ( -0.8801773607111009756, 48.06368534415484817, 1.068504757029289695E-15 ) ) ;
#27590 = CARTESIAN_POINT ( 'NONE',  ( 10.00000000000000000, 41.81368534415484106, -10.88017736071110342 ) ) ;
#27591 = CARTESIAN_POINT ( 'NONE',  ( 12.91533473730992121, 49.52201867748817676, 10.88017736071110164 ) ) ;
#27592 = AXIS2_PLACEMENT_3D ( 'NONE', #52250, #28754, #66251 ) ;
#27593 = CYLINDRICAL_SURFACE ( 'NONE', #42609, 0.2500000000000002220 ) ;
#27594 = CARTESIAN_POINT ( 'NONE',  ( 10.00000000000000000, 36.81368534415484106, -10.88017736071110342 ) ) ;
#27595 = DIRECTION ( 'NONE',  ( -1.483861936729427615E-16, 1.000000000000000000, 0.000000000000000000 ) ) ;
#27596 = EDGE_CURVE ( 'NONE', #65885, #42615, #72924, .T. ) ;
#27598 = ORIENTED_EDGE ( 'NONE', *, *, #19770, .F. ) ;
#27597 = CARTESIAN_POINT ( 'NONE',  ( 19.72487221294570858, 7.802231764288317883, -6.499999999999999112 ) ) ;
#27599 = CARTESIAN_POINT ( 'NONE',  ( 14.92337183194729988, 24.34226448433411960, -8.527530157486177487 ) ) ;
#27600 = VERTEX_POINT ( 'NONE', #17735 ) ;
#27601 = CARTESIAN_POINT ( 'NONE',  ( 2.791683348922240793, 61.63393115100079456, 7.208316651077764092 ) ) ;
#27602 = DIRECTION ( 'NONE',  ( -1.000000000000000000, 0.000000000000000000, 0.000000000000000000 ) ) ;
#27603 = COLOUR_RGB ( '', 0.31764706, 0.68627451, 0.89019608) ;
#27604 = CARTESIAN_POINT ( 'NONE',  ( -6.982525766139713319, -88.11956320875633253, 3.750000000000000444 ) ) ;
#27605 = CARTESIAN_POINT ( 'NONE',  ( -9.509319644403765537, 13.17686044187662020, 7.198808227794258663 ) ) ;
#27606 = DIRECTION ( 'NONE',  ( -1.000000000000000000, 4.510281037539694659E-14, 0.000000000000000000 ) ) ;
#27607 = CARTESIAN_POINT ( 'NONE',  ( 12.63842701281683922, 64.55059781766745175, -9.846743663894590881 ) ) ;
#27608 = CARTESIAN_POINT ( 'NONE',  ( -2.266590686148945544, 57.22041550158063217, 7.082119434687048631 ) ) ;
#27609 = DIRECTION ( 'NONE',  ( -0.1993679344172108459, -0.000000000000000000, 0.9799247046208268141 ) ) ;
#27610 = VERTEX_POINT ( 'NONE', #98919 ) ;
#27611 = FACE_OUTER_BOUND ( 'NONE', #94102, .T. ) ;
#27612 = CARTESIAN_POINT ( 'NONE',  ( 0.1532563361054083140, 36.00893115100078745, 1.131784320476157264E-15 ) ) ;
#27613 = CARTESIAN_POINT ( 'NONE',  ( -2.816281873526471635, 63.91530133659708923, -3.434112377981056508 ) ) ;
#27614 = CARTESIAN_POINT ( 'NONE',  ( 19.38216949554541557, 2.248634669930420049, -9.382169495545420901 ) ) ;
#27615 = CARTESIAN_POINT ( 'NONE',  ( 12.63842701281683034, 7.467264484334118713, 9.846743663894596210 ) ) ;
#27616 = FILL_AREA_STYLE ('',( #2695 ) ) ;
#27617 = CARTESIAN_POINT ( 'NONE',  ( 5.076628168052703671, 6.842264484334118713, 8.527530157486179263 ) ) ;
#27618 = CARTESIAN_POINT ( 'NONE',  ( 0.1532563361054083140, 56.00893115100078745, 1.131784320476157264E-15 ) ) ;
#27619 = CARTESIAN_POINT ( 'NONE',  ( 20.00000000000000711, 98.59912998021083297, 4.500000000000000888 ) ) ;
#27620 = CIRCLE ( 'NONE', #83529, 18.53834841531100608 ) ;
#27621 = B_SPLINE_CURVE_WITH_KNOTS ( 'NONE', 3,
 ( #90198, #88721, #42252, #49729 ),
 .UNSPECIFIED., .F., .F.,
 ( 4, 4 ),
 ( 0.000000000000000000, 0.002657014572710868390 ),
 .UNSPECIFIED. ) ;
#27622 = VERTEX_POINT ( 'NONE', #9732 ) ;
#27623 = CARTESIAN_POINT ( 'NONE',  ( 0.5774900079438590739, 7.647018677488171434, -5.440088680355550821 ) ) ;
#27624 = CARTESIAN_POINT ( 'NONE',  ( -4.164238869374098151, 11.59541550158063217, -3.795296366450310543 ) ) ;
#27625 = CARTESIAN_POINT ( 'NONE',  ( 19.84674366389459266, 13.71726448433411782, -2.638427012816827677 ) ) ;
#27626 = CARTESIAN_POINT ( 'NONE',  ( 15.44008868035555260, 49.73035201082150536, 9.422509992056143702 ) ) ;
#27628 = DIRECTION ( 'NONE',  ( -0.000000000000000000, -1.000000000000000000, -0.000000000000000000 ) ) ;
#27627 = CARTESIAN_POINT ( 'NONE',  ( -2.816281873526473856, 24.33196800326375353, 3.434112377981055619 ) ) ;
#27629 = CARTESIAN_POINT ( 'NONE',  ( -3.897244926436316703, 15.00000000000000000, 13.96644127841325300 ) ) ;
#27630 = CARTESIAN_POINT ( 'NONE',  ( 17.39651004071838969, 59.08210964143329846, -6.500000000000027534 ) ) ;
#27631 = FILL_AREA_STYLE_COLOUR ( '', #5705 ) ;
#27632 = CARTESIAN_POINT ( 'NONE',  ( 10.00000000000000000, 7.873634669930421381, -12.81628187352647608 ) ) ;
#27633 = CARTESIAN_POINT ( 'NONE',  ( 10.00000000000000000, 59.75893115100078745, -9.846743663894594434 ) ) ;
#27634 = CARTESIAN_POINT ( 'NONE',  ( 7.361572987183169658, 14.96726448433411960, -9.846743663894592657 ) ) ;
#27635 = CARTESIAN_POINT ( 'NONE',  ( -7.964842623401172439, -26.31131465584515539, 7.964842623401183097 ) ) ;
#27636 = CARTESIAN_POINT ( 'NONE',  ( 19.38216949554541202, 15.99863466993042138, 9.382169495545424454 ) ) ;
#27637 = CARTESIAN_POINT ( 'NONE',  ( -11.63911236830571916, -77.84336773400802656, -3.750000000000000000 ) ) ;
#27638 = CARTESIAN_POINT ( 'NONE',  ( 10.00000000000000000, 31.81368534415483751, -10.88017736071110342 ) ) ;
#27639 = FACE_OUTER_BOUND ( 'NONE', #98814, .T. ) ;
#27640 = CARTESIAN_POINT ( 'NONE',  ( 6.204703633549690345, 47.84541550158064638, 14.16423886937410082 ) ) ;
#27641 = EDGE_CURVE ( 'NONE', #5883, #23594, #87840, .T. ) ;
#27642 = SURFACE_SIDE_STYLE ('',( #96158 ) ) ;
#27643 = CARTESIAN_POINT ( 'NONE',  ( 2.035157376598824452, 33.68868534415484106, 7.964842623401179544 ) ) ;
#27644 = CARTESIAN_POINT ( 'NONE',  ( 2.791683348922240793, 56.63393115100078035, 7.208316651077764092 ) ) ;
#27645 = CARTESIAN_POINT ( 'NONE',  ( 2.035157376598822676, 57.43868534415484106, -7.964842623401177768 ) ) ;
#27646 = CARTESIAN_POINT ( 'NONE',  ( 20.36894250292379382, 28.67874883491396787, 10.36894250292379205 ) ) ;
#27647 = CARTESIAN_POINT ( 'NONE',  ( 2.962741594153077251, 0.000000000000000000, -13.93860331045673107 ) ) ;
#27648 = AXIS2_PLACEMENT_3D ( 'NONE', #76674, #15705, #83694 ) ;
#27649 = CARTESIAN_POINT ( 'NONE',  ( 14.92337183194729988, 39.34226448433412315, -8.527530157486177487 ) ) ;
#27650 = CARTESIAN_POINT ( 'NONE',  ( 0.6178305044545818747, 58.49863466993042493, -9.382169495545419124 ) ) ;
#27651 = CARTESIAN_POINT ( 'NONE',  ( 22.81628187352647785, 1.623634669930420271, 6.195893100308588602E-16 ) ) ;
#27652 = VERTEX_POINT ( 'NONE', #70244 ) ;
#27653 = CARTESIAN_POINT ( 'NONE',  ( -0.8801773607111009756, 23.06368534415484106, 1.068504757029289695E-15 ) ) ;
#27654 = STYLED_ITEM ( 'NONE', ( #54570 ), #93062 ) ;
#27655 = FACE_OUTER_BOUND ( 'NONE', #89145, .T. ) ;
#27656 = CARTESIAN_POINT ( 'NONE',  ( 19.42250999205614548, 20.98035201082150891, -5.440088680355545492 ) ) ;
#27657 = CARTESIAN_POINT ( 'NONE',  ( -4.164238869374099927, 27.01208216824730357, 3.795296366450308767 ) ) ;
#27658 = CARTESIAN_POINT ( 'NONE',  ( 18.52753015748617571, 18.09226448433411960, 4.923371831947298993 ) ) ;
#27659 = CARTESIAN_POINT ( 'NONE',  ( 0.1532563361054082862, 61.21726448433412315, 2.638427012816831674 ) ) ;
#27660 = CARTESIAN_POINT ( 'NONE',  ( 4.559911319644449179, 28.89701867748817321, 9.422509992056141925 ) ) ;
#27661 = AXIS2_PLACEMENT_3D ( 'NONE', #59324, #44324, #74825 ) ;
#27662 = CYLINDRICAL_SURFACE ( 'NONE', #71906, 2.999999999999999556 ) ;
#27663 = CARTESIAN_POINT ( 'NONE',  ( -12.80781515976305762, 15.00000000000000000, -6.246788841744501219 ) ) ;
#27664 = ORIENTED_EDGE ( 'NONE', *, *, #72416, .F. ) ;
#27665 = B_SPLINE_CURVE_WITH_KNOTS ( 'NONE', 3,
 ( #59593, #90583, #44596, #90091 ),
 .UNSPECIFIED., .F., .F.,
 ( 4, 4 ),
 ( 0.000000000000000000, 0.002562518741975322069 ),
 .UNSPECIFIED. ) ;
#27666 = CARTESIAN_POINT ( 'NONE',  ( -14.16722289976688565, 15.00000000000000000, 4.928467845925418089 ) ) ;
#27667 = CARTESIAN_POINT ( 'NONE',  ( 5.076628168052703671, 46.84226448433412315, 8.527530157486179263 ) ) ;
#27668 = EDGE_LOOP ( 'NONE', ( #79985, #77231, #79900, #83761, #97327, #30320 ) ) ;
#27669 = ORIENTED_EDGE ( 'NONE', *, *, #70155, .T. ) ;
#27670 = CARTESIAN_POINT ( 'NONE',  ( -14.24131928502211863, 15.00000000000000000, 0.4973178280104966764 ) ) ;
#27671 = CARTESIAN_POINT ( 'NONE',  ( 20.36894250292379382, 3.678748834913967869, 10.36894250292379205 ) ) ;
#27673 = ADVANCED_FACE ( 'NONE', ( #45384 ), #78720, .F. ) ;
#27672 = CARTESIAN_POINT ( 'NONE',  ( 22.26659068614894466, 3.887082168247300906, 7.082119434687054849 ) ) ;
#27674 = CARTESIAN_POINT ( 'NONE',  ( -0.8801773607111008646, 43.27201867748817676, 2.915334737309923430 ) ) ;
#27675 = CARTESIAN_POINT ( 'NONE',  ( 10.00000000000000178, 58.05374883491397497, 14.16423886937410082 ) ) ;
#27676 = CARTESIAN_POINT ( 'NONE',  ( -1.099225684535947600, 3.706968003263753531, -6.408140936763238038 ) ) ;
#27677 = CARTESIAN_POINT ( 'NONE',  ( 18.52753015748617571, 33.09226448433411605, 4.923371831947298993 ) ) ;
#27678 = SURFACE_STYLE_FILL_AREA ( #4709 ) ;
#27680 = CARTESIAN_POINT ( 'NONE',  ( 3.591859063236763294, 8.290301336597087456, -11.09922568453595026 ) ) ;
#27679 = CARTESIAN_POINT ( 'NONE',  ( 15.44008868035555793, 36.39701867748816966, -9.422509992056140149 ) ) ;
#27681 =( LENGTH_UNIT ( ) NAMED_UNIT ( * ) SI_UNIT ( .MILLI., .METRE. ) );
#27682 = CARTESIAN_POINT ( 'NONE',  ( 10.00000000000000000, 55.55374883491396787, -14.16423886937410082 ) ) ;
#27683 = CARTESIAN_POINT ( 'NONE',  ( -0.8801773607110991993, 12.85535201082150358, -2.915334737309923874 ) ) ;
#27684 = CARTESIAN_POINT ( 'NONE',  ( 18.04007052943772749, 38.01528370094808196, 5.767676674365840306 ) ) ;
#27685 = CARTESIAN_POINT ( 'NONE',  ( -32.19000000000001194, 93.50000000000000000, -10.09898361729590199 ) ) ;
#27686 = EDGE_CURVE ( 'NONE', #56421, #4086, #75386, .T. ) ;
#27687 = CARTESIAN_POINT ( 'NONE',  ( 9.846743663894590881, -36.69940218233254114, 2.638427012816828565 ) ) ;
#27688 = ORIENTED_EDGE ( 'NONE', *, *, #70921, .T. ) ;
#27689 = CARTESIAN_POINT ( 'NONE',  ( 20.15039907845753220, 20.60158574516643171, -6.262539305110077947 ) ) ;
#27690 = EDGE_LOOP ( 'NONE', ( #66517, #96293, #87567, #37873 ) ) ;
#27691 = VERTEX_POINT ( 'NONE', #98426 ) ;
#27692 = CARTESIAN_POINT ( 'NONE',  ( 6.204703633549690345, 52.84541550158062506, 14.16423886937410082 ) ) ;
#27693 = CARTESIAN_POINT ( 'NONE',  ( 10.00000000000000000, 49.75893115100078745, -9.846743663894594434 ) ) ;
#27694 = CARTESIAN_POINT ( 'NONE',  ( -0.8801773607111008646, 53.27201867748816966, 2.915334737309923430 ) ) ;
#27695 = MECHANICAL_DESIGN_GEOMETRIC_PRESENTATION_REPRESENTATION (  '', ( #14950 ), #10152 ) ;
#27696 = CARTESIAN_POINT ( 'NONE',  ( 13.78891971893208357, 0.5000000000000004441, -5.904717858191528279 ) ) ;
#27697 = CARTESIAN_POINT ( 'NONE',  ( 19.42250999205614548, 50.98035201082151247, -5.440088680355545492 ) ) ;
#27698 = VECTOR ( 'NONE', #11376, 1000.000000000000000 ) ;
#27699 = CARTESIAN_POINT ( 'NONE',  ( -12.81628187352647252, 4.331968003263747313, 3.434112377981066722 ) ) ;
#27700 = ORIENTED_EDGE ( 'NONE', *, *, #80581, .T. ) ;
#27701 = CARTESIAN_POINT ( 'NONE',  ( 24.16423886937409904, 19.09541550158063927, 3.795296366450317205 ) ) ;
#27702 = CARTESIAN_POINT ( 'NONE',  ( 10.00000000000000178, 30.37363466993042138, 12.81628187352647608 ) ) ;
#27703 = ORIENTED_EDGE ( 'NONE', *, *, #32410, .T. ) ;
#27704 = CARTESIAN_POINT ( 'NONE',  ( 19.38216949554541202, 50.99863466993042493, 9.382169495545424454 ) ) ;
#27705 = EDGE_CURVE ( 'NONE', #78351, #21503, #48968, .T. ) ;
#27706 = CARTESIAN_POINT ( 'NONE',  ( 12.91533473730993009, 21.60535201082150536, -10.88017736071109987 ) ) ;
#27707 = CARTESIAN_POINT ( 'NONE',  ( 14.92337183194729633, 42.67559781766745886, 8.527530157486181039 ) ) ;
#27708 = CARTESIAN_POINT ( 'NONE',  ( 0.5774900079438607392, 8.480352010821505360, 5.440088680355550821 ) ) ;
#27709 = CARTESIAN_POINT ( 'NONE',  ( 13.43411237798105340, 50.58196800326375353, 12.81628187352647963 ) ) ;
#27710 = DIRECTION ( 'NONE',  ( 1.000000000000000000, 0.000000000000000000, 0.000000000000000000 ) ) ;
#27711 = CARTESIAN_POINT ( 'NONE',  ( 18.52753015748617571, 38.09226448433412315, 4.923371831947298993 ) ) ;
#27712 = EDGE_CURVE ( 'NONE', #45908, #15070, #11192, .T. ) ;
#27713 = B_SPLINE_CURVE_WITH_KNOTS ( 'NONE', 3,
 ( #94656, #26165, #56658, #72144, #92685, #54677 ),
 .UNSPECIFIED., .F., .F.,
 ( 4, 2, 4 ),
 ( 3.409110551496208618E-05, 0.0004400426677367994194, 0.0008459942299586367459 ),
 .UNSPECIFIED. ) ;
#27714 = CARTESIAN_POINT ( 'NONE',  ( 12.34086200392821908, 0.000000000000000000, 7.125000000000058620 ) ) ;
#27715 = PRESENTATION_LAYER_ASSIGNMENT (  '', '', ( #96403 ) ) ;
#27716 = CARTESIAN_POINT ( 'NONE',  ( 0.000000000000000000, 14.49999999999999822, 0.000000000000000000 ) ) ;
#27717 = LINE ( 'NONE', #21215, #54748 ) ;
#27718 = CARTESIAN_POINT ( 'NONE',  ( -12.83294900548068895, 0.5000000000000004441, 7.766300266068274283 ) ) ;
#27719 = CARTESIAN_POINT ( 'NONE',  ( 12.63842701281683034, 17.46726448433411250, 9.846743663894596210 ) ) ;
#27720 = CARTESIAN_POINT ( 'NONE',  ( 19.38216949554541557, 22.24863466993041428, -9.382169495545420901 ) ) ;
#27721 = DIRECTION ( 'NONE',  ( -0.000000000000000000, -0.000000000000000000, -1.000000000000000000 ) ) ;
#27722 = EDGE_LOOP ( 'NONE', ( #11217, #26349, #6161, #78355, #21378 ) ) ;
#27723 = CARTESIAN_POINT ( 'NONE',  ( 14.92337183194729633, 57.67559781766745886, 8.527530157486181039 ) ) ;
#27724 = FACE_OUTER_BOUND ( 'NONE', #15768, .T. ) ;
#27725 = CARTESIAN_POINT ( 'NONE',  ( -0.3689425029237881626, 22.42874883491397142, 10.36894250292379027 ) ) ;
#27726 = CARTESIAN_POINT ( 'NONE',  ( 18.52753015748618282, 38.92559781766745175, -4.923371831947291888 ) ) ;
#27727 = CARTESIAN_POINT ( 'NONE',  ( -2.816281873526473856, 44.33196800326375353, 3.434112377981055619 ) ) ;
#27728 = DIRECTION ( 'NONE',  ( -0.8433914458128884961, 0.000000000000000000, 0.5372996083468194461 ) ) ;
#27729 = CARTESIAN_POINT ( 'NONE',  ( 2.035157376598824452, 58.68868534415482685, 7.964842623401179544 ) ) ;
#27730 = CARTESIAN_POINT ( 'NONE',  ( 3.591859063236761518, 14.95696800326375531, 11.09922568453594849 ) ) ;
#27731 = DIRECTION ( 'NONE',  ( 0.000000000000000000, 1.000000000000000000, 0.000000000000000000 ) ) ;
#27732 = CARTESIAN_POINT ( 'NONE',  ( 5.076628168052703671, 36.84226448433412315, 8.527530157486179263 ) ) ;
#27733 = CARTESIAN_POINT ( 'NONE',  ( 2.035157376598822676, 42.43868534415483396, -7.964842623401177768 ) ) ;
#27734 = CARTESIAN_POINT ( 'NONE',  ( 13.43411237798106583, 42.66530133659707502, -12.81628187352647252 ) ) ;
#27735 = CARTESIAN_POINT ( 'NONE',  ( 14.92337183194729633, 37.67559781766745175, 8.527530157486181039 ) ) ;
#27736 =( LENGTH_UNIT ( ) NAMED_UNIT ( * ) SI_UNIT ( .MILLI., .METRE. ) );
#27737 = FACE_OUTER_BOUND ( 'NONE', #86153, .T. ) ;
#27738 = CARTESIAN_POINT ( 'NONE',  ( 17.96484262340118221, 29.93868534415484106, 7.964842623401181321 ) ) ;
#27739 = CARTESIAN_POINT ( 'NONE',  ( -3.014428414850141458, 4.076366962315985276, -11.25000000000000000 ) ) ;
#27740 = CARTESIAN_POINT ( 'NONE',  ( 19.42250999205614548, 5.980352010821504471, -5.440088680355545492 ) ) ;
#27742 = CARTESIAN_POINT ( 'NONE',  ( 7.084665262690076126, 34.10535201082151247, 10.88017736071109987 ) ) ;
#27741 = CARTESIAN_POINT ( 'NONE',  ( 0.1532563361054100626, 50.80059781766745175, -2.638427012816831230 ) ) ;
#27743 = CARTESIAN_POINT ( 'NONE',  ( -39.69000000000001194, 92.00000000000000000, -10.09898361729590199 ) ) ;
#27744 = CARTESIAN_POINT ( 'NONE',  ( -0.8801773607111008646, 58.27201867748816966, 2.915334737309923430 ) ) ;
#27746 = CARTESIAN_POINT ( 'NONE',  ( 0.000000000000000000, 78.20247855283322735, -8.810553791401492418 ) ) ;
#27745 = CARTESIAN_POINT ( 'NONE',  ( 12.91533473730993009, 26.60535201082150536, -10.88017736071109987 ) ) ;
#27747 =( LENGTH_UNIT ( ) NAMED_UNIT ( * ) SI_UNIT ( .MILLI., .METRE. ) );
#27748 = CARTESIAN_POINT ( 'NONE',  ( 5.076628168052703671, 26.84226448433411960, 8.527530157486179263 ) ) ;
#27749 = LINE ( 'NONE', #88255, #58540 ) ;
#27750 = CARTESIAN_POINT ( 'NONE',  ( 12.63842701281683034, 47.46726448433412315, 9.846743663894596210 ) ) ;
#27752 = CARTESIAN_POINT ( 'NONE',  ( 4.573290919439518376, -6.402485759401510101, 3.750000000000000444 ) ) ;
#27751 = CARTESIAN_POINT ( 'NONE',  ( 24.16423886937410614, 59.30374883491397497, 8.672049930838204340E-16 ) ) ;
#27753 =( LENGTH_UNIT ( ) NAMED_UNIT ( * ) SI_UNIT ( .MILLI., .METRE. ) );
#27754 = CARTESIAN_POINT ( 'NONE',  ( 24.16423886937410614, 4.512082168247300906, -3.795296366450302550 ) ) ;
#27755 = ADVANCED_FACE ( 'NONE', ( #45897 ), #93712, .F. ) ;
#27756 = CARTESIAN_POINT ( 'NONE',  ( 13.79529636645030344, 33.26208216824730357, 14.16423886937410614 ) ) ;
#27757 = CARTESIAN_POINT ( 'NONE',  ( -2.816281873526473856, 4.331968003263754419, 3.434112377981055619 ) ) ;
#27758 = CARTESIAN_POINT ( 'NONE',  ( -6.867514901617631118, -58.37540207706140194, 2.749999999999999556 ) ) ;
#27759 = VERTEX_POINT ( 'NONE', #93216 ) ;
#27760 = CARTESIAN_POINT ( 'NONE',  ( 20.88017736071110875, 10.77201867748817143, -2.915334737309920765 ) ) ;
#27761 = EDGE_CURVE ( 'NONE', #74710, #63139, #66848, .T. ) ;
#27762 = CARTESIAN_POINT ( 'NONE',  ( 0.1532563361054100626, 40.80059781766745886, -2.638427012816831230 ) ) ;
#27764 = CARTESIAN_POINT ( 'NONE',  ( -12.29167862325965821, 90.46743899975646741, -7.079701151216127641 ) ) ;
#27763 = DIRECTION ( 'NONE',  ( -1.000000000000000000, 0.000000000000000000, 0.000000000000000000 ) ) ;
#27765 = CARTESIAN_POINT ( 'NONE',  ( 0.5774900079438607392, 53.48035201082151247, 5.440088680355550821 ) ) ;
#27766 = DIRECTION ( 'NONE',  ( 0.000000000000000000, 0.000000000000000000, -1.000000000000000000 ) ) ;
#27767 = CARTESIAN_POINT ( 'NONE',  ( 3.591859063236763294, 63.29030133659708923, -11.09922568453595026 ) ) ;
#27768 = CARTESIAN_POINT ( 'NONE',  ( 10.00000000000000178, 30.37363466993042138, 12.81628187352647608 ) ) ;
#27769 = CARTESIAN_POINT ( 'NONE',  ( 10.00000000000000000, 34.75893115100078745, -9.846743663894594434 ) ) ;
#27770 = ORIENTED_EDGE ( 'NONE', *, *, #34348, .F. ) ;
#27771 = DIRECTION ( 'NONE',  ( 1.000000000000000000, 0.000000000000000000, 0.000000000000000000 ) ) ;
#27772 = DIRECTION ( 'NONE',  ( 1.927470528863119542E-16, -1.000000000000000000, -0.000000000000000000 ) ) ;
#27773 = CARTESIAN_POINT ( 'NONE',  ( 0.5774900079438607392, 3.480352010821504916, 5.440088680355550821 ) ) ;
#27774 = CARTESIAN_POINT ( 'NONE',  ( 7.084665262690076126, 9.105352010821503583, 10.88017736071109987 ) ) ;
#27775 = CARTESIAN_POINT ( 'NONE',  ( -0.3689425029237881626, 47.42874883491396787, 10.36894250292379027 ) ) ;
#27776 = CARTESIAN_POINT ( 'NONE',  ( 4.559911319644449179, 28.89701867748817321, 9.422509992056141925 ) ) ;
#27777 = CARTESIAN_POINT ( 'NONE',  ( 0.5774900079438590739, 57.64701867748817676, -5.440088680355550821 ) ) ;
#27778 = CARTESIAN_POINT ( 'NONE',  ( -0.8653096853310142667, 14.99999999999806377, -14.59999144043309016 ) ) ;
#27779 = CARTESIAN_POINT ( 'NONE',  ( -6.382347221874512755, 15.00000000000000000, 13.57444820018223375 ) ) ;
#27780 = CARTESIAN_POINT ( 'NONE',  ( 2.791683348922237240, 20.38393115100078745, -7.208316651077763204 ) ) ;
#27781 = LINE ( 'NONE', #95805, #27415 ) ;
#27782 = CARTESIAN_POINT ( 'NONE',  ( 5.076628168052704559, 5.175597817667451750, -8.527530157486179263 ) ) ;
#27783 = CARTESIAN_POINT ( 'NONE',  ( 5.076628168052704559, 40.17559781766745175, -8.527530157486179263 ) ) ;
#27784 = CARTESIAN_POINT ( 'NONE',  ( 10.00000000000000178, 0.3736346699304200492, 12.81628187352647608 ) ) ;
#27785 = CARTESIAN_POINT ( 'NONE',  ( 10.00000000000000000, 41.81368534415484106, -10.88017736071110342 ) ) ;
#27786 = VERTEX_POINT ( 'NONE', #83886 ) ;
#27787 = CARTESIAN_POINT ( 'NONE',  ( -2.816281873526473856, 44.33196800326375353, 3.434112377981055619 ) ) ;
#27789 = EDGE_CURVE ( 'NONE', #75926, #89237, #78220, .T. ) ;
#27788 = DIRECTION ( 'NONE',  ( 0.8320502943378436100, -0.5547001962252291474, 0.000000000000000000 ) ) ;
#27790 = VECTOR ( 'NONE', #1760, 1000.000000000000000 ) ;
#27791 = CARTESIAN_POINT ( 'NONE',  ( 2.035157376598822676, 62.43868534415483396, -7.964842623401177768 ) ) ;
#27792 = CARTESIAN_POINT ( 'NONE',  ( 6.565887622018943937, 48.08196800326375353, -12.81628187352647608 ) ) ;
#27794 = CARTESIAN_POINT ( 'NONE',  ( 7.361572987183169658, 39.96726448433411605, -9.846743663894592657 ) ) ;
#27793 = CARTESIAN_POINT ( 'NONE',  ( 24.16423886937410614, 59.30374883491397497, 8.672049930838204340E-16 ) ) ;
#27795 = CARTESIAN_POINT ( 'NONE',  ( -7.684764310694707667, 0.5000000000000004441, -12.88194075009945472 ) ) ;
#27796 = CARTESIAN_POINT ( 'NONE',  ( -12.60589901313227124, 15.00000000000000000, 8.129656208641961257 ) ) ;
#27797 = CARTESIAN_POINT ( 'NONE',  ( 24.16423886937410614, 34.30374883491396787, 8.672049930838204340E-16 ) ) ;
#27798 = CARTESIAN_POINT ( 'NONE',  ( 5.076628168052704559, 45.17559781766745175, -8.527530157486179263 ) ) ;
#27799 = CARTESIAN_POINT ( 'NONE',  ( 18.00000000000000000, 78.80384757729336798, 3.750000000000000000 ) ) ;
#27800 = CARTESIAN_POINT ( 'NONE',  ( -0.8801773607110991993, 32.85535201082151247, -2.915334737309923874 ) ) ;
#27801 = EDGE_CURVE ( 'NONE', #89795, #87207, #55218, .T. ) ;
#27802 = AXIS2_PLACEMENT_3D ( 'NONE', #89619, #50635, #89124 ) ;
#27803 = CARTESIAN_POINT ( 'NONE',  ( 4.559911319644449179, 53.89701867748817676, 9.422509992056141925 ) ) ;
#27804 = CYLINDRICAL_SURFACE ( 'NONE', #62113, 0.2500000000000002220 ) ;
#27805 = ORIENTED_EDGE ( 'NONE', *, *, #44993, .T. ) ;
#27806 = CARTESIAN_POINT ( 'NONE',  ( 22.81628187352647785, 41.62363466993042493, 6.195893100308588602E-16 ) ) ;
#27807 = ORIENTED_EDGE ( 'NONE', *, *, #40035, .F. ) ;
#27808 = CARTESIAN_POINT ( 'NONE',  ( 10.00000000000000178, 64.31368534415483396, 10.88017736071110342 ) ) ;
#27809 = VERTEX_POINT ( 'NONE', #40231 ) ;
#27810 = CARTESIAN_POINT ( 'NONE',  ( -4.164238869374098151, 1.595415501580634388, -3.795296366450310543 ) ) ;
#27811 = LINE ( 'NONE', #78852, #64900 ) ;
#27812 = DIRECTION ( 'NONE',  ( -0.000000000000000000, -1.000000000000000000, -0.000000000000000000 ) ) ;
#27813 = ORIENTED_EDGE ( 'NONE', *, *, #33783, .T. ) ;
#27814 = CYLINDRICAL_SURFACE ( 'NONE', #25402, 0.2500000000000002220 ) ;
#27815 = CARTESIAN_POINT ( 'NONE',  ( -0.8801773607110991993, 17.85535201082150536, -2.915334737309923874 ) ) ;
#27816 = CARTESIAN_POINT ( 'NONE',  ( 20.88017736071110164, 60.35535201082150536, 2.915334737309930979 ) ) ;
#27817 = CARTESIAN_POINT ( 'NONE',  ( -4.164238869374099927, 22.01208216824730357, 3.795296366450308767 ) ) ;
#27818 = CARTESIAN_POINT ( 'NONE',  ( -0.8801773607110991993, 17.85535201082150536, -2.915334737309923874 ) ) ;
#27819 = CARTESIAN_POINT ( 'NONE',  ( 19.84674366389459621, 63.50893115100078745, 7.409399052514197653E-17 ) ) ;
#27820 = EDGE_LOOP ( 'NONE', ( #66502, #96209, #91892, #68307 ) ) ;
#27821 = CARTESIAN_POINT ( 'NONE',  ( 14.92337183194729633, 57.67559781766745886, 8.527530157486181039 ) ) ;
#27822 = EDGE_LOOP ( 'NONE', ( #67173, #44455, #28322, #83049 ) ) ;
#27823 = CARTESIAN_POINT ( 'NONE',  ( 15.44008868035555260, 54.73035201082150536, 9.422509992056143702 ) ) ;
#27824 = DIRECTION ( 'NONE',  ( 0.7604059656000297096, -0.000000000000000000, 0.6494480483301851015 ) ) ;
#27825 = CARTESIAN_POINT ( 'NONE',  ( 19.38216949554541557, 37.24863466993041783, -9.382169495545420901 ) ) ;
#27827 = CARTESIAN_POINT ( 'NONE',  ( 34.56412365047464874, 11.99999999999999645, 9.500000000000000000 ) ) ;
#27826 = CARTESIAN_POINT ( 'NONE',  ( 20.88017736071110875, 10.77201867748817143, -2.915334737309920765 ) ) ;
#27828 = CARTESIAN_POINT ( 'NONE',  ( 10.00000000000000000, -0.2410688489992152128, -9.846743663894594434 ) ) ;
#27829 = CARTESIAN_POINT ( 'NONE',  ( 15.44008868035555793, 16.39701867748817321, -9.422509992056140149 ) ) ;
#27830 = VECTOR ( 'NONE', #4820, 1000.000000000000114 ) ;
#27831 = EDGE_CURVE ( 'NONE', #27552, #94563, #54293, .T. ) ;
#27832 = ORIENTED_EDGE ( 'NONE', *, *, #50458, .T. ) ;
#27833 = CARTESIAN_POINT ( 'NONE',  ( 6.565887622018943937, 60.16530133659707502, 12.81628187352647430 ) ) ;
#27834 = CARTESIAN_POINT ( 'NONE',  ( 20.88017736071110875, 25.77201867748816966, -2.915334737309920765 ) ) ;
#27835 = CARTESIAN_POINT ( 'NONE',  ( -46.94000000000001194, 102.4632489371167452, -6.394394627233738859 ) ) ;
#27836 = CARTESIAN_POINT ( 'NONE',  ( 16.40814093676324603, 37.45696800326376064, -11.09922568453594671 ) ) ;
#27837 = CARTESIAN_POINT ( 'NONE',  ( -0.8801773607110991993, 47.85535201082150536, -2.915334737309923874 ) ) ;
#27838 = EDGE_LOOP ( 'NONE', ( #51547, #35114, #65796, #8071 ) ) ;
#27839 = CARTESIAN_POINT ( 'NONE',  ( -0.1503990784575242878, 49.24884699246889141, -6.262539305110083276 ) ) ;
#27840 = CARTESIAN_POINT ( 'NONE',  ( 14.92337183194729988, 9.342264484334119601, -8.527530157486177487 ) ) ;
#27841 = CARTESIAN_POINT ( 'NONE',  ( 13.43411237798105340, 0.5819680032637533085, 12.81628187352647963 ) ) ;
#27843 = CARTESIAN_POINT ( 'NONE',  ( 17.20831665107776587, 49.13393115100078745, -7.208316651077762316 ) ) ;
#27842 = CARTESIAN_POINT ( 'NONE',  ( -13.79715839871649763, 90.89647188945875200, -7.777600768747879201 ) ) ;
#27844 = CARTESIAN_POINT ( 'NONE',  ( 19.42250999205614548, 25.98035201082150891, -5.440088680355545492 ) ) ;
#27845 = CARTESIAN_POINT ( 'NONE',  ( 19.84674366389459266, 53.71726448433411605, -2.638427012816827677 ) ) ;
#27846 = CARTESIAN_POINT ( 'NONE',  ( -3.750000000000000000, 36.75000000000000000, 2.500000000000000000 ) ) ;
#27847 = DIRECTION ( 'NONE',  ( 0.000000000000000000, 0.000000000000000000, -1.000000000000000000 ) ) ;
#27848 = CARTESIAN_POINT ( 'NONE',  ( 0.1532563361054100626, 5.800597817667452638, -2.638427012816831230 ) ) ;
#27850 = ORIENTED_EDGE ( 'NONE', *, *, #3759, .T. ) ;
#27849 = CARTESIAN_POINT ( 'NONE',  ( 0.1532563361054082862, 56.21726448433411605, 2.638427012816831674 ) ) ;
#27851 = CARTESIAN_POINT ( 'NONE',  ( 0.000000000000000000, 15.00000000000000000, 0.000000000000000000 ) ) ;
#27852 = CARTESIAN_POINT ( 'NONE',  ( 13.43411237798106583, 32.66530133659708213, -12.81628187352647252 ) ) ;
#27853 = CARTESIAN_POINT ( 'NONE',  ( 19.84674366389459266, 33.71726448433410894, -2.638427012816827677 ) ) ;
#27854 = AXIS2_PLACEMENT_3D ( 'NONE', #82959, #14474, #88481 ) ;
#27855 = CARTESIAN_POINT ( 'NONE',  ( 0.5774900079438607392, 58.48035201082151247, 5.440088680355550821 ) ) ;
#27856 = CARTESIAN_POINT ( 'NONE',  ( 13.79529636645031943, 60.34541550158063927, -14.16423886937409904 ) ) ;
#27857 = CARTESIAN_POINT ( 'NONE',  ( 19.84674366389459621, 28.50893115100078745, 7.409399052514197653E-17 ) ) ;
#27858 = B_SPLINE_CURVE_WITH_KNOTS ( 'NONE', 3,
 ( #35776, #13273, #30109, #60615, #42796, #96800 ),
 .UNSPECIFIED., .F., .F.,
 ( 4, 2, 4 ),
 ( 0.0002800065468393074129, 0.0006862118402932828112, 0.001092417133747258318 ),
 .UNSPECIFIED. ) ;
#27859 =( GEOMETRIC_REPRESENTATION_CONTEXT ( 3 ) GLOBAL_UNCERTAINTY_ASSIGNED_CONTEXT ( ( #3533 ) ) GLOBAL_UNIT_ASSIGNED_CONTEXT ( ( #4520, #27491, #20495 ) ) REPRESENTATION_CONTEXT ( 'NONE', 'WORKASPACE' ) );
#27860 = CARTESIAN_POINT ( 'NONE',  ( -0.1503990784575247319, 47.22266099184918886, -6.262539305110083276 ) ) ;
#27861 = AXIS2_PLACEMENT_3D ( 'NONE', #64521, #95027, #26536 ) ;
#27862 = CARTESIAN_POINT ( 'NONE',  ( -2.266590686148945544, 51.38708216824730357, -7.082119434687050408 ) ) ;
#27863 = CARTESIAN_POINT ( 'NONE',  ( 7.684764310694887079, 0.3639308364404311713, -12.88194075009938899 ) ) ;
#27864 = CARTESIAN_POINT ( 'NONE',  ( 20.88017736071110519, 15.56368534415483751, 2.639326808657452039E-16 ) ) ;
#27865 = CARTESIAN_POINT ( 'NONE',  ( -4.164238869374099927, 37.01208216824731068, 3.795296366450308767 ) ) ;
#27867 = DIRECTION ( 'NONE',  ( -0.000000000000000000, -1.000000000000000000, -0.000000000000000000 ) ) ;
#27866 = CARTESIAN_POINT ( 'NONE',  ( 13.79529636645031943, 55.34541550158062506, -14.16423886937409904 ) ) ;
#27868 = CARTESIAN_POINT ( 'NONE',  ( -45.94000000000000483, 92.50000000000000000, -9.500000000000000000 ) ) ;
#27869 = AXIS2_PLACEMENT_3D ( 'NONE', #67342, #23836, #37850 ) ;
#27870 = CARTESIAN_POINT ( 'NONE',  ( 0.1532563361054083140, 6.008931151000784787, 1.131784320476157264E-15 ) ) ;
#27871 = CARTESIAN_POINT ( 'NONE',  ( 10.00000000000000000, 2.873634669930420049, -12.81628187352647608 ) ) ;
#27872 = CARTESIAN_POINT ( 'NONE',  ( 18.50749283717776805, 14.69955587570481192, 6.500000000000000888 ) ) ;
#27873 = CARTESIAN_POINT ( 'NONE',  ( -0.8801773607111008646, 53.27201867748816966, 2.915334737309923430 ) ) ;
#27874 = SURFACE_STYLE_USAGE ( .BOTH. , #20880 ) ;
#27875 = CARTESIAN_POINT ( 'NONE',  ( 18.52753015748618282, 48.92559781766745886, -4.923371831947291888 ) ) ;
#27876 = DIRECTION ( 'NONE',  ( 1.000000000000000000, -0.000000000000000000, -0.000000000000000000 ) ) ;
#27877 = FACE_OUTER_BOUND ( 'NONE', #24653, .T. ) ;
#27878 = CARTESIAN_POINT ( 'NONE',  ( 14.99847009497950800, 14.49999999999999112, -0.2142307401080081053 ) ) ;
#27879 = CARTESIAN_POINT ( 'NONE',  ( 6.204703633549690345, 45.76208216824729647, -14.16423886937410259 ) ) ;
#27880 = EDGE_CURVE ( 'NONE', #76346, #51781, #17247, .T. ) ;
#27881 = EDGE_CURVE ( 'NONE', #86629, #5244, #58860, .T. ) ;
#27883 = DIRECTION ( 'NONE',  ( 0.000000000000000000, 1.000000000000000000, -0.000000000000000000 ) ) ;
#27882 = CARTESIAN_POINT ( 'NONE',  ( 0.000000000000000000, 0.5000000000000004441, 0.000000000000000000 ) ) ;
#27884 = CARTESIAN_POINT ( 'NONE',  ( -0.8801773607110991993, 17.85535201082150536, -2.915334737309923874 ) ) ;
#27885 = CARTESIAN_POINT ( 'NONE',  ( 22.81628187352647785, 41.62363466993042493, 6.195893100308588602E-16 ) ) ;
#27886 = LINE ( 'NONE', #26410, #22518 ) ;
#27887 = CARTESIAN_POINT ( 'NONE',  ( 22.81628187352647785, 21.41530133659708923, 3.434112377981063169 ) ) ;
#27888 = CARTESIAN_POINT ( 'NONE',  ( 19.38216949554541557, 62.24863466993041072, -9.382169495545420901 ) ) ;
#27889 = ORIENTED_EDGE ( 'NONE', *, *, #87102, .T. ) ;
#27890 = CARTESIAN_POINT ( 'NONE',  ( 6.935087012919454175, -80.58470470491536730, -4.000000000001609379 ) ) ;
#27891 = LINE ( 'NONE', #58887, #86169 ) ;
#27892 = CARTESIAN_POINT ( 'NONE',  ( -0.3689425029237898834, 1.178748834913967869, -10.36894250292378850 ) ) ;
#27893 = CARTESIAN_POINT ( 'NONE',  ( -4.511864039100093926, -13.83704418182128038, 3.999999999999999112 ) ) ;
#27894 = CARTESIAN_POINT ( 'NONE',  ( 0.5774900079438607392, 23.48035201082150536, 5.440088680355550821 ) ) ;
#27895 = CARTESIAN_POINT ( 'NONE',  ( 0.000000000000000000, 14.49999999999999822, 0.000000000000000000 ) ) ;
#27896 = DIRECTION ( 'NONE',  ( -0.000000000000000000, -1.000000000000000000, -0.000000000000000000 ) ) ;
#27897 = CARTESIAN_POINT ( 'NONE',  ( 12.91533473730993009, 36.60535201082151247, -10.88017736071109987 ) ) ;
#27898 = CARTESIAN_POINT ( 'NONE',  ( 19.42250999205614193, 50.14701867748817676, 5.440088680355555262 ) ) ;
#27899 = CARTESIAN_POINT ( 'NONE',  ( -1.099225684535947600, 8.706968003263753531, -6.408140936763238038 ) ) ;
#27900 = CARTESIAN_POINT ( 'NONE',  ( -0.1042174387088625198, 48.10736173766201773, 6.337391062633416894 ) ) ;
#27901 = PLANE ( 'NONE',  #27578 ) ;
#27902 = CARTESIAN_POINT ( 'NONE',  ( 10.00000000000000000, 29.75893115100078745, -9.846743663894594434 ) ) ;
#27903 = CIRCLE ( 'NONE', #61445, 14.49999999999999822 ) ;
#27904 = CARTESIAN_POINT ( 'NONE',  ( 0.5774900079438590739, 42.64701867748816966, -5.440088680355550821 ) ) ;
#27905 = CARTESIAN_POINT ( 'NONE',  ( -2.816281873526473856, 9.123634669930421381, 9.499525473075851096E-16 ) ) ;
#27906 = CARTESIAN_POINT ( 'NONE',  ( 2.791683348922237240, 20.38393115100078745, -7.208316651077763204 ) ) ;
#27907 = CARTESIAN_POINT ( 'NONE',  ( 6.565887622018943937, 53.08196800326374643, -12.81628187352647608 ) ) ;
#27908 = CARTESIAN_POINT ( 'NONE',  ( 7.361572987183169658, 9.967264484334119601, -9.846743663894592657 ) ) ;
#27909 = ORIENTED_EDGE ( 'NONE', *, *, #50128, .T. ) ;
#27910 = DIRECTION ( 'NONE',  ( 0.000000000000000000, 1.000000000000000000, 0.000000000000000000 ) ) ;
#27911 = PLANE ( 'NONE',  #67015 ) ;
#27912 = CARTESIAN_POINT ( 'NONE',  ( 2.035157376598822676, 17.43868534415483751, -7.964842623401177768 ) ) ;
#27914 = CARTESIAN_POINT ( 'NONE',  ( 10.00000000000000178, 28.05374883491396787, 14.16423886937410082 ) ) ;
#27913 = CARTESIAN_POINT ( 'NONE',  ( 20.15039907845753930, 70.00000000000000000, 6.262539305110068177 ) ) ;
#27915 = EDGE_CURVE ( 'NONE', #74651, #89307, #22416, .T. ) ;
#27916 = CARTESIAN_POINT ( 'NONE',  ( 14.92337183194729988, 24.34226448433411960, -8.527530157486177487 ) ) ;
#27917 = CARTESIAN_POINT ( 'NONE',  ( 0.5774900079438590739, 17.64701867748817321, -5.440088680355550821 ) ) ;
#27918 = CARTESIAN_POINT ( 'NONE',  ( 10.00000000000000178, 68.05374883491397497, 14.16423886937410082 ) ) ;
#27919 = ORIENTED_EDGE ( 'NONE', *, *, #95494, .T. ) ;
#27920 = VECTOR ( 'NONE', #9456, 1000.000000000000000 ) ;
#27921 = CARTESIAN_POINT ( 'NONE',  ( 19.42250999205614193, 10.14701867748816966, 5.440088680355555262 ) ) ;
#27922 = CARTESIAN_POINT ( 'NONE',  ( 20.88017736071110519, 40.56368534415484106, 2.639326808657452039E-16 ) ) ;
#27924 = CARTESIAN_POINT ( 'NONE',  ( 19.42250999205614548, 35.98035201082151247, -5.440088680355545492 ) ) ;
#27923 = CARTESIAN_POINT ( 'NONE',  ( -12.22474924877131031, 14.76984934309701636, -8.589397507025012146 ) ) ;
#27925 = ORIENTED_EDGE ( 'NONE', *, *, #41663, .F. ) ;
#27926 = CARTESIAN_POINT ( 'NONE',  ( 7.361572987183170547, 67.05059781766746596, 9.846743663894590881 ) ) ;
#27927 = CARTESIAN_POINT ( 'NONE',  ( 10.00000000000000000, 31.81368534415483751, -10.88017736071110342 ) ) ;
#27928 = CARTESIAN_POINT ( 'NONE',  ( 0.000000000000000000, 0.000000000000000000, 0.000000000000000000 ) ) ;
#27929 = CARTESIAN_POINT ( 'NONE',  ( 19.38216949554541557, 62.24863466993041072, -9.382169495545420901 ) ) ;
#27930 = LINE ( 'NONE', #96960, #87590 ) ;
#27932 = CARTESIAN_POINT ( 'NONE',  ( 13.79529636645030344, 38.26208216824729647, 14.16423886937410614 ) ) ;
#27931 = AXIS2_PLACEMENT_3D ( 'NONE', #67341, #59335, #50356 ) ;
#27933 = CARTESIAN_POINT ( 'NONE',  ( 19.42250999205614193, 50.14701867748817676, 5.440088680355555262 ) ) ;
#27934 = CARTESIAN_POINT ( 'NONE',  ( 4.559911319644449179, 27.23035201082150536, -9.422509992056141925 ) ) ;
#27935 = CARTESIAN_POINT ( 'NONE',  ( 19.72487221294571569, 42.80223176428830811, -6.499999999999990230 ) ) ;
#27936 = AXIS2_PLACEMENT_3D ( 'NONE', #98854, #30308, #52818 ) ;
#27937 = DIRECTION ( 'NONE',  ( 0.7604059656000297096, 0.000000000000000000, 0.6494480483301851015 ) ) ;
#27938 = CARTESIAN_POINT ( 'NONE',  ( 5.076628168052704559, 50.17559781766745886, -8.527530157486179263 ) ) ;
#27939 = ORIENTED_EDGE ( 'NONE', *, *, #1615, .F. ) ;
#27940 = FACE_OUTER_BOUND ( 'NONE', #25540, .T. ) ;
#27941 = CARTESIAN_POINT ( 'NONE',  ( 5.076628168052703671, 16.84226448433411960, 8.527530157486179263 ) ) ;
#27942 = CARTESIAN_POINT ( 'NONE',  ( 11.09922568453595026, -13.79303199673624647, 6.408140936763232709 ) ) ;
#27943 = CARTESIAN_POINT ( 'NONE',  ( 10.00000000000000178, 19.31368534415484106, 10.88017736071110342 ) ) ;
#27944 = CARTESIAN_POINT ( 'NONE',  ( 1.472469842513823179, 21.42559781766745175, 4.923371831947296329 ) ) ;
#27945 = CARTESIAN_POINT ( 'NONE',  ( -2.816281873526473856, 9.123634669930421381, 9.499525473075851096E-16 ) ) ;
#27947 = CARTESIAN_POINT ( 'NONE',  ( 17.96484262340118221, 49.93868534415484106, 7.964842623401181321 ) ) ;
#27946 = CARTESIAN_POINT ( 'NONE',  ( 2.035157376598824452, 63.68868534415484106, 7.964842623401179544 ) ) ;
#27949 = CARTESIAN_POINT ( 'NONE',  ( 22.81628187352647785, 56.41530133659708213, 3.434112377981063169 ) ) ;
#27948 = CARTESIAN_POINT ( 'NONE',  ( 10.00000000000000178, 14.31368534415483751, 10.88017736071110342 ) ) ;
#27950 = CARTESIAN_POINT ( 'NONE',  ( 10.00000000000000000, 45.55374883491397497, -14.16423886937410082 ) ) ;
#27951 = VECTOR ( 'NONE', #19491, 1000.000000000000000 ) ;
#27952 = DIRECTION ( 'NONE',  ( -0.000000000000000000, -1.000000000000000000, -0.000000000000000000 ) ) ;
#27953 = ORIENTED_EDGE ( 'NONE', *, *, #90389, .T. ) ;
#27954 = CARTESIAN_POINT ( 'NONE',  ( 22.81628187352647785, 1.415301336597087012, 3.434112377981063169 ) ) ;
#27955 = CARTESIAN_POINT ( 'NONE',  ( 4.559911319644449179, 13.89701867748817143, 9.422509992056141925 ) ) ;
#27956 = CARTESIAN_POINT ( 'NONE',  ( 12.91533473730992121, 29.52201867748817321, 10.88017736071110164 ) ) ;
#27957 = CARTESIAN_POINT ( 'NONE',  ( 1.472469842513823179, 60.59226448433412315, -4.923371831947296329 ) ) ;
#27958 = ORIENTED_EDGE ( 'NONE', *, *, #30452, .F. ) ;
#27959 = CARTESIAN_POINT ( 'NONE',  ( 5.076628168052703671, 21.84226448433411960, 8.527530157486179263 ) ) ;
#27960 = CARTESIAN_POINT ( 'NONE',  ( 0.1532563361054100626, 15.80059781766745353, -2.638427012816831230 ) ) ;
#27961 = CARTESIAN_POINT ( 'NONE',  ( 2.791683348922237240, 20.38393115100078745, -7.208316651077763204 ) ) ;
#27962 = CARTESIAN_POINT ( 'NONE',  ( 0.1532563361054082862, 6.217264484334118713, 2.638427012816831674 ) ) ;
#27963 = PRESENTATION_STYLE_ASSIGNMENT (( #65965 ) ) ;
#27965 = EDGE_CURVE ( 'NONE', #56218, #62023, #59077, .T. ) ;
#27964 = MECHANICAL_DESIGN_GEOMETRIC_PRESENTATION_REPRESENTATION (  '', ( #31181 ), #91871 ) ;
#27966 = DIRECTION ( 'NONE',  ( 0.000000000000000000, 6.938893903907222067E-15, 1.000000000000000000 ) ) ;
#27968 = CARTESIAN_POINT ( 'NONE',  ( -0.1042174387088609239, 23.10736173766202839, 6.337391062633419558 ) ) ;
#27967 = CARTESIAN_POINT ( 'NONE',  ( 18.52753015748618282, 3.925597817667451306, -4.923371831947291888 ) ) ;
#27969 = CARTESIAN_POINT ( 'NONE',  ( 7.361572987183169658, -0.03273551566588185635, -9.846743663894592657 ) ) ;
#27971 = VERTEX_POINT ( 'NONE', #71501 ) ;
#27970 = CARTESIAN_POINT ( 'NONE',  ( 17.20831665107776587, 24.13393115100078035, -7.208316651077762316 ) ) ;
#27972 = CARTESIAN_POINT ( 'NONE',  ( 5.170517050971797701, -13.81852248048419263, 4.000000000000000000 ) ) ;
#27973 = CARTESIAN_POINT ( 'NONE',  ( 0.6178305044545838731, -0.2513653300695798953, 9.382169495545420901 ) ) ;
#27974 = AXIS2_PLACEMENT_3D ( 'NONE', #68743, #46237, #77213 ) ;
#27975 = ORIENTED_EDGE ( 'NONE', *, *, #43388, .T. ) ;
#27976 = DIRECTION ( 'NONE',  ( -0.1736481776669272503, 0.9848077530122086864, -0.000000000000000000 ) ) ;
#27977 = CARTESIAN_POINT ( 'NONE',  ( 24.16423886937410614, 19.51208216824729647, -3.795296366450302550 ) ) ;
#27978 = DIRECTION ( 'NONE',  ( 0.000000000000000000, 0.000000000000000000, 1.000000000000000000 ) ) ;
#27979 = CARTESIAN_POINT ( 'NONE',  ( 20.36894250292379382, 13.67874883491396965, 10.36894250292379205 ) ) ;
#27980 = CARTESIAN_POINT ( 'NONE',  ( 24.16423886937410614, 49.30374883491396787, 8.672049930838204340E-16 ) ) ;
#27981 = SURFACE_SIDE_STYLE ('',( #57006 ) ) ;
#27982 = CARTESIAN_POINT ( 'NONE',  ( 10.00000000000000000, 10.55374883491396787, -14.16423886937410082 ) ) ;
#27983 = CARTESIAN_POINT ( 'NONE',  ( -0.8801773607111009756, 38.06368534415484106, 1.068504757029289695E-15 ) ) ;
#27984 = CARTESIAN_POINT ( 'NONE',  ( -11.42945456197624665, 15.00000000000000888, 9.127207413380620693 ) ) ;
#27985 = STYLED_ITEM ( 'NONE', ( #29555 ), #41388 ) ;
#27986 = ORIENTED_EDGE ( 'NONE', *, *, #35113, .F. ) ;
#27987 = CARTESIAN_POINT ( 'NONE',  ( 0.1532563361054100626, 15.80059781766745353, -2.638427012816831230 ) ) ;
#27988 = EDGE_CURVE ( 'NONE', #44781, #46930, #20764, .T. ) ;
#27990 = CARTESIAN_POINT ( 'NONE',  ( 17.20831665107776587, 32.88393115100078745, 7.208316651077764980 ) ) ;
#27989 = CARTESIAN_POINT ( 'NONE',  ( 12.91533473730992121, 54.52201867748816255, 10.88017736071110164 ) ) ;
#27991 = CARTESIAN_POINT ( 'NONE',  ( 2.035157376598822676, 7.438685344154837509, -7.964842623401177768 ) ) ;
#27992 = CARTESIAN_POINT ( 'NONE',  ( -2.816281873526473856, 64.12363466993042493, 9.499525473075851096E-16 ) ) ;
#27993 = CARTESIAN_POINT ( 'NONE',  ( 0.1532563361054082862, 56.21726448433411605, 2.638427012816831674 ) ) ;
#27994 = DIRECTION ( 'NONE',  ( 1.000000000000000000, 1.257402221000612102E-16, 0.000000000000000000 ) ) ;
#27995 = CARTESIAN_POINT ( 'NONE',  ( 21.09922568453595559, 37.04030133659708923, -6.408140936763230044 ) ) ;
#27996 = CARTESIAN_POINT ( 'NONE',  ( -7.082119434687058401, -14.02958449841935895, -12.26659068614894110 ) ) ;
#27997 = CARTESIAN_POINT ( 'NONE',  ( 18.52753015748618282, 33.92559781766745886, -4.923371831947291888 ) ) ;
#27998 = EDGE_CURVE ( 'NONE', #38297, #60237, #62494, .T. ) ;
#27999 = CARTESIAN_POINT ( 'NONE',  ( 6.204703633549690345, 32.84541550158063927, 14.16423886937410082 ) ) ;
#28000 = VERTEX_POINT ( 'NONE', #25513 ) ;
#28001 = PRESENTATION_STYLE_ASSIGNMENT (( #66000 ) ) ;
#28002 = VECTOR ( 'NONE', #4456, 1000.000000000000114 ) ;
#28003 = EDGE_CURVE ( 'NONE', #46643, #23582, #12755, .T. ) ;
#28004 = CARTESIAN_POINT ( 'NONE',  ( 0.5774900079438607392, 43.48035201082151247, 5.440088680355550821 ) ) ;
#28005 = CARTESIAN_POINT ( 'NONE',  ( 2.035157376598822676, 62.43868534415483396, -7.964842623401177768 ) ) ;
#28006 = CARTESIAN_POINT ( 'NONE',  ( 24.16423886937410614, 39.30374883491396787, 8.672049930838204340E-16 ) ) ;
#28007 = CARTESIAN_POINT ( 'NONE',  ( 7.361572987183170547, 67.05059781766746596, 9.846743663894590881 ) ) ;
#28008 = CARTESIAN_POINT ( 'NONE',  ( -2.816281873526473856, 64.33196800326376774, 3.434112377981055619 ) ) ;
#28009 = CARTESIAN_POINT ( 'NONE',  ( 20.88017736071110164, 40.35535201082150536, 2.915334737309930979 ) ) ;
#28010 = CARTESIAN_POINT ( 'NONE',  ( -6.715867195167534831, 4.123781235506717606E-16, 12.85095824508322693 ) ) ;
#28011 = CARTESIAN_POINT ( 'NONE',  ( 0.6178305044545818747, 28.49863466993041783, -9.382169495545419124 ) ) ;
#28012 = CARTESIAN_POINT ( 'NONE',  ( 7.361572987183169658, 59.96726448433410894, -9.846743663894592657 ) ) ;
#28013 = CARTESIAN_POINT ( 'NONE',  ( -5.440088680355547268, 18.89701867748817676, 9.422509992056143702 ) ) ;
#28014 = CARTESIAN_POINT ( 'NONE',  ( 15.44008868035555793, 6.397018677488171434, -9.422509992056140149 ) ) ;
#28015 = ORIENTED_EDGE ( 'NONE', *, *, #87250, .T. ) ;
#28016 =( NAMED_UNIT ( * ) SI_UNIT ( $, .STERADIAN. ) SOLID_ANGLE_UNIT ( ) );
#28017 = SURFACE_SIDE_STYLE ('',( #51519 ) ) ;
#28018 =( BOUNDED_CURVE ( )  B_SPLINE_CURVE ( 2, ( #92421, #24439, #54415, #85418, #90937, #16439, #1451, #30433, #31903 ),
 .UNSPECIFIED., .F., .F. ) 
 B_SPLINE_CURVE_WITH_KNOTS ( ( 3, 2, 2, 2, 3 ),
 ( 0.6901409369402313754, 0.6904761904761904656, 0.6964285714285713969, 0.7023809523809523281, 0.7027162059169114183 ),
 .UNSPECIFIED. ) 
 CURVE ( )  GEOMETRIC_REPRESENTATION_ITEM ( )  RATIONAL_B_SPLINE_CURVE ( ( 0.9963778908391764944, 0.9980808541467923733, 1.000000000000000000, 0.9659258262890683122, 1.000000000000000000, 0.9659258262890683122, 1.000000000000000000, 0.9980808541467923733, 0.9963778908391766054 ) ) 
 REPRESENTATION_ITEM ( '' )  );
#28019 = CARTESIAN_POINT ( 'NONE',  ( 2.791683348922240793, 1.633931151000784565, 7.208316651077764092 ) ) ;
#28020 = CARTESIAN_POINT ( 'NONE',  ( 20.88017736071110875, 65.77201867748817676, -2.915334737309920765 ) ) ;
#28021 = CARTESIAN_POINT ( 'NONE',  ( -14.17193700899791153, -0.03417435944610275333, 1.489530601563921808 ) ) ;
#28022 = VECTOR ( 'NONE', #82610, 1000.000000000000114 ) ;
#28024 = EDGE_CURVE ( 'NONE', #28504, #60588, #31988, .T. ) ;
#28023 = CARTESIAN_POINT ( 'NONE',  ( 0.1532563361054100626, 35.80059781766745175, -2.638427012816831230 ) ) ;
#28025 = CARTESIAN_POINT ( 'NONE',  ( 19.42250999205614193, 20.14701867748817321, 5.440088680355555262 ) ) ;
#28026 = CARTESIAN_POINT ( 'NONE',  ( 16.40814093676324603, 2.456968003263753531, -11.09922568453594671 ) ) ;
#28028 = CARTESIAN_POINT ( 'NONE',  ( 5.963430220938287007, 9.328790035174485240, 10.32896413005679825 ) ) ;
#28027 = CARTESIAN_POINT ( 'NONE',  ( 10.00000000000000178, 29.31368534415483751, 10.88017736071110342 ) ) ;
#28029 = CARTESIAN_POINT ( 'NONE',  ( 4.428481664934704527E-16, 23.03999999999999915, 0.000000000000000000 ) ) ;
#28030 = CARTESIAN_POINT ( 'NONE',  ( -2.816281873526473856, 39.33196800326374643, 3.434112377981055619 ) ) ;
#28031 = ORIENTED_EDGE ( 'NONE', *, *, #63010, .T. ) ;
#28032 = CARTESIAN_POINT ( 'NONE',  ( 15.44008868035555793, 66.39701867748817676, -9.422509992056140149 ) ) ;
#28034 = CARTESIAN_POINT ( 'NONE',  ( 19.80448550324509682, 51.82703681773345039, 6.500000000002705391 ) ) ;
#28033 = CARTESIAN_POINT ( 'NONE',  ( 6.565887622018943937, 18.08196800326375708, -12.81628187352647608 ) ) ;
#28035 = ADVANCED_FACE ( 'NONE', ( #75662 ), #7173, .F. ) ;
#28036 = CARTESIAN_POINT ( 'NONE',  ( 10.00000000000000000, 36.81368534415484106, -10.88017736071110342 ) ) ;
#28037 = FACE_OUTER_BOUND ( 'NONE', #12335, .T. ) ;
#28038 = CARTESIAN_POINT ( 'NONE',  ( 22.26659068614895176, 64.72041550158064638, -7.082119434687042414 ) ) ;
#28039 = CARTESIAN_POINT ( 'NONE',  ( 0.1532563361054100626, 55.80059781766745175, -2.638427012816831230 ) ) ;
#28040 = CARTESIAN_POINT ( 'NONE',  ( 19.84674366389459266, 8.300597817667451750, 2.638427012816836559 ) ) ;
#28041 = CARTESIAN_POINT ( 'NONE',  ( 12.91533473730993009, 61.60535201082150536, -10.88017736071109987 ) ) ;
#28042 = FACE_OUTER_BOUND ( 'NONE', #42138, .T. ) ;
#28043 = CARTESIAN_POINT ( 'NONE',  ( 17.08211943468705840, 25.13708216824730357, -12.26659068614894466 ) ) ;
#28044 = AXIS2_PLACEMENT_3D ( 'NONE', #72627, #57634, #34133 ) ;
#28045 =( LENGTH_UNIT ( ) NAMED_UNIT ( * ) SI_UNIT ( .MILLI., .METRE. ) );
#28046 = CARTESIAN_POINT ( 'NONE',  ( 19.54819611545891789, 81.00370271165274971, -4.999999999999999112 ) ) ;
#28047 = ORIENTED_EDGE ( 'NONE', *, *, #87534, .T. ) ;
#28048 = CARTESIAN_POINT ( 'NONE',  ( 10.00000000000000178, 63.05374883491396076, 14.16423886937410082 ) ) ;
#28049 = CARTESIAN_POINT ( 'NONE',  ( 10.00000000000000178, 48.05374883491396787, 14.16423886937410082 ) ) ;
#28050 = CARTESIAN_POINT ( 'NONE',  ( 18.52753015748617571, 28.09226448433411960, 4.923371831947298993 ) ) ;
#28052 = CARTESIAN_POINT ( 'NONE',  ( 21.09922568453595559, 27.04030133659708568, -6.408140936763230044 ) ) ;
#28051 = VECTOR ( 'NONE', #33319, 1000.000000000000000 ) ;
#28053 = CARTESIAN_POINT ( 'NONE',  ( -15.00000000000000000, 83.99999999999998579, -4.000000000000000000 ) ) ;
#28054 = CARTESIAN_POINT ( 'NONE',  ( 15.44008868035555793, 11.39701867748817143, -9.422509992056140149 ) ) ;
#28055 = CARTESIAN_POINT ( 'NONE',  ( 17.08211943468705130, 63.47041550158063927, 12.26659068614894998 ) ) ;
#28056 = CARTESIAN_POINT ( 'NONE',  ( 5.076628168052704559, 35.17559781766745175, -8.527530157486179263 ) ) ;
#28057 = DIRECTION ( 'NONE',  ( 0.000000000000000000, 0.000000000000000000, 1.000000000000000000 ) ) ;
#28058 = CARTESIAN_POINT ( 'NONE',  ( 0.1532563361054100626, 5.800597817667452638, -2.638427012816831230 ) ) ;
#28059 = CARTESIAN_POINT ( 'NONE',  ( 20.10493008474208310, 14.71697413083878914, 6.336235997365745831 ) ) ;
#28060 = CARTESIAN_POINT ( 'NONE',  ( 9.846743663894590881, 3.717264484334123598, -2.638427012816833894 ) ) ;
#28061 = ORIENTED_EDGE ( 'NONE', *, *, #18993, .F. ) ;
#28062 = ORIENTED_EDGE ( 'NONE', *, *, #27082, .F. ) ;
#28063 = CARTESIAN_POINT ( 'NONE',  ( -3.750000000000000000, 10.25000000000000000, -2.750000000000000000 ) ) ;
#28064 = ORIENTED_EDGE ( 'NONE', *, *, #92560, .F. ) ;
#28065 = CARTESIAN_POINT ( 'NONE',  ( 2.917880565312948704, 12.63708216824730179, 12.26659068614894643 ) ) ;
#28067 = CARTESIAN_POINT ( 'NONE',  ( 0.5774900079438607392, 23.48035201082150536, 5.440088680355550821 ) ) ;
#28066 = CARTESIAN_POINT ( 'NONE',  ( 10.00000000000000000, 16.81368534415483751, -10.88017736071110342 ) ) ;
#28069 = CARTESIAN_POINT ( 'NONE',  ( 0.6178305044545838731, 19.74863466993042138, 9.382169495545420901 ) ) ;
#28068 = CARTESIAN_POINT ( 'NONE',  ( 7.361572987183170547, 47.05059781766745175, 9.846743663894590881 ) ) ;
#28070 = CARTESIAN_POINT ( 'NONE',  ( 13.79529636645031943, 10.34541550158063394, -14.16423886937409904 ) ) ;
#28071 = CIRCLE ( 'NONE', #26426, 11.25000000000000178 ) ;
#28072 = VECTOR ( 'NONE', #32855, 1000.000000000000000 ) ;
#28073 = AXIS2_PLACEMENT_3D ( 'NONE', #43843, #74338, #91323 ) ;
#28075 = CARTESIAN_POINT ( 'NONE',  ( 0.6178305044545818747, 28.49863466993041783, -9.382169495545419124 ) ) ;
#28074 = AXIS2_PLACEMENT_3D ( 'NONE', #41150, #8664, #17660 ) ;
#28076 = ORIENTED_EDGE ( 'NONE', *, *, #84212, .F. ) ;
#28077 = CARTESIAN_POINT ( 'NONE',  ( 12.63842701281683034, 27.46726448433411250, 9.846743663894596210 ) ) ;
#28078 = CARTESIAN_POINT ( 'NONE',  ( -4.164238869374099039, 56.80374883491397497, 8.674139862899312516E-16 ) ) ;
#28079 = ORIENTED_EDGE ( 'NONE', *, *, #30121, .F. ) ;
#28080 = CARTESIAN_POINT ( 'NONE',  ( 2.035157376598824452, 3.688685344154837953, 7.964842623401179544 ) ) ;
#28081 = ORIENTED_EDGE ( 'NONE', *, *, #62664, .F. ) ;
#28082 = CARTESIAN_POINT ( 'NONE',  ( 20.88017736071110875, 50.77201867748817676, -2.915334737309920765 ) ) ;
#28083 = CARTESIAN_POINT ( 'NONE',  ( 0.5774900079438590739, 47.64701867748817676, -5.440088680355550821 ) ) ;
#28084 = CARTESIAN_POINT ( 'NONE',  ( 12.91533473730993009, 51.60535201082149825, -10.88017736071109987 ) ) ;
#28085 = DIRECTION ( 'NONE',  ( -3.996802888650564177E-14, 0.000000000000000000, 1.000000000000000000 ) ) ;
#28086 = CARTESIAN_POINT ( 'NONE',  ( 12.91533473730993009, 41.60535201082149825, -10.88017736071109987 ) ) ;
#28087 = CARTESIAN_POINT ( 'NONE',  ( 1.175037534397131322, -2.824431362619463692E-15, 14.57833316477037400 ) ) ;
#28088 = ADVANCED_FACE ( 'NONE', ( #78496 ), #37676, .T. ) ;
#28089 = ORIENTED_EDGE ( 'NONE', *, *, #91027, .F. ) ;
#28090 = AXIS2_PLACEMENT_3D ( 'NONE', #14127, #6127, #85450 ) ;
#28091 = CARTESIAN_POINT ( 'NONE',  ( 19.84674366389459266, 23.30059781766745530, 2.638427012816836559 ) ) ;
#28092 = ORIENTED_EDGE ( 'NONE', *, *, #56558, .T. ) ;
#28093 = CARTESIAN_POINT ( 'NONE',  ( 5.076628168052703671, 61.84226448433412315, 8.527530157486179263 ) ) ;
#28094 = CARTESIAN_POINT ( 'NONE',  ( -45.94000000000001194, 99.99999999999998579, -12.00000000000000000 ) ) ;
#28095 = CARTESIAN_POINT ( 'NONE',  ( 22.26659068614894466, 3.887082168247300906, 7.082119434687054849 ) ) ;
#28096 = ORIENTED_EDGE ( 'NONE', *, *, #94646, .F. ) ;
#28097 = CARTESIAN_POINT ( 'NONE',  ( -3.521970993462044230, -0.8418523783473399469, 3.750000000000000444 ) ) ;
#28098 = DIRECTION ( 'NONE',  ( 0.000000000000000000, 1.000000000000000000, 0.000000000000000000 ) ) ;
#28099 = CARTESIAN_POINT ( 'NONE',  ( 22.26659068614895176, 64.72041550158064638, -7.082119434687042414 ) ) ;
#28100 = LINE ( 'NONE', #75583, #83416 ) ;
#28101 = ORIENTED_EDGE ( 'NONE', *, *, #54099, .F. ) ;
#28102 = CARTESIAN_POINT ( 'NONE',  ( 17.85999999999999943, 37.99999999999997868, -9.500000000000000000 ) ) ;
#28103 = CARTESIAN_POINT ( 'NONE',  ( 0.1532563361054082862, 36.21726448433410894, 2.638427012816831674 ) ) ;
#28104 = CARTESIAN_POINT ( 'NONE',  ( 8.880000000000000782, 1.019547802438459216, 3.750000000000000000 ) ) ;
#28105 = AXIS2_PLACEMENT_3D ( 'NONE', #32068, #71082, #17102 ) ;
#28106 = VECTOR ( 'NONE', #20122, 1000.000000000000000 ) ;
#28107 = CARTESIAN_POINT ( 'NONE',  ( 13.43411237798105340, 0.5819680032637533085, 12.81628187352647963 ) ) ;
#28108 = CARTESIAN_POINT ( 'NONE',  ( 18.52753015748617571, 13.09226448433411960, 4.923371831947298993 ) ) ;
#28109 = CARTESIAN_POINT ( 'NONE',  ( 3.969999999999999751, 0.000000000000000000, 2.750000000000000000 ) ) ;
#28110 = CARTESIAN_POINT ( 'NONE',  ( 7.361572987183169658, 4.967264484334119601, -9.846743663894592657 ) ) ;
#28111 = CARTESIAN_POINT ( 'NONE',  ( 10.00000000000000000, -2.126365330069579951, -12.81628187352647608 ) ) ;
#28112 = CARTESIAN_POINT ( 'NONE',  ( 19.10478245763047056, 21.02576239577082262, -5.990408912944402253 ) ) ;
#28113 = ADVANCED_FACE ( 'NONE', ( #78001 ), #70510, .F. ) ;
#28114 = ORIENTED_EDGE ( 'NONE', *, *, #98201, .T. ) ;
#28115 = ADVANCED_FACE ( 'NONE', ( #17519 ), #68175, .F. ) ;
#28116 = CARTESIAN_POINT ( 'NONE',  ( 15.44008868035555793, 11.39701867748817143, -9.422509992056140149 ) ) ;
#28117 = CARTESIAN_POINT ( 'NONE',  ( 2.917880565312948704, 7.637082168247301794, 12.26659068614894643 ) ) ;
#28118 = CARTESIAN_POINT ( 'NONE',  ( 2.791683348922240793, 21.63393115100078745, 7.208316651077764092 ) ) ;
#28119 = CARTESIAN_POINT ( 'NONE',  ( 2.035157376598822676, 52.43868534415483396, -7.964842623401177768 ) ) ;
#28121 = SURFACE_SIDE_STYLE ('',( #6124 ) ) ;
#28120 = CARTESIAN_POINT ( 'NONE',  ( 10.00000000000000178, 30.37363466993042138, 12.81628187352647608 ) ) ;
#28122 = CARTESIAN_POINT ( 'NONE',  ( -16.94999999999999574, 99.99999999999998579, -7.750000000000000000 ) ) ;
#28123 = B_SPLINE_CURVE_WITH_KNOTS ( 'NONE', 3,
 ( #48283, #86791, #39329, #77796, #78795, #62296 ),
 .UNSPECIFIED., .F., .F.,
 ( 4, 2, 4 ),
 ( 3.409110551494651432E-05, 0.0004400426677367913963, 0.0008459942299586362038 ),
 .UNSPECIFIED. ) ;
#28124 = DIRECTION ( 'NONE',  ( -0.000000000000000000, -0.000000000000000000, -1.000000000000000000 ) ) ;
#28125 = DIRECTION ( 'NONE',  ( -0.000000000000000000, -1.000000000000000000, -0.000000000000000000 ) ) ;
#28126 = ADVANCED_FACE ( 'NONE', ( #26463 ), #95967, .T. ) ;
#28127 = CARTESIAN_POINT ( 'NONE',  ( 10.00000000000000000, 2.873634669930420049, -12.81628187352647608 ) ) ;
#28128 = CARTESIAN_POINT ( 'NONE',  ( 19.38216949554541202, 0.9986346699304200492, 9.382169495545424454 ) ) ;
#28129 = CARTESIAN_POINT ( 'NONE',  ( 14.92337183194729988, 9.342264484334119601, -8.527530157486177487 ) ) ;
#28130 = CARTESIAN_POINT ( 'NONE',  ( 7.964842623401181321, -30.06131465584516249, 7.964842623401174215 ) ) ;
#28131 = CARTESIAN_POINT ( 'NONE',  ( 19.38216949554541202, 20.99863466993042138, 9.382169495545424454 ) ) ;
#28132 = CARTESIAN_POINT ( 'NONE',  ( -11.38910604374480506, -77.84323126540351723, -4.000000000000000000 ) ) ;
#28133 = CARTESIAN_POINT ( 'NONE',  ( 2.035157376598824452, 28.68868534415484106, 7.964842623401179544 ) ) ;
#28134 = STYLED_ITEM ( 'NONE', ( #16217 ), #848 ) ;
#28135 = CARTESIAN_POINT ( 'NONE',  ( 2.261421327065750830, 0.000000000000000000, -4.962236210031242045 ) ) ;
#28136 = CARTESIAN_POINT ( 'NONE',  ( 24.16423886937410614, 49.51208216824730357, -3.795296366450302550 ) ) ;
#28137 = DIRECTION ( 'NONE',  ( -0.06975647374410356982, -0.9975640502598257520, 0.000000000000000000 ) ) ;
#28138 = CIRCLE ( 'NONE', #84047, 0.5000000000000000000 ) ;
#28139 = CARTESIAN_POINT ( 'NONE',  ( 15.44008868035555793, 26.39701867748817321, -9.422509992056140149 ) ) ;
#28140 = STYLED_ITEM ( 'NONE', ( #8814 ), #42728 ) ;
#28141 = CARTESIAN_POINT ( 'NONE',  ( 5.076628168052703671, 51.84226448433412315, 8.527530157486179263 ) ) ;
#28142 = CARTESIAN_POINT ( 'NONE',  ( 19.42250999205614193, 55.14701867748817676, 5.440088680355555262 ) ) ;
#28143 = EDGE_CURVE ( 'NONE', #11978, #95286, #72451, .T. ) ;
#28144 = CARTESIAN_POINT ( 'NONE',  ( 20.36894250292379382, 33.67874883491396076, 10.36894250292379205 ) ) ;
#28145 = CARTESIAN_POINT ( 'NONE',  ( 17.39651004071842166, 32.93575266056827644, 6.499999999999998224 ) ) ;
#28146 = AXIS2_PLACEMENT_3D ( 'NONE', #3269, #78773, #19245 ) ;
#28147 = UNCERTAINTY_MEASURE_WITH_UNIT (LENGTH_MEASURE( 1.000000000000000082E-05 ), #33557, 'distance_accuracy_value', 'NONE');
#28148 = CARTESIAN_POINT ( 'NONE',  ( 19.84674366389459266, 43.30059781766744464, 2.638427012816836559 ) ) ;
#28149 = CARTESIAN_POINT ( 'NONE',  ( 16.40814093676324603, 2.456968003263753531, -11.09922568453594671 ) ) ;
#28150 = ORIENTED_EDGE ( 'NONE', *, *, #60958, .F. ) ;
#28151 = CARTESIAN_POINT ( 'NONE',  ( 2.035157376598824452, 18.68868534415484106, 7.964842623401179544 ) ) ;
#28152 = LINE ( 'NONE', #3700, #12572 ) ;
#28153 = CARTESIAN_POINT ( 'NONE',  ( 0.5774900079438607392, 13.48035201082150358, 5.440088680355550821 ) ) ;
#28154 = CARTESIAN_POINT ( 'NONE',  ( 2.791683348922240793, 1.633931151000784565, 7.208316651077764092 ) ) ;
#28155 = CARTESIAN_POINT ( 'NONE',  ( 24.16423886937410614, 29.51208216824729647, -3.795296366450302550 ) ) ;
#28156 = CARTESIAN_POINT ( 'NONE',  ( 18.52753015748617571, 13.09226448433411960, 4.923371831947298993 ) ) ;
#28157 = CARTESIAN_POINT ( 'NONE',  ( 5.076628168052704559, 65.17559781766745175, -8.527530157486179263 ) ) ;
#28158 = CARTESIAN_POINT ( 'NONE',  ( 15.44008868035555793, 36.39701867748816966, -9.422509992056140149 ) ) ;
#28159 = DIRECTION ( 'NONE',  ( -0.8241261886220241362, -0.000000000000000000, 0.5664062369248205053 ) ) ;
#28160 = DIRECTION ( 'NONE',  ( 0.9981347984218662539, 0.000000000000000000, 0.06104853953487057033 ) ) ;
#28162 = ORIENTED_EDGE ( 'NONE', *, *, #11560, .F. ) ;
#28161 = AXIS2_PLACEMENT_3D ( 'NONE', #98751, #76695, #82719 ) ;
#28163 = CARTESIAN_POINT ( 'NONE',  ( 2.913501739333663743, 15.00000000000000000, 14.20427779279537184 ) ) ;
#28164 = CARTESIAN_POINT ( 'NONE',  ( 14.92337183194729633, 47.67559781766745175, 8.527530157486181039 ) ) ;
#28165 = CIRCLE ( 'NONE', #25053, 15.00000000000000000 ) ;
#28166 = VERTEX_POINT ( 'NONE', #18980 ) ;
#28167 = VERTEX_POINT ( 'NONE', #88451 ) ;
#28168 = CARTESIAN_POINT ( 'NONE',  ( 8.880000000000020322, 80.07179676972448590, -4.250000000000000000 ) ) ;
#28169 = CARTESIAN_POINT ( 'NONE',  ( -2.266590686148945544, 27.22041550158063572, 7.082119434687048631 ) ) ;
#28171 = CIRCLE ( 'NONE', #79275, 0.2500000000000002220 ) ;
#28170 = CARTESIAN_POINT ( 'NONE',  ( 22.26659068614895176, 14.72041550158063572, -7.082119434687042414 ) ) ;
#28172 = CARTESIAN_POINT ( 'NONE',  ( 19.42250999205614193, 65.14701867748817676, 5.440088680355555262 ) ) ;
#28173 = CARTESIAN_POINT ( 'NONE',  ( 6.204703633549690345, 55.76208216824730357, -14.16423886937410259 ) ) ;
#28174 = CARTESIAN_POINT ( 'NONE',  ( 2.791683348922240793, 36.63393115100078035, 7.208316651077764092 ) ) ;
#28175 = CARTESIAN_POINT ( 'NONE',  ( -16.94999999999999574, 99.99999999999998579, 7.750000000000000000 ) ) ;
#28177 = CARTESIAN_POINT ( 'NONE',  ( 21.09922568453594849, 6.206968003263753531, 6.408140936763242479 ) ) ;
#28176 = CARTESIAN_POINT ( 'NONE',  ( 0.5774900079438607392, 28.48035201082150891, 5.440088680355550821 ) ) ;
#28178 = CARTESIAN_POINT ( 'NONE',  ( -2.266590686148945544, 21.38708216824730357, -7.082119434687050408 ) ) ;
#28179 = CARTESIAN_POINT ( 'NONE',  ( 6.204703633549690345, 57.84541550158063927, 14.16423886937410082 ) ) ;
#28180 = CARTESIAN_POINT ( 'NONE',  ( -0.8801773607111008646, 18.27201867748817321, 2.915334737309923430 ) ) ;
#28181 = LINE ( 'NONE', #65678, #35476 ) ;
#28182 = CARTESIAN_POINT ( 'NONE',  ( -0.3289641300567998083, 3.078790035174471029, 5.963430220938281678 ) ) ;
#28183 = CARTESIAN_POINT ( 'NONE',  ( 17.96484262340118221, 41.18868534415484106, -7.964842623401177768 ) ) ;
#28184 = CARTESIAN_POINT ( 'NONE',  ( -3.469446951953614189E-15, -35.24106884899921255, -9.846743663894594434 ) ) ;
#28185 = ORIENTED_EDGE ( 'NONE', *, *, #37407, .F. ) ;
#28186 = PRESENTATION_STYLE_ASSIGNMENT (( #88685 ) ) ;
#28187 = ORIENTED_EDGE ( 'NONE', *, *, #32045, .F. ) ;
#28188 = ORIENTED_EDGE ( 'NONE', *, *, #42477, .F. ) ;
#28189 = CARTESIAN_POINT ( 'NONE',  ( 2.917880565312950480, 50.97041550158064638, -12.26659068614894821 ) ) ;
#28190 = CARTESIAN_POINT ( 'NONE',  ( 14.92337183194729633, 52.67559781766745175, 8.527530157486181039 ) ) ;
#28191 = CARTESIAN_POINT ( 'NONE',  ( 20.88017736071110164, 55.35535201082149825, 2.915334737309930979 ) ) ;
#28192 = DIRECTION ( 'NONE',  ( 1.000000000000000000, 0.000000000000000000, 0.000000000000000000 ) ) ;
#28193 = CARTESIAN_POINT ( 'NONE',  ( 12.91533473730993009, 51.60535201082149825, -10.88017736071109987 ) ) ;
#28194 = CARTESIAN_POINT ( 'NONE',  ( 13.43411237798105340, 60.58196800326376064, 12.81628187352647963 ) ) ;
#28195 = CARTESIAN_POINT ( 'NONE',  ( 3.469446951953614189E-15, 10.37363466993042316, 12.81628187352647608 ) ) ;
#28196 = ORIENTED_EDGE ( 'NONE', *, *, #96714, .F. ) ;
#28197 = CARTESIAN_POINT ( 'NONE',  ( 20.36894250292379738, 24.92874883491396787, -10.36894250292379027 ) ) ;
#28198 = CARTESIAN_POINT ( 'NONE',  ( 10.00000000000000178, 25.37363466993041783, 12.81628187352647608 ) ) ;
#28199 = ORIENTED_EDGE ( 'NONE', *, *, #72493, .T. ) ;
#28200 = CARTESIAN_POINT ( 'NONE',  ( 0.6178305044545818747, 38.49863466993042493, -9.382169495545419124 ) ) ;
#28201 = CARTESIAN_POINT ( 'NONE',  ( 10.00000000000000000, 16.81368534415483751, -10.88017736071110342 ) ) ;
#28202 = CARTESIAN_POINT ( 'NONE',  ( 1.472469842513823179, 31.42559781766745530, 4.923371831947296329 ) ) ;
#28203 = CARTESIAN_POINT ( 'NONE',  ( -0.8801773607111009756, 13.06368534415483929, 1.068504757029289695E-15 ) ) ;
#28204 = CARTESIAN_POINT ( 'NONE',  ( 6.565887622018943937, 58.08196800326376064, -12.81628187352647608 ) ) ;
#28205 = CARTESIAN_POINT ( 'NONE',  ( -11.64999999999999680, 98.49999999999998579, -8.525133428036873795 ) ) ;
#28206 = CARTESIAN_POINT ( 'NONE',  ( 14.92337183194729633, 42.67559781766745886, 8.527530157486181039 ) ) ;
#28207 = EDGE_CURVE ( 'NONE', #34886, #21097, #95468, .T. ) ;
#28208 = CARTESIAN_POINT ( 'NONE',  ( 0.000000000000000000, 14.49999999999999822, 0.000000000000000000 ) ) ;
#28209 = CARTESIAN_POINT ( 'NONE',  ( 0.1089645850228891377, 3.162345557925709372, 6.479102184480797000 ) ) ;
#28210 = DIRECTION ( 'NONE',  ( -0.000000000000000000, -1.000000000000000000, -0.000000000000000000 ) ) ;
#28211 = PLANE ( 'NONE',  #81862 ) ;
#28212 = TOROIDAL_SURFACE ( 'NONE', #23465, 14.49999999999999822, 0.5000000000000000000 ) ;
#28213 = DIRECTION ( 'NONE',  ( 0.000000000000000000, -1.000000000000000000, 0.000000000000000000 ) ) ;
#28214 = CARTESIAN_POINT ( 'NONE',  ( 0.1532563361054083140, 21.00893115100078745, 1.131784320476157264E-15 ) ) ;
#28215 = CARTESIAN_POINT ( 'NONE',  ( 10.00000000000000178, 20.37363466993042138, 12.81628187352647608 ) ) ;
#28216 = CARTESIAN_POINT ( 'NONE',  ( 3.115783986955559470, 4.823715477197806954E-16, -14.16128137375397777 ) ) ;
#28217 = ORIENTED_EDGE ( 'NONE', *, *, #74833, .F. ) ;
#28218 = CARTESIAN_POINT ( 'NONE',  ( 1.472469842513823179, 55.59226448433412315, -4.923371831947296329 ) ) ;
#28219 = DIRECTION ( 'NONE',  ( 0.000000000000000000, -1.000000000000000000, 0.000000000000000000 ) ) ;
#28220 = CARTESIAN_POINT ( 'NONE',  ( 17.08211943468705130, 18.47041550158063572, 12.26659068614894998 ) ) ;
#28221 = CARTESIAN_POINT ( 'NONE',  ( 2.791683348922240793, 51.63393115100078745, 7.208316651077764092 ) ) ;
#28222 = CARTESIAN_POINT ( 'NONE',  ( 0.6178305044545838731, 44.74863466993042493, 9.382169495545420901 ) ) ;
#28223 = CARTESIAN_POINT ( 'NONE',  ( 13.34343830728404079, 15.00000000000000000, -6.852200678592596184 ) ) ;
#28224 = CARTESIAN_POINT ( 'NONE',  ( 15.44008868035555260, 64.73035201082151957, 9.422509992056143702 ) ) ;
#28225 = CARTESIAN_POINT ( 'NONE',  ( 0.1077916266722774852, 67.24062864464239908, -6.478736007406002528 ) ) ;
#28226 = CARTESIAN_POINT ( 'NONE',  ( 7.361572987183170547, 32.05059781766745175, 9.846743663894590881 ) ) ;
#28227 = CARTESIAN_POINT ( 'NONE',  ( 7.084665262690076126, 37.02201867748817676, -10.88017736071110164 ) ) ;
#28228 = CARTESIAN_POINT ( 'NONE',  ( 21.09922568453595559, 37.04030133659708923, -6.408140936763230044 ) ) ;
#28229 = TOROIDAL_SURFACE ( 'NONE', #84139, 14.49999999999999822, 0.5000000000000000000 ) ;
#28230 = CARTESIAN_POINT ( 'NONE',  ( 19.84674366389459266, 28.71726448433411960, -2.638427012816827677 ) ) ;
#28231 = VECTOR ( 'NONE', #53129, 1000.000000000000000 ) ;
#28232 = DIRECTION ( 'NONE',  ( -0.8610351672809775092, 0.4339697742547262704, -0.2651201156810271131 ) ) ;
#28233 = CARTESIAN_POINT ( 'NONE',  ( -13.87912815710419068, 90.90967772850538609, 7.772688653987089857 ) ) ;
#28235 = ADVANCED_FACE ( 'NONE', ( #27940 ), #65443, .T. ) ;
#28234 = AXIS2_PLACEMENT_3D ( 'NONE', #19519, #64992, #80519 ) ;
#28236 = CARTESIAN_POINT ( 'NONE',  ( -0.8801773607111008646, 38.27201867748816255, 2.915334737309923430 ) ) ;
#28237 = ORIENTED_EDGE ( 'NONE', *, *, #34348, .T. ) ;
#28238 = PLANE ( 'NONE',  #34575 ) ;
#28239 = CARTESIAN_POINT ( 'NONE',  ( 7.084665262690076126, 12.02201867748817143, -10.88017736071110164 ) ) ;
#28241 = CARTESIAN_POINT ( 'NONE',  ( 7.084665262690076126, 42.02201867748816966, -10.88017736071110164 ) ) ;
#28240 = CARTESIAN_POINT ( 'NONE',  ( 0.1532563361054100626, 55.80059781766745175, -2.638427012816831230 ) ) ;
#28242 = CARTESIAN_POINT ( 'NONE',  ( 6.880000000000009663, 40.99999999999999289, 6.500000000000000888 ) ) ;
#28243 = CARTESIAN_POINT ( 'NONE',  ( 19.42250999205614548, 60.98035201082151247, -5.440088680355545492 ) ) ;
#28245 = DIRECTION ( 'NONE',  ( -0.5664062369248369366, 0.000000000000000000, 0.8241261886220129229 ) ) ;
#28244 = CARTESIAN_POINT ( 'NONE',  ( 7.084665262690076126, 32.02201867748816966, -10.88017736071110164 ) ) ;
#28246 = CARTESIAN_POINT ( 'NONE',  ( 10.00000000000000000, 4.758931151000784787, -9.846743663894594434 ) ) ;
#28247 = CARTESIAN_POINT ( 'NONE',  ( 17.20831665107776587, 29.13393115100078390, -7.208316651077762316 ) ) ;
#28248 = FACE_OUTER_BOUND ( 'NONE', #71439, .T. ) ;
#28249 = CARTESIAN_POINT ( 'NONE',  ( -7.082119434687058401, 10.97041550158064283, -12.26659068614894110 ) ) ;
#28250 = CARTESIAN_POINT ( 'NONE',  ( 7.361572987183169658, 49.96726448433410894, -9.846743663894592657 ) ) ;
#28251 = CLOSED_SHELL ( 'NONE', ( #40089, #93361, #59049, #9311, #82063, #34808, #58866, #28235, #10064, #49984, #37767, #72656, #56477, #58568, #50063, #96661, #4915 ) ) ;
#28252 = CARTESIAN_POINT ( 'NONE',  ( 2.917880565312950480, 55.97041550158063217, -12.26659068614894821 ) ) ;
#28253 = CARTESIAN_POINT ( 'NONE',  ( 1.602071938427537923, 62.02224192338640307, -6.500000000000073719 ) ) ;
#28254 = CARTESIAN_POINT ( 'NONE',  ( 17.08211943468705840, 10.13708216824730179, -12.26659068614894466 ) ) ;
#28255 = CARTESIAN_POINT ( 'NONE',  ( 2.917880565312948704, 42.63708216824729647, 12.26659068614894643 ) ) ;
#28256 = CARTESIAN_POINT ( 'NONE',  ( 13.43411237798106583, 2.665301336597086568, -12.81628187352647252 ) ) ;
#28257 = ORIENTED_EDGE ( 'NONE', *, *, #8210, .F. ) ;
#28258 = CARTESIAN_POINT ( 'NONE',  ( 19.42250999205614193, 20.14701867748817321, 5.440088680355555262 ) ) ;
#28259 = CARTESIAN_POINT ( 'NONE',  ( 18.52753015748617571, 48.09226448433412315, 4.923371831947298993 ) ) ;
#28261 = CARTESIAN_POINT ( 'NONE',  ( -13.75801628063875803, 15.00000000000000000, -4.578972376164643698 ) ) ;
#28260 = FILL_AREA_STYLE_COLOUR ( '', #78713 ) ;
#28262 =( NAMED_UNIT ( * ) PLANE_ANGLE_UNIT ( ) SI_UNIT ( $, .RADIAN. ) );
#28263 = CIRCLE ( 'NONE', #85743, 15.00000000000000000 ) ;
#28264 = LINE ( 'NONE', #66760, #13191 ) ;
#28265 = CARTESIAN_POINT ( 'NONE',  ( 13.43411237798106583, 27.66530133659708568, -12.81628187352647252 ) ) ;
#28266 = CARTESIAN_POINT ( 'NONE',  ( 17.20831665107776587, 22.88393115100078745, 7.208316651077764980 ) ) ;
#28267 = VERTEX_POINT ( 'NONE', #50945 ) ;
#28268 = CARTESIAN_POINT ( 'NONE',  ( 7.361572987183169658, 14.96726448433411960, -9.846743663894592657 ) ) ;
#28269 = SURFACE_STYLE_FILL_AREA ( #66765 ) ;
#28270 = CARTESIAN_POINT ( 'NONE',  ( 12.91533473730992121, 4.522018677488170546, 10.88017736071110164 ) ) ;
#28271 = CARTESIAN_POINT ( 'NONE',  ( 12.91533473730992121, 14.52201867748817143, 10.88017736071110164 ) ) ;
#28272 = CARTESIAN_POINT ( 'NONE',  ( 20.36894250292379382, 38.67874883491396076, 10.36894250292379205 ) ) ;
#28273 = CARTESIAN_POINT ( 'NONE',  ( 7.084665262690076126, 44.10535201082151247, 10.88017736071109987 ) ) ;
#28274 = CARTESIAN_POINT ( 'NONE',  ( 4.559911319644449179, 58.89701867748817676, 9.422509992056141925 ) ) ;
#28275 = DIRECTION ( 'NONE',  ( 0.06104853953485662316, 0.000000000000000000, 0.9981347984218670311 ) ) ;
#28276 = EDGE_CURVE ( 'NONE', #36269, #49707, #81439, .T. ) ;
#28277 = CARTESIAN_POINT ( 'NONE',  ( 20.32896413005680358, 39.74545670184114243, 5.963430220938287007 ) ) ;
#28278 = CARTESIAN_POINT ( 'NONE',  ( 5.076628168052704559, 20.17559781766745175, -8.527530157486179263 ) ) ;
#28279 = PRESENTATION_STYLE_ASSIGNMENT (( #96803 ) ) ;
#28280 = CARTESIAN_POINT ( 'NONE',  ( 2.791683348922240793, 6.633931151000785675, 7.208316651077764092 ) ) ;
#28281 = CARTESIAN_POINT ( 'NONE',  ( 8.630000000000000782, 1.085138116723527427E-15, -6.250000000000000000 ) ) ;
#28282 = CARTESIAN_POINT ( 'NONE',  ( 0.1532563361054083140, 31.00893115100078390, 1.131784320476157264E-15 ) ) ;
#28283 = CARTESIAN_POINT ( 'NONE',  ( -1.099225684535947600, -1.293031996736246469, -6.408140936763238038 ) ) ;
#28284 = EDGE_CURVE ( 'NONE', #39981, #63027, #73937, .T. ) ;
#28285 = CARTESIAN_POINT ( 'NONE',  ( 20.88017736071110875, 35.77201867748816966, -2.915334737309920765 ) ) ;
#28286 = ORIENTED_EDGE ( 'NONE', *, *, #68762, .T. ) ;
#28287 = CARTESIAN_POINT ( 'NONE',  ( -2.816281873526473856, 59.12363466993042493, 9.499525473075851096E-16 ) ) ;
#28288 = DIRECTION ( 'NONE',  ( -0.9170600743851211600, 0.000000000000000000, -0.3987490689252528031 ) ) ;
#28289 = CARTESIAN_POINT ( 'NONE',  ( 0.1532563361054083140, 1.008931151000784787, 1.131784320476157264E-15 ) ) ;
#28290 = CARTESIAN_POINT ( 'NONE',  ( 6.565887622018943937, 43.08196800326374643, -12.81628187352647608 ) ) ;
#28292 = CARTESIAN_POINT ( 'NONE',  ( 7.361572987183170547, 37.05059781766744464, 9.846743663894590881 ) ) ;
#28291 = CARTESIAN_POINT ( 'NONE',  ( 24.16423886937410614, 64.30374883491396076, 8.672049930838204340E-16 ) ) ;
#28293 = CARTESIAN_POINT ( 'NONE',  ( -0.03447792253739352664, 60.15514106990690379, 6.401564815979744694 ) ) ;
#28294 = AXIS2_PLACEMENT_3D ( 'NONE', #24071, #40048, #1085 ) ;
#28295 = CARTESIAN_POINT ( 'NONE',  ( 19.84674366389459621, 63.50893115100078745, 7.409399052514197653E-17 ) ) ;
#28296 = CARTESIAN_POINT ( 'NONE',  ( -4.164238869374099927, 47.01208216824729647, 3.795296366450308767 ) ) ;
#28297 = CARTESIAN_POINT ( 'NONE',  ( 0.1532563361054083140, 41.00893115100078745, 1.131784320476157264E-15 ) ) ;
#28298 = CARTESIAN_POINT ( 'NONE',  ( -14.69227023463711568, 0.04922511925147164680, 1.335400878252435808 ) ) ;
#28299 = CARTESIAN_POINT ( 'NONE',  ( 15.44008868035555793, 41.39701867748817676, -9.422509992056140149 ) ) ;
#28300 = CARTESIAN_POINT ( 'NONE',  ( 19.42250999205614193, 60.14701867748817676, 5.440088680355555262 ) ) ;
#28301 = STYLED_ITEM ( 'NONE', ( #18022 ), #11513 ) ;
#28302 = CARTESIAN_POINT ( 'NONE',  ( -0.08248232600719085372, 0.1423898869303599768, 6.349449577244200782 ) ) ;
#28303 = ORIENTED_EDGE ( 'NONE', *, *, #11000, .F. ) ;
#28304 = CARTESIAN_POINT ( 'NONE',  ( 19.38216949554541557, 47.24863466993041783, -9.382169495545420901 ) ) ;
#28305 = ORIENTED_EDGE ( 'NONE', *, *, #34448, .F. ) ;
#28306 = CARTESIAN_POINT ( 'NONE',  ( 10.00000000000000000, -0.2410688489992152128, -9.846743663894594434 ) ) ;
#28307 = ORIENTED_EDGE ( 'NONE', *, *, #80156, .T. ) ;
#28308 = CARTESIAN_POINT ( 'NONE',  ( 10.00000000000000178, 8.053748834913967869, 14.16423886937410082 ) ) ;
#28309 = CARTESIAN_POINT ( 'NONE',  ( 17.20831665107776587, 9.133931151000787452, -7.208316651077762316 ) ) ;
#28310 = AXIS2_PLACEMENT_3D ( 'NONE', #79871, #49369, #11375 ) ;
#28311 = FACE_OUTER_BOUND ( 'NONE', #11482, .T. ) ;
#28312 = ORIENTED_EDGE ( 'NONE', *, *, #2682, .F. ) ;
#28313 = AXIS2_PLACEMENT_3D ( 'NONE', #53008, #7542, #92484 ) ;
#28314 = CARTESIAN_POINT ( 'NONE',  ( 0.5774900079438607392, 8.480352010821505360, 5.440088680355550821 ) ) ;
#28315 = CARTESIAN_POINT ( 'NONE',  ( 20.36894250292379738, 14.92874883491396432, -10.36894250292379027 ) ) ;
#28316 = ORIENTED_EDGE ( 'NONE', *, *, #47634, .F. ) ;
#28317 = CARTESIAN_POINT ( 'NONE',  ( 17.96484262340118221, 24.93868534415484461, 7.964842623401181321 ) ) ;
#28318 = CARTESIAN_POINT ( 'NONE',  ( 12.63842701281683034, 57.46726448433411605, 9.846743663894596210 ) ) ;
#28319 = EDGE_LOOP ( 'NONE', ( #9267, #8654, #38863, #48401 ) ) ;
#28320 = B_SPLINE_CURVE_WITH_KNOTS ( 'NONE', 3,
 ( #89040, #5057, #36033, #7030, #35541, #36544 ),
 .UNSPECIFIED., .F., .F.,
 ( 4, 2, 4 ),
 ( 0.000000000000000000, 0.0002701661927229369623, 0.0005403323854458739247 ),
 .UNSPECIFIED. ) ;
#28321 = CARTESIAN_POINT ( 'NONE',  ( 0.1532563361054100626, 55.80059781766745175, -2.638427012816831230 ) ) ;
#28322 = ORIENTED_EDGE ( 'NONE', *, *, #4085, .T. ) ;
#28323 = CARTESIAN_POINT ( 'NONE',  ( 15.44008868035555793, 61.39701867748817676, -9.422509992056140149 ) ) ;
#28324 = CARTESIAN_POINT ( 'NONE',  ( 2.791683348922240793, 61.63393115100079456, 7.208316651077764092 ) ) ;
#28325 = CARTESIAN_POINT ( 'NONE',  ( -2.816281873526471635, 38.91530133659708213, -3.434112377981056508 ) ) ;
#28327 = DIRECTION ( 'NONE',  ( -1.927470528863119542E-16, 1.000000000000000000, 0.000000000000000000 ) ) ;
#28326 = CARTESIAN_POINT ( 'NONE',  ( 7.084665262690076126, 7.022018677488169658, -10.88017736071110164 ) ) ;
#28328 = CARTESIAN_POINT ( 'NONE',  ( 18.52753015748618282, 3.925597817667451306, -4.923371831947291888 ) ) ;
#28329 = CARTESIAN_POINT ( 'NONE',  ( 0.5774900079438607392, 23.48035201082150536, 5.440088680355550821 ) ) ;
#28330 = EDGE_CURVE ( 'NONE', #49375, #9043, #97088, .T. ) ;
#28331 = ORIENTED_EDGE ( 'NONE', *, *, #40561, .F. ) ;
#28332 = CARTESIAN_POINT ( 'NONE',  ( 3.591859063236763294, 48.29030133659708923, -11.09922568453595026 ) ) ;
#28333 = CARTESIAN_POINT ( 'NONE',  ( 20.88017736071110875, 45.77201867748816966, -2.915334737309920765 ) ) ;
#28334 = DIRECTION ( 'NONE',  ( 0.000000000000000000, -0.000000000000000000, -1.000000000000000000 ) ) ;
#28335 = CARTESIAN_POINT ( 'NONE',  ( -2.816281873526471635, 43.91530133659708923, -3.434112377981056508 ) ) ;
#28336 = CARTESIAN_POINT ( 'NONE',  ( 2.035157376598822676, 47.43868534415484817, -7.964842623401177768 ) ) ;
#28337 = AXIS2_PLACEMENT_3D ( 'NONE', #78887, #76917, #77898 ) ;
#28338 = CARTESIAN_POINT ( 'NONE',  ( 19.84674366389459266, 58.71726448433411605, -2.638427012816827677 ) ) ;
#28339 = ORIENTED_EDGE ( 'NONE', *, *, #51194, .T. ) ;
#28340 = CARTESIAN_POINT ( 'NONE',  ( -7.640917710489092407, 14.95077488074853811, 12.61992379908748418 ) ) ;
#28341 = CARTESIAN_POINT ( 'NONE',  ( 18.52753015748618282, 23.92559781766745530, -4.923371831947291888 ) ) ;
#28342 = CARTESIAN_POINT ( 'NONE',  ( 22.81628187352647785, 1.415301336597087012, 3.434112377981063169 ) ) ;
#28344 = CARTESIAN_POINT ( 'NONE',  ( -7.313705784284714184, 14.63606873438734546, 13.09617149020741778 ) ) ;
#28343 = CARTESIAN_POINT ( 'NONE',  ( 10.00000000000000178, 70.00000000000000000, 0.000000000000000000 ) ) ;
#28345 = CARTESIAN_POINT ( 'NONE',  ( 20.88017736071110164, 20.35535201082150891, 2.915334737309930979 ) ) ;
#28346 = CARTESIAN_POINT ( 'NONE',  ( 7.361572987183170547, 52.05059781766745175, 9.846743663894590881 ) ) ;
#28347 = CARTESIAN_POINT ( 'NONE',  ( 10.84451454130500636, 4.196149184706192213E-16, 9.625305416630906663 ) ) ;
#28348 = PLANE ( 'NONE',  #35934 ) ;
#28349 = PRESENTATION_LAYER_ASSIGNMENT (  '', '', ( #71482 ) ) ;
#28350 = CARTESIAN_POINT ( 'NONE',  ( 19.84674366389459266, 8.300597817667451750, 2.638427012816836559 ) ) ;
#28351 =( NAMED_UNIT ( * ) SI_UNIT ( $, .STERADIAN. ) SOLID_ANGLE_UNIT ( ) );
#28353 = EDGE_LOOP ( 'NONE', ( #11722, #4832, #52423, #55489, #31991, #71519 ) ) ;
#28352 = CARTESIAN_POINT ( 'NONE',  ( 6.565887622018943937, 0.1653013365970866511, 12.81628187352647430 ) ) ;
#28354 = AXIS2_PLACEMENT_3D ( 'NONE', #49561, #18112, #95577 ) ;
#28355 = DIRECTION ( 'NONE',  ( -1.000000000000000000, -1.927470528863119542E-16, 0.000000000000000000 ) ) ;
#28356 = CARTESIAN_POINT ( 'NONE',  ( -2.816281873526473856, 34.12363466993042493, 9.499525473075851096E-16 ) ) ;
#28357 = EDGE_CURVE ( 'NONE', #91269, #49746, #35445, .T. ) ;
#28358 = CARTESIAN_POINT ( 'NONE',  ( 12.63842701281683922, 34.55059781766745886, -9.846743663894590881 ) ) ;
#28359 = DIRECTION ( 'NONE',  ( 0.000000000000000000, 0.000000000000000000, -1.000000000000000000 ) ) ;
#28360 = CARTESIAN_POINT ( 'NONE',  ( 22.26659068614894466, 63.88708216824730357, 7.082119434687054849 ) ) ;
#28361 = CARTESIAN_POINT ( 'NONE',  ( 1.472469842513823179, 26.42559781766745175, 4.923371831947296329 ) ) ;
#28362 = CARTESIAN_POINT ( 'NONE',  ( 1.350000000000004086, 98.49999999999998579, 8.000000000000000000 ) ) ;
#28363 = EDGE_CURVE ( 'NONE', #75159, #90793, #28747, .T. ) ;
#28364 = CARTESIAN_POINT ( 'NONE',  ( 12.91533473730992121, 9.522018677488171434, 10.88017736071110164 ) ) ;
#28365 = CARTESIAN_POINT ( 'NONE',  ( -10.17570567488968081, 89.26421072723886141, -5.905278573613798265 ) ) ;
#28366 = CARTESIAN_POINT ( 'NONE',  ( 2.035157376598822676, 17.43868534415483751, -7.964842623401177768 ) ) ;
#28368 = STYLED_ITEM ( 'NONE', ( #51937 ), #12766 ) ;
#28367 = CARTESIAN_POINT ( 'NONE',  ( -2.266590686148945544, 56.38708216824731068, -7.082119434687050408 ) ) ;
#28370 = CARTESIAN_POINT ( 'NONE',  ( -10.76445796112991360, -3.815459910906994300E-15, 9.901260316209766543 ) ) ;
#28369 = CARTESIAN_POINT ( 'NONE',  ( -2.266590686148945544, 51.38708216824730357, -7.082119434687050408 ) ) ;
#28371 = CARTESIAN_POINT ( 'NONE',  ( 0.1532563361054100626, 10.80059781766745175, -2.638427012816831230 ) ) ;
#28372 = CARTESIAN_POINT ( 'NONE',  ( 7.361572987183169658, 64.96726448433412315, -9.846743663894592657 ) ) ;
#28373 = VECTOR ( 'NONE', #12872, 1000.000000000000114 ) ;
#28374 = VERTEX_POINT ( 'NONE', #79481 ) ;
#28375 = CARTESIAN_POINT ( 'NONE',  ( 2.035157376598822676, 47.43868534415484817, -7.964842623401177768 ) ) ;
#28376 = CARTESIAN_POINT ( 'NONE',  ( 0.5774900079438607392, 18.48035201082150536, 5.440088680355550821 ) ) ;
#28378 = FACE_OUTER_BOUND ( 'NONE', #398, .T. ) ;
#28377 = COLOUR_RGB ( '', 0.08235294, 0.09019608, 0.10196078) ;
#28379 = AXIS2_PLACEMENT_3D ( 'NONE', #53147, #66679, #60149 ) ;
#28380 = FACE_OUTER_BOUND ( 'NONE', #61405, .T. ) ;
#28381 = CARTESIAN_POINT ( 'NONE',  ( 19.84674366389459621, 13.50893115100078568, 7.409399052514197653E-17 ) ) ;
#28382 = CARTESIAN_POINT ( 'NONE',  ( 17.39651004071838614, 47.93575266056826933, 6.500000000000032863 ) ) ;
#28383 = CARTESIAN_POINT ( 'NONE',  ( 10.00000000000000178, 38.05374883491396787, 14.16423886937410082 ) ) ;
#28384 = DIRECTION ( 'NONE',  ( 0.000000000000000000, 1.000000000000000000, 0.000000000000000000 ) ) ;
#28386 =( NAMED_UNIT ( * ) SI_UNIT ( $, .STERADIAN. ) SOLID_ANGLE_UNIT ( ) );
#28385 = CARTESIAN_POINT ( 'NONE',  ( -6.617417514236028531, -58.37570470593282579, -2.500000000000000000 ) ) ;
#28387 = CARTESIAN_POINT ( 'NONE',  ( 19.42250999205614193, 30.14701867748817321, 5.440088680355555262 ) ) ;
#28388 = CARTESIAN_POINT ( 'NONE',  ( 10.00000000000000000, 32.87363466993042493, -12.81628187352647608 ) ) ;
#28389 = CARTESIAN_POINT ( 'NONE',  ( 3.591859063236761518, 29.95696800326375708, 11.09922568453594849 ) ) ;
#28390 = CARTESIAN_POINT ( 'NONE',  ( -1.099225684535947600, 64.54030133659709634, 6.408140936763237150 ) ) ;
#28391 = ORIENTED_EDGE ( 'NONE', *, *, #41225, .F. ) ;
#28392 = DIRECTION ( 'NONE',  ( -0.000000000000000000, -0.000000000000000000, -1.000000000000000000 ) ) ;
#28393 = CARTESIAN_POINT ( 'NONE',  ( -10.53011945866294852, -98.59345040283277228, -4.000000000000000000 ) ) ;
#28394 = CARTESIAN_POINT ( 'NONE',  ( 10.00000000000000000, 30.55374883491397142, -14.16423886937410082 ) ) ;
#28395 = CARTESIAN_POINT ( 'NONE',  ( -2.266590686148945544, 7.220415501580634832, 7.082119434687048631 ) ) ;
#28396 = CARTESIAN_POINT ( 'NONE',  ( 10.00000000000000178, 4.313685344154837509, 10.88017736071110342 ) ) ;
#28397 = CARTESIAN_POINT ( 'NONE',  ( 4.559911319644449179, 28.89701867748817321, 9.422509992056141925 ) ) ;
#28398 = LINE ( 'NONE', #34901, #12744 ) ;
#28399 = CARTESIAN_POINT ( 'NONE',  ( 0.000000000000000000, 0.000000000000000000, 0.000000000000000000 ) ) ;
#28400 = CARTESIAN_POINT ( 'NONE',  ( 2.035157376598824452, 58.68868534415482685, 7.964842623401179544 ) ) ;
#28401 = CARTESIAN_POINT ( 'NONE',  ( 0.5774900079438607392, 48.48035201082150536, 5.440088680355550821 ) ) ;
#28402 = CARTESIAN_POINT ( 'NONE',  ( 16.40814093676323893, 10.79030133659708923, 11.09922568453595026 ) ) ;
#28403 = LINE ( 'NONE', #98413, #55472 ) ;
#28404 = LINE ( 'NONE', #95425, #19591 ) ;
#28405 = CARTESIAN_POINT ( 'NONE',  ( 10.00000000000000000, 19.75893115100078390, -9.846743663894594434 ) ) ;
#28406 = CARTESIAN_POINT ( 'NONE',  ( 2.035157376598822676, 37.43868534415484106, -7.964842623401177768 ) ) ;
#28407 = EDGE_CURVE ( 'NONE', #8981, #50127, #10981, .T. ) ;
#28408 = B_SPLINE_CURVE_WITH_KNOTS ( 'NONE', 3,
 ( #5377, #35852, #21352, #51844 ),
 .UNSPECIFIED., .F., .F.,
 ( 4, 4 ),
 ( 0.000000000000000000, 0.001060528352562004799 ),
 .UNSPECIFIED. ) ;
#28409 = CARTESIAN_POINT ( 'NONE',  ( 6.565887622018943937, 0.1653013365970866511, 12.81628187352647430 ) ) ;
#28410 = CARTESIAN_POINT ( 'NONE',  ( 17.20831665107776587, 19.13393115100078035, -7.208316651077762316 ) ) ;
#28411 = CARTESIAN_POINT ( 'NONE',  ( 3.591859063236763294, 53.29030133659708923, -11.09922568453595026 ) ) ;
#28412 = CARTESIAN_POINT ( 'NONE',  ( 0.1532563361054082862, 21.21726448433412315, 2.638427012816831674 ) ) ;
#28413 = ORIENTED_EDGE ( 'NONE', *, *, #97438, .T. ) ;
#28414 = CARTESIAN_POINT ( 'NONE',  ( 6.204703633549690345, 10.76208216824729824, -14.16423886937410259 ) ) ;
#28415 = CARTESIAN_POINT ( 'NONE',  ( 0.5774900079438590739, 22.64701867748817321, -5.440088680355550821 ) ) ;
#28417 = CARTESIAN_POINT ( 'NONE',  ( 24.16423886937409904, 29.09541550158063572, 3.795296366450317205 ) ) ;
#28416 = SURFACE_SIDE_STYLE ('',( #44886 ) ) ;
#28418 = CARTESIAN_POINT ( 'NONE',  ( 0.1532563361054100626, 25.80059781766744820, -2.638427012816831230 ) ) ;
#28419 = CARTESIAN_POINT ( 'NONE',  ( 15.44008868035555793, 21.39701867748817321, -9.422509992056140149 ) ) ;
#28420 = CARTESIAN_POINT ( 'NONE',  ( 4.559911319644449179, 7.230352010821505360, -9.422509992056141925 ) ) ;
#28421 = VERTEX_POINT ( 'NONE', #36585 ) ;
#28422 = CARTESIAN_POINT ( 'NONE',  ( 0.5774900079438590739, 22.64701867748817321, -5.440088680355550821 ) ) ;
#28423 = CARTESIAN_POINT ( 'NONE',  ( 10.00000000000000000, 31.81368534415483751, -10.88017736071110342 ) ) ;
#28425 = CARTESIAN_POINT ( 'NONE',  ( 12.91533473730992121, 39.52201867748817676, 10.88017736071110164 ) ) ;
#28424 = CARTESIAN_POINT ( 'NONE',  ( 0.2751277870542967463, 70.00000000000000000, -6.000000000000000000 ) ) ;
#28426 = ORIENTED_EDGE ( 'NONE', *, *, #47526, .T. ) ;
#28427 = CARTESIAN_POINT ( 'NONE',  ( 7.361572987183169658, 54.96726448433413026, -9.846743663894592657 ) ) ;
#28428 = CARTESIAN_POINT ( 'NONE',  ( 12.91533473730992121, 39.52201867748817676, 10.88017736071110164 ) ) ;
#28429 = CARTESIAN_POINT ( 'NONE',  ( 4.380000000000001670, 1.019547802438464768, 4.000000000000000000 ) ) ;
#28430 = FILL_AREA_STYLE ('',( #36432 ) ) ;
#28431 = CARTESIAN_POINT ( 'NONE',  ( 3.591859063236761518, 59.95696800326375353, 11.09922568453594849 ) ) ;
#28432 = CARTESIAN_POINT ( 'NONE',  ( 0.2751277870542980231, 9.366073187301308778, -6.500000000000002665 ) ) ;
#28433 = CARTESIAN_POINT ( 'NONE',  ( -4.164238869374099927, 37.01208216824731068, 3.795296366450308767 ) ) ;
#28434 = CARTESIAN_POINT ( 'NONE',  ( 17.96484262340118221, 56.18868534415484817, -7.964842623401177768 ) ) ;
#28435 = B_SPLINE_CURVE_WITH_KNOTS ( 'NONE', 3,
 ( #82305, #89809, #15323, #44797, #90798, #21829 ),
 .UNSPECIFIED., .F., .F.,
 ( 4, 2, 4 ),
 ( 0.000000000000000000, 0.0002626113303184787295, 0.0005252226606369574590 ),
 .UNSPECIFIED. ) ;
#28436 = DIRECTION ( 'NONE',  ( 0.2164396139380906914, 0.000000000000000000, 0.9762960071199361378 ) ) ;
#28437 = FACE_OUTER_BOUND ( 'NONE', #44516, .T. ) ;
#28439 = ADVANCED_FACE ( 'NONE', ( #46535 ), #83563, .T. ) ;
#28438 = CARTESIAN_POINT ( 'NONE',  ( 10.00000000000000178, 52.25893115100078745, 9.846743663894594434 ) ) ;
#28440 = CARTESIAN_POINT ( 'NONE',  ( 17.20831665107776587, 2.883931151000785231, 7.208316651077764980 ) ) ;
#28441 = VERTEX_POINT ( 'NONE', #65709 ) ;
#28442 = CARTESIAN_POINT ( 'NONE',  ( 17.20831665107776587, 24.13393115100078035, -7.208316651077762316 ) ) ;
#28443 = CARTESIAN_POINT ( 'NONE',  ( -6.408140936763232709, -25.04303199673624292, 11.09922568453595026 ) ) ;
#28444 = VECTOR ( 'NONE', #65099, 1000.000000000000000 ) ;
#28445 = CARTESIAN_POINT ( 'NONE',  ( 20.88017736071110519, 25.56368534415483751, 2.639326808657452039E-16 ) ) ;
#28446 = CARTESIAN_POINT ( 'NONE',  ( 14.92337183194729633, 27.67559781766745530, 8.527530157486181039 ) ) ;
#28447 = CARTESIAN_POINT ( 'NONE',  ( -1.099225684535947600, 9.540301336597087456, 6.408140936763237150 ) ) ;
#28448 = CARTESIAN_POINT ( 'NONE',  ( 15.44008868035555260, 54.73035201082150536, 9.422509992056143702 ) ) ;
#28450 = CARTESIAN_POINT ( 'NONE',  ( -1.099225684535947600, 53.70696800326376064, -6.408140936763238038 ) ) ;
#28449 = CARTESIAN_POINT ( 'NONE',  ( 7.084665262690076126, 32.02201867748816966, -10.88017736071110164 ) ) ;
#28451 = CARTESIAN_POINT ( 'NONE',  ( 20.36894250292379738, 44.92874883491396787, -10.36894250292379027 ) ) ;
#28452 = MECHANICAL_DESIGN_GEOMETRIC_PRESENTATION_REPRESENTATION (  '', ( #15696 ), #78052 ) ;
#28453 = EDGE_CURVE ( 'NONE', #51651, #89050, #64714, .T. ) ;
#28454 = AXIS2_PLACEMENT_3D ( 'NONE', #88562, #87091, #11099 ) ;
#28455 = B_SPLINE_CURVE_WITH_KNOTS ( 'NONE', 3,
 ( #10271, #28087, #51088, #93759, #88094, #65085 ),
 .UNSPECIFIED., .F., .F.,
 ( 4, 2, 4 ),
 ( 0.0002800267093036927718, 0.0006862322000113845692, 0.001092437690719076258 ),
 .UNSPECIFIED. ) ;
#28456 = CARTESIAN_POINT ( 'NONE',  ( -10.64017930668218881, 14.49999999999999112, 10.57291749337211151 ) ) ;
#28457 = EDGE_CURVE ( 'NONE', #18519, #74674, #60035, .T. ) ;
#28458 = ORIENTED_EDGE ( 'NONE', *, *, #66199, .T. ) ;
#28459 = CARTESIAN_POINT ( 'NONE',  ( 3.591859063236763294, 3.290301336597087012, -11.09922568453595026 ) ) ;
#28460 = CARTESIAN_POINT ( 'NONE',  ( 0.5774900079438607392, 8.480352010821505360, 5.440088680355550821 ) ) ;
#28461 = CARTESIAN_POINT ( 'NONE',  ( 0.5774900079438590739, 47.64701867748817676, -5.440088680355550821 ) ) ;
#28462 = CARTESIAN_POINT ( 'NONE',  ( 17.20831665107776587, 64.13393115100079456, -7.208316651077762316 ) ) ;
#28463 = ORIENTED_EDGE ( 'NONE', *, *, #92676, .T. ) ;
#28465 = DIRECTION ( 'NONE',  ( 1.000000000000000000, 0.000000000000000000, 0.000000000000000000 ) ) ;
#28464 = CARTESIAN_POINT ( 'NONE',  ( 10.00000000000000178, 12.25893115100078568, 9.846743663894594434 ) ) ;
#28466 = CARTESIAN_POINT ( 'NONE',  ( 4.559911319644449179, 57.23035201082150536, -9.422509992056141925 ) ) ;
#28467 = CARTESIAN_POINT ( 'NONE',  ( 0.1532563361054083140, 31.00893115100078390, 1.131784320476157264E-15 ) ) ;
#28468 = CARTESIAN_POINT ( 'NONE',  ( 19.84674366389459266, 18.30059781766745175, 2.638427012816836559 ) ) ;
#28469 = CARTESIAN_POINT ( 'NONE',  ( 1.472469842513823179, 20.59226448433411960, -4.923371831947296329 ) ) ;
#28470 = CARTESIAN_POINT ( 'NONE',  ( 0.2751277870542875315, 65.30223176428830811, 6.499999999999984901 ) ) ;
#28472 = CARTESIAN_POINT ( 'NONE',  ( -0.1503990784575280903, 23.10158574516642815, 6.262539305110076171 ) ) ;
#28471 = CARTESIAN_POINT ( 'NONE',  ( 15.44008868035555793, 66.39701867748817676, -9.422509992056140149 ) ) ;
#28474 = VERTEX_POINT ( 'NONE', #79743 ) ;
#28473 = CARTESIAN_POINT ( 'NONE',  ( 1.472469842513823179, 30.59226448433411960, -4.923371831947296329 ) ) ;
#28475 = CARTESIAN_POINT ( 'NONE',  ( 7.185089000015947747, -80.58569572050201657, 3.999999999999999112 ) ) ;
#28477 = ADVANCED_FACE ( 'NONE', ( #73209 ), #41554, .T. ) ;
#28476 = CARTESIAN_POINT ( 'NONE',  ( 19.38216949554541557, 2.248634669930420049, -9.382169495545420901 ) ) ;
#28478 = CARTESIAN_POINT ( 'NONE',  ( 2.035157376598822676, 2.438685344154837953, -7.964842623401177768 ) ) ;
#28479 = CARTESIAN_POINT ( 'NONE',  ( 17.08211943468705130, 18.47041550158063572, 12.26659068614894998 ) ) ;
#28480 = UNCERTAINTY_MEASURE_WITH_UNIT (LENGTH_MEASURE( 1.000000000000000082E-05 ), #90379, 'distance_accuracy_value', 'NONE');
#28481 = CARTESIAN_POINT ( 'NONE',  ( 11.62719953690058361, 0.5000000000000004441, 9.476720473301874392 ) ) ;
#28482 = ADVANCED_FACE ( 'NONE', ( #18759 ), #26733, .T. ) ;
#28483 = CARTESIAN_POINT ( 'NONE',  ( 6.204703633549690345, 15.76208216824730179, -14.16423886937410259 ) ) ;
#28484 = CARTESIAN_POINT ( 'NONE',  ( -0.3689425029237881626, 42.42874883491396787, 10.36894250292379027 ) ) ;
#28485 = CARTESIAN_POINT ( 'NONE',  ( -4.164238869374098151, 1.595415501580634388, -3.795296366450310543 ) ) ;
#28487 = CARTESIAN_POINT ( 'NONE',  ( 3.969999999999999751, 10.25000000000000000, -3.750000000000000000 ) ) ;
#28486 = CARTESIAN_POINT ( 'NONE',  ( -4.164238869374099039, 11.80374883491396965, 8.674139862899312516E-16 ) ) ;
#28488 = CARTESIAN_POINT ( 'NONE',  ( 12.91533473730993009, 46.60535201082150536, -10.88017736071109987 ) ) ;
#28489 = FACE_OUTER_BOUND ( 'NONE', #29284, .T. ) ;
#28490 = ORIENTED_EDGE ( 'NONE', *, *, #39969, .F. ) ;
#28491 = CARTESIAN_POINT ( 'NONE',  ( 5.076628168052703671, 26.84226448433411960, 8.527530157486179263 ) ) ;
#28493 = CARTESIAN_POINT ( 'NONE',  ( 1.472469842513823179, 25.59226448433412315, -4.923371831947296329 ) ) ;
#28492 = CARTESIAN_POINT ( 'NONE',  ( 0.5774900079438607392, 68.48035201082150536, 5.440088680355550821 ) ) ;
#28494 = CARTESIAN_POINT ( 'NONE',  ( 0.5774900079438607392, 8.480352010821505360, 5.440088680355550821 ) ) ;
#28495 = CARTESIAN_POINT ( 'NONE',  ( 6.565887622018943937, 55.16530133659709634, 12.81628187352647430 ) ) ;
#28496 = CARTESIAN_POINT ( 'NONE',  ( 12.63842701281683034, 52.46726448433413026, 9.846743663894596210 ) ) ;
#28497 = CARTESIAN_POINT ( 'NONE',  ( 0.000000000000000000, 14.49999999999999822, 0.000000000000000000 ) ) ;
#28498 = CARTESIAN_POINT ( 'NONE',  ( 2.791683348922240793, 26.63393115100078745, 7.208316651077764092 ) ) ;
#28499 = CARTESIAN_POINT ( 'NONE',  ( -1.099225684535947600, 43.70696800326375353, -6.408140936763238038 ) ) ;
#28500 = CARTESIAN_POINT ( 'NONE',  ( -7.082119434687058401, -19.02958449841936428, -12.26659068614894110 ) ) ;
#28501 = CARTESIAN_POINT ( 'NONE',  ( 12.91533473730993009, 41.60535201082149825, -10.88017736071109987 ) ) ;
#28502 = CARTESIAN_POINT ( 'NONE',  ( 19.84674366389459266, 38.71726448433412315, -2.638427012816827677 ) ) ;
#28503 = CARTESIAN_POINT ( 'NONE',  ( 10.00000000000000000, 25.55374883491396787, -14.16423886937410082 ) ) ;
#28504 = VERTEX_POINT ( 'NONE', #6212 ) ;
#28505 = CARTESIAN_POINT ( 'NONE',  ( -2.266590686148945544, 6.387082168247300906, -7.082119434687050408 ) ) ;
#28506 = CARTESIAN_POINT ( 'NONE',  ( 10.00000000000000000, 46.81368534415484106, -10.88017736071110342 ) ) ;
#28507 = CARTESIAN_POINT ( 'NONE',  ( 20.88017736071110164, 65.35535201082150536, 2.915334737309930979 ) ) ;
#28508 = CARTESIAN_POINT ( 'NONE',  ( 24.16423886937410614, 49.30374883491396787, 8.672049930838204340E-16 ) ) ;
#28509 = CARTESIAN_POINT ( 'NONE',  ( 17.20831665107776587, 62.88393115100078745, 7.208316651077764980 ) ) ;
#28510 = FACE_OUTER_BOUND ( 'NONE', #93710, .T. ) ;
#28511 = CARTESIAN_POINT ( 'NONE',  ( 20.88017736071110875, 60.77201867748817676, -2.915334737309920765 ) ) ;
#28512 = CARTESIAN_POINT ( 'NONE',  ( -6.871316085749034741, -73.24163895400424451, -2.500000000000000000 ) ) ;
#28513 = CARTESIAN_POINT ( 'NONE',  ( 19.38216949554541557, 22.24863466993041428, -9.382169495545420901 ) ) ;
#28514 = CARTESIAN_POINT ( 'NONE',  ( 18.52753015748618282, 63.92559781766745886, -4.923371831947291888 ) ) ;
#28515 = CARTESIAN_POINT ( 'NONE',  ( -5.204170427930421283E-15, 26.81368534415484817, -10.88017736071110342 ) ) ;
#28516 = CARTESIAN_POINT ( 'NONE',  ( 4.559911319644449179, 18.89701867748817321, 9.422509992056141925 ) ) ;
#28517 = CARTESIAN_POINT ( 'NONE',  ( 19.42250999205614548, 5.980352010821504471, -5.440088680355545492 ) ) ;
#28518 = FACE_OUTER_BOUND ( 'NONE', #65681, .T. ) ;
#28519 = VERTEX_POINT ( 'NONE', #97235 ) ;
#28520 = CARTESIAN_POINT ( 'NONE',  ( 20.88017736071110164, 5.355352010821502695, 2.915334737309930979 ) ) ;
#28521 = EDGE_CURVE ( 'NONE', #24774, #3863, #30174, .T. ) ;
#28522 = AXIS2_PLACEMENT_3D ( 'NONE', #71274, #55774, #24304 ) ;
#28523 = CARTESIAN_POINT ( 'NONE',  ( 1.472469842513823179, 6.425597817667451750, 4.923371831947296329 ) ) ;
#28524 = CARTESIAN_POINT ( 'NONE',  ( 2.791683348922237240, 35.38393115100079456, -7.208316651077763204 ) ) ;
#28525 = CARTESIAN_POINT ( 'NONE',  ( 17.96484262340118221, 41.18868534415484106, -7.964842623401177768 ) ) ;
#28526 = CARTESIAN_POINT ( 'NONE',  ( 6.565887622018943937, 3.081968003263753531, -12.81628187352647608 ) ) ;
#28528 = DIRECTION ( 'NONE',  ( -0.6225146366376237417, 0.000000000000000000, 0.7826081568524104748 ) ) ;
#28527 = CARTESIAN_POINT ( 'NONE',  ( 10.00000000000000178, 39.31368534415484106, 10.88017736071110342 ) ) ;
#28529 = CARTESIAN_POINT ( 'NONE',  ( 13.43411237798105340, 55.58196800326374643, 12.81628187352647963 ) ) ;
#28530 = ORIENTED_EDGE ( 'NONE', *, *, #44833, .F. ) ;
#28531 = CARTESIAN_POINT ( 'NONE',  ( -0.8801773607110991993, 62.85535201082150536, -2.915334737309923874 ) ) ;
#28533 = CARTESIAN_POINT ( 'NONE',  ( 17.08211943468705130, 8.470415501580635720, 12.26659068614894998 ) ) ;
#28532 = CARTESIAN_POINT ( 'NONE',  ( -2.816281873526473856, 29.12363466993041783, 9.499525473075851096E-16 ) ) ;
#28534 = CARTESIAN_POINT ( 'NONE',  ( 1.472469842513823179, 1.425597817667451528, 4.923371831947296329 ) ) ;
#28535 = CARTESIAN_POINT ( 'NONE',  ( -0.8801773607111008646, 38.27201867748816255, 2.915334737309923430 ) ) ;
#28536 = CARTESIAN_POINT ( 'NONE',  ( 13.34343830728399283, 15.00000000000000000, 6.852200678592689442 ) ) ;
#28537 = CARTESIAN_POINT ( 'NONE',  ( -4.164238869374098151, 61.59541550158063217, -3.795296366450310543 ) ) ;
#28538 = CARTESIAN_POINT ( 'NONE',  ( 17.20831665107776587, 59.13393115100078745, -7.208316651077762316 ) ) ;
#28539 = CARTESIAN_POINT ( 'NONE',  ( 14.92337183194729988, 19.34226448433411960, -8.527530157486177487 ) ) ;
#28540 = CIRCLE ( 'NONE', #79634, 15.00000000000000000 ) ;
#28541 = CARTESIAN_POINT ( 'NONE',  ( 2.035157376598824452, 68.68868534415484817, 7.964842623401179544 ) ) ;
#28542 = DIRECTION ( 'NONE',  ( -0.6087614290087131064, 0.000000000000000000, -0.7933533402912409382 ) ) ;
#28543 = CARTESIAN_POINT ( 'NONE',  ( 22.26659068614895176, 34.72041550158063927, -7.082119434687042414 ) ) ;
#28544 =( BOUNDED_SURFACE ( )  B_SPLINE_SURFACE ( 3, 2, ( 
 ( #15299, #60278, #38286 ),
 ( #52774, #76275, #13799 ),
 ( #794, #46272, #76757 ),
 ( #8275, #59780, #31247 ),
 ( #51796, #74789, #36800 ),
 ( #67294, #97821, #63712 ),
 ( #32231, #85749, #85255 ),
 ( #17261, #55746, #64199 ),
 ( #16270, #25262, #70259 ),
 ( #71724, #2764, #18235 ),
 ( #3233, #62732, #9746 ),
 ( #32726, #31744, #1291 ),
 ( #47736, #40737, #62240 ),
 ( #93232, #23785, #54250 ),
 ( #33219, #8755, #16763 ),
 ( #92746, #86733, #78233 ),
 ( #24757, #55235, #48716 ),
 ( #24270, #40248, #41248 ),
 ( #33699, #70756, #94216 ),
 ( #2270, #84762, #25746 ),
 ( #93729, #54736, #63224 ),
 ( #46752, #47236, #86237 ) ),
 .UNSPECIFIED., .F., .F., .T. ) 
 B_SPLINE_SURFACE_WITH_KNOTS ( ( 4, 2, 2, 2, 2, 2, 2, 2, 2, 2, 4 ),
 ( 3, 3 ),
 ( -1.040834085586084257E-17, 0.002789288213736764842, 0.005578576427473540093, 0.01115715285494709059, 0.02231430570989419160, 0.03347145856484129434, 0.04462861141978839707, 0.06694291712968260255, 0.07810006998462970529, 0.08367864641210326360, 0.08925722283957680803 ),
 ( 0.000000000000000000, 1.000000000000000000 ),
 .UNSPECIFIED. ) 
 GEOMETRIC_REPRESENTATION_ITEM ( )  RATIONAL_B_SPLINE_SURFACE ( (
 ( 1.000000000000000000, 0.7071067811865482389, 1.000000000000000000),
 ( 1.000000000000000000, 0.7071067811865482389, 1.000000000000000000),
 ( 1.000000000000000000, 0.7071067811865493491, 1.000000000000000000),
 ( 1.000000000000000000, 0.7071067811865493491, 1.000000000000000000),
 ( 1.000000000000000000, 0.7071067811865475727, 1.000000000000000000),
 ( 1.000000000000000000, 0.7071067811865475727, 1.000000000000000000),
 ( 1.000000000000000000, 0.7071067811865475727, 1.000000000000000000),
 ( 1.000000000000000000, 0.7071067811865475727, 1.000000000000000000),
 ( 1.000000000000000000, 0.7071067811865487940, 1.000000000000000000),
 ( 1.000000000000000000, 0.7071067811865487940, 1.000000000000000000),
 ( 1.000000000000000000, 0.7071067811865475727, 1.000000000000000000),
 ( 1.000000000000000000, 0.7071067811865475727, 1.000000000000000000),
 ( 1.000000000000000000, 0.7071067811865487940, 1.000000000000000000),
 ( 1.000000000000000000, 0.7071067811865487940, 1.000000000000000000),
 ( 1.000000000000000000, 0.7071067811865463515, 1.000000000000000000),
 ( 1.000000000000000000, 0.7071067811865463515, 1.000000000000000000),
 ( 1.000000000000000000, 0.7071067811865456854, 1.000000000000000000),
 ( 1.000000000000000000, 0.7071067811865456854, 1.000000000000000000),
 ( 1.000000000000000000, 0.7071067811865475727, 1.000000000000000000),
 ( 1.000000000000000000, 0.7071067811865475727, 1.000000000000000000),
 ( 1.000000000000000000, 0.7071067811865475727, 1.000000000000000000),
 ( 1.000000000000000000, 0.7071067811865475727, 1.000000000000000000) ) ) 
 REPRESENTATION_ITEM ( '' )  SURFACE ( )  );
#28545 = LINE ( 'NONE', #89542, #5863 ) ;
#28546 = CARTESIAN_POINT ( 'NONE',  ( 11.27041535450084631, -90.94092909150046466, -3.750000000000000000 ) ) ;
#28547 = CARTESIAN_POINT ( 'NONE',  ( 19.67388390623025529, 87.39738367702956623, -5.439653449514034733 ) ) ;
#28548 = ORIENTED_EDGE ( 'NONE', *, *, #83671, .T. ) ;
#28549 = CARTESIAN_POINT ( 'NONE',  ( -4.164238869374099927, 57.01208216824731068, 3.795296366450308767 ) ) ;
#28550 = CARTESIAN_POINT ( 'NONE',  ( 2.035157376598824452, 3.688685344154837953, 7.964842623401179544 ) ) ;
#28551 = CARTESIAN_POINT ( 'NONE',  ( 19.84674366389459621, 33.50893115100078745, 7.409399052514197653E-17 ) ) ;
#28552 = CARTESIAN_POINT ( 'NONE',  ( 4.180366052176858638, 15.00000000000000711, -14.01545757926328584 ) ) ;
#28553 = CARTESIAN_POINT ( 'NONE',  ( -0.2418659066527630297, 43.09014588040357552, 6.114288769123057854 ) ) ;
#28554 = CARTESIAN_POINT ( 'NONE',  ( 2.035157376598822676, 12.43868534415483751, -7.964842623401177768 ) ) ;
#28555 = CARTESIAN_POINT ( 'NONE',  ( -4.164238869374099927, 57.01208216824731068, 3.795296366450308767 ) ) ;
#28556 = CARTESIAN_POINT ( 'NONE',  ( 18.52753015748617571, 33.09226448433411605, 4.923371831947298993 ) ) ;
#28557 = CARTESIAN_POINT ( 'NONE',  ( 13.99999999999999822, 60.50000000000000000, 5.000000000000000000 ) ) ;
#28558 = CARTESIAN_POINT ( 'NONE',  ( 19.84674366389459266, 3.300597817667451750, 2.638427012816836559 ) ) ;
#28559 = CARTESIAN_POINT ( 'NONE',  ( 18.04007052943773104, 4.002578601053487617, -5.767676674365832312 ) ) ;
#28560 = CARTESIAN_POINT ( 'NONE',  ( 2.638427012816835227, 22.46726448433412315, 9.846743663894590881 ) ) ;
#28561 = VERTEX_POINT ( 'NONE', #66711 ) ;
#28562 = EDGE_LOOP ( 'NONE', ( #6185, #77661, #54555, #98607 ) ) ;
#28563 = EDGE_CURVE ( 'NONE', #92892, #52439, #77915, .T. ) ;
#28564 = ORIENTED_EDGE ( 'NONE', *, *, #93242, .T. ) ;
#28565 = CARTESIAN_POINT ( 'NONE',  ( 12.63842701281683034, 42.46726448433412315, 9.846743663894596210 ) ) ;
#28566 = CARTESIAN_POINT ( 'NONE',  ( 10.00000000000000178, 18.05374883491396787, 14.16423886937410082 ) ) ;
#28568 = CARTESIAN_POINT ( 'NONE',  ( 2.035157376598824452, 28.68868534415484106, 7.964842623401179544 ) ) ;
#28567 = CARTESIAN_POINT ( 'NONE',  ( 0.5774900079438590739, 17.64701867748817321, -5.440088680355550821 ) ) ;
#28570 = CARTESIAN_POINT ( 'NONE',  ( 3.591859063236763294, 18.29030133659708568, -11.09922568453595026 ) ) ;
#28569 = CARTESIAN_POINT ( 'NONE',  ( 14.92337183194729633, 57.67559781766745886, 8.527530157486181039 ) ) ;
#28571 = CARTESIAN_POINT ( 'NONE',  ( -2.266590686148945544, 2.220415501580634388, 7.082119434687048631 ) ) ;
#28572 = EDGE_CURVE ( 'NONE', #44777, #1179, #28540, .T. ) ;
#28573 = CARTESIAN_POINT ( 'NONE',  ( 16.40814093676324603, 37.45696800326376064, -11.09922568453594671 ) ) ;
#28574 = EDGE_CURVE ( 'NONE', #11231, #44163, #68202, .T. ) ;
#28575 = EDGE_LOOP ( 'NONE', ( #28614, #87497, #68562, #81339 ) ) ;
#28576 = CARTESIAN_POINT ( 'NONE',  ( 7.361572987183170547, 27.05059781766745175, 9.846743663894590881 ) ) ;
#28577 = CARTESIAN_POINT ( 'NONE',  ( 4.559911319644449179, 3.897018677488171434, 9.422509992056141925 ) ) ;
#28578 = ORIENTED_EDGE ( 'NONE', *, *, #9865, .T. ) ;
#28579 = CARTESIAN_POINT ( 'NONE',  ( 10.00000000000000178, 68.05374883491397497, 14.16423886937410082 ) ) ;
#28580 = ORIENTED_EDGE ( 'NONE', *, *, #73737, .T. ) ;
#28581 = CARTESIAN_POINT ( 'NONE',  ( 10.00000000000000178, 44.31368534415484106, 10.88017736071110342 ) ) ;
#28582 = CARTESIAN_POINT ( 'NONE',  ( 2.035157376598822676, 62.43868534415483396, -7.964842623401177768 ) ) ;
#28583 = CIRCLE ( 'NONE', #55779, 14.49999999999999822 ) ;
#28584 = CARTESIAN_POINT ( 'NONE',  ( 2.035157376598824452, 53.68868534415484817, 7.964842623401179544 ) ) ;
#28585 = CARTESIAN_POINT ( 'NONE',  ( 7.084665262690076126, 37.02201867748817676, -10.88017736071110164 ) ) ;
#28586 = CARTESIAN_POINT ( 'NONE',  ( -1.926860441876562025, 29.47997603579417358, -3.195792623639529761 ) ) ;
#28587 = STYLED_ITEM ( 'NONE', ( #84534 ), #60633 ) ;
#28588 = CIRCLE ( 'NONE', #84492, 14.49999999999999822 ) ;
#28589 = VERTEX_POINT ( 'NONE', #20723 ) ;
#28590 = CARTESIAN_POINT ( 'NONE',  ( 5.076628168052704559, 35.17559781766745175, -8.527530157486179263 ) ) ;
#28591 = EDGE_LOOP ( 'NONE', ( #14742, #97207, #21806, #48206 ) ) ;
#28592 = CARTESIAN_POINT ( 'NONE',  ( 19.84674366389459621, 58.50893115100078745, 7.409399052514197653E-17 ) ) ;
#28593 = CARTESIAN_POINT ( 'NONE',  ( 20.15039907845753220, 40.60158574516643171, -6.262539305110077947 ) ) ;
#28594 = EDGE_CURVE ( 'NONE', #21190, #15328, #97732, .T. ) ;
#28595 = CARTESIAN_POINT ( 'NONE',  ( -4.164238869374099927, 7.012082168247302683, 3.795296366450308767 ) ) ;
#28596 = VERTEX_POINT ( 'NONE', #74191 ) ;
#28597 = CARTESIAN_POINT ( 'NONE',  ( 19.39188664607695856, 50.83703382326398668, -6.499999999999941380 ) ) ;
#28598 = CARTESIAN_POINT ( 'NONE',  ( -3.888850863501575716, -8.270211729787575905, 3.750000000000000888 ) ) ;
#28599 = CARTESIAN_POINT ( 'NONE',  ( 0.1532563361054082862, 36.21726448433410894, 2.638427012816831674 ) ) ;
#28600 = CARTESIAN_POINT ( 'NONE',  ( 17.08211943468705130, 58.47041550158063927, 12.26659068614894998 ) ) ;
#28601 = PLANE ( 'NONE',  #40304 ) ;
#28602 = ORIENTED_EDGE ( 'NONE', *, *, #15726, .T. ) ;
#28603 = CARTESIAN_POINT ( 'NONE',  ( -8.731067818237029599, 5.313309369127510173, 8.731067818237042033 ) ) ;
#28604 = CARTESIAN_POINT ( 'NONE',  ( 12.63842701281683922, 49.55059781766744464, -9.846743663894590881 ) ) ;
#28605 = LINE ( 'NONE', #90088, #25951 ) ;
#28606 = CARTESIAN_POINT ( 'NONE',  ( 3.591859063236761518, 24.95696800326375353, 11.09922568453594849 ) ) ;
#28607 = CARTESIAN_POINT ( 'NONE',  ( 5.076628168052703671, 6.842264484334118713, 8.527530157486179263 ) ) ;
#28608 = CYLINDRICAL_SURFACE ( 'NONE', #32948, 11.92686044187656513 ) ;
#28609 = CARTESIAN_POINT ( 'NONE',  ( 19.84674366389459621, 13.50893115100078568, 7.409399052514197653E-17 ) ) ;
#28610 = CARTESIAN_POINT ( 'NONE',  ( 10.00000000000000000, 7.873634669930421381, -12.81628187352647608 ) ) ;
#28611 = ADVANCED_FACE ( 'NONE', ( #5724 ), #13709, .T. ) ;
#28612 = CARTESIAN_POINT ( 'NONE',  ( -6.382347221874519860, 0.3640475087720974057, 13.57444820018223908 ) ) ;
#28613 = B_SPLINE_CURVE_WITH_KNOTS ( 'NONE', 3,
 ( #62460, #84497, #1010, #536, #38507, #24496 ),
 .UNSPECIFIED., .F., .F.,
 ( 4, 2, 4 ),
 ( 0.0002800760588349493702, 0.0006862820326512249040, 0.001092488006467500329 ),
 .UNSPECIFIED. ) ;
#28614 = ORIENTED_EDGE ( 'NONE', *, *, #30245, .T. ) ;
#28615 = CARTESIAN_POINT ( 'NONE',  ( 19.42250999205614548, 10.98035201082150536, -5.440088680355545492 ) ) ;
#28616 = CARTESIAN_POINT ( 'NONE',  ( 20.36894250292379738, 9.928748834913966093, -10.36894250292379027 ) ) ;
#28617 = CARTESIAN_POINT ( 'NONE',  ( 7.361572987183169658, 24.96726448433412315, -9.846743663894592657 ) ) ;
#28618 = CARTESIAN_POINT ( 'NONE',  ( 10.00000000000000178, 59.31368534415484106, 10.88017736071110342 ) ) ;
#28620 = CARTESIAN_POINT ( 'NONE',  ( -3.530007528296587704, -1.230351260576522110, -3.750000000000000000 ) ) ;
#28619 = CARTESIAN_POINT ( 'NONE',  ( 3.591859063236763294, 33.29030133659708213, -11.09922568453595026 ) ) ;
#28621 = CARTESIAN_POINT ( 'NONE',  ( 17.96484262340118221, 19.93868534415484106, 7.964842623401181321 ) ) ;
#28622 = DIRECTION ( 'NONE',  ( 0.6755902076156493630, 0.000000000000000000, 0.7372773368101340763 ) ) ;
#28623 = DIRECTION ( 'NONE',  ( 0.9890158633619168249, -0.000000000000000000, 0.1478094111296113511 ) ) ;
#28624 = CARTESIAN_POINT ( 'NONE',  ( 5.076628168052704559, 60.17559781766745175, -8.527530157486179263 ) ) ;
#28625 = CARTESIAN_POINT ( 'NONE',  ( 19.84674366389459266, 13.30059781766745353, 2.638427012816836559 ) ) ;
#28626 = CARTESIAN_POINT ( 'NONE',  ( -10.88017736071110342, -26.93631465584515894, 3.903127820947815962E-15 ) ) ;
#28627 = CARTESIAN_POINT ( 'NONE',  ( 22.81628187352648496, 31.83196800326375353, -3.434112377981050290 ) ) ;
#28628 = CARTESIAN_POINT ( 'NONE',  ( 1.821708436314909196, 51.66792564121896447, -6.499999999999929834 ) ) ;
#28630 = LINE ( 'NONE', #97651, #6499 ) ;
#28629 = CARTESIAN_POINT ( 'NONE',  ( 20.88017736071110164, 35.35535201082150536, 2.915334737309930979 ) ) ;
#28631 = CARTESIAN_POINT ( 'NONE',  ( 14.35840480524206697, 14.49999999999999112, -4.340070442838847242 ) ) ;
#28632 = CARTESIAN_POINT ( 'NONE',  ( 19.42250999205614193, 25.14701867748817321, 5.440088680355555262 ) ) ;
#28633 = CARTESIAN_POINT ( 'NONE',  ( 17.96484262340118221, 34.93868534415482685, 7.964842623401181321 ) ) ;
#28634 = CARTESIAN_POINT ( 'NONE',  ( 7.361572987183169658, 49.96726448433410894, -9.846743663894592657 ) ) ;
#28635 = CARTESIAN_POINT ( 'NONE',  ( 17.96484262340118221, 54.93868534415484106, 7.964842623401181321 ) ) ;
#28636 = CARTESIAN_POINT ( 'NONE',  ( 2.917880565312948704, 37.63708216824731068, 12.26659068614894643 ) ) ;
#28637 = CARTESIAN_POINT ( 'NONE',  ( 12.63842701281683922, 39.55059781766744464, -9.846743663894590881 ) ) ;
#28638 = FACE_OUTER_BOUND ( 'NONE', #52712, .T. ) ;
#28639 = CARTESIAN_POINT ( 'NONE',  ( 3.591859063236763294, 3.290301336597087012, -11.09922568453595026 ) ) ;
#28640 = ORIENTED_EDGE ( 'NONE', *, *, #68773, .T. ) ;
#28641 = CARTESIAN_POINT ( 'NONE',  ( 12.91533473730992121, 19.52201867748816611, 10.88017736071110164 ) ) ;
#28642 = CYLINDRICAL_SURFACE ( 'NONE', #58962, 0.2500000000000002220 ) ;
#28643 = CARTESIAN_POINT ( 'NONE',  ( 7.084665262690076126, 17.02201867748817676, -10.88017736071110164 ) ) ;
#28644 = CARTESIAN_POINT ( 'NONE',  ( 19.42250999205614193, 65.14701867748817676, 5.440088680355555262 ) ) ;
#28645 = CARTESIAN_POINT ( 'NONE',  ( 6.204703633549690345, 22.84541550158062861, 14.16423886937410082 ) ) ;
#28646 = EDGE_CURVE ( 'NONE', #58305, #2418, #89209, .T. ) ;
#28647 = CARTESIAN_POINT ( 'NONE',  ( 7.361572987183169658, 14.96726448433411960, -9.846743663894592657 ) ) ;
#28648 = CARTESIAN_POINT ( 'NONE',  ( 0.1532563361054082862, 66.21726448433413736, 2.638427012816831674 ) ) ;
#28649 = CARTESIAN_POINT ( 'NONE',  ( 4.559911319644449179, 48.89701867748817676, 9.422509992056141925 ) ) ;
#28650 = CARTESIAN_POINT ( 'NONE',  ( 8.606322355898619492, 15.00000000000000000, -11.66967075399251996 ) ) ;
#28651 = CARTESIAN_POINT ( 'NONE',  ( 20.00000000000000000, 0.000000000000000000, 5.000000000000000000 ) ) ;
#28652 = ADVANCED_FACE ( 'NONE', ( #74702 ), #21718, .T. ) ;
#28653 = ORIENTED_EDGE ( 'NONE', *, *, #91547, .T. ) ;
#28654 = CARTESIAN_POINT ( 'NONE',  ( -6.689969769698787871, -0.03417435944610275333, -12.58200319823979285 ) ) ;
#28655 = CARTESIAN_POINT ( 'NONE',  ( 1.472469842513823179, 45.59226448433412315, -4.923371831947296329 ) ) ;
#28656 = ORIENTED_EDGE ( 'NONE', *, *, #43887, .T. ) ;
#28657 = VERTEX_POINT ( 'NONE', #52200 ) ;
#28658 = CARTESIAN_POINT ( 'NONE',  ( -14.88232117145528655, 0.5000000000000004441, -1.875237731503337946 ) ) ;
#28659 = CARTESIAN_POINT ( 'NONE',  ( 24.16423886937410614, 24.30374883491396787, 8.672049930838204340E-16 ) ) ;
#28660 = CARTESIAN_POINT ( 'NONE',  ( -4.164238869374098151, 21.59541550158063217, -3.795296366450310543 ) ) ;
#28661 = CARTESIAN_POINT ( 'NONE',  ( 19.42250999205614193, 60.14701867748817676, 5.440088680355555262 ) ) ;
#28662 = CARTESIAN_POINT ( 'NONE',  ( 20.36894250292379738, 49.92874883491396787, -10.36894250292379027 ) ) ;
#28663 = CARTESIAN_POINT ( 'NONE',  ( 7.361572987183169658, 64.96726448433412315, -9.846743663894592657 ) ) ;
#28664 = CARTESIAN_POINT ( 'NONE',  ( 2.791683348922237240, 45.38393115100079456, -7.208316651077763204 ) ) ;
#28665 = PRESENTATION_STYLE_ASSIGNMENT (( #20182 ) ) ;
#28667 = CARTESIAN_POINT ( 'NONE',  ( 16.40814093676324603, 7.456968003263754419, -11.09922568453594671 ) ) ;
#28666 = CARTESIAN_POINT ( 'NONE',  ( 20.88017736071110875, 50.77201867748817676, -2.915334737309920765 ) ) ;
#28668 = CARTESIAN_POINT ( 'NONE',  ( 2.917880565312950480, 20.97041550158063217, -12.26659068614894821 ) ) ;
#28669 = CARTESIAN_POINT ( 'NONE',  ( 17.08211943468705840, 55.13708216824731068, -12.26659068614894466 ) ) ;
#28670 = CARTESIAN_POINT ( 'NONE',  ( -0.8801773607110991993, 17.85535201082150536, -2.915334737309923874 ) ) ;
#28671 = B_SPLINE_CURVE_WITH_KNOTS ( 'NONE', 3,
 ( #97182, #14159, #75136, #37159 ),
 .UNSPECIFIED., .F., .F.,
 ( 4, 4 ),
 ( 6.254634441385501671E-17, 0.001060528352562000462 ),
 .UNSPECIFIED. ) ;
#28672 = CARTESIAN_POINT ( 'NONE',  ( 20.32896413005680714, 5.578790035174471029, -5.963430220938276349 ) ) ;
#28673 = CARTESIAN_POINT ( 'NONE',  ( 0.5774900079438590739, 47.64701867748817676, -5.440088680355550821 ) ) ;
#28674 = CARTESIAN_POINT ( 'NONE',  ( -4.923371831947292776, -18.15773551566587685, 8.527530157486181039 ) ) ;
#28675 = ORIENTED_EDGE ( 'NONE', *, *, #17613, .T. ) ;
#28676 = DIRECTION ( 'NONE',  ( -0.000000000000000000, -1.000000000000000000, -0.000000000000000000 ) ) ;
#28677 = VERTEX_POINT ( 'NONE', #29679 ) ;
#28678 = ORIENTED_EDGE ( 'NONE', *, *, #44876, .F. ) ;
#28679 = CARTESIAN_POINT ( 'NONE',  ( 22.26659068614895176, 39.72041550158063217, -7.082119434687042414 ) ) ;
#28680 = CARTESIAN_POINT ( 'NONE',  ( 18.52753015748617571, 48.09226448433412315, 4.923371831947298993 ) ) ;
#28681 = DIRECTION ( 'NONE',  ( 0.000000000000000000, 0.000000000000000000, 1.000000000000000000 ) ) ;
#28682 = CARTESIAN_POINT ( 'NONE',  ( 6.767445849361153343, 0.5000000000000004441, 13.38662304974501360 ) ) ;
#28683 = CARTESIAN_POINT ( 'NONE',  ( 4.559911319644449179, 48.89701867748817676, 9.422509992056141925 ) ) ;
#28684 = EDGE_CURVE ( 'NONE', #21166, #51739, #73115, .T. ) ;
#28685 = B_SPLINE_CURVE_WITH_KNOTS ( 'NONE', 3,
 ( #47615, #33576, #10603, #32098, #33094, #48588 ),
 .UNSPECIFIED., .F., .F.,
 ( 4, 2, 4 ),
 ( 0.000000000000000000, 0.0002701661927229335471, 0.0005403323854458670942 ),
 .UNSPECIFIED. ) ;
#28686 = CARTESIAN_POINT ( 'NONE',  ( 19.38216949554541202, 60.99863466993042493, 9.382169495545424454 ) ) ;
#28687 = CARTESIAN_POINT ( 'NONE',  ( 3.434112377981054287, 7.665301336597081239, -12.81628187352647608 ) ) ;
#28688 = ADVANCED_FACE ( 'NONE', ( #6701 ), #84432, .T. ) ;
#28689 = ORIENTED_EDGE ( 'NONE', *, *, #61551, .F. ) ;
#28690 = CARTESIAN_POINT ( 'NONE',  ( -0.3689425029237881626, 37.42874883491396787, 10.36894250292379027 ) ) ;
#28691 = CARTESIAN_POINT ( 'NONE',  ( 21.09922568453594849, 26.20696800326375353, 6.408140936763242479 ) ) ;
#28692 = ORIENTED_EDGE ( 'NONE', *, *, #18588, .F. ) ;
#28693 = CARTESIAN_POINT ( 'NONE',  ( 21.09922568453594849, 41.20696800326375353, 6.408140936763242479 ) ) ;
#28694 = MECHANICAL_DESIGN_GEOMETRIC_PRESENTATION_REPRESENTATION (  '', ( #76585 ), #52750 ) ;
#28695 = CARTESIAN_POINT ( 'NONE',  ( 0.1532563361054083140, 36.00893115100078745, 1.131784320476157264E-15 ) ) ;
#28696 = CARTESIAN_POINT ( 'NONE',  ( -0.8801773607110991993, 12.85535201082150358, -2.915334737309923874 ) ) ;
#28697 = CARTESIAN_POINT ( 'NONE',  ( 16.40814093676324603, 57.45696800326375353, -11.09922568453594671 ) ) ;
#28698 = DIRECTION ( 'NONE',  ( 0.1132032137679171296, 0.000000000000000000, -0.9935718556765862353 ) ) ;
#28699 = CARTESIAN_POINT ( 'NONE',  ( 19.84674366389459266, 48.71726448433413026, -2.638427012816827677 ) ) ;
#28701 = ORIENTED_EDGE ( 'NONE', *, *, #70808, .F. ) ;
#28700 = CARTESIAN_POINT ( 'NONE',  ( 20.24186590665277663, 21.76028685723174050, 6.114288769123037426 ) ) ;
#28702 = AXIS2_PLACEMENT_3D ( 'NONE', #2086, #63533, #93049 ) ;
#28703 = CARTESIAN_POINT ( 'NONE',  ( 19.72487221294571569, 17.80223176428831522, -6.499999999999990230 ) ) ;
#28704 = CARTESIAN_POINT ( 'NONE',  ( -12.60874940350938189, 3.923185800807110140E-16, -7.160268045227207168 ) ) ;
#28705 = CARTESIAN_POINT ( 'NONE',  ( 8.629999999999995453, 41.24999999999999289, 6.250000000000000000 ) ) ;
#28706 = EDGE_CURVE ( 'NONE', #83059, #75159, #32579, .T. ) ;
#28707 = CARTESIAN_POINT ( 'NONE',  ( -12.80781515976305762, 15.00000000000000000, -6.246788841744501219 ) ) ;
#28708 = CARTESIAN_POINT ( 'NONE',  ( 19.84674366389459266, 13.30059781766745353, 2.638427012816836559 ) ) ;
#28709 = CARTESIAN_POINT ( 'NONE',  ( -2.816281873526471635, 28.91530133659708213, -3.434112377981056508 ) ) ;
#28710 = DIRECTION ( 'NONE',  ( -0.000000000000000000, 1.000000000000000000, 0.000000000000000000 ) ) ;
#28711 = EDGE_CURVE ( 'NONE', #56832, #19862, #91026, .T. ) ;
#28712 = ORIENTED_EDGE ( 'NONE', *, *, #60792, .T. ) ;
#28713 = CARTESIAN_POINT ( 'NONE',  ( 18.52753015748618282, 53.92559781766745175, -4.923371831947291888 ) ) ;
#28714 = DIRECTION ( 'NONE',  ( 0.000000000000000000, -0.000000000000000000, -1.000000000000000000 ) ) ;
#28715 = CARTESIAN_POINT ( 'NONE',  ( 10.00000000000000000, 25.55374883491396787, -14.16423886937410082 ) ) ;
#28716 = CARTESIAN_POINT ( 'NONE',  ( 18.52753015748617571, 48.09226448433412315, 4.923371831947298993 ) ) ;
#28717 = CARTESIAN_POINT ( 'NONE',  ( 6.565887622018943937, 50.16530133659708213, 12.81628187352647430 ) ) ;
#28719 = CARTESIAN_POINT ( 'NONE',  ( -15.00000000000000000, 83.99999999999998579, 4.000000000000000000 ) ) ;
#28718 = DIRECTION ( 'NONE',  ( 0.000000000000000000, 1.000000000000000000, 0.000000000000000000 ) ) ;
#28720 = CARTESIAN_POINT ( 'NONE',  ( 0.1532563361054100626, 10.80059781766745175, -2.638427012816831230 ) ) ;
#28721 = CARTESIAN_POINT ( 'NONE',  ( 20.15039907845753575, 47.62777174578613426, -6.262539305110073506 ) ) ;
#28722 = CARTESIAN_POINT ( 'NONE',  ( 17.20831665107776587, 52.88393115100078035, 7.208316651077764980 ) ) ;
#28723 = CARTESIAN_POINT ( 'NONE',  ( 20.88017736071110519, 45.56368534415484106, 2.639326808657452039E-16 ) ) ;
#28724 = CARTESIAN_POINT ( 'NONE',  ( 10.00000000000000178, 32.25893115100078745, 9.846743663894594434 ) ) ;
#28725 = DIRECTION ( 'NONE',  ( 0.5049712402759914953, 0.6679043323762693385, -0.5467246558251572797 ) ) ;
#28726 = CARTESIAN_POINT ( 'NONE',  ( -10.09048698379360687, 46.92328126389585208, 0.000000000000000000 ) ) ;
#28727 = CARTESIAN_POINT ( 'NONE',  ( 0.5774900079438590739, 42.64701867748816966, -5.440088680355550821 ) ) ;
#28728 = VERTEX_POINT ( 'NONE', #46184 ) ;
#28729 = CARTESIAN_POINT ( 'NONE',  ( 10.00000000000000178, 69.31368534415484817, 10.88017736071110342 ) ) ;
#28730 = CARTESIAN_POINT ( 'NONE',  ( 4.559911319644449179, 13.89701867748817143, 9.422509992056141925 ) ) ;
#28732 = CARTESIAN_POINT ( 'NONE',  ( 2.035157376598822676, 47.43868534415484817, -7.964842623401177768 ) ) ;
#28731 = CARTESIAN_POINT ( 'NONE',  ( 0.1532563361054083140, 51.00893115100078745, 1.131784320476157264E-15 ) ) ;
#28733 = DIRECTION ( 'NONE',  ( 0.000000000000000000, 1.000000000000000000, 0.000000000000000000 ) ) ;
#28734 = CARTESIAN_POINT ( 'NONE',  ( 10.00000000000000178, 54.31368534415484106, 10.88017736071110342 ) ) ;
#28735 = AXIS2_PLACEMENT_3D ( 'NONE', #84124, #1127, #31589 ) ;
#28737 = DIRECTION ( 'NONE',  ( 0.000000000000000000, 0.000000000000000000, 1.000000000000000000 ) ) ;
#28736 = CARTESIAN_POINT ( 'NONE',  ( 0.5774900079438590739, 27.64701867748817676, -5.440088680355550821 ) ) ;
#28738 = CARTESIAN_POINT ( 'NONE',  ( 7.361572987183169658, -0.03273551566588185635, -9.846743663894592657 ) ) ;
#28739 = CARTESIAN_POINT ( 'NONE',  ( 1.472469842513823179, 20.59226448433411960, -4.923371831947296329 ) ) ;
#28740 = CARTESIAN_POINT ( 'NONE',  ( 2.831191079880678085, 79.91181047996344944, 5.000000000000000000 ) ) ;
#28741 = CARTESIAN_POINT ( 'NONE',  ( -14.16423886937410082, 6.803748834913976751, 4.336808689942017736E-15 ) ) ;
#28742 = CARTESIAN_POINT ( 'NONE',  ( 19.84674366389459266, 48.71726448433413026, -2.638427012816827677 ) ) ;
#28743 = AXIS2_PLACEMENT_3D ( 'NONE', #72338, #28327, #3870 ) ;
#28745 = CARTESIAN_POINT ( 'NONE',  ( -0.1503990784575359729, 18.10158574516642460, 6.262539305110062848 ) ) ;
#28744 = CARTESIAN_POINT ( 'NONE',  ( 0.5774900079438590739, 2.647018677488171434, -5.440088680355550821 ) ) ;
#28746 = DIRECTION ( 'NONE',  ( -4.085620730620576069E-14, 0.000000000000000000, 1.000000000000000000 ) ) ;
#28747 = CIRCLE ( 'NONE', #23992, 15.00000000000000000 ) ;
#28748 = CARTESIAN_POINT ( 'NONE',  ( -0.3689425029237898834, 6.178748834913968757, -10.36894250292378850 ) ) ;
#28749 = CARTESIAN_POINT ( 'NONE',  ( 2.917880565312950480, 50.97041550158064638, -12.26659068614894821 ) ) ;
#28750 = CARTESIAN_POINT ( 'NONE',  ( -2.816281873526473856, -0.6680319967362464695, 3.434112377981055619 ) ) ;
#28751 = VERTEX_POINT ( 'NONE', #706 ) ;
#28752 = CARTESIAN_POINT ( 'NONE',  ( 17.96484262340118221, 14.93868534415484106, 7.964842623401181321 ) ) ;
#28753 = CARTESIAN_POINT ( 'NONE',  ( 19.84674366389459266, 43.71726448433410894, -2.638427012816827677 ) ) ;
#28755 = CARTESIAN_POINT ( 'NONE',  ( -13.45431060380788502, 90.84076481352336430, -7.653071044409292867 ) ) ;
#28754 = DIRECTION ( 'NONE',  ( -0.4146932426562403573, 0.000000000000000000, 0.9099612708765426605 ) ) ;
#28756 = SURFACE_STYLE_USAGE ( .BOTH. , #51263 ) ;
#28757 = CARTESIAN_POINT ( 'NONE',  ( 5.500000000000000000, 11.00000000000000000, 5.000000000000000000 ) ) ;
#28758 = CARTESIAN_POINT ( 'NONE',  ( 19.38216949554541557, 22.24863466993041428, -9.382169495545420901 ) ) ;
#28759 = CARTESIAN_POINT ( 'NONE',  ( 7.361572987183170547, 22.05059781766745530, 9.846743663894590881 ) ) ;
#28760 = ORIENTED_EDGE ( 'NONE', *, *, #93915, .T. ) ;
#28761 = CARTESIAN_POINT ( 'NONE',  ( 19.84674366389459266, 8.300597817667451750, 2.638427012816836559 ) ) ;
#28762 = SURFACE_SIDE_STYLE ('',( #28269 ) ) ;
#28763 = CARTESIAN_POINT ( 'NONE',  ( -14.82269085861174140, 14.63606914776923418, 2.299529454046852273 ) ) ;
#28764 = CARTESIAN_POINT ( 'NONE',  ( 2.035157376598824452, 18.68868534415484106, 7.964842623401179544 ) ) ;
#28765 = CARTESIAN_POINT ( 'NONE',  ( 6.204703633549690345, 37.84541550158063927, 14.16423886937410082 ) ) ;
#28766 = CARTESIAN_POINT ( 'NONE',  ( 10.00000000000000000, 66.81368534415484817, -10.88017736071110342 ) ) ;
#28767 = DIRECTION ( 'NONE',  ( 0.1305261922200514901, 0.000000000000000000, 0.9914448613738104932 ) ) ;
#28768 = CARTESIAN_POINT ( 'NONE',  ( 17.20831665107776587, 19.13393115100078035, -7.208316651077762316 ) ) ;
#28769 = CARTESIAN_POINT ( 'NONE',  ( 12.63842701281683922, 4.550597817667451750, -9.846743663894590881 ) ) ;
#28770 = CARTESIAN_POINT ( 'NONE',  ( 10.00000000000000178, 42.25893115100078745, 9.846743663894594434 ) ) ;
#28771 = CARTESIAN_POINT ( 'NONE',  ( 14.92337183194729988, 64.34226448433412315, -8.527530157486177487 ) ) ;
#28772 = EDGE_CURVE ( 'NONE', #1179, #21240, #53673, .T. ) ;
#28773 = CARTESIAN_POINT ( 'NONE',  ( 15.44008868035555793, 31.39701867748817676, -9.422509992056140149 ) ) ;
#28774 = EDGE_LOOP ( 'NONE', ( #89573, #87379, #51668, #14811 ) ) ;
#28775 = CARTESIAN_POINT ( 'NONE',  ( -1.099225684535947600, 59.54030133659708923, 6.408140936763237150 ) ) ;
#28776 =( LENGTH_UNIT ( ) NAMED_UNIT ( * ) SI_UNIT ( .MILLI., .METRE. ) );
#28777 = CARTESIAN_POINT ( 'NONE',  ( 19.84674366389459266, 3.717264484334118713, -2.638427012816827677 ) ) ;
#28778 = CARTESIAN_POINT ( 'NONE',  ( 10.00000000000000000, 47.87363466993042493, -12.81628187352647608 ) ) ;
#28780 = CARTESIAN_POINT ( 'NONE',  ( 1.472469842513823179, 36.42559781766745175, 4.923371831947296329 ) ) ;
#28779 = CARTESIAN_POINT ( 'NONE',  ( -4.164238869374098151, 66.59541550158060375, -3.795296366450310543 ) ) ;
#28781 =( NAMED_UNIT ( * ) SI_UNIT ( $, .STERADIAN. ) SOLID_ANGLE_UNIT ( ) );
#28782 =( NAMED_UNIT ( * ) SI_UNIT ( $, .STERADIAN. ) SOLID_ANGLE_UNIT ( ) );
#28783 = CARTESIAN_POINT ( 'NONE',  ( 22.26659068614895176, 19.72041550158063572, -7.082119434687042414 ) ) ;
#28784 = CARTESIAN_POINT ( 'NONE',  ( 22.26659068614895176, 49.72041550158063927, -7.082119434687042414 ) ) ;
#28785 = CARTESIAN_POINT ( 'NONE',  ( 17.20831665107776587, 49.13393115100078745, -7.208316651077762316 ) ) ;
#28786 = DIRECTION ( 'NONE',  ( -0.08715574274765415519, -0.9961946980917458783, 0.000000000000000000 ) ) ;
#28787 = CARTESIAN_POINT ( 'NONE',  ( 2.035157376598824452, 33.68868534415484106, 7.964842623401179544 ) ) ;
#28788 = CARTESIAN_POINT ( 'NONE',  ( 15.44008868035555793, 66.39701867748817676, -9.422509992056140149 ) ) ;
#28789 = SURFACE_STYLE_FILL_AREA ( #19328 ) ;
#28790 = ORIENTED_EDGE ( 'NONE', *, *, #21764, .T. ) ;
#28791 = CARTESIAN_POINT ( 'NONE',  ( -1.099225684535947600, 63.70696800326376774, -6.408140936763238038 ) ) ;
#28792 = CARTESIAN_POINT ( 'NONE',  ( 17.96484262340118221, 64.93868534415483396, 7.964842623401181321 ) ) ;
#28793 = ORIENTED_EDGE ( 'NONE', *, *, #64138, .T. ) ;
#28794 = CARTESIAN_POINT ( 'NONE',  ( 18.52753015748618282, 3.925597817667451306, -4.923371831947291888 ) ) ;
#28795 = CARTESIAN_POINT ( 'NONE',  ( -46.31228368244003946, 103.3337736655113588, -5.775421524742657020 ) ) ;
#28796 = ORIENTED_EDGE ( 'NONE', *, *, #25263, .T. ) ;
#28797 = VECTOR ( 'NONE', #11189, 1000.000000000000000 ) ;
#28798 = CARTESIAN_POINT ( 'NONE',  ( 17.96484262340118221, 9.938685344154837509, 7.964842623401181321 ) ) ;
#28799 = EDGE_CURVE ( 'NONE', #60724, #55655, #43383, .T. ) ;
#28800 = EDGE_CURVE ( 'NONE', #87709, #14505, #12274, .T. ) ;
#28801 = ORIENTED_EDGE ( 'NONE', *, *, #26710, .F. ) ;
#28802 = CARTESIAN_POINT ( 'NONE',  ( 20.88017736071110164, 20.35535201082150891, 2.915334737309930979 ) ) ;
#28803 = CIRCLE ( 'NONE', #51149, 0.2500000000000002220 ) ;
#28804 = CARTESIAN_POINT ( 'NONE',  ( 0.1532563361054082862, 56.21726448433411605, 2.638427012816831674 ) ) ;
#28805 = ORIENTED_EDGE ( 'NONE', *, *, #60675, .F. ) ;
#28806 = AXIS2_PLACEMENT_3D ( 'NONE', #93466, #32953, #79933 ) ;
#28807 = CARTESIAN_POINT ( 'NONE',  ( 5.076628168052703671, 66.84226448433412315, 8.527530157486179263 ) ) ;
#28808 = VERTEX_POINT ( 'NONE', #1195 ) ;
#28809 = CARTESIAN_POINT ( 'NONE',  ( 5.076628168052704559, 0.1755978176674514724, -8.527530157486179263 ) ) ;
#28810 = CARTESIAN_POINT ( 'NONE',  ( 12.63842701281683034, 62.46726448433410894, 9.846743663894596210 ) ) ;
#28812 = CARTESIAN_POINT ( 'NONE',  ( -12.98685442714202232, 15.00000000000000000, 6.449155920600843750 ) ) ;
#28811 = CARTESIAN_POINT ( 'NONE',  ( 4.559911319644449179, 22.23035201082150536, -9.422509992056141925 ) ) ;
#28813 = CARTESIAN_POINT ( 'NONE',  ( 1.472469842513823179, 5.592264484334118713, -4.923371831947296329 ) ) ;
#28814 = VECTOR ( 'NONE', #87720, 1000.000000000000000 ) ;
#28815 = CARTESIAN_POINT ( 'NONE',  ( 12.91533473730992121, 19.52201867748816611, 10.88017736071110164 ) ) ;
#28816 = CARTESIAN_POINT ( 'NONE',  ( 3.591859063236761518, 49.95696800326375353, 11.09922568453594849 ) ) ;
#28817 = CARTESIAN_POINT ( 'NONE',  ( 0.5774900079438607392, 48.48035201082150536, 5.440088680355550821 ) ) ;
#28818 = DIRECTION ( 'NONE',  ( 0.9752498888222641549, -0.2211055276381879986, 0.000000000000000000 ) ) ;
#28819 = CARTESIAN_POINT ( 'NONE',  ( -1.099225684535947600, 59.54030133659708923, 6.408140936763237150 ) ) ;
#28820 = CARTESIAN_POINT ( 'NONE',  ( 20.88017736071110519, 50.56368534415484106, 2.639326808657452039E-16 ) ) ;
#28821 = CARTESIAN_POINT ( 'NONE',  ( 14.92337183194729633, 52.67559781766745175, 8.527530157486181039 ) ) ;
#28822 = CARTESIAN_POINT ( 'NONE',  ( 18.52753015748617571, 23.09226448433411960, 4.923371831947298993 ) ) ;
#28823 = CARTESIAN_POINT ( 'NONE',  ( 22.81628187352647785, 6.623634669930420493, 6.195893100308588602E-16 ) ) ;
#28825 = CARTESIAN_POINT ( 'NONE',  ( 1.472469842513823179, 61.42559781766745175, 4.923371831947296329 ) ) ;
#28824 = LINE ( 'NONE', #66331, #37257 ) ;
#28826 = CARTESIAN_POINT ( 'NONE',  ( 20.88017736071110875, 25.77201867748816966, -2.915334737309920765 ) ) ;
#28827 = CARTESIAN_POINT ( 'NONE',  ( 1.472469842513823179, 56.42559781766745886, 4.923371831947296329 ) ) ;
#28828 = EDGE_CURVE ( 'NONE', #68783, #3546, #79303, .T. ) ;
#28829 = CARTESIAN_POINT ( 'NONE',  ( 12.63842701281683922, 9.550597817667449974, -9.846743663894590881 ) ) ;
#28830 = CARTESIAN_POINT ( 'NONE',  ( -11.39601241150444189, -0.03417435944610275333, -11.22534175661882294 ) ) ;
#28832 = VERTEX_POINT ( 'NONE', #15699 ) ;
#28831 = CARTESIAN_POINT ( 'NONE',  ( 6.565887622018943937, 5.165301336597086568, 12.81628187352647430 ) ) ;
#28833 = AXIS2_PLACEMENT_3D ( 'NONE', #24684, #25187, #9673 ) ;
#28834 = CARTESIAN_POINT ( 'NONE',  ( 22.81628187352647785, 41.62363466993042493, 6.195893100308588602E-16 ) ) ;
#28835 = CARTESIAN_POINT ( 'NONE',  ( 0.1532563361054100626, 30.80059781766744820, -2.638427012816831230 ) ) ;
#28836 = CARTESIAN_POINT ( 'NONE',  ( 11.25000000000000000, 7.409700295649311208, 3.014428414850128135 ) ) ;
#28837 = CARTESIAN_POINT ( 'NONE',  ( -0.8801773607111009756, 8.063685344154837509, 1.068504757029289695E-15 ) ) ;
#28838 = CARTESIAN_POINT ( 'NONE',  ( 2.791683348922237240, 25.38393115100078390, -7.208316651077763204 ) ) ;
#28839 = DIRECTION ( 'NONE',  ( 0.000000000000000000, 0.000000000000000000, -1.000000000000000000 ) ) ;
#28840 = CARTESIAN_POINT ( 'NONE',  ( 10.00000000000000178, 68.05374883491397497, 14.16423886937410082 ) ) ;
#28841 = CARTESIAN_POINT ( 'NONE',  ( -10.79772875661416087, 89.74400587740484525, -6.349085400557793690 ) ) ;
#28842 = CARTESIAN_POINT ( 'NONE',  ( 0.5774900079438590739, 17.64701867748817321, -5.440088680355550821 ) ) ;
#28843 = CARTESIAN_POINT ( 'NONE',  ( 22.26659068614895176, 49.72041550158063927, -7.082119434687042414 ) ) ;
#28845 = CARTESIAN_POINT ( 'NONE',  ( -18.00000000000000355, 75.73428692542562146, -3.000000000000000000 ) ) ;
#28844 = CARTESIAN_POINT ( 'NONE',  ( 22.26659068614894466, 53.88708216824731068, 7.082119434687054849 ) ) ;
#28846 = CARTESIAN_POINT ( 'NONE',  ( 0.000000000000000000, 0.5000000000000004441, 0.000000000000000000 ) ) ;
#28847 = CARTESIAN_POINT ( 'NONE',  ( 5.076628168052704559, 10.17559781766745175, -8.527530157486179263 ) ) ;
#28848 = CARTESIAN_POINT ( 'NONE',  ( 0.6178305044545838731, 4.748634669930420493, 9.382169495545420901 ) ) ;
#28849 = ORIENTED_EDGE ( 'NONE', *, *, #31158, .T. ) ;
#28850 = CARTESIAN_POINT ( 'NONE',  ( -46.34323875807881166, 103.6109741468810483, 6.190393423093142999 ) ) ;
#28851 = CARTESIAN_POINT ( 'NONE',  ( 5.076628168052703671, 56.84226448433412315, 8.527530157486179263 ) ) ;
#28852 = CARTESIAN_POINT ( 'NONE',  ( 10.69820648722788015, 1.823139558123380688, 5.272416709312279792 ) ) ;
#28853 = CARTESIAN_POINT ( 'NONE',  ( 14.99999999999998046, 69.99999999999998579, 6.250000000000000000 ) ) ;
#28854 = CARTESIAN_POINT ( 'NONE',  ( 24.16423886937409904, 4.095415501580634832, 3.795296366450317205 ) ) ;
#28855 = CIRCLE ( 'NONE', #86339, 15.00000000000000000 ) ;
#28856 = CARTESIAN_POINT ( 'NONE',  ( 17.20831665107776587, 24.13393115100078035, -7.208316651077762316 ) ) ;
#28857 = FACE_OUTER_BOUND ( 'NONE', #78849, .T. ) ;
#28858 = ORIENTED_EDGE ( 'NONE', *, *, #51717, .T. ) ;
#28859 = CARTESIAN_POINT ( 'NONE',  ( -0.3689425029237881626, 42.42874883491396787, 10.36894250292379027 ) ) ;
#28860 = CARTESIAN_POINT ( 'NONE',  ( 7.361572987183169658, 9.967264484334119601, -9.846743663894592657 ) ) ;
#28862 = FACE_OUTER_BOUND ( 'NONE', #80753, .T. ) ;
#28861 = CARTESIAN_POINT ( 'NONE',  ( -3.927832320392065313, -0.03417435944610275333, -13.69797916712109398 ) ) ;
#28863 = CARTESIAN_POINT ( 'NONE',  ( -0.8801773607111009756, 33.06368534415484106, 1.068504757029289695E-15 ) ) ;
#28864 = CARTESIAN_POINT ( 'NONE',  ( -1.099225684535947600, 33.70696800326375353, -6.408140936763238038 ) ) ;
#28865 = SURFACE_STYLE_FILL_AREA ( #66378 ) ;
#28866 = COLOUR_RGB ( '', 0.40784314, 0.44705882, 0.49803922) ;
#28867 = CARTESIAN_POINT ( 'NONE',  ( 13.43411237798106583, 37.66530133659708923, -12.81628187352647252 ) ) ;
#28868 = CARTESIAN_POINT ( 'NONE',  ( -2.816281873526471635, 58.91530133659707502, -3.434112377981056508 ) ) ;
#28869 = ORIENTED_EDGE ( 'NONE', *, *, #98825, .T. ) ;
#28870 = CYLINDRICAL_SURFACE ( 'NONE', #581, 0.2500000000000002220 ) ;
#28871 = DIRECTION ( 'NONE',  ( -0.000000000000000000, -1.000000000000000000, -0.000000000000000000 ) ) ;
#28872 = CARTESIAN_POINT ( 'NONE',  ( 6.204703633549690345, 42.84541550158063217, 14.16423886937410082 ) ) ;
#28873 = CARTESIAN_POINT ( 'NONE',  ( 0.5774900079438607392, 3.480352010821504027, 5.440088680355550821 ) ) ;
#28874 = CARTESIAN_POINT ( 'NONE',  ( 7.084665262690076126, 17.02201867748817676, -10.88017736071110164 ) ) ;
#28875 = DIRECTION ( 'NONE',  ( 0.9970872288863209532, 0.07626964003977952655, -0.000000000000000000 ) ) ;
#28876 = CARTESIAN_POINT ( 'NONE',  ( 19.72487221294570858, 70.00000000000000000, 6.000000000000000000 ) ) ;
#28877 = CARTESIAN_POINT ( 'NONE',  ( 12.91533473730993009, 51.60535201082149825, -10.88017736071109987 ) ) ;
#28878 = CARTESIAN_POINT ( 'NONE',  ( 7.084665262690076126, 57.02201867748817676, -10.88017736071110164 ) ) ;
#28879 = CARTESIAN_POINT ( 'NONE',  ( 19.38216949554541202, 10.99863466993042138, 9.382169495545424454 ) ) ;
#28880 = DIRECTION ( 'NONE',  ( 0.9862856015372331031, 0.000000000000000000, -0.1650476058606676344 ) ) ;
#28881 = CARTESIAN_POINT ( 'NONE',  ( 10.00000000000000178, 17.25893115100078745, 9.846743663894594434 ) ) ;
#28882 = CARTESIAN_POINT ( 'NONE',  ( -0.8801773607111009756, 63.06368534415484106, 1.068504757029289695E-15 ) ) ;
#28883 = EDGE_CURVE ( 'NONE', #9875, #31048, #28263, .T. ) ;
#28884 = CARTESIAN_POINT ( 'NONE',  ( 16.40814093676323893, 15.79030133659708746, 11.09922568453595026 ) ) ;
#28885 = CARTESIAN_POINT ( 'NONE',  ( 6.579634127946654587, -87.99828267815715321, 3.750000000000000000 ) ) ;
#28886 = CARTESIAN_POINT ( 'NONE',  ( 20.88017736071110519, 5.563685344154837509, 2.639326808657452039E-16 ) ) ;
#28887 = CARTESIAN_POINT ( 'NONE',  ( 12.63842701281683922, 44.55059781766745175, -9.846743663894590881 ) ) ;
#28888 = CARTESIAN_POINT ( 'NONE',  ( -1.099225684535947600, 49.54030133659708923, 6.408140936763237150 ) ) ;
#28889 = CARTESIAN_POINT ( 'NONE',  ( 1.472469842513823179, 16.42559781766745175, 4.923371831947296329 ) ) ;
#28890 = CARTESIAN_POINT ( 'NONE',  ( 24.16423886937409904, 9.095415501580633943, 3.795296366450317205 ) ) ;
#28891 = DIRECTION ( 'NONE',  ( -0.000000000000000000, -1.000000000000000000, 0.000000000000000000 ) ) ;
#28892 = CARTESIAN_POINT ( 'NONE',  ( 17.96484262340118221, 26.18868534415483396, -7.964842623401177768 ) ) ;
#28894 = CARTESIAN_POINT ( 'NONE',  ( -4.164238869374099927, 32.01208216824730357, 3.795296366450308767 ) ) ;
#28893 = DIRECTION ( 'NONE',  ( -0.000000000000000000, 1.000000000000000000, -0.000000000000000000 ) ) ;
#28895 = CARTESIAN_POINT ( 'NONE',  ( 1.472469842513823179, 45.59226448433412315, -4.923371831947296329 ) ) ;
#28896 = CARTESIAN_POINT ( 'NONE',  ( 10.00000000000000000, 21.81368534415484106, -10.88017736071110342 ) ) ;
#28897 = CARTESIAN_POINT ( 'NONE',  ( 2.035157376598822676, 12.43868534415483751, -7.964842623401177768 ) ) ;
#28898 = ORIENTED_EDGE ( 'NONE', *, *, #51816, .T. ) ;
#28899 = CIRCLE ( 'NONE', #52890, 0.4999999999999995559 ) ;
#28900 = CARTESIAN_POINT ( 'NONE',  ( 0.5774900079438607392, 28.48035201082150891, 5.440088680355550821 ) ) ;
#28901 = CIRCLE ( 'NONE', #32118, 0.5000000000000004441 ) ;
#28902 = CARTESIAN_POINT ( 'NONE',  ( 19.38216949554541202, 40.99863466993042493, 9.382169495545424454 ) ) ;
#28903 = CARTESIAN_POINT ( 'NONE',  ( -0.8801773607111008646, 28.27201867748817321, 2.915334737309923430 ) ) ;
#28904 = CARTESIAN_POINT ( 'NONE',  ( 0.5774900079438590739, 37.64701867748817676, -5.440088680355550821 ) ) ;
#28905 = ORIENTED_EDGE ( 'NONE', *, *, #14389, .T. ) ;
#28906 = CARTESIAN_POINT ( 'NONE',  ( 17.20831665107776587, 54.13393115100079456, -7.208316651077762316 ) ) ;
#28907 = CARTESIAN_POINT ( 'NONE',  ( 17.96484262340118221, 31.18868534415483751, -7.964842623401177768 ) ) ;
#28908 = CARTESIAN_POINT ( 'NONE',  ( 0.1532563361054100626, 65.80059781766745175, -2.638427012816831230 ) ) ;
#28909 = SURFACE_STYLE_FILL_AREA ( #97445 ) ;
#28910 = EDGE_CURVE ( 'NONE', #54024, #27786, #41060, .T. ) ;
#28911 = DIRECTION ( 'NONE',  ( -1.000000000000000000, 0.000000000000000000, 0.000000000000000000 ) ) ;
#28912 = CARTESIAN_POINT ( 'NONE',  ( 10.00000000000000178, 53.05374883491396787, 14.16423886937410082 ) ) ;
#28913 = CARTESIAN_POINT ( 'NONE',  ( -0.8801773607111009756, 58.06368534415484106, 1.068504757029289695E-15 ) ) ;
#28914 = DIRECTION ( 'NONE',  ( 0.000000000000000000, 0.000000000000000000, 1.000000000000000000 ) ) ;
#28915 =( BOUNDED_CURVE ( )  B_SPLINE_CURVE ( 2, ( #77962, #93954, #23995, #9469, #25480, #10457, #40966, #61968, #71464 ),
 .UNSPECIFIED., .F., .F. ) 
 B_SPLINE_CURVE_WITH_KNOTS ( ( 3, 2, 2, 2, 3 ),
 ( 0.1544266512259456492, 0.1547619047619047672, 0.1607142857142856984, 0.1666666666666666297, 0.1670019202026257477 ),
 .UNSPECIFIED. ) 
 CURVE ( )  GEOMETRIC_REPRESENTATION_ITEM ( )  RATIONAL_B_SPLINE_CURVE ( ( 0.9963778908391762723, 0.9980808541467921513, 1.000000000000000000, 0.9659258262890683122, 1.000000000000000000, 0.9659258262890683122, 1.000000000000000000, 0.9980808541467922623, 0.9963778908391764944 ) ) 
 REPRESENTATION_ITEM ( '' )  );
#28916 = CARTESIAN_POINT ( 'NONE',  ( 8.564643372776545860, 14.63606914147656646, 12.31449893000750428 ) ) ;
#28917 = CARTESIAN_POINT ( 'NONE',  ( 12.63842701281683922, 64.55059781766745175, -9.846743663894590881 ) ) ;
#28918 = CARTESIAN_POINT ( 'NONE',  ( 10.00000000000000000, 14.75893115100078568, -9.846743663894594434 ) ) ;
#28919 = EDGE_CURVE ( 'NONE', #28474, #13062, #23698, .T. ) ;
#28920 = ORIENTED_EDGE ( 'NONE', *, *, #78578, .F. ) ;
#28921 = CARTESIAN_POINT ( 'NONE',  ( 1.472469842513823179, 26.42559781766745175, 4.923371831947296329 ) ) ;
#28922 = CARTESIAN_POINT ( 'NONE',  ( 6.408140936763236262, -12.54303199673624469, -11.09922568453595026 ) ) ;
#28923 = CARTESIAN_POINT ( 'NONE',  ( 0.5774900079438590739, 22.64701867748817321, -5.440088680355550821 ) ) ;
#28924 = CARTESIAN_POINT ( 'NONE',  ( 19.84674366389459266, 23.30059781766745530, 2.638427012816836559 ) ) ;
#28926 = CARTESIAN_POINT ( 'NONE',  ( 17.96484262340118221, 59.93868534415484106, 7.964842623401181321 ) ) ;
#28925 = CARTESIAN_POINT ( 'NONE',  ( 19.42250999205614548, 65.98035201082151957, -5.440088680355545492 ) ) ;
#28928 = CARTESIAN_POINT ( 'NONE',  ( 16.40814093676324603, 52.45696800326375353, -11.09922568453594671 ) ) ;
#28927 = CARTESIAN_POINT ( 'NONE',  ( 19.42250999205614548, 30.98035201082150536, -5.440088680355545492 ) ) ;
#28929 = CARTESIAN_POINT ( 'NONE',  ( 2.917880565312950480, 40.97041550158063217, -12.26659068614894821 ) ) ;
#28930 = AXIS2_PLACEMENT_3D ( 'NONE', #92955, #16983, #62954 ) ;
#28931 = FACE_OUTER_BOUND ( 'NONE', #42415, .T. ) ;
#28932 = VERTEX_POINT ( 'NONE', #39179 ) ;
#28933 = CARTESIAN_POINT ( 'NONE',  ( 19.38216949554541202, 5.998634669930420493, 9.382169495545424454 ) ) ;
#28934 = CARTESIAN_POINT ( 'NONE',  ( 12.91533473730993009, 6.605352010821504471, -10.88017736071109987 ) ) ;
#28935 = CARTESIAN_POINT ( 'NONE',  ( 4.559911319644449179, 43.89701867748816966, 9.422509992056141925 ) ) ;
#28936 = AXIS2_PLACEMENT_3D ( 'NONE', #62461, #46975, #92964 ) ;
#28937 = DIRECTION ( 'NONE',  ( 0.000000000000000000, 1.000000000000000000, 0.000000000000000000 ) ) ;
#28938 = ORIENTED_EDGE ( 'NONE', *, *, #58216, .T. ) ;
#28940 = CARTESIAN_POINT ( 'NONE',  ( -12.60589901313227124, 0.5000000000000004441, 8.129656208641961257 ) ) ;
#28939 = CARTESIAN_POINT ( 'NONE',  ( 5.076628168052704559, 15.17559781766745175, -8.527530157486179263 ) ) ;
#28941 = CARTESIAN_POINT ( 'NONE',  ( 15.44008868035555793, 61.39701867748817676, -9.422509992056140149 ) ) ;
#28942 = AXIS2_PLACEMENT_3D ( 'NONE', #39626, #8622, #39132 ) ;
#28943 = CARTESIAN_POINT ( 'NONE',  ( 10.00000000000000178, 37.25893115100078745, 9.846743663894594434 ) ) ;
#28944 = CARTESIAN_POINT ( 'NONE',  ( 17.20831665107776587, 17.88393115100078745, 7.208316651077764980 ) ) ;
#28945 = CARTESIAN_POINT ( 'NONE',  ( 19.84674366389459266, 18.30059781766745175, 2.638427012816836559 ) ) ;
#28947 = CARTESIAN_POINT ( 'NONE',  ( -2.816281873526473856, 44.12363466993042493, 9.499525473075851096E-16 ) ) ;
#28946 = CARTESIAN_POINT ( 'NONE',  ( 19.72487221294571924, 62.80223176428831522, -6.499999999999984901 ) ) ;
#28948 = EDGE_CURVE ( 'NONE', #51986, #26486, #95281, .T. ) ;
#28950 = DIRECTION ( 'NONE',  ( -0.000000000000000000, -1.000000000000000000, -0.000000000000000000 ) ) ;
#28949 = CARTESIAN_POINT ( 'NONE',  ( 19.42250999205614548, 65.98035201082151957, -5.440088680355545492 ) ) ;
#28951 = CARTESIAN_POINT ( 'NONE',  ( 10.93736952761193670, -97.13260119835408091, 4.000000000000000000 ) ) ;
#28953 = ORIENTED_EDGE ( 'NONE', *, *, #80003, .F. ) ;
#28952 = CARTESIAN_POINT ( 'NONE',  ( 12.63842701281683922, 34.55059781766745886, -9.846743663894590881 ) ) ;
#28954 = CARTESIAN_POINT ( 'NONE',  ( 21.09922568453595559, 57.04030133659708923, -6.408140936763230044 ) ) ;
#28955 = CARTESIAN_POINT ( 'NONE',  ( 0.1552420861328543400, -3.159856409732166232E-15, 14.62478754979302842 ) ) ;
#28956 = CARTESIAN_POINT ( 'NONE',  ( 10.00000000000000178, 67.25893115100079456, 9.846743663894594434 ) ) ;
#28957 = CARTESIAN_POINT ( 'NONE',  ( -0.8801773607111009756, 18.06368534415484106, 1.068504757029289695E-15 ) ) ;
#28958 = CARTESIAN_POINT ( 'NONE',  ( -4.164238869374098151, 26.59541550158063217, -3.795296366450310543 ) ) ;
#28959 = CYLINDRICAL_SURFACE ( 'NONE', #26428, 11.92686044187656513 ) ;
#28960 = CARTESIAN_POINT ( 'NONE',  ( -4.164238869374099039, 36.80374883491396787, 8.674139862899312516E-16 ) ) ;
#28961 = EDGE_CURVE ( 'NONE', #32737, #2953, #47388, .T. ) ;
#28962 = CARTESIAN_POINT ( 'NONE',  ( 10.00000000000000000, 40.55374883491397497, -14.16423886937410082 ) ) ;
#28963 = CARTESIAN_POINT ( 'NONE',  ( -2.266590686148945544, 11.38708216824730179, -7.082119434687050408 ) ) ;
#28965 = DIRECTION ( 'NONE',  ( 0.000000000000000000, 0.000000000000000000, -1.000000000000000000 ) ) ;
#28964 = CARTESIAN_POINT ( 'NONE',  ( 17.08211943468705130, 8.470415501580635720, 12.26659068614894998 ) ) ;
#28966 = CARTESIAN_POINT ( 'NONE',  ( 10.00000000000000000, 46.81368534415484106, -10.88017736071110342 ) ) ;
#28967 = CARTESIAN_POINT ( 'NONE',  ( -18.89999999999999503, 98.99999999999998579, -8.000000000000000000 ) ) ;
#28968 = ORIENTED_EDGE ( 'NONE', *, *, #24656, .T. ) ;
#28969 = CARTESIAN_POINT ( 'NONE',  ( 10.00000000000000000, 34.75893115100078745, -9.846743663894594434 ) ) ;
#28971 = CARTESIAN_POINT ( 'NONE',  ( 14.92337183194729633, 22.67559781766745175, 8.527530157486181039 ) ) ;
#28970 = CARTESIAN_POINT ( 'NONE',  ( 3.640395162852215538, 107.5383484153110203, 5.000000000000000000 ) ) ;
#28972 = CARTESIAN_POINT ( 'NONE',  ( 20.88017736071110875, 15.77201867748817143, -2.915334737309920765 ) ) ;
#28973 = CARTESIAN_POINT ( 'NONE',  ( 3.591859063236761518, 54.95696800326376064, 11.09922568453594849 ) ) ;
#28974 = CARTESIAN_POINT ( 'NONE',  ( 19.84674366389459266, 53.71726448433411605, -2.638427012816827677 ) ) ;
#28975 = FACE_OUTER_BOUND ( 'NONE', #92677, .T. ) ;
#28976 = CARTESIAN_POINT ( 'NONE',  ( 19.84674366389459621, 23.50893115100078390, 7.409399052514197653E-17 ) ) ;
#28977 = CARTESIAN_POINT ( 'NONE',  ( 19.38216949554541557, 42.24863466993041783, -9.382169495545420901 ) ) ;
#28978 = CARTESIAN_POINT ( 'NONE',  ( -14.16423886937409726, -17.98791783175269643, 3.795296366450320757 ) ) ;
#28979 = CARTESIAN_POINT ( 'NONE',  ( 7.084665262690076126, 42.02201867748816966, -10.88017736071110164 ) ) ;
#28980 = CARTESIAN_POINT ( 'NONE',  ( 18.52753015748617571, 38.09226448433412315, 4.923371831947298993 ) ) ;
#28981 = CARTESIAN_POINT ( 'NONE',  ( 24.16423886937410614, 24.51208216824730002, -3.795296366450302550 ) ) ;
#28982 = ORIENTED_EDGE ( 'NONE', *, *, #39699, .F. ) ;
#28983 = CARTESIAN_POINT ( 'NONE',  ( 17.96484262340118221, 59.93868534415484106, 7.964842623401181321 ) ) ;
#28984 = CARTESIAN_POINT ( 'NONE',  ( 10.82361996478181432, 14.95037106895532020, 10.02529603627583121 ) ) ;
#28985 = CARTESIAN_POINT ( 'NONE',  ( 2.917880565312948704, 62.63708216824730357, 12.26659068614894643 ) ) ;
#28986 = CARTESIAN_POINT ( 'NONE',  ( 1.472469842513823179, 65.59226448433412315, -4.923371831947296329 ) ) ;
#28987 = DIRECTION ( 'NONE',  ( 0.9588197348681928300, 0.000000000000000000, 0.2840153447039234780 ) ) ;
#28988 = CARTESIAN_POINT ( 'NONE',  ( 19.42250999205614548, 50.98035201082151247, -5.440088680355545492 ) ) ;
#28989 = CARTESIAN_POINT ( 'NONE',  ( -2.915334737309934532, 32.02201867748817676, -10.88017736071109987 ) ) ;
#28990 = CARTESIAN_POINT ( 'NONE',  ( 7.084665262690076126, 14.10535201082150358, 10.88017736071109987 ) ) ;
#28991 = CARTESIAN_POINT ( 'NONE',  ( 2.035157376598824452, 13.68868534415483751, 7.964842623401179544 ) ) ;
#28992 = CARTESIAN_POINT ( 'NONE',  ( 17.20831665107776587, 39.13393115100079456, -7.208316651077762316 ) ) ;
#28993 = CARTESIAN_POINT ( 'NONE',  ( 6.565887622018943937, 55.16530133659709634, 12.81628187352647430 ) ) ;
#28994 = CARTESIAN_POINT ( 'NONE',  ( 70.19910379943080159, 41.67447916666664298, -9.500000000000000000 ) ) ;
#28995 = EDGE_LOOP ( 'NONE', ( #84560, #23188, #90586, #30784 ) ) ;
#28996 = CARTESIAN_POINT ( 'NONE',  ( 2.035157376598822676, 12.43868534415483751, -7.964842623401177768 ) ) ;
#28997 = EDGE_CURVE ( 'NONE', #60588, #7347, #98054, .T. ) ;
#28998 = CARTESIAN_POINT ( 'NONE',  ( 6.565887622018943937, 5.165301336597086568, 12.81628187352647430 ) ) ;
#28999 = CARTESIAN_POINT ( 'NONE',  ( 6.579634127946654587, -87.99828267815715321, 2.750000000000000888 ) ) ;
#29000 = CARTESIAN_POINT ( 'NONE',  ( 0.1532563361054082862, 11.21726448433411605, 2.638427012816831674 ) ) ;
#29001 = VECTOR ( 'NONE', #15132, 1000.000000000000000 ) ;
#29002 = CARTESIAN_POINT ( 'NONE',  ( 19.84674366389459266, 43.71726448433410894, -2.638427012816827677 ) ) ;
#29003 = EDGE_CURVE ( 'NONE', #21081, #76760, #74033, .T. ) ;
#29004 = CARTESIAN_POINT ( 'NONE',  ( 17.96484262340118221, 29.93868534415484106, 7.964842623401181321 ) ) ;
#29005 = CARTESIAN_POINT ( 'NONE',  ( -2.816281873526473856, 14.12363466993041961, 9.499525473075851096E-16 ) ) ;
#29007 = CARTESIAN_POINT ( 'NONE',  ( 11.92686044187656691, 10.16212336850781028, -2.602085213965210642E-15 ) ) ;
#29006 = CARTESIAN_POINT ( 'NONE',  ( -0.8801773607111009756, 53.06368534415484106, 1.068504757029289695E-15 ) ) ;
#29008 = DIRECTION ( 'NONE',  ( -1.000000000000000000, 0.000000000000000000, 0.000000000000000000 ) ) ;
#29009 = MECHANICAL_DESIGN_GEOMETRIC_PRESENTATION_REPRESENTATION (  '', ( #11468 ), #96119 ) ;
#29010 = CARTESIAN_POINT ( 'NONE',  ( 22.81628187352647785, 51.62363466993042493, 6.195893100308588602E-16 ) ) ;
#29011 = ORIENTED_EDGE ( 'NONE', *, *, #98083, .T. ) ;
#29012 = CARTESIAN_POINT ( 'NONE',  ( 0.5774900079438607392, 58.48035201082151247, 5.440088680355550821 ) ) ;
#29014 = CARTESIAN_POINT ( 'NONE',  ( 22.26659068614894466, 8.887082168247300018, 7.082119434687054849 ) ) ;
#29013 = CARTESIAN_POINT ( 'NONE',  ( 3.591859063236763294, 38.29030133659708923, -11.09922568453595026 ) ) ;
#29015 = CARTESIAN_POINT ( 'NONE',  ( -0.8801773607111009756, 43.06368534415484106, 1.068504757029289695E-15 ) ) ;
#29016 = DIRECTION ( 'NONE',  ( 0.000000000000000000, 1.000000000000000000, 0.000000000000000000 ) ) ;
#29017 = CARTESIAN_POINT ( 'NONE',  ( 1.472469842513823179, 60.59226448433412315, -4.923371831947296329 ) ) ;
#29018 = CARTESIAN_POINT ( 'NONE',  ( 10.00000000000000178, 17.25893115100078745, 9.846743663894594434 ) ) ;
#29019 = CARTESIAN_POINT ( 'NONE',  ( 0.1532563361054083140, 11.00893115100078568, 1.131784320476157264E-15 ) ) ;
#29020 = DIRECTION ( 'NONE',  ( 0.000000000000000000, -1.000000000000000000, -0.000000000000000000 ) ) ;
#29021 = CARTESIAN_POINT ( 'NONE',  ( 22.26659068614895176, 39.72041550158063217, -7.082119434687042414 ) ) ;
#29022 = VECTOR ( 'NONE', #49017, 1000.000000000000114 ) ;
#29023 = EDGE_CURVE ( 'NONE', #11086, #44839, #51590, .T. ) ;
#29024 = DIRECTION ( 'NONE',  ( 0.000000000000000000, 0.000000000000000000, -1.000000000000000000 ) ) ;
#29025 = CARTESIAN_POINT ( 'NONE',  ( 10.86470958188973768, -97.91370008131707436, -3.750000000016808333 ) ) ;
#29026 = CARTESIAN_POINT ( 'NONE',  ( -7.037696230105376927, -86.26312365675100580, -3.750000000000000000 ) ) ;
#29027 = VERTEX_POINT ( 'NONE', #57 ) ;
#29028 = VERTEX_POINT ( 'NONE', #45017 ) ;
#29029 = CARTESIAN_POINT ( 'NONE',  ( 24.16423886937410614, 59.30374883491397497, 8.672049930838204340E-16 ) ) ;
#29030 = CARTESIAN_POINT ( 'NONE',  ( 13.79529636645031943, 65.34541550158063217, -14.16423886937409904 ) ) ;
#29031 = CARTESIAN_POINT ( 'NONE',  ( 0.1532563361054100626, 35.80059781766745175, -2.638427012816831230 ) ) ;
#29032 = DIRECTION ( 'NONE',  ( -0.000000000000000000, 0.000000000000000000, 1.000000000000000000 ) ) ;
#29034 = CARTESIAN_POINT ( 'NONE',  ( 10.00000000000000178, 8.053748834913967869, 14.16423886937410082 ) ) ;
#29033 = CARTESIAN_POINT ( 'NONE',  ( -0.3289641300568009741, 42.24545670184114243, -5.963430220938281678 ) ) ;
#29035 = CARTESIAN_POINT ( 'NONE',  ( 7.084665262690076126, 7.022018677488169658, -10.88017736071110164 ) ) ;
#29036 = CARTESIAN_POINT ( 'NONE',  ( 24.16423886937410614, 59.51208216824728936, -3.795296366450302550 ) ) ;
#29037 = CARTESIAN_POINT ( 'NONE',  ( 19.84674366389459266, 33.71726448433410894, -2.638427012816827677 ) ) ;
#29038 = DIRECTION ( 'NONE',  ( -0.000000000000000000, 0.000000000000000000, 1.000000000000000000 ) ) ;
#29039 = CARTESIAN_POINT ( 'NONE',  ( 2.791683348922240793, 11.63393115100078568, 7.208316651077764092 ) ) ;
#29040 = EDGE_CURVE ( 'NONE', #35385, #8055, #53506, .T. ) ;
#29041 = DIRECTION ( 'NONE',  ( -0.000000000000000000, -1.000000000000000000, -0.000000000000000000 ) ) ;
#29042 = CARTESIAN_POINT ( 'NONE',  ( -7.208316651077764980, 10.38393115100079100, -7.208316651077759651 ) ) ;
#29043 = VERTEX_POINT ( 'NONE', #6051 ) ;
#29044 = ORIENTED_EDGE ( 'NONE', *, *, #96550, .F. ) ;
#29045 = EDGE_LOOP ( 'NONE', ( #49812, #56430, #39875, #31536, #64427, #10433 ) ) ;
#29046 = CARTESIAN_POINT ( 'NONE',  ( 17.20831665107776587, 47.88393115100078745, 7.208316651077764980 ) ) ;
#29047 = CARTESIAN_POINT ( 'NONE',  ( 2.917880565312950480, 15.97041550158063217, -12.26659068614894821 ) ) ;
#29049 = CARTESIAN_POINT ( 'NONE',  ( 2.035157376598822676, 22.43868534415483396, -7.964842623401177768 ) ) ;
#29048 = CARTESIAN_POINT ( 'NONE',  ( 19.42250999205614193, 20.14701867748817321, 5.440088680355555262 ) ) ;
#29051 = CARTESIAN_POINT ( 'NONE',  ( 19.38216949554541202, 15.99863466993042138, 9.382169495545424454 ) ) ;
#29050 = CARTESIAN_POINT ( 'NONE',  ( 7.361572987183170547, 62.05059781766745886, 9.846743663894590881 ) ) ;
#29052 = CARTESIAN_POINT ( 'NONE',  ( -4.164238869374098151, 6.595415501580634832, -3.795296366450310543 ) ) ;
#29053 = B_SPLINE_CURVE_WITH_KNOTS ( 'NONE', 3,
 ( #95459, #3485, #88443, #50437, #71961, #87943 ),
 .UNSPECIFIED., .F., .F.,
 ( 4, 2, 4 ),
 ( 3.409110551494651432E-05, 0.0004400426677367951910, 0.0008459942299586437932 ),
 .UNSPECIFIED. ) ;
#29054 = CARTESIAN_POINT ( 'NONE',  ( 15.44008868035555793, 66.39701867748817676, -9.422509992056140149 ) ) ;
#29055 = CIRCLE ( 'NONE', #1965, 14.49999999999999822 ) ;
#29056 = B_SPLINE_CURVE_WITH_KNOTS ( 'NONE', 3,
 ( #98908, #46365, #54345, #84858, #85345, #53871, #76853, #69366, #39849, #45882 ),
 .UNSPECIFIED., .F., .F.,
 ( 4, 3, 3, 4 ),
 ( 1.734723475976807094E-17, 0.0006253016069560725148, 0.001250604074564909364, 0.002501455912506525721 ),
 .UNSPECIFIED. ) ;
#29057 = CARTESIAN_POINT ( 'NONE',  ( 19.38216949554541557, 37.24863466993041783, -9.382169495545420901 ) ) ;
#29058 = ORIENTED_EDGE ( 'NONE', *, *, #85472, .T. ) ;
#29059 = CARTESIAN_POINT ( 'NONE',  ( 7.361572987183169658, 34.96726448433411605, -9.846743663894592657 ) ) ;
#29060 = CARTESIAN_POINT ( 'NONE',  ( 15.44008868035555793, 11.39701867748817143, -9.422509992056140149 ) ) ;
#29061 = ORIENTED_EDGE ( 'NONE', *, *, #64702, .F. ) ;
#29062 = CARTESIAN_POINT ( 'NONE',  ( 19.42250999205614193, 5.147018677488171434, 5.440088680355555262 ) ) ;
#29063 = ORIENTED_EDGE ( 'NONE', *, *, #71677, .T. ) ;
#29064 = CARTESIAN_POINT ( 'NONE',  ( 4.559911319644449179, 42.23035201082151247, -9.422509992056141925 ) ) ;
#29065 = CARTESIAN_POINT ( 'NONE',  ( 12.91533473730992121, 64.52201867748817676, 10.88017736071110164 ) ) ;
#29066 = CARTESIAN_POINT ( 'NONE',  ( 7.084665262690076126, 69.10535201082151957, 10.88017736071109987 ) ) ;
#29067 = DIRECTION ( 'NONE',  ( 0.6494480483301745544, 0.000000000000000000, 0.7604059656000387024 ) ) ;
#29068 = CARTESIAN_POINT ( 'NONE',  ( 15.44008868035555260, 59.73035201082151247, 9.422509992056143702 ) ) ;
#29069 = CARTESIAN_POINT ( 'NONE',  ( -0.3289641300567998083, 53.07879003517447813, 5.963430220938281678 ) ) ;
#29070 = EDGE_CURVE ( 'NONE', #64436, #93697, #1494, .T. ) ;
#29073 = ORIENTED_EDGE ( 'NONE', *, *, #83340, .T. ) ;
#29072 = VECTOR ( 'NONE', #441, 1000.000000000000114 ) ;
#29071 = CARTESIAN_POINT ( 'NONE',  ( 11.19532980485324103, -77.48602862270493574, 4.000000000000000000 ) ) ;
#29074 = CARTESIAN_POINT ( 'NONE',  ( 17.20831665107776587, 27.88393115100078390, 7.208316651077764980 ) ) ;
#29075 = ORIENTED_EDGE ( 'NONE', *, *, #98332, .F. ) ;
#29076 = CARTESIAN_POINT ( 'NONE',  ( 10.00000000000000178, 62.25893115100078745, 9.846743663894594434 ) ) ;
#29077 = CARTESIAN_POINT ( 'NONE',  ( 4.850115630859590965, 0.04922511925147064066, 13.93278430610810936 ) ) ;
#29078 = AXIS2_PLACEMENT_3D ( 'NONE', #46305, #21841, #37341 ) ;
#29079 =( GEOMETRIC_REPRESENTATION_CONTEXT ( 3 ) GLOBAL_UNCERTAINTY_ASSIGNED_CONTEXT ( ( #25358 ) ) GLOBAL_UNIT_ASSIGNED_CONTEXT ( ( #93751, #40760, #70777 ) ) REPRESENTATION_CONTEXT ( 'NONE', 'WORKASPACE' ) );
#29080 = AXIS2_PLACEMENT_3D ( 'NONE', #42095, #59046, #13053 ) ;
#29081 = CARTESIAN_POINT ( 'NONE',  ( 10.00000000000000000, 0.5537488349139675359, -14.16423886937410082 ) ) ;
#29082 = DIRECTION ( 'NONE',  ( 0.000000000000000000, 0.000000000000000000, 1.000000000000000000 ) ) ;
#29083 = CARTESIAN_POINT ( 'NONE',  ( 15.00000000000000000, 60.50000000000000000, 6.000000000000000000 ) ) ;
#29084 = CARTESIAN_POINT ( 'NONE',  ( 10.00000000000000000, 39.75893115100078745, -9.846743663894594434 ) ) ;
#29085 = CARTESIAN_POINT ( 'NONE',  ( -0.8801773607110991993, 12.85535201082150358, -2.915334737309923874 ) ) ;
#29086 = DIRECTION ( 'NONE',  ( 0.000000000000000000, 0.000000000000000000, -1.000000000000000000 ) ) ;
#29087 = EDGE_LOOP ( 'NONE', ( #13161, #37588, #2003, #54058 ) ) ;
#29088 = CARTESIAN_POINT ( 'NONE',  ( -11.92686044187656691, 4.479976035794177136, -3.195792623639521324 ) ) ;
#29089 = CARTESIAN_POINT ( 'NONE',  ( 14.92337183194729633, 52.67559781766745175, 8.527530157486181039 ) ) ;
#29090 = DIRECTION ( 'NONE',  ( 0.000000000000000000, 1.000000000000000000, 0.000000000000000000 ) ) ;
#29091 = CARTESIAN_POINT ( 'NONE',  ( 3.591859063236761518, 19.95696800326375353, 11.09922568453594849 ) ) ;
#29092 = CARTESIAN_POINT ( 'NONE',  ( 5.076628168052704559, 15.17559781766745175, -8.527530157486179263 ) ) ;
#29093 = FACE_OUTER_BOUND ( 'NONE', #26095, .T. ) ;
#29094 = CARTESIAN_POINT ( 'NONE',  ( 12.63842701281683922, 19.55059781766745175, -9.846743663894590881 ) ) ;
#29095 = CARTESIAN_POINT ( 'NONE',  ( 1.472469842513823179, 66.42559781766745175, 4.923371831947296329 ) ) ;
#29096 = PRESENTATION_LAYER_ASSIGNMENT (  '', '', ( #54644 ) ) ;
#29097 = DIRECTION ( 'NONE',  ( 0.000000000000000000, 0.000000000000000000, 1.000000000000000000 ) ) ;
#29098 = ORIENTED_EDGE ( 'NONE', *, *, #62557, .F. ) ;
#29099 = CARTESIAN_POINT ( 'NONE',  ( 12.91533473730992121, 14.52201867748817143, 10.88017736071110164 ) ) ;
#29100 = CARTESIAN_POINT ( 'NONE',  ( -4.164238869374099927, 17.01208216824730357, 3.795296366450308767 ) ) ;
#29101 = CARTESIAN_POINT ( 'NONE',  ( 0.1532563361054100626, 30.80059781766744820, -2.638427012816831230 ) ) ;
#29102 = CARTESIAN_POINT ( 'NONE',  ( 15.44008868035555793, 61.39701867748817676, -9.422509992056140149 ) ) ;
#29104 = FACE_OUTER_BOUND ( 'NONE', #2353, .T. ) ;
#29103 = CARTESIAN_POINT ( 'NONE',  ( 6.565887622018943937, 45.16530133659708923, 12.81628187352647430 ) ) ;
#29105 = CARTESIAN_POINT ( 'NONE',  ( -0.8801773607111008646, 13.27201867748817143, 2.915334737309923430 ) ) ;
#29106 = CARTESIAN_POINT ( 'NONE',  ( 5.800000000000003375, 99.99999999999998579, -8.525133428036873795 ) ) ;
#29107 = DIRECTION ( 'NONE',  ( 0.7253743710122867450, 0.000000000000000000, -0.6883545756937550220 ) ) ;
#29108 = CARTESIAN_POINT ( 'NONE',  ( 0.6178305044545818747, -1.501365330069579951, -9.382169495545419124 ) ) ;
#29109 = CARTESIAN_POINT ( 'NONE',  ( 14.92337183194729988, 29.34226448433411960, -8.527530157486177487 ) ) ;
#29110 = CARTESIAN_POINT ( 'NONE',  ( -7.964842623401172439, -11.31131465584515361, 7.964842623401183097 ) ) ;
#29111 = CARTESIAN_POINT ( 'NONE',  ( 0.6178305044545818747, 38.49863466993042493, -9.382169495545419124 ) ) ;
#29112 = CARTESIAN_POINT ( 'NONE',  ( 4.431036607602467647, 14.49999999999999822, 14.33059365769914351 ) ) ;
#29114 = CARTESIAN_POINT ( 'NONE',  ( -13.40508947812168827, 15.00000000000000000, 5.527528931045992522 ) ) ;
#29113 = CARTESIAN_POINT ( 'NONE',  ( 10.00000000000000000, 46.81368534415484106, -10.88017736071110342 ) ) ;
#29115 = FACE_OUTER_BOUND ( 'NONE', #86617, .T. ) ;
#29116 = CARTESIAN_POINT ( 'NONE',  ( 4.559911319644449179, 38.89701867748817676, 9.422509992056141925 ) ) ;
#29117 = EDGE_CURVE ( 'NONE', #57472, #28657, #15539, .T. ) ;
#29119 = CARTESIAN_POINT ( 'NONE',  ( 0.5774900079438607392, 38.48035201082150536, 5.440088680355550821 ) ) ;
#29118 = TOROIDAL_SURFACE ( 'NONE', #88217, 14.49999999999999822, 0.5000000000000000000 ) ;
#29120 = LINE ( 'NONE', #53602, #4225 ) ;
#29121 = CARTESIAN_POINT ( 'NONE',  ( 20.88017736071110519, 60.56368534415484106, 2.639326808657452039E-16 ) ) ;
#29122 = EDGE_CURVE ( 'NONE', #10914, #59056, #5115, .T. ) ;
#29123 = ADVANCED_FACE ( 'NONE', ( #7037 ), #67039, .T. ) ;
#29124 = UNCERTAINTY_MEASURE_WITH_UNIT (LENGTH_MEASURE( 1.000000000000000082E-05 ), #59871, 'distance_accuracy_value', 'NONE');
#29125 = CARTESIAN_POINT ( 'NONE',  ( 7.361572987183169658, 34.96726448433411605, -9.846743663894592657 ) ) ;
#29126 = CARTESIAN_POINT ( 'NONE',  ( 2.035157376598824452, 8.688685344154839285, 7.964842623401179544 ) ) ;
#29127 = CARTESIAN_POINT ( 'NONE',  ( 10.00000000000000000, 17.87363466993041783, -12.81628187352647608 ) ) ;
#29128 = ORIENTED_EDGE ( 'NONE', *, *, #42368, .F. ) ;
#29129 = CARTESIAN_POINT ( 'NONE',  ( 0.5774900079438590739, 27.64701867748817676, -5.440088680355550821 ) ) ;
#29130 = CARTESIAN_POINT ( 'NONE',  ( 18.72515096720570327, 16.07228050351031712, -6.499999999999992006 ) ) ;
#29131 = CARTESIAN_POINT ( 'NONE',  ( 15.44008868035555260, 24.73035201082150891, 9.422509992056143702 ) ) ;
#29132 = CARTESIAN_POINT ( 'NONE',  ( -0.8801773607111009756, 63.06368534415484106, 1.068504757029289695E-15 ) ) ;
#29133 = CARTESIAN_POINT ( 'NONE',  ( 10.00000000000000000, 20.55374883491396787, -14.16423886937410082 ) ) ;
#29134 = CARTESIAN_POINT ( 'NONE',  ( 17.20831665107776587, 19.13393115100078035, -7.208316651077762316 ) ) ;
#29135 = CARTESIAN_POINT ( 'NONE',  ( 17.96484262340118221, 44.93868534415483396, 7.964842623401181321 ) ) ;
#29136 = CARTESIAN_POINT ( 'NONE',  ( 0.000000000000000000, 15.00000000000000000, 0.000000000000000000 ) ) ;
#29137 = DIRECTION ( 'NONE',  ( -6.608470384673550777E-17, -1.000000000000000000, 0.000000000000000000 ) ) ;
#29138 = ORIENTED_EDGE ( 'NONE', *, *, #21641, .T. ) ;
#29139 = CARTESIAN_POINT ( 'NONE',  ( -14.76100041229768856, 14.76930270348881002, -2.313205896731025391 ) ) ;
#29140 = CARTESIAN_POINT ( 'NONE',  ( 14.92337183194729988, 49.34226448433411605, -8.527530157486177487 ) ) ;
#29141 = EDGE_LOOP ( 'NONE', ( #19724, #82796, #75015, #15673 ) ) ;
#29142 = ORIENTED_EDGE ( 'NONE', *, *, #82411, .T. ) ;
#29143 = CARTESIAN_POINT ( 'NONE',  ( 10.00000000000000178, 23.05374883491397142, 14.16423886937410082 ) ) ;
#29144 = CARTESIAN_POINT ( 'NONE',  ( 22.26659068614895176, 24.72041550158063572, -7.082119434687042414 ) ) ;
#29145 = CARTESIAN_POINT ( 'NONE',  ( 20.88017736071110164, 65.35535201082150536, 2.915334737309930979 ) ) ;
#29146 = CARTESIAN_POINT ( 'NONE',  ( 22.26659068614894466, 63.88708216824730357, 7.082119434687054849 ) ) ;
#29147 = CARTESIAN_POINT ( 'NONE',  ( 5.076628168052704559, 65.17559781766745175, -8.527530157486179263 ) ) ;
#29148 = CARTESIAN_POINT ( 'NONE',  ( 14.92337183194729988, 49.34226448433411605, -8.527530157486177487 ) ) ;
#29150 = CARTESIAN_POINT ( 'NONE',  ( -1.099225684535947600, 3.706968003263753531, -6.408140936763238038 ) ) ;
#29149 = CARTESIAN_POINT ( 'NONE',  ( 10.00000000000000000, 51.81368534415484106, -10.88017736071110342 ) ) ;
#29151 = CARTESIAN_POINT ( 'NONE',  ( 2.917880565312950480, 15.97041550158063217, -12.26659068614894821 ) ) ;
#29152 = CARTESIAN_POINT ( 'NONE',  ( 4.559911319644449179, 13.89701867748817321, 9.422509992056141925 ) ) ;
#29153 = PRESENTATION_LAYER_ASSIGNMENT (  '', '', ( #57913 ) ) ;
#29154 = CARTESIAN_POINT ( 'NONE',  ( -0.8801773607111009756, 13.06368534415483929, 1.068504757029289695E-15 ) ) ;
#29155 = AXIS2_PLACEMENT_3D ( 'NONE', #25065, #27005, #71050 ) ;
#29156 = DIRECTION ( 'NONE',  ( 0.000000000000000000, 0.000000000000000000, 1.000000000000000000 ) ) ;
#29157 = CARTESIAN_POINT ( 'NONE',  ( 2.035157376598824452, 48.68868534415483396, 7.964842623401179544 ) ) ;
#29158 = EDGE_CURVE ( 'NONE', #10376, #14429, #90026, .T. ) ;
#29159 = CIRCLE ( 'NONE', #81821, 14.49999999999999822 ) ;
#29160 = CARTESIAN_POINT ( 'NONE',  ( 2.638427012816835227, -27.53273551566587329, 9.846743663894590881 ) ) ;
#29161 = ORIENTED_EDGE ( 'NONE', *, *, #95830, .T. ) ;
#29162 = CARTESIAN_POINT ( 'NONE',  ( 8.879999999999991900, 76.07179676972447169, -4.000000000000000000 ) ) ;
#29163 = AXIS2_PLACEMENT_3D ( 'NONE', #19286, #72761, #41326 ) ;
#29164 = ORIENTED_EDGE ( 'NONE', *, *, #98936, .T. ) ;
#29165 = CARTESIAN_POINT ( 'NONE',  ( 0.1532563361054082862, 31.21726448433412315, 2.638427012816831674 ) ) ;
#29166 = EDGE_LOOP ( 'NONE', ( #73609, #23930, #30669, #67153 ) ) ;
#29167 = CARTESIAN_POINT ( 'NONE',  ( 3.640395162852214650, 89.00000000000000000, -9.500000000000000000 ) ) ;
#29169 = CARTESIAN_POINT ( 'NONE',  ( 4.559911319644449179, 8.897018677488173211, 9.422509992056141925 ) ) ;
#29168 = CARTESIAN_POINT ( 'NONE',  ( 6.204703633549690345, 40.76208216824731778, -14.16423886937410259 ) ) ;
#29171 = CARTESIAN_POINT ( 'NONE',  ( 0.1532563361054082862, 46.21726448433411605, 2.638427012816831674 ) ) ;
#29170 = CARTESIAN_POINT ( 'NONE',  ( 17.20831665107776587, 17.88393115100078745, 7.208316651077764980 ) ) ;
#29172 = CARTESIAN_POINT ( 'NONE',  ( 3.836325488036083087, 0.5000000000000004441, 14.50112432709425114 ) ) ;
#29173 = DIRECTION ( 'NONE',  ( -0.000000000000000000, -1.000000000000000000, -0.000000000000000000 ) ) ;
#29174 = EDGE_CURVE ( 'NONE', #84535, #94230, #87512, .T. ) ;
#29175 = TOROIDAL_SURFACE ( 'NONE', #52929, 14.49999999999999822, 0.5000000000000000000 ) ;
#29176 = CARTESIAN_POINT ( 'NONE',  ( 14.92337183194729988, 4.342264484334117824, -8.527530157486177487 ) ) ;
#29177 = CARTESIAN_POINT ( 'NONE',  ( -9.382169495545422677, 23.49863466993043204, -9.382169495545417348 ) ) ;
#29178 = VERTEX_POINT ( 'NONE', #22048 ) ;
#29179 = CARTESIAN_POINT ( 'NONE',  ( 20.36894250292379738, 29.92874883491396432, -10.36894250292379027 ) ) ;
#29180 = CARTESIAN_POINT ( 'NONE',  ( -1.099225684535947600, 24.54030133659708923, 6.408140936763237150 ) ) ;
#29181 = VERTEX_POINT ( 'NONE', #45516 ) ;
#29182 = STYLED_ITEM ( 'NONE', ( #35539 ), #9315 ) ;
#29183 = CARTESIAN_POINT ( 'NONE',  ( 10.00000000000000000, 42.87363466993042493, -12.81628187352647608 ) ) ;
#29184 = CARTESIAN_POINT ( 'NONE',  ( 10.00000000000000178, 19.31368534415484106, 10.88017736071110342 ) ) ;
#29185 = CARTESIAN_POINT ( 'NONE',  ( 17.20831665107776587, 34.13393115100078745, -7.208316651077762316 ) ) ;
#29186 = CARTESIAN_POINT ( 'NONE',  ( 4.559911319644449179, 32.23035201082150536, -9.422509992056141925 ) ) ;
#29187 = CARTESIAN_POINT ( 'NONE',  ( 16.40814093676324603, 62.45696800326376064, -11.09922568453594671 ) ) ;
#29188 = DIRECTION ( 'NONE',  ( 0.000000000000000000, 1.000000000000000000, 0.000000000000000000 ) ) ;
#29189 = CARTESIAN_POINT ( 'NONE',  ( 14.92337183194729988, 49.34226448433411605, -8.527530157486177487 ) ) ;
#29190 = CARTESIAN_POINT ( 'NONE',  ( 0.1532563361054083140, 56.00893115100078745, 1.131784320476157264E-15 ) ) ;
#29191 = CARTESIAN_POINT ( 'NONE',  ( -3.836325488036279818, 14.49999999999999822, 14.50112432709419963 ) ) ;
#29192 =( GEOMETRIC_REPRESENTATION_CONTEXT ( 3 ) GLOBAL_UNCERTAINTY_ASSIGNED_CONTEXT ( ( #49495 ) ) GLOBAL_UNIT_ASSIGNED_CONTEXT ( ( #75690, #21720, #7706 ) ) REPRESENTATION_CONTEXT ( 'NONE', 'WORKASPACE' ) );
#29193 = CARTESIAN_POINT ( 'NONE',  ( -3.753761956877497585, 0.000000000000000000, 3.955639745193215706 ) ) ;
#29194 = DIRECTION ( 'NONE',  ( -1.049065152435176504E-16, 1.000000000000000000, -0.000000000000000000 ) ) ;
#29195 = DIRECTION ( 'NONE',  ( 0.000000000000000000, 0.000000000000000000, -1.000000000000000000 ) ) ;
#29196 = PLANE ( 'NONE',  #62126 ) ;
#29197 = CARTESIAN_POINT ( 'NONE',  ( 0.1532563361054083140, 16.00893115100078390, 1.131784320476157264E-15 ) ) ;
#29198 = CARTESIAN_POINT ( 'NONE',  ( -1.099225684535947600, 33.70696800326375353, -6.408140936763238038 ) ) ;
#29199 = DIRECTION ( 'NONE',  ( 0.000000000000000000, 1.000000000000000000, 0.000000000000000000 ) ) ;
#29200 = ORIENTED_EDGE ( 'NONE', *, *, #24417, .T. ) ;
#29201 = CARTESIAN_POINT ( 'NONE',  ( 19.84674366389459621, 53.50893115100078745, 7.409399052514197653E-17 ) ) ;
#29202 = DIRECTION ( 'NONE',  ( -1.000000000000000000, -0.000000000000000000, -0.000000000000000000 ) ) ;
#29203 = CARTESIAN_POINT ( 'NONE',  ( 12.63842701281683922, 44.55059781766745175, -9.846743663894590881 ) ) ;
#29204 = CARTESIAN_POINT ( 'NONE',  ( 17.08211943468705840, 40.13708216824731068, -12.26659068614894466 ) ) ;
#29205 = CARTESIAN_POINT ( 'NONE',  ( 5.076628168052704559, 45.17559781766745175, -8.527530157486179263 ) ) ;
#29206 = CARTESIAN_POINT ( 'NONE',  ( 21.09922568453594849, 41.20696800326375353, 6.408140936763242479 ) ) ;
#29208 = DIRECTION ( 'NONE',  ( -1.000000000000000000, 0.000000000000000000, 0.000000000000000000 ) ) ;
#29207 = CARTESIAN_POINT ( 'NONE',  ( -4.096035146099030300, 15.00000000000000000, 13.90943910019935714 ) ) ;
#29209 = CARTESIAN_POINT ( 'NONE',  ( 12.63842701281683922, 9.550597817667449974, -9.846743663894590881 ) ) ;
#29210 = CARTESIAN_POINT ( 'NONE',  ( -10.93781366033333313, 0.3640475087720989600, -10.26470809774081339 ) ) ;
#29211 = EDGE_CURVE ( 'NONE', #60175, #25131, #96965, .T. ) ;
#29212 = CARTESIAN_POINT ( 'NONE',  ( 10.00000000000000178, 47.25893115100078745, 9.846743663894594434 ) ) ;
#29213 = CARTESIAN_POINT ( 'NONE',  ( 15.44008868035555260, 39.73035201082150536, 9.422509992056143702 ) ) ;
#29214 = CARTESIAN_POINT ( 'NONE',  ( 5.076628168052703671, 41.84226448433411605, 8.527530157486179263 ) ) ;
#29215 = DIRECTION ( 'NONE',  ( -0.5075383629607084224, 0.000000000000000000, 0.8616291604415232674 ) ) ;
#29216 = CARTESIAN_POINT ( 'NONE',  ( -0.8801773607111009756, 43.06368534415484106, 1.068504757029289695E-15 ) ) ;
#29217 = VECTOR ( 'NONE', #53194, 1000.000000000000114 ) ;
#29218 = EDGE_LOOP ( 'NONE', ( #71486, #33139, #38912, #70482 ) ) ;
#29219 = AXIS2_PLACEMENT_3D ( 'NONE', #70338, #79789, #24837 ) ;
#29220 = CARTESIAN_POINT ( 'NONE',  ( -8.235571585149871865, 4.493033628982647798, -8.235571585149866536 ) ) ;
#29221 = CARTESIAN_POINT ( 'NONE',  ( 7.084665262690076126, 14.10535201082150358, 10.88017736071109987 ) ) ;
#29223 = CARTESIAN_POINT ( 'NONE',  ( 7.084665262690076126, 44.10535201082151247, 10.88017736071109987 ) ) ;
#29222 = CARTESIAN_POINT ( 'NONE',  ( 22.81628187352647785, 6.623634669930420493, 6.195893100308588602E-16 ) ) ;
#29224 = CARTESIAN_POINT ( 'NONE',  ( 20.88017736071110164, 55.35535201082149825, 2.915334737309930979 ) ) ;
#29225 = CARTESIAN_POINT ( 'NONE',  ( 6.683985746567200792, -73.15435785430807414, 2.500000000000000888 ) ) ;
#29227 = CARTESIAN_POINT ( 'NONE',  ( -46.51330368012592942, 100.8237035043309504, 9.500000000000191847 ) ) ;
#29226 = CARTESIAN_POINT ( 'NONE',  ( 0.5774900079438590739, 22.64701867748817321, -5.440088680355550821 ) ) ;
#29228 = CARTESIAN_POINT ( 'NONE',  ( 18.52753015748617571, 8.092264484334117824, 4.923371831947298993 ) ) ;
#29229 = CARTESIAN_POINT ( 'NONE',  ( 19.84674366389459266, 28.30059781766745886, 2.638427012816836559 ) ) ;
#29230 = CARTESIAN_POINT ( 'NONE',  ( -1.847340224724952629, 14.95077488074853456, 14.63671528203489558 ) ) ;
#29231 = MECHANICAL_DESIGN_GEOMETRIC_PRESENTATION_REPRESENTATION (  '', ( #16482 ), #54778 ) ;
#29232 = CARTESIAN_POINT ( 'NONE',  ( -7.082119434687044190, 17.63708216824730357, 12.26659068614894998 ) ) ;
#29233 = CARTESIAN_POINT ( 'NONE',  ( -2.816281873526473856, -0.6680319967362464695, 3.434112377981055619 ) ) ;
#29234 = EDGE_CURVE ( 'NONE', #50106, #57707, #5564, .T. ) ;
#29236 = CARTESIAN_POINT ( 'NONE',  ( -0.03932841506544072774, 18.12161441960501662, 6.397827110478939261 ) ) ;
#29235 = CARTESIAN_POINT ( 'NONE',  ( 17.96484262340118221, 4.938685344154837509, 7.964842623401181321 ) ) ;
#29237 = FACE_OUTER_BOUND ( 'NONE', #58482, .T. ) ;
#29238 = CARTESIAN_POINT ( 'NONE',  ( 20.36894250292379738, 9.928748834913966093, -10.36894250292379027 ) ) ;
#29239 = CARTESIAN_POINT ( 'NONE',  ( 22.26659068614895176, 49.72041550158063927, -7.082119434687042414 ) ) ;
#29240 = CARTESIAN_POINT ( 'NONE',  ( 10.00000000000000000, 1.813685344154837731, -10.88017736071110342 ) ) ;
#29241 = EDGE_CURVE ( 'NONE', #14567, #96338, #28545, .T. ) ;
#29242 = EDGE_LOOP ( 'NONE', ( #70038, #21086, #46632 ) ) ;
#29243 = CARTESIAN_POINT ( 'NONE',  ( 2.791683348922240793, 21.63393115100078745, 7.208316651077764092 ) ) ;
#29244 = CARTESIAN_POINT ( 'NONE',  ( 0.5774900079438590739, 12.64701867748817321, -5.440088680355550821 ) ) ;
#29245 = CARTESIAN_POINT ( 'NONE',  ( 18.52753015748618282, 48.92559781766745886, -4.923371831947291888 ) ) ;
#29247 = CARTESIAN_POINT ( 'NONE',  ( 0.000000000000000000, 0.5000000000000004441, 0.000000000000000000 ) ) ;
#29246 =( NAMED_UNIT ( * ) SI_UNIT ( $, .STERADIAN. ) SOLID_ANGLE_UNIT ( ) );
#29248 = CARTESIAN_POINT ( 'NONE',  ( 4.219999999999999751, 36.75000000000000000, -3.750000000000000000 ) ) ;
#29249 = ADVANCED_FACE ( 'NONE', ( #51543 ), #96886, .T. ) ;
#29250 = CARTESIAN_POINT ( 'NONE',  ( 0.6178305044545818747, 28.49863466993041783, -9.382169495545419124 ) ) ;
#29251 = CARTESIAN_POINT ( 'NONE',  ( 1.472469842513823179, 36.42559781766745175, 4.923371831947296329 ) ) ;
#29252 = VERTEX_POINT ( 'NONE', #76998 ) ;
#29253 = CARTESIAN_POINT ( 'NONE',  ( 10.00000000000000000, 9.758931151000785675, -9.846743663894594434 ) ) ;
#29254 = CARTESIAN_POINT ( 'NONE',  ( 11.40632470798694342, -69.21560994247114706, -3.750000000000000000 ) ) ;
#29255 = CYLINDRICAL_SURFACE ( 'NONE', #25173, 0.5000000000000004441 ) ;
#29256 = CARTESIAN_POINT ( 'NONE',  ( 17.96484262340118221, 16.18868534415483396, -7.964842623401177768 ) ) ;
#29257 = CARTESIAN_POINT ( 'NONE',  ( 10.00000000000000000, 35.55374883491396787, -14.16423886937410082 ) ) ;
#29258 = CARTESIAN_POINT ( 'NONE',  ( 12.91533473730992121, 44.52201867748816966, 10.88017736071110164 ) ) ;
#29259 = CARTESIAN_POINT ( 'NONE',  ( 17.96484262340118221, 64.93868534415483396, 7.964842623401181321 ) ) ;
#29260 = CARTESIAN_POINT ( 'NONE',  ( -12.25993886608611660, 0.5000000000000004441, 8.642563219313529999 ) ) ;
#29261 = CARTESIAN_POINT ( 'NONE',  ( 10.00000000000000178, 17.25893115100078745, 9.846743663894594434 ) ) ;
#29262 = CARTESIAN_POINT ( 'NONE',  ( -0.8801773607111009756, 3.063685344154837509, 1.068504757029289695E-15 ) ) ;
#29263 = CARTESIAN_POINT ( 'NONE',  ( 19.84674366389459621, 3.508931151000785231, 7.409399052514197653E-17 ) ) ;
#29264 = CARTESIAN_POINT ( 'NONE',  ( -46.78776334578036256, 100.7330867235808114, 9.217280700845517316 ) ) ;
#29265 = CARTESIAN_POINT ( 'NONE',  ( 18.52753015748618282, 33.92559781766745886, -4.923371831947291888 ) ) ;
#29266 = AXIS2_PLACEMENT_3D ( 'NONE', #19162, #58124, #72153 ) ;
#29267 = CARTESIAN_POINT ( 'NONE',  ( 0.5774900079438607392, 33.48035201082150536, 5.440088680355550821 ) ) ;
#29268 = CIRCLE ( 'NONE', #50038, 2.899999999999999023 ) ;
#29269 = ORIENTED_EDGE ( 'NONE', *, *, #81676, .F. ) ;
#29270 = CARTESIAN_POINT ( 'NONE',  ( 16.40814093676323893, 55.79030133659708923, 11.09922568453595026 ) ) ;
#29271 = CARTESIAN_POINT ( 'NONE',  ( 0.2510757737844357407, 80.99999999999994316, 0.000000000000000000 ) ) ;
#29272 = CARTESIAN_POINT ( 'NONE',  ( 17.20831665107776587, 7.883931151000784787, 7.208316651077764980 ) ) ;
#29273 = CARTESIAN_POINT ( 'NONE',  ( -2.816281873526471635, 48.91530133659708213, -3.434112377981056508 ) ) ;
#29275 = CARTESIAN_POINT ( 'NONE',  ( 0.1532563361054083140, 36.00893115100078745, 1.131784320476157264E-15 ) ) ;
#29274 = CARTESIAN_POINT ( 'NONE',  ( -0.8801773607111009756, 8.063685344154837509, 1.068504757029289695E-15 ) ) ;
#29276 = DIRECTION ( 'NONE',  ( 0.5547001962252290364, 0.8320502943378437211, 0.000000000000000000 ) ) ;
#29277 = CARTESIAN_POINT ( 'NONE',  ( -14.35840480524209894, 14.49999999999999112, 4.340070442838745102 ) ) ;
#29278 = CARTESIAN_POINT ( 'NONE',  ( 20.36894250292379382, 43.67874883491397497, 10.36894250292379205 ) ) ;
#29279 = CARTESIAN_POINT ( 'NONE',  ( 0.1532563361054100626, 45.80059781766745886, -2.638427012816831230 ) ) ;
#29280 = CARTESIAN_POINT ( 'NONE',  ( -7.750000000000000000, 80.32179676972448590, -4.250000000000000000 ) ) ;
#29281 = CARTESIAN_POINT ( 'NONE',  ( 15.44008868035555260, 39.73035201082150536, 9.422509992056143702 ) ) ;
#29282 = EDGE_CURVE ( 'NONE', #48771, #17080, #31398, .T. ) ;
#29283 = CARTESIAN_POINT ( 'NONE',  ( 19.84674366389459621, 3.508931151000785231, 7.409399052514197653E-17 ) ) ;
#29284 = EDGE_LOOP ( 'NONE', ( #65613, #85369, #29296, #28047 ) ) ;
#29285 = CARTESIAN_POINT ( 'NONE',  ( 16.40814093676324603, 52.45696800326375353, -11.09922568453594671 ) ) ;
#29286 = CARTESIAN_POINT ( 'NONE',  ( 5.076628168052704559, 0.1755978176674514724, -8.527530157486179263 ) ) ;
#29287 = ORIENTED_EDGE ( 'NONE', *, *, #60048, .F. ) ;
#29288 = CARTESIAN_POINT ( 'NONE',  ( -2.266590686148945544, 1.387082168247301128, -7.082119434687050408 ) ) ;
#29289 = CARTESIAN_POINT ( 'NONE',  ( 0.1532563361054082862, 6.217264484334118713, 2.638427012816831674 ) ) ;
#29290 = LINE ( 'NONE', #74288, #15327 ) ;
#29291 = ORIENTED_EDGE ( 'NONE', *, *, #91840, .F. ) ;
#29292 = CARTESIAN_POINT ( 'NONE',  ( 7.084665262690076126, 22.02201867748817321, -10.88017736071110164 ) ) ;
#29293 = VECTOR ( 'NONE', #89877, 1000.000000000000000 ) ;
#29295 = EDGE_CURVE ( 'NONE', #62733, #25669, #8994, .T. ) ;
#29294 = AXIS2_PLACEMENT_3D ( 'NONE', #41158, #71154, #86647 ) ;
#29296 = ORIENTED_EDGE ( 'NONE', *, *, #9727, .T. ) ;
#29297 = CARTESIAN_POINT ( 'NONE',  ( 10.00000000000000000, 36.81368534415484106, -10.88017736071110342 ) ) ;
#29298 = CARTESIAN_POINT ( 'NONE',  ( 5.076628168052703671, 66.84226448433412315, 8.527530157486179263 ) ) ;
#29299 = EDGE_LOOP ( 'NONE', ( #35072, #77263, #84584, #41938 ) ) ;
#29300 = ORIENTED_EDGE ( 'NONE', *, *, #71911, .F. ) ;
#29301 = STYLED_ITEM ( 'NONE', ( #33260 ), #77673 ) ;
#29302 = CARTESIAN_POINT ( 'NONE',  ( 12.91533473730993009, 66.60535201082150536, -10.88017736071109987 ) ) ;
#29303 = CARTESIAN_POINT ( 'NONE',  ( 2.393480905993186969, 14.49999999999999112, -14.80781041047757185 ) ) ;
#29305 = FACE_OUTER_BOUND ( 'NONE', #3751, .T. ) ;
#29304 = CARTESIAN_POINT ( 'NONE',  ( 12.91533473730992121, 24.52201867748816966, 10.88017736071110164 ) ) ;
#29306 = CARTESIAN_POINT ( 'NONE',  ( 2.791683348922240793, 6.633931151000785675, 7.208316651077764092 ) ) ;
#29307 = CARTESIAN_POINT ( 'NONE',  ( 20.88017736071110519, 20.56368534415484106, 2.639326808657452039E-16 ) ) ;
#29308 = VERTEX_POINT ( 'NONE', #31972 ) ;
#29309 = CARTESIAN_POINT ( 'NONE',  ( 0.6178305044545838731, 54.74863466993042493, 9.382169495545420901 ) ) ;
#29310 = CARTESIAN_POINT ( 'NONE',  ( 19.42250999205614193, 45.14701867748817676, 5.440088680355555262 ) ) ;
#29311 = DIRECTION ( 'NONE',  ( 0.2211055276381909129, 0.9752498888222635998, -0.000000000000000000 ) ) ;
#29312 = CARTESIAN_POINT ( 'NONE',  ( 21.09922568453595559, 52.04030133659708923, -6.408140936763230044 ) ) ;
#29313 = CARTESIAN_POINT ( 'NONE',  ( 15.44008868035555260, 49.73035201082150536, 9.422509992056143702 ) ) ;
#29314 = CARTESIAN_POINT ( 'NONE',  ( 14.92337183194729988, 64.34226448433412315, -8.527530157486177487 ) ) ;
#29315 = CARTESIAN_POINT ( 'NONE',  ( 15.96747533562963639, -0.03417435944610275333, -0.9576679184940652956 ) ) ;
#29316 = CARTESIAN_POINT ( 'NONE',  ( 19.84674366389459621, 13.50893115100078568, 7.409399052514197653E-17 ) ) ;
#29317 = CARTESIAN_POINT ( 'NONE',  ( 6.565887622018943937, 10.16530133659708746, 12.81628187352647430 ) ) ;
#29319 = CARTESIAN_POINT ( 'NONE',  ( 7.361572987183170547, 62.05059781766745886, 9.846743663894590881 ) ) ;
#29318 = SURFACE_SIDE_STYLE ('',( #54287 ) ) ;
#29320 = CARTESIAN_POINT ( 'NONE',  ( 7.084665262690076126, 32.02201867748816966, -10.88017736071110164 ) ) ;
#29321 = CARTESIAN_POINT ( 'NONE',  ( 17.20831665107776587, 47.88393115100078745, 7.208316651077764980 ) ) ;
#29322 =( LENGTH_UNIT ( ) NAMED_UNIT ( * ) SI_UNIT ( .MILLI., .METRE. ) );
#29323 = EDGE_CURVE ( 'NONE', #97221, #27349, #23531, .T. ) ;
#29324 = CARTESIAN_POINT ( 'NONE',  ( 14.92337183194729988, 9.342264484334119601, -8.527530157486177487 ) ) ;
#29326 = VERTEX_POINT ( 'NONE', #2015 ) ;
#29325 = CARTESIAN_POINT ( 'NONE',  ( 22.81628187352647785, 1.623634669930420271, 6.195893100308588602E-16 ) ) ;
#29327 = SURFACE_STYLE_FILL_AREA ( #95883 ) ;
#29328 = CARTESIAN_POINT ( 'NONE',  ( -5.204170427930421283E-15, 6.412123368507812948, -11.92686044187656513 ) ) ;
#29329 = CARTESIAN_POINT ( 'NONE',  ( 22.81628187352648496, 56.83196800326374643, -3.434112377981050290 ) ) ;
#29330 = CARTESIAN_POINT ( 'NONE',  ( 17.20831665107776587, 27.88393115100078390, 7.208316651077764980 ) ) ;
#29331 = CARTESIAN_POINT ( 'NONE',  ( 6.910443788714468738, -84.29081344360214700, -2.749999999994367617 ) ) ;
#29332 = CARTESIAN_POINT ( 'NONE',  ( 2.035157376598824452, 3.688685344154837953, 7.964842623401179544 ) ) ;
#29333 = CARTESIAN_POINT ( 'NONE',  ( 7.361572987183170547, 47.05059781766745175, 9.846743663894590881 ) ) ;
#29334 = ORIENTED_EDGE ( 'NONE', *, *, #22608, .T. ) ;
#29335 = CARTESIAN_POINT ( 'NONE',  ( 1.816707512666849045, 25.10290668512023871, -6.499999999999981348 ) ) ;
#29336 = CARTESIAN_POINT ( 'NONE',  ( -2.266590686148945544, 67.22041550158063217, 7.082119434687048631 ) ) ;
#29337 = CARTESIAN_POINT ( 'NONE',  ( 0.000000000000000000, 14.49999999999999822, 0.000000000000000000 ) ) ;
#29338 = CARTESIAN_POINT ( 'NONE',  ( 0.5774900079438590739, 22.64701867748817321, -5.440088680355550821 ) ) ;
#29339 = CARTESIAN_POINT ( 'NONE',  ( -4.164238869374099927, 52.01208216824729647, 3.795296366450308767 ) ) ;
#29341 = FACE_OUTER_BOUND ( 'NONE', #39661, .T. ) ;
#29340 = CARTESIAN_POINT ( 'NONE',  ( -2.266590686148945544, 57.22041550158063217, 7.082119434687048631 ) ) ;
#29342 = CARTESIAN_POINT ( 'NONE',  ( 18.52753015748618282, 3.925597817667451306, -4.923371831947291888 ) ) ;
#29343 = CARTESIAN_POINT ( 'NONE',  ( 19.84674366389459266, 23.30059781766745530, 2.638427012816836559 ) ) ;
#29344 = CARTESIAN_POINT ( 'NONE',  ( 19.38216949554541557, 2.248634669930420049, -9.382169495545420901 ) ) ;
#29345 = ORIENTED_EDGE ( 'NONE', *, *, #87540, .F. ) ;
#29346 = DIRECTION ( 'NONE',  ( -0.8870108331782183830, 0.000000000000000000, -0.4617486132350405170 ) ) ;
#29347 = EDGE_LOOP ( 'NONE', ( #90257, #21204, #72433, #4998 ) ) ;
#29348 = CARTESIAN_POINT ( 'NONE',  ( 1.816707512666854818, 40.10290668512022449, -6.500000000000003553 ) ) ;
#29349 = CARTESIAN_POINT ( 'NONE',  ( 0.1532563361054083140, 56.00893115100078745, 1.131784320476157264E-15 ) ) ;
#29350 = CARTESIAN_POINT ( 'NONE',  ( 20.36894250292379738, 9.928748834913966093, -10.36894250292379027 ) ) ;
#29351 = CARTESIAN_POINT ( 'NONE',  ( 7.361572987183169658, 24.96726448433412315, -9.846743663894592657 ) ) ;
#29352 = ADVANCED_FACE ( 'NONE', ( #54003 ), #39510, .T. ) ;
#29353 = CARTESIAN_POINT ( 'NONE',  ( 14.35840480524206697, 14.49999999999999112, -4.340070442838847242 ) ) ;
#29354 = ORIENTED_EDGE ( 'NONE', *, *, #5213, .F. ) ;
#29355 = CARTESIAN_POINT ( 'NONE',  ( 13.79529636645031943, 40.34541550158063217, -14.16423886937409904 ) ) ;
#29356 = CARTESIAN_POINT ( 'NONE',  ( 17.20831665107776587, 2.883931151000785231, 7.208316651077764980 ) ) ;
#29358 = CARTESIAN_POINT ( 'NONE',  ( -2.361121941888906672, 0.2301505397289878574, -14.75287579053852660 ) ) ;
#29357 = CARTESIAN_POINT ( 'NONE',  ( 2.831191079880678085, 79.91181047996344944, 9.500000000000000000 ) ) ;
#29359 = CARTESIAN_POINT ( 'NONE',  ( 0.5774900079438607392, 28.48035201082150891, 5.440088680355550821 ) ) ;
#29360 = CARTESIAN_POINT ( 'NONE',  ( 16.40814093676324603, 42.45696800326375353, -11.09922568453594671 ) ) ;
#29361 = ADVANCED_FACE ( 'NONE', ( #16009 ), #32613, .T. ) ;
#29362 = CARTESIAN_POINT ( 'NONE',  ( -2.816281873526473856, 29.12363466993041783, 9.499525473075851096E-16 ) ) ;
#29363 = CARTESIAN_POINT ( 'NONE',  ( 0.6178305044545838731, 64.74863466993043914, 9.382169495545420901 ) ) ;
#29364 = ORIENTED_EDGE ( 'NONE', *, *, #24514, .T. ) ;
#29365 = VECTOR ( 'NONE', #37741, 1000.000000000000114 ) ;
#29366 = CARTESIAN_POINT ( 'NONE',  ( 17.75000000000001776, 4.561680251642722724E-15, -3.750000000000000000 ) ) ;
#29367 = CARTESIAN_POINT ( 'NONE',  ( -10.09048698379360864, 46.92328126389585208, -3.000000000000000000 ) ) ;
#29368 = CARTESIAN_POINT ( 'NONE',  ( 24.16423886937409904, 44.09541550158063927, 3.795296366450317205 ) ) ;
#29369 = CARTESIAN_POINT ( 'NONE',  ( 24.16423886937410614, 4.512082168247300906, -3.795296366450302550 ) ) ;
#29370 = CARTESIAN_POINT ( 'NONE',  ( -0.8801773607111008646, 8.272018677488171434, 2.915334737309923430 ) ) ;
#29371 = CARTESIAN_POINT ( 'NONE',  ( 2.035157376598824452, 28.68868534415484106, 7.964842623401179544 ) ) ;
#29372 = DIRECTION ( 'NONE',  ( 0.000000000000000000, 0.000000000000000000, 1.000000000000000000 ) ) ;
#29373 = CARTESIAN_POINT ( 'NONE',  ( 26.00000000000000355, 35.99999999999997158, 7.000000000000000888 ) ) ;
#29374 = CARTESIAN_POINT ( 'NONE',  ( -0.8801773607110991993, 57.85535201082149825, -2.915334737309923874 ) ) ;
#29375 = CARTESIAN_POINT ( 'NONE',  ( -15.00000000000004974, 91.25000000000000000, 7.750000000000000000 ) ) ;
#29376 = CARTESIAN_POINT ( 'NONE',  ( 3.591859063236763294, 33.29030133659708213, -11.09922568453595026 ) ) ;
#29377 = CYLINDRICAL_SURFACE ( 'NONE', #17157, 0.5000000000000004441 ) ;
#29378 = CARTESIAN_POINT ( 'NONE',  ( -3.420591144908359027, 14.63595249122788999, -14.60477854057961800 ) ) ;
#29379 = CARTESIAN_POINT ( 'NONE',  ( 17.20831665107776587, 27.88393115100078390, 7.208316651077764980 ) ) ;
#29380 = CARTESIAN_POINT ( 'NONE',  ( 10.00000000000000178, 59.31368534415484106, 10.88017736071110342 ) ) ;
#29381 = CARTESIAN_POINT ( 'NONE',  ( 3.591859063236763294, 23.29030133659708568, -11.09922568453595026 ) ) ;
#29382 = DIRECTION ( 'NONE',  ( 0.000000000000000000, 1.000000000000000000, 0.000000000000000000 ) ) ;
#29383 = CARTESIAN_POINT ( 'NONE',  ( -0.8801773607110991993, 7.855352010821504471, -2.915334737309923874 ) ) ;
#29384 = CARTESIAN_POINT ( 'NONE',  ( 19.84674366389459266, 33.30059781766744464, 2.638427012816836559 ) ) ;
#29385 = CARTESIAN_POINT ( 'NONE',  ( 3.591859063236763294, 63.29030133659708923, -11.09922568453595026 ) ) ;
#29386 = CARTESIAN_POINT ( 'NONE',  ( 5.076628168052703671, 16.84226448433411960, 8.527530157486179263 ) ) ;
#29387 = CARTESIAN_POINT ( 'NONE',  ( -4.164238869374099039, 6.803748834913967869, 8.674139862899312516E-16 ) ) ;
#29388 = DIRECTION ( 'NONE',  ( 0.000000000000000000, 1.000000000000000000, 0.000000000000000000 ) ) ;
#29389 = CARTESIAN_POINT ( 'NONE',  ( 7.084665262690076126, 39.10535201082150536, 10.88017736071109987 ) ) ;
#29390 = CARTESIAN_POINT ( 'NONE',  ( 13.79529636645030344, 33.26208216824730357, 14.16423886937410614 ) ) ;
#29391 = CARTESIAN_POINT ( 'NONE',  ( 18.52753015748617571, 43.09226448433412315, 4.923371831947298993 ) ) ;
#29392 = CARTESIAN_POINT ( 'NONE',  ( -0.8801773607110991993, 32.85535201082151247, -2.915334737309923874 ) ) ;
#29393 = CARTESIAN_POINT ( 'NONE',  ( 4.559911319644449179, 22.23035201082150536, -9.422509992056141925 ) ) ;
#29394 = ORIENTED_EDGE ( 'NONE', *, *, #40916, .F. ) ;
#29395 =( BOUNDED_SURFACE ( )  B_SPLINE_SURFACE ( 1, 2, ( 
 ( #1843, #11280, #32301, #25328, #41799, #2338, #62805, #93305, #24829, #55306, #55814, #50252, #96278, #74741, #21257, #80769, #89253, #43254, #27258, #27754, #36757, #97773, #65750, #58238, #89738, #51754, #12263, #28748, #11774, #42282, #57758, #97274, #88757, #67249, #44237, #20269, #50766, #12756, #96778, #66750, #43746, #81258, #74232, #6253, #36254, #29238, #28254, #73748, #35756, #59239, #42773, #5279, #66243, #58749, #82238, #20765, #4781, #13752, #59736, #72754, #51253, #81739, #13254, #5765, #19278, #49762, #80273, #4288, #34761, #65250, #95779, #88261, #19766, #73255, #35254, #61220, #30217, #44735, #60233, #90728, #46703, #75235, #52243, #92213, #77202, #98270, #67750, #53228, #15255, #8232, #29726, #45732, #83732, #23244, #75731, #22254, #23739, #84236, #54201, #8708, #39224, #22745, #76712, #69712, #31203, #52729, #68733, #83236, #6745, #37263, #14759, #38725, #45232, #76233, #261, #30708, #61697, #84717, #98767, #7246, #16220, #37751, #60721, #68249, #7747, #1240, #91218, #38241, #91724, #53717, #751, #82736, #14255, #15743, #69225, #46227, #31696, #90231, #21763, #32679, #55695, #40691, #10681, #86682, #2220, #18186, #49165, #79168, #41684, #71191, #40194, #78686, #41197, #24710, #70701, #93680, #86192, #71676, #2714, #47693, #64148, #87155, #54686, #33168, #17704, #63173, #94167, #48174, #56188, #10197, #72154, #85209, #25214, #3187, #9698, #63662, #55180, #18680, #25698, #48667, #16713, #32181, #62683, #79668, #47186, #24221, #94666, #11164, #70207, #39717, #33653, #26175, #56667, #1726, #3682, #62187, #92697, #78185, #93183, #77689, #9204, #85697, #17215, #52979, #65633, #22016, #83493, #75491, #65137, #12639, #95658, #87649, #80149, #27142, #52490, #19163, #96157, #43136, #73629, #7003, #29980, #42654, #42174, #37508, #57645, #73130, #34639, #27640, #15012, #4171, #58125, #4672, #68001, #49641, #80655, #28136, #72638, #5153, #64638, #58635, #82997, #60485, #88140, #12149, #90974, #98527, #19653, #35641, #88635, #50145, #35133, #45481, #75983, #20142, #50647, #22507, #34144, #66127, #81137, #96657, #95146, #89136, #26656, #57152, #11660, #14515, #44984, #24971, #47451, #38491, #84962, #68985, #60971, #53472, #520, #24479, #91483, #38982, #16478, #46954, #77950, #1980, #15981, #15507, #9457, #30967, #46468, #7992, #69474, #85958, #76478, #31454, #76964, #39958, #23004, #53971, #1487, #45989, #77448, #38003, #31940, #54942, #32446, #61464, #84480, #62943, #70459, #91971, #8961, #61956, #23500, #8476, #55456, #17468, #993, #92455, #93446, #47935, #23983, #16971, #23, #30470, #54454, #85457, #39478 ),
 ( #69968, #7512, #62441, #92944, #68496, #83982, #41943, #63435, #71924, #79914, #72406, #56917, #57894, #49910, #78440, #33903, #40954, #11422, #49413, #87418, #95418, #17948, #80421, #41457, #3445, #3933, #40462, #88408, #48923, #18935, #64411, #63914, #65397, #94917, #57411, #72901, #70960, #27404, #42421, #86928, #26416, #79435, #34402, #95923, #25940, #33415, #11917, #4435, #78936, #64891, #18440, #19908, #34900, #56442, #10933, #26914, #87904, #19418, #9956, #2479, #32934, #93941, #25469, #55951, #86450, #48435, #10446, #71451, #2965, #94424, #81882, #74373, #67382, #28874, #35891, #52375, #75369, #42909, #21398, #5900, #89390, #82374, #36395, #44381, #97407, #29863, #73391, #51395, #90360, #96920, #58891, #43392, #6884, #51892, #20906, #4920, #20412, #50898, #37397, #35397, #12403, #82879, #67885, #58383, #27894, #13394, #66888, #97911, #88902, #59376, #43877, #13896, #66386, #81393, #14395, #74879, #44866, #98407, #60365, #89880, #36894, #90861, #21898, #12895, #6379, #73890, #65890, #96420, #5421, #29371, #28397, #59872, #50399, #80909, #92836, #16852, #30856, #30354, #62328, #53359, #61353, #22887, #53865, #1867, #91361, #46359, #91862, #24364, #75871, #68874, #16359, #60861, #881, #52868, #46840, #69856, #47327, #83866, #404, #77827, #54827, #15390, #92348, #76847, #45876, #23380, #39843, #32325, #84375, #15874, #85339, #9341, #76366, #31832, #14896, #45367, #7880, #1378, #8361, #38373, #38869, #70349, #62828, #69360, #31341, #22392, #83374, #61842, #7392, #37891, #68382, #23874, #98902, #54338, #84852, #77335, #8847, #39361, #86821, #71812, #41823, #18818, #33305, #49299, #80295, #11303, #72773, #3318, #71331, #10822, #72289, #55834, #2851, #25828, #18324, #3820, #33781, #78822, #95292, #19301, #85839, #64288, #48805, #63797, #26302, #79314, #87298, #41341, #4310, #17352, #94304, #34275, #40831, #56326, #86328, #49787, #94800, #56802, #47822, #63310, #93821, #11793, #78322, #55331, #26795, #42301, #2359, #70846, #79801, #64776, #57291, #32814, #87785, #34784, #93328, #10332, #25351, #24849, #9842, #40343, #17832, #48314, #96799, #51773, #82758, #6271, #96301, #43765, #27777, #19785, #12287, #58262, #82256, #50273, #28274, #74254, #5785, #36777, #59755, #73769, #73279, #67269, #88777, #5298, #65772, #58770, #44753, #35277, #89273, #35775, #97797, #80790, #12777, #59259, #4801, #36274, #95800, #89760, #13773, #90251, #20288, #43274, #21783, #29259, #50787, #66770, #44259, #97293, #81277, #52262, #14280, #57779, #28766, #20784, #66264, #21277, #51275, #74764, #13272, #75255, #88286, #81760, #6768, #65272, #27281 ) ),
 .UNSPECIFIED., .F., .F., .T. ) 
 B_SPLINE_SURFACE_WITH_KNOTS ( ( 2, 2 ),
 ( 3, 2, 2, 2, 2, 2, 2, 2, 2, 2, 2, 2, 2, 2, 2, 2, 2, 2, 2, 2, 2, 2, 2, 2, 2, 2, 2, 2, 2, 2, 2, 2, 2, 2, 2, 2, 2, 2, 2, 2, 2, 2, 2, 2, 2, 2, 2, 2, 2, 2, 2, 2, 2, 2, 2, 2, 2, 2, 2, 2, 2, 2, 2, 2, 2, 2, 2, 2, 2, 2, 2, 2, 2, 2, 2, 2, 2, 2, 2, 2, 2, 2, 2, 2, 2, 2, 2, 2, 2, 2, 2, 2, 2, 2, 2, 2, 2, 2, 2, 2, 2, 2, 2, 2, 2, 2, 2, 2, 2, 2, 2, 2, 2, 2, 2, 2, 2, 2, 2, 2, 2, 2, 2, 2, 2, 2, 2, 2, 2, 2, 2, 2, 2, 2, 2, 2, 2, 2, 2, 2, 2, 2, 2, 2, 2, 2, 2, 2, 2, 2, 2, 2, 2, 2, 2, 2, 2, 2, 2, 2, 2, 2, 3 ),
 ( 0.000000000000000000, 1.000000000000000000 ),
 ( 0.000000000000000000, 0.005952380952380952051, 0.01190476190476190410, 0.01785714285714285615, 0.02380952380952380820, 0.02976190476190476025, 0.03571428571428571230, 0.04166666666666666435, 0.04761904761904761640, 0.05357142857142856845, 0.05952380952380952051, 0.06547619047619047949, 0.07142857142857142461, 0.07738095238095238360, 0.08333333333333332871, 0.08928571428571428770, 0.09523809523809523281, 0.1011904761904761918, 0.1071428571428571369, 0.1130952380952380959, 0.1190476190476190410, 0.1250000000000000000, 0.1309523809523809590, 0.1369047619047619180, 0.1428571428571428492, 0.1488095238095238082, 0.1547619047619047672, 0.1607142857142857262, 0.1666666666666666574, 0.1726190476190476164, 0.1785714285714285754, 0.1845238095238095344, 0.1904761904761904656, 0.1964285714285714246, 0.2023809523809523836, 0.2083333333333333426, 0.2142857142857142738, 0.2202380952380952328, 0.2261904761904761918, 0.2321428571428571508, 0.2380952380952380820, 0.2440476190476190410, 0.2500000000000000000, 0.2559523809523809312, 0.2619047619047619180, 0.2678571428571428492, 0.2738095238095238360, 0.2797619047619047672, 0.2857142857142856984, 0.2916666666666666852, 0.2976190476190476164, 0.3035714285714285476, 0.3095238095238095344, 0.3154761904761904656, 0.3214285714285714524, 0.3273809523809523836, 0.3333333333333333148, 0.3392857142857143016, 0.3452380952380952328, 0.3511904761904761640, 0.3571428571428571508, 0.3630952380952380820, 0.3690476190476190688, 0.3750000000000000000, 0.3809523809523809312, 0.3869047619047619180, 0.3928571428571428492, 0.3988095238095238360, 0.4047619047619047672, 0.4107142857142856984, 0.4166666666666666852, 0.4226190476190476164, 0.4285714285714285476, 0.4345238095238095344, 0.4404761904761904656, 0.4464285714285714524, 0.4523809523809523836, 0.4583333333333333148, 0.4642857142857143016, 0.4702380952380952328, 0.4761904761904761640, 0.4821428571428571508, 0.4880952380952380820, 0.4940476190476190688, 0.5000000000000000000, 0.5059523809523809312, 0.5119047619047618625, 0.5178571428571429047, 0.5238095238095238360, 0.5297619047619047672, 0.5357142857142856984, 0.5416666666666666297, 0.5476190476190476719, 0.5535714285714286031, 0.5595238095238095344, 0.5654761904761904656, 0.5714285714285713969, 0.5773809523809523281, 0.5833333333333333703, 0.5892857142857143016, 0.5952380952380952328, 0.6011904761904761640, 0.6071428571428570953, 0.6130952380952381375, 0.6190476190476190688, 0.6250000000000000000, 0.6309523809523809312, 0.6369047619047618625, 0.6428571428571429047, 0.6488095238095238360, 0.6547619047619047672, 0.6607142857142856984, 0.6666666666666666297, 0.6726190476190476719, 0.6785714285714286031, 0.6845238095238095344, 0.6904761904761904656, 0.6964285714285713969, 0.7023809523809523281, 0.7083333333333333703, 0.7142857142857143016, 0.7202380952380952328, 0.7261904761904761640, 0.7321428571428570953, 0.7380952380952381375, 0.7440476190476190688, 0.7500000000000000000, 0.7559523809523809312, 0.7619047619047618625, 0.7678571428571429047, 0.7738095238095238360, 0.7797619047619047672, 0.7857142857142856984, 0.7916666666666666297, 0.7976190476190476719, 0.8035714285714286031, 0.8095238095238095344, 0.8154761904761904656, 0.8214285714285713969, 0.8273809523809523281, 0.8333333333333333703, 0.8392857142857143016, 0.8452380952380952328, 0.8511904761904761640, 0.8571428571428570953, 0.8630952380952381375, 0.8690476190476190688, 0.8750000000000000000, 0.8809523809523809312, 0.8869047619047618625, 0.8928571428571429047, 0.8988095238095238360, 0.9047619047619047672, 0.9107142857142856984, 0.9166666666666666297, 0.9226190476190476719, 0.9285714285714286031, 0.9345238095238095344, 0.9404761904761904656, 0.9464285714285713969, 0.9523809523809523281, 0.9583333333333333703, 0.9642857142857143016 ),
 .UNSPECIFIED. ) 
 GEOMETRIC_REPRESENTATION_ITEM ( )  RATIONAL_B_SPLINE_SURFACE ( (
 ( 1.000000000000000000, 0.9659258262890683122, 1.000000000000000000, 0.9659258262890683122, 1.000000000000000000, 0.9659258262890683122, 1.000000000000000000, 0.9659258262890683122, 1.000000000000000000, 0.9659258262890683122, 1.000000000000000000, 0.9659258262890683122, 1.000000000000000000, 0.9659258262890683122, 1.000000000000000000, 0.9659258262890683122, 1.000000000000000000, 0.9659258262890683122, 1.000000000000000000, 0.9659258262890683122, 1.000000000000000000, 0.9659258262890683122, 1.000000000000000000, 0.9659258262890683122, 1.000000000000000000, 0.9659258262890683122, 1.000000000000000000, 0.9659258262890683122, 1.000000000000000000, 0.9659258262890683122, 1.000000000000000000, 0.9659258262890683122, 1.000000000000000000, 0.9659258262890683122, 1.000000000000000000, 0.9659258262890683122, 1.000000000000000000, 0.9659258262890683122, 1.000000000000000000, 0.9659258262890683122, 1.000000000000000000, 0.9659258262890683122, 1.000000000000000000, 0.9659258262890683122, 1.000000000000000000, 0.9659258262890683122, 1.000000000000000000, 0.9659258262890683122, 1.000000000000000000, 0.9659258262890683122, 1.000000000000000000, 0.9659258262890683122, 1.000000000000000000, 0.9659258262890683122, 1.000000000000000000, 0.9659258262890683122, 1.000000000000000000, 0.9659258262890683122, 1.000000000000000000, 0.9659258262890683122, 1.000000000000000000, 0.9659258262890683122, 1.000000000000000000, 0.9659258262890683122, 1.000000000000000000, 0.9659258262890683122, 1.000000000000000000, 0.9659258262890683122, 1.000000000000000000, 0.9659258262890683122, 1.000000000000000000, 0.9659258262890683122, 1.000000000000000000, 0.9659258262890683122, 1.000000000000000000, 0.9659258262890683122, 1.000000000000000000, 0.9659258262890683122, 1.000000000000000000, 0.9659258262890683122, 1.000000000000000000, 0.9659258262890683122, 1.000000000000000000, 0.9659258262890683122, 1.000000000000000000, 0.9659258262890683122, 1.000000000000000000, 0.9659258262890683122, 1.000000000000000000, 0.9659258262890683122, 1.000000000000000000, 0.9659258262890683122, 1.000000000000000000, 0.9659258262890683122, 1.000000000000000000, 0.9659258262890683122, 1.000000000000000000, 0.9659258262890683122, 1.000000000000000000, 0.9659258262890683122, 1.000000000000000000, 0.9659258262890683122, 1.000000000000000000, 0.9659258262890683122, 1.000000000000000000, 0.9659258262890683122, 1.000000000000000000, 0.9659258262890683122, 1.000000000000000000, 0.9659258262890683122, 1.000000000000000000, 0.9659258262890683122, 1.000000000000000000, 0.9659258262890683122, 1.000000000000000000, 0.9659258262890683122, 1.000000000000000000, 0.9659258262890683122, 1.000000000000000000, 0.9659258262890683122, 1.000000000000000000, 0.9659258262890683122, 1.000000000000000000, 0.9659258262890683122, 1.000000000000000000, 0.9659258262890683122, 1.000000000000000000, 0.9659258262890683122, 1.000000000000000000, 0.9659258262890683122, 1.000000000000000000, 0.9659258262890683122, 1.000000000000000000, 0.9659258262890683122, 1.000000000000000000, 0.9659258262890683122, 1.000000000000000000, 0.9659258262890683122, 1.000000000000000000, 0.9659258262890683122, 1.000000000000000000, 0.9659258262890683122, 1.000000000000000000, 0.9659258262890683122, 1.000000000000000000, 0.9659258262890683122, 1.000000000000000000, 0.9659258262890683122, 1.000000000000000000, 0.9659258262890683122, 1.000000000000000000, 0.9659258262890683122, 1.000000000000000000, 0.9659258262890683122, 1.000000000000000000, 0.9659258262890683122, 1.000000000000000000, 0.9659258262890683122, 1.000000000000000000, 0.9659258262890683122, 1.000000000000000000, 0.9659258262890683122, 1.000000000000000000, 0.9659258262890683122, 1.000000000000000000, 0.9659258262890683122, 1.000000000000000000, 0.9659258262890683122, 1.000000000000000000, 0.9659258262890683122, 1.000000000000000000, 0.9659258262890683122, 1.000000000000000000, 0.9659258262890683122, 1.000000000000000000, 0.9659258262890683122, 1.000000000000000000, 0.9659258262890683122, 1.000000000000000000, 0.9659258262890683122, 1.000000000000000000, 0.9659258262890683122, 1.000000000000000000, 0.9659258262890683122, 1.000000000000000000, 0.9659258262890683122, 1.000000000000000000, 0.9659258262890683122, 1.000000000000000000, 0.9659258262890683122, 1.000000000000000000, 0.9659258262890683122, 1.000000000000000000, 0.9659258262890683122, 1.000000000000000000, 0.9659258262890683122, 1.000000000000000000, 0.9659258262890683122, 1.000000000000000000, 0.9659258262890683122, 1.000000000000000000, 0.9659258262890683122, 1.000000000000000000, 0.9659258262890683122, 1.000000000000000000, 0.9659258262890683122, 1.000000000000000000, 0.9659258262890683122, 1.000000000000000000, 0.9659258262890683122, 1.000000000000000000, 0.9659258262890683122, 1.000000000000000000, 0.9659258262890683122, 1.000000000000000000, 0.9659258262890683122, 1.000000000000000000, 0.9659258262890683122, 1.000000000000000000, 0.9659258262890683122, 1.000000000000000000, 0.9659258262890683122, 1.000000000000000000, 0.9659258262890683122, 1.000000000000000000, 0.9659258262890683122, 1.000000000000000000, 0.9659258262890683122, 1.000000000000000000, 0.9659258262890683122, 1.000000000000000000, 0.9659258262890683122, 1.000000000000000000, 0.9659258262890683122, 1.000000000000000000, 0.9659258262890683122, 1.000000000000000000, 0.9659258262890683122, 1.000000000000000000, 0.9659258262890683122, 1.000000000000000000, 0.9659258262890683122, 1.000000000000000000, 0.9659258262890683122, 1.000000000000000000, 0.9659258262890683122, 1.000000000000000000, 0.9659258262890683122, 1.000000000000000000, 0.9659258262890683122, 1.000000000000000000, 0.9659258262890683122, 1.000000000000000000, 0.9659258262890683122, 1.000000000000000000, 0.9659258262890683122, 1.000000000000000000, 0.9659258262890683122, 1.000000000000000000, 0.9659258262890683122, 1.000000000000000000, 0.9659258262890683122, 1.000000000000000000, 0.9659258262890683122, 1.000000000000000000, 0.9659258262890683122, 1.000000000000000000, 0.9659258262890683122, 1.000000000000000000, 0.9659258262890683122, 1.000000000000000000, 0.9659258262890683122, 1.000000000000000000, 0.9659258262890683122, 1.000000000000000000, 0.9659258262890683122, 1.000000000000000000, 0.9659258262890683122, 1.000000000000000000, 0.9659258262890683122, 1.000000000000000000, 0.9659258262890683122, 1.000000000000000000, 0.9659258262890683122, 1.000000000000000000, 0.9659258262890683122, 1.000000000000000000, 0.9659258262890683122, 1.000000000000000000, 0.9659258262890683122, 1.000000000000000000, 0.9659258262890683122, 1.000000000000000000, 0.9659258262890683122, 1.000000000000000000, 0.9659258262890683122, 1.000000000000000000, 0.9659258262890683122, 1.000000000000000000, 0.9659258262890683122, 1.000000000000000000, 0.9659258262890683122, 1.000000000000000000, 0.9659258262890683122, 1.000000000000000000, 0.9659258262890683122, 1.000000000000000000, 0.9659258262890683122, 1.000000000000000000, 0.9659258262890683122, 1.000000000000000000, 0.9659258262890683122, 1.000000000000000000, 0.9659258262890683122, 1.000000000000000000, 0.9659258262890683122, 1.000000000000000000, 0.9659258262890683122, 1.000000000000000000, 0.9659258262890683122, 1.000000000000000000, 0.9659258262890683122, 1.000000000000000000, 0.9659258262890683122, 1.000000000000000000),
 ( 1.000000000000000000, 0.9659258262890683122, 1.000000000000000000, 0.9659258262890683122, 1.000000000000000000, 0.9659258262890683122, 1.000000000000000000, 0.9659258262890683122, 1.000000000000000000, 0.9659258262890683122, 1.000000000000000000, 0.9659258262890683122, 1.000000000000000000, 0.9659258262890683122, 1.000000000000000000, 0.9659258262890683122, 1.000000000000000000, 0.9659258262890683122, 1.000000000000000000, 0.9659258262890683122, 1.000000000000000000, 0.9659258262890683122, 1.000000000000000000, 0.9659258262890683122, 1.000000000000000000, 0.9659258262890683122, 1.000000000000000000, 0.9659258262890683122, 1.000000000000000000, 0.9659258262890683122, 1.000000000000000000, 0.9659258262890683122, 1.000000000000000000, 0.9659258262890683122, 1.000000000000000000, 0.9659258262890683122, 1.000000000000000000, 0.9659258262890683122, 1.000000000000000000, 0.9659258262890683122, 1.000000000000000000, 0.9659258262890683122, 1.000000000000000000, 0.9659258262890683122, 1.000000000000000000, 0.9659258262890683122, 1.000000000000000000, 0.9659258262890683122, 1.000000000000000000, 0.9659258262890683122, 1.000000000000000000, 0.9659258262890683122, 1.000000000000000000, 0.9659258262890683122, 1.000000000000000000, 0.9659258262890683122, 1.000000000000000000, 0.9659258262890683122, 1.000000000000000000, 0.9659258262890683122, 1.000000000000000000, 0.9659258262890683122, 1.000000000000000000, 0.9659258262890683122, 1.000000000000000000, 0.9659258262890683122, 1.000000000000000000, 0.9659258262890683122, 1.000000000000000000, 0.9659258262890683122, 1.000000000000000000, 0.9659258262890683122, 1.000000000000000000, 0.9659258262890683122, 1.000000000000000000, 0.9659258262890683122, 1.000000000000000000, 0.9659258262890683122, 1.000000000000000000, 0.9659258262890683122, 1.000000000000000000, 0.9659258262890683122, 1.000000000000000000, 0.9659258262890683122, 1.000000000000000000, 0.9659258262890683122, 1.000000000000000000, 0.9659258262890683122, 1.000000000000000000, 0.9659258262890683122, 1.000000000000000000, 0.9659258262890683122, 1.000000000000000000, 0.9659258262890683122, 1.000000000000000000, 0.9659258262890683122, 1.000000000000000000, 0.9659258262890683122, 1.000000000000000000, 0.9659258262890683122, 1.000000000000000000, 0.9659258262890683122, 1.000000000000000000, 0.9659258262890683122, 1.000000000000000000, 0.9659258262890683122, 1.000000000000000000, 0.9659258262890683122, 1.000000000000000000, 0.9659258262890683122, 1.000000000000000000, 0.9659258262890683122, 1.000000000000000000, 0.9659258262890683122, 1.000000000000000000, 0.9659258262890683122, 1.000000000000000000, 0.9659258262890683122, 1.000000000000000000, 0.9659258262890683122, 1.000000000000000000, 0.9659258262890683122, 1.000000000000000000, 0.9659258262890683122, 1.000000000000000000, 0.9659258262890683122, 1.000000000000000000, 0.9659258262890683122, 1.000000000000000000, 0.9659258262890683122, 1.000000000000000000, 0.9659258262890683122, 1.000000000000000000, 0.9659258262890683122, 1.000000000000000000, 0.9659258262890683122, 1.000000000000000000, 0.9659258262890683122, 1.000000000000000000, 0.9659258262890683122, 1.000000000000000000, 0.9659258262890683122, 1.000000000000000000, 0.9659258262890683122, 1.000000000000000000, 0.9659258262890683122, 1.000000000000000000, 0.9659258262890683122, 1.000000000000000000, 0.9659258262890683122, 1.000000000000000000, 0.9659258262890683122, 1.000000000000000000, 0.9659258262890683122, 1.000000000000000000, 0.9659258262890683122, 1.000000000000000000, 0.9659258262890683122, 1.000000000000000000, 0.9659258262890683122, 1.000000000000000000, 0.9659258262890683122, 1.000000000000000000, 0.9659258262890683122, 1.000000000000000000, 0.9659258262890683122, 1.000000000000000000, 0.9659258262890683122, 1.000000000000000000, 0.9659258262890683122, 1.000000000000000000, 0.9659258262890683122, 1.000000000000000000, 0.9659258262890683122, 1.000000000000000000, 0.9659258262890683122, 1.000000000000000000, 0.9659258262890683122, 1.000000000000000000, 0.9659258262890683122, 1.000000000000000000, 0.9659258262890683122, 1.000000000000000000, 0.9659258262890683122, 1.000000000000000000, 0.9659258262890683122, 1.000000000000000000, 0.9659258262890683122, 1.000000000000000000, 0.9659258262890683122, 1.000000000000000000, 0.9659258262890683122, 1.000000000000000000, 0.9659258262890683122, 1.000000000000000000, 0.9659258262890683122, 1.000000000000000000, 0.9659258262890683122, 1.000000000000000000, 0.9659258262890683122, 1.000000000000000000, 0.9659258262890683122, 1.000000000000000000, 0.9659258262890683122, 1.000000000000000000, 0.9659258262890683122, 1.000000000000000000, 0.9659258262890683122, 1.000000000000000000, 0.9659258262890683122, 1.000000000000000000, 0.9659258262890683122, 1.000000000000000000, 0.9659258262890683122, 1.000000000000000000, 0.9659258262890683122, 1.000000000000000000, 0.9659258262890683122, 1.000000000000000000, 0.9659258262890683122, 1.000000000000000000, 0.9659258262890683122, 1.000000000000000000, 0.9659258262890683122, 1.000000000000000000, 0.9659258262890683122, 1.000000000000000000, 0.9659258262890683122, 1.000000000000000000, 0.9659258262890683122, 1.000000000000000000, 0.9659258262890683122, 1.000000000000000000, 0.9659258262890683122, 1.000000000000000000, 0.9659258262890683122, 1.000000000000000000, 0.9659258262890683122, 1.000000000000000000, 0.9659258262890683122, 1.000000000000000000, 0.9659258262890683122, 1.000000000000000000, 0.9659258262890683122, 1.000000000000000000, 0.9659258262890683122, 1.000000000000000000, 0.9659258262890683122, 1.000000000000000000, 0.9659258262890683122, 1.000000000000000000, 0.9659258262890683122, 1.000000000000000000, 0.9659258262890683122, 1.000000000000000000, 0.9659258262890683122, 1.000000000000000000, 0.9659258262890683122, 1.000000000000000000, 0.9659258262890683122, 1.000000000000000000, 0.9659258262890683122, 1.000000000000000000, 0.9659258262890683122, 1.000000000000000000, 0.9659258262890683122, 1.000000000000000000, 0.9659258262890683122, 1.000000000000000000, 0.9659258262890683122, 1.000000000000000000, 0.9659258262890683122, 1.000000000000000000, 0.9659258262890683122, 1.000000000000000000, 0.9659258262890683122, 1.000000000000000000, 0.9659258262890683122, 1.000000000000000000, 0.9659258262890683122, 1.000000000000000000, 0.9659258262890683122, 1.000000000000000000, 0.9659258262890683122, 1.000000000000000000, 0.9659258262890683122, 1.000000000000000000, 0.9659258262890683122, 1.000000000000000000, 0.9659258262890683122, 1.000000000000000000, 0.9659258262890683122, 1.000000000000000000, 0.9659258262890683122, 1.000000000000000000, 0.9659258262890683122, 1.000000000000000000, 0.9659258262890683122, 1.000000000000000000, 0.9659258262890683122, 1.000000000000000000, 0.9659258262890683122, 1.000000000000000000, 0.9659258262890683122, 1.000000000000000000, 0.9659258262890683122, 1.000000000000000000, 0.9659258262890683122, 1.000000000000000000, 0.9659258262890683122, 1.000000000000000000, 0.9659258262890683122, 1.000000000000000000, 0.9659258262890683122, 1.000000000000000000, 0.9659258262890683122, 1.000000000000000000, 0.9659258262890683122, 1.000000000000000000, 0.9659258262890683122, 1.000000000000000000, 0.9659258262890683122, 1.000000000000000000, 0.9659258262890683122, 1.000000000000000000) ) ) 
 REPRESENTATION_ITEM ( '' )  SURFACE ( )  );
#29396 = CARTESIAN_POINT ( 'NONE',  ( -0.8801773607110991993, 27.85535201082150181, -2.915334737309923874 ) ) ;
#29397 = CARTESIAN_POINT ( 'NONE',  ( 3.591859063236761518, 44.95696800326376064, 11.09922568453594849 ) ) ;
#29398 = CARTESIAN_POINT ( 'NONE',  ( 2.035157376598824452, 38.68868534415483396, 7.964842623401179544 ) ) ;
#29400 = CARTESIAN_POINT ( 'NONE',  ( 7.084665262690076126, 44.10535201082151247, 10.88017736071109987 ) ) ;
#29399 = DIRECTION ( 'NONE',  ( -0.000000000000000000, 0.000000000000000000, 1.000000000000000000 ) ) ;
#29401 = ORIENTED_EDGE ( 'NONE', *, *, #9740, .T. ) ;
#29402 = CARTESIAN_POINT ( 'NONE',  ( 10.00000000000000178, 57.25893115100078745, 9.846743663894594434 ) ) ;
#29403 = CARTESIAN_POINT ( 'NONE',  ( 0.5774900079438590739, 32.64701867748816966, -5.440088680355550821 ) ) ;
#29404 = FACE_OUTER_BOUND ( 'NONE', #73995, .T. ) ;
#29405 = CARTESIAN_POINT ( 'NONE',  ( -0.3689425029237898834, 41.17874883491397497, -10.36894250292378850 ) ) ;
#29406 = CARTESIAN_POINT ( 'NONE',  ( 20.88017736071110519, 55.56368534415484817, 2.639326808657452039E-16 ) ) ;
#29407 = CARTESIAN_POINT ( 'NONE',  ( 20.10421743870886857, 25.60736173766202839, -6.337391062633416006 ) ) ;
#29408 = CARTESIAN_POINT ( 'NONE',  ( -3.999999999999994671, 43.00000000000000711, -6.500000000000000888 ) ) ;
#29409 = CARTESIAN_POINT ( 'NONE',  ( 2.791683348922240793, 66.63393115100079456, 7.208316651077764092 ) ) ;
#29410 = CARTESIAN_POINT ( 'NONE',  ( 17.20831665107776587, 29.13393115100078390, -7.208316651077762316 ) ) ;
#29411 = ORIENTED_EDGE ( 'NONE', *, *, #75409, .T. ) ;
#29412 = CARTESIAN_POINT ( 'NONE',  ( 0.1532563361054082862, 21.21726448433412315, 2.638427012816831674 ) ) ;
#29413 = CARTESIAN_POINT ( 'NONE',  ( 12.81628187352647608, -18.37636533006957507, -2.602085213965210642E-15 ) ) ;
#29414 = CARTESIAN_POINT ( 'NONE',  ( 7.084665262690076126, 29.10535201082150181, 10.88017736071109987 ) ) ;
#29415 = CARTESIAN_POINT ( 'NONE',  ( 7.361572987183169658, 19.96726448433411960, -9.846743663894592657 ) ) ;
#29416 = CARTESIAN_POINT ( 'NONE',  ( 6.565887622018943937, 15.16530133659708568, 12.81628187352647430 ) ) ;
#29418 = CARTESIAN_POINT ( 'NONE',  ( 20.88017736071110875, 55.77201867748816966, -2.915334737309920765 ) ) ;
#29417 = CARTESIAN_POINT ( 'NONE',  ( 7.084665262690076126, 69.10535201082151957, 10.88017736071109987 ) ) ;
#29420 = CARTESIAN_POINT ( 'NONE',  ( 0.5774900079438590739, 2.647018677488170990, -5.440088680355550821 ) ) ;
#29419 = CARTESIAN_POINT ( 'NONE',  ( 19.42250999205614193, 35.14701867748816966, 5.440088680355555262 ) ) ;
#29422 = B_SPLINE_CURVE_WITH_KNOTS ( 'NONE', 3,
 ( #79137, #78657, #10648, #57608 ),
 .UNSPECIFIED., .F., .F.,
 ( 4, 4 ),
 ( 3.469446951953614189E-18, 0.002562518741975320334 ),
 .UNSPECIFIED. ) ;
#29421 = CARTESIAN_POINT ( 'NONE',  ( -0.3689425029237898834, 46.17874883491397497, -10.36894250292378850 ) ) ;
#29423 = CIRCLE ( 'NONE', #24668, 0.09999999999999939493 ) ;
#29424 = PLANE ( 'NONE',  #72231 ) ;
#29425 = ORIENTED_EDGE ( 'NONE', *, *, #4975, .T. ) ;
#29426 = CARTESIAN_POINT ( 'NONE',  ( 16.40814093676324603, 12.45696800326375353, -11.09922568453594671 ) ) ;
#29427 = CARTESIAN_POINT ( 'NONE',  ( 7.084665262690076126, 9.105352010821503583, 10.88017736071109987 ) ) ;
#29428 = CARTESIAN_POINT ( 'NONE',  ( 10.00000000000000000, 41.81368534415484106, -10.88017736071110342 ) ) ;
#29429 = DIRECTION ( 'NONE',  ( 0.9969173337331278528, -0.000000000000000000, 0.07845909572784538766 ) ) ;
#29430 = ORIENTED_EDGE ( 'NONE', *, *, #76753, .T. ) ;
#29431 = CARTESIAN_POINT ( 'NONE',  ( 4.559911319644449179, 58.89701867748817676, 9.422509992056141925 ) ) ;
#29432 = CARTESIAN_POINT ( 'NONE',  ( 0.1532563361054082862, 41.21726448433411605, 2.638427012816831674 ) ) ;
#29433 = CARTESIAN_POINT ( 'NONE',  ( 5.076628168052704559, 20.17559781766745175, -8.527530157486179263 ) ) ;
#29434 = CARTESIAN_POINT ( 'NONE',  ( 7.361572987183169658, 9.967264484334119601, -9.846743663894592657 ) ) ;
#29436 = CARTESIAN_POINT ( 'NONE',  ( 19.38216949554541557, 37.24863466993041783, -9.382169495545420901 ) ) ;
#29435 = CARTESIAN_POINT ( 'NONE',  ( -6.822528426060553208, -84.39592987140930802, 2.500000000000000000 ) ) ;
#29437 = EDGE_CURVE ( 'NONE', #91084, #87032, #12409, .T. ) ;
#29439 = DIRECTION ( 'NONE',  ( 0.000000000000000000, 0.000000000000000000, 1.000000000000000000 ) ) ;
#29438 = CARTESIAN_POINT ( 'NONE',  ( 10.00000000000000178, 64.31368534415483396, 10.88017736071110342 ) ) ;
#29440 = CARTESIAN_POINT ( 'NONE',  ( 6.825220758711188829, -50.90060425938847288, -4.000000000000000000 ) ) ;
#29442 = ORIENTED_EDGE ( 'NONE', *, *, #84593, .F. ) ;
#29441 = CARTESIAN_POINT ( 'NONE',  ( 19.84674366389459266, 38.71726448433412315, -2.638427012816827677 ) ) ;
#29443 = CARTESIAN_POINT ( 'NONE',  ( 3.591859063236761518, 49.95696800326375353, 11.09922568453594849 ) ) ;
#29444 = LINE ( 'NONE', #65973, #10257 ) ;
#29445 = CARTESIAN_POINT ( 'NONE',  ( 21.09922568453595559, 17.04030133659708923, -6.408140936763230044 ) ) ;
#29446 = CARTESIAN_POINT ( 'NONE',  ( 24.16423886937410614, 29.51208216824729647, -3.795296366450302550 ) ) ;
#29447 = UNCERTAINTY_MEASURE_WITH_UNIT (LENGTH_MEASURE( 1.000000000000000082E-05 ), #97388, 'distance_accuracy_value', 'NONE');
#29448 = CARTESIAN_POINT ( 'NONE',  ( 1.711636803080561098, 41.84492782695770785, -6.500000000000035527 ) ) ;
#29449 = CARTESIAN_POINT ( 'NONE',  ( 24.16423886937410614, 29.51208216824729647, -3.795296366450302550 ) ) ;
#29450 = CARTESIAN_POINT ( 'NONE',  ( 13.79529636645031943, 45.34541550158062506, -14.16423886937409904 ) ) ;
#29451 = CARTESIAN_POINT ( 'NONE',  ( 20.36894250292379738, 4.928748834913967869, -10.36894250292379027 ) ) ;
#29452 = CARTESIAN_POINT ( 'NONE',  ( 17.08211943468705840, 10.13708216824730179, -12.26659068614894466 ) ) ;
#29453 = CARTESIAN_POINT ( 'NONE',  ( 15.44008868035555793, 46.39701867748817676, -9.422509992056140149 ) ) ;
#29454 = DIRECTION ( 'NONE',  ( 1.483861936729427615E-16, -1.000000000000000000, -0.000000000000000000 ) ) ;
#29455 = CARTESIAN_POINT ( 'NONE',  ( 2.791683348922237240, 30.38393115100078390, -7.208316651077763204 ) ) ;
#29457 = CARTESIAN_POINT ( 'NONE',  ( 5.076628168052704559, 35.17559781766745175, -8.527530157486179263 ) ) ;
#29456 = CARTESIAN_POINT ( 'NONE',  ( 10.00000000000000178, 64.31368534415483396, 10.88017736071110342 ) ) ;
#29458 = CARTESIAN_POINT ( 'NONE',  ( 0.5774900079438590739, 27.64701867748817676, -5.440088680355550821 ) ) ;
#29459 = CARTESIAN_POINT ( 'NONE',  ( 13.43411237798105340, 60.58196800326376064, 12.81628187352647963 ) ) ;
#29460 = CARTESIAN_POINT ( 'NONE',  ( 19.84674366389459266, 63.71726448433412315, -2.638427012816827677 ) ) ;
#29461 = VECTOR ( 'NONE', #45666, 1000.000000000000114 ) ;
#29462 = SURFACE_SIDE_STYLE ('',( #66989 ) ) ;
#29463 = CARTESIAN_POINT ( 'NONE',  ( 5.076628168052704559, 25.17559781766745175, -8.527530157486179263 ) ) ;
#29464 = CARTESIAN_POINT ( 'NONE',  ( 3.591859063236761518, 39.95696800326375353, 11.09922568453594849 ) ) ;
#29465 = CARTESIAN_POINT ( 'NONE',  ( -5.204170427930421283E-15, -19.44625116508602503, -14.16423886937410082 ) ) ;
#29466 = CARTESIAN_POINT ( 'NONE',  ( -0.8801773607111009756, 38.06368534415484106, 1.068504757029289695E-15 ) ) ;
#29467 = CARTESIAN_POINT ( 'NONE',  ( 7.361572987183169658, 49.96726448433410894, -9.846743663894592657 ) ) ;
#29468 = CARTESIAN_POINT ( 'NONE',  ( 13.79529636645031943, 20.34541550158063572, -14.16423886937409904 ) ) ;
#29469 = ADVANCED_FACE ( 'NONE', ( #70966 ), #95424, .F. ) ;
#29470 = ORIENTED_EDGE ( 'NONE', *, *, #46893, .T. ) ;
#29471 = CARTESIAN_POINT ( 'NONE',  ( 17.96484262340118221, 61.18868534415482685, -7.964842623401177768 ) ) ;
#29472 = CARTESIAN_POINT ( 'NONE',  ( 10.93781366033342017, 14.63606902047321334, 10.26470809774076187 ) ) ;
#29473 = CARTESIAN_POINT ( 'NONE',  ( 13.79529636645030344, 63.26208216824730357, 14.16423886937410614 ) ) ;
#29474 = CARTESIAN_POINT ( 'NONE',  ( 0.6178305044545818747, -1.501365330069579951, -9.382169495545419124 ) ) ;
#29475 = CARTESIAN_POINT ( 'NONE',  ( 0.1922240491738437529, 53.18878173731740588, 6.499999999999968026 ) ) ;
#29476 = CARTESIAN_POINT ( 'NONE',  ( 19.42250999205614548, 55.98035201082150536, -5.440088680355545492 ) ) ;
#29477 = CARTESIAN_POINT ( 'NONE',  ( 2.603489959281614308, 56.58210964143329846, 6.500000000000031086 ) ) ;
#29478 = CARTESIAN_POINT ( 'NONE',  ( 2.915334737309928315, 24.52201867748817676, 10.88017736071109987 ) ) ;
#29479 = CARTESIAN_POINT ( 'NONE',  ( -0.8801773607111009756, 8.063685344154837509, 1.068504757029289695E-15 ) ) ;
#29480 = CARTESIAN_POINT ( 'NONE',  ( 0.5774900079438590739, 7.647018677488171434, -5.440088680355550821 ) ) ;
#29481 = AXIS2_PLACEMENT_3D ( 'NONE', #82778, #90770, #98308 ) ;
#29482 = CARTESIAN_POINT ( 'NONE',  ( 0.1532563361054100626, 50.80059781766745175, -2.638427012816831230 ) ) ;
#29483 = CARTESIAN_POINT ( 'NONE',  ( -2.816281873526473856, 49.33196800326374643, 3.434112377981055619 ) ) ;
#29484 = SURFACE_STYLE_USAGE ( .BOTH. , #14022 ) ;
#29485 = EDGE_LOOP ( 'NONE', ( #89752, #16624, #86138, #91933 ) ) ;
#29486 = CARTESIAN_POINT ( 'NONE',  ( 12.91533473730993009, 16.60535201082150891, -10.88017736071109987 ) ) ;
#29487 = CARTESIAN_POINT ( 'NONE',  ( -2.816281873526471635, 13.91530133659708746, -3.434112377981056508 ) ) ;
#29488 = DIRECTION ( 'NONE',  ( -0.000000000000000000, 0.000000000000000000, 1.000000000000000000 ) ) ;
#29489 = CARTESIAN_POINT ( 'NONE',  ( 5.076628168052703671, 6.842264484334118713, 8.527530157486179263 ) ) ;
#29490 = CARTESIAN_POINT ( 'NONE',  ( 14.92337183194729633, 42.67559781766745886, 8.527530157486181039 ) ) ;
#29491 = CARTESIAN_POINT ( 'NONE',  ( -0.8801773607111008646, 38.27201867748816255, 2.915334737309923430 ) ) ;
#29492 = VECTOR ( 'NONE', #50386, 1000.000000000000000 ) ;
#29493 = CARTESIAN_POINT ( 'NONE',  ( 13.43411237798106583, 2.665301336597086568, -12.81628187352647252 ) ) ;
#29495 = DIRECTION ( 'NONE',  ( 0.000000000000000000, 0.000000000000000000, -1.000000000000000000 ) ) ;
#29494 = CARTESIAN_POINT ( 'NONE',  ( 2.035157376598822676, 42.43868534415483396, -7.964842623401177768 ) ) ;
#29496 =( BOUNDED_SURFACE ( )  B_SPLINE_SURFACE ( 1, 2, ( 
 ( #97537, #57038, #95543, #50529, #87542, #80538, #12036, #74010, #66017, #51517, #42536, #73019, #89023, #4552, #20533, #74505, #35018, #28520, #82011, #65519, #88525, #43030, #13016, #27033, #5039, #72525, #57531, #51017, #81511, #36524, #88027, #43514, #96041, #27525, #19053, #81024, #13521, #66519, #80037, #58016, #5538, #44003, #23013, #46479, #38992, #75004, #53481, #7011, #90984, #37015, #83007, #28996, #30976, #29988, #83991, #22515, #14524, #7520, #76488, #90488, #67512, #15516, #68994, #52987, #21523, #30480, #75500, #84489, #53980, #60495, #61473, #29486, #52017, #529, #45998, #68009, #69484, #15020, #68503, #8002, #22025, #37517, #83502, #45489, #38500, #38011, #44992, #44504, #75991, #82508, #59507, #34, #98536, #60980, #91493, #98031, #91980, #8487, #23509, #15991, #76974, #90003, #14024, #6508, #59995, #52497, #24488, #77458, #33425, #2490, #8971, #25949, #10455, #70470, #70970, #1990, #32456, #24981, #56451, #31464, #23993, #86938, #39487, #32944, #85469, #69977, #2975, #93952, #46964, #84970, #9966, #55961, #18450, #48932, #79444, #62451, #63923, #9467, #71462, #86461, #62952, #61965, #47945, #78451, #10943, #63445, #17958, #93456, #1498, #41467, #92953, #39968, #92465, #55466, #1002, #54465, #31949, #94435, #16489, #54952, #40472, #16981, #47459, #25478, #48445, #78945, #77959, #85968, #17477, #40963, #35902, #28406, #73899, #34412, #42920, #5432, #73401, #12412, #72913, #96431, #4929, #35408, #50907, #72415, #20915, #51404, #43402, #94927, #11433, #81403, #80430, #89399, #96930, #49919, #42430, #12906, #27904, #34911, #57421, #50409, #20422, #64902, #41953, #58393, #66396, #95933, #64420, #65901, #19429, #58902, #81891, #80919, #3943, #88911, #4445, #95428, #13403, #71936, #65408, #27414, #3457, #33912, #26425, #26924, #56926, #87429, #18946, #57905, #49423, #79925, #87916, #11928, #88418, #19919, #9227, #74383, #21406, #16243, #54224, #62214, #82384, #6386, #36902, #771, #47213, #59882, #82888, #69737, #44390, #61720, #1750, #43888, #85233, #32205, #85722, #52385, #31223, #46725, #92235, #14404, #77224, #23762, #67391, #8729, #6893, #44875, #74888, #97416, #62706, #75378, #5909, #36404, #13907, #37406, #66897, #97919, #29380, #92720, #84739, #77714, #90370, #21910, #39247, #69251, #1263, #93206, #31718, #16736, #39736, #24245, #54711, #70231, #24729, #55207, #28882, #59385, #89889, #51902, #79688, #34662, #55718, #72176, #33192, #78710, #27163, #48690, #72657, #95169, #65159, #93702, #64170, #95677, #11186, #57663, #17235, #63197, #41706, #94188, #79193, #25237, #71215, #47713, #19181, #18211, #86213 ),
 ( #32701, #10705, #9720, #78208, #71697, #56210, #49186, #3211, #17724, #3705, #40219, #33673, #63685, #34166, #41220, #70728, #2243, #48197, #10221, #40710, #2736, #49662, #18702, #25718, #42193, #26676, #86705, #87181, #94691, #26196, #56688, #4192, #64656, #57171, #87668, #80172, #11683, #73645, #58146, #90129, #82137, #35153, #73150, #97179, #44131, #75134, #44640, #37157, #50667, #21659, #96677, #59638, #74642, #58652, #50163, #36151, #66655, #6640, #89645, #6152, #81642, #96175, #67653, #81155, #28156, #80672, #43649, #98163, #88160, #20163, #82639, #19674, #88655, #28647, #12167, #42672, #21157, #13646, #36657, #29619, #35659, #4691, #12660, #52143, #65652, #14156, #43159, #59137, #27658, #51658, #67144, #89152, #97668, #29134, #5174, #66144, #20662, #51158, #13150, #74134, #5669, #98670, #39127, #68633, #77592, #85107, #38147, #30612, #1136, #16618, #91627, #92601, #60623, #83134, #31598, #54105, #163, #659, #52631, #14659, #92114, #84618, #16122, #70110, #7654, #45125, #91124, #24125, #47094, #62092, #22647, #31107, #54594, #61600, #23645, #61118, #46606, #77105, #8618, #69614, #53127, #9107, #39621, #1635, #75631, #30117, #60125, #23143, #90623, #22147, #53616, #84134, #7143, #37647, #15646, #68144, #83635, #15150, #45629, #76128, #46128, #76616, #8133, #38626, #69127, #93585, #40601, #63575, #56096, #49075, #10587, #17609, #47603, #94084, #24620, #62584, #86589, #71098, #64057, #18098, #2130, #26088, #11564, #48575, #78592, #18582, #25604, #85606, #93089, #32590, #63085, #55604, #9600, #64546, #33561, #40103, #57059, #41598, #2624, #3106, #33079, #79074, #41099, #87560, #55086, #17121, #19069, #70604, #94569, #48079, #25122, #34050, #56583, #78097, #86098, #71595, #87073, #49548, #80060, #42082, #10104, #95053, #79577, #3591, #11077, #72066, #26562, #72545, #32086, #59527, #5559, #89537, #96564, #12055, #90020, #96061, #12551, #65036, #58534, #21542, #4078, #35035, #97556, #34541, #73040, #20553, #52033, #95562, #44022, #82526, #44523, #43053, #89042, #36035, #51038, #73532, #74028, #81531, #27544, #66538, #66035, #5059, #4575, #57549, #14042, #35544, #27051, #88048, #42556, #28039, #19561, #58038, #88546, #21047, #13037, #36545, #20047, #50549, #97066, #81044, #43534, #50057, #65538, #74525, #6046, #28538, #59031, #51537, #82028, #13538, #67034, #80561, #29017, #69014, #38516, #92482, #14541, #30992, #91003, #37537, #84991, #7538, #31479, #53999, #24008, #52518, #23029, #54480, #545, #16506, #75022, #22043, #61490, #53005, #38030, #83024, #30005, #6527, #76994, #76010, #91996, #68521, #60511, #53501, #23527 ) ),
 .UNSPECIFIED., .F., .F., .F. ) 
 B_SPLINE_SURFACE_WITH_KNOTS ( ( 2, 2 ),
 ( 3, 2, 2, 2, 2, 2, 2, 2, 2, 2, 2, 2, 2, 2, 2, 2, 2, 2, 2, 2, 2, 2, 2, 2, 2, 2, 2, 2, 2, 2, 2, 2, 2, 2, 2, 2, 2, 2, 2, 2, 2, 2, 2, 2, 2, 2, 2, 2, 2, 2, 2, 2, 2, 2, 2, 2, 2, 2, 2, 2, 2, 2, 2, 2, 2, 2, 2, 2, 2, 2, 2, 2, 2, 2, 2, 2, 2, 2, 2, 2, 2, 2, 2, 2, 2, 2, 2, 2, 2, 2, 2, 2, 2, 2, 2, 2, 2, 2, 2, 2, 2, 2, 2, 2, 2, 2, 2, 2, 2, 2, 2, 2, 2, 2, 2, 2, 2, 2, 2, 2, 2, 2, 2, 2, 2, 2, 2, 2, 2, 2, 2, 2, 2, 2, 2, 2, 2, 2, 2, 2, 2, 2, 2, 2, 2, 2, 2, 2, 2, 2, 2, 2, 2, 2, 2, 2, 2, 2, 2, 2, 2, 2, 3 ),
 ( 0.000000000000000000, 1.000000000000000000 ),
 ( 0.000000000000000000, 0.005952380952380952051, 0.01190476190476190410, 0.01785714285714285615, 0.02380952380952380820, 0.02976190476190476025, 0.03571428571428571230, 0.04166666666666666435, 0.04761904761904761640, 0.05357142857142856845, 0.05952380952380952051, 0.06547619047619047949, 0.07142857142857142461, 0.07738095238095238360, 0.08333333333333332871, 0.08928571428571428770, 0.09523809523809523281, 0.1011904761904761918, 0.1071428571428571369, 0.1130952380952380959, 0.1190476190476190410, 0.1250000000000000000, 0.1309523809523809590, 0.1369047619047619180, 0.1428571428571428492, 0.1488095238095238082, 0.1547619047619047672, 0.1607142857142857262, 0.1666666666666666574, 0.1726190476190476164, 0.1785714285714285754, 0.1845238095238095344, 0.1904761904761904656, 0.1964285714285714246, 0.2023809523809523836, 0.2083333333333333426, 0.2142857142857142738, 0.2202380952380952328, 0.2261904761904761918, 0.2321428571428571508, 0.2380952380952380820, 0.2440476190476190410, 0.2500000000000000000, 0.2559523809523809312, 0.2619047619047619180, 0.2678571428571428492, 0.2738095238095238360, 0.2797619047619047672, 0.2857142857142856984, 0.2916666666666666852, 0.2976190476190476164, 0.3035714285714285476, 0.3095238095238095344, 0.3154761904761904656, 0.3214285714285714524, 0.3273809523809523836, 0.3333333333333333148, 0.3392857142857143016, 0.3452380952380952328, 0.3511904761904761640, 0.3571428571428571508, 0.3630952380952380820, 0.3690476190476190688, 0.3750000000000000000, 0.3809523809523809312, 0.3869047619047619180, 0.3928571428571428492, 0.3988095238095238360, 0.4047619047619047672, 0.4107142857142856984, 0.4166666666666666852, 0.4226190476190476164, 0.4285714285714285476, 0.4345238095238095344, 0.4404761904761904656, 0.4464285714285714524, 0.4523809523809523836, 0.4583333333333333148, 0.4642857142857143016, 0.4702380952380952328, 0.4761904761904761640, 0.4821428571428571508, 0.4880952380952380820, 0.4940476190476190688, 0.5000000000000000000, 0.5059523809523809312, 0.5119047619047618625, 0.5178571428571429047, 0.5238095238095238360, 0.5297619047619047672, 0.5357142857142856984, 0.5416666666666666297, 0.5476190476190476719, 0.5535714285714286031, 0.5595238095238095344, 0.5654761904761904656, 0.5714285714285713969, 0.5773809523809523281, 0.5833333333333333703, 0.5892857142857143016, 0.5952380952380952328, 0.6011904761904761640, 0.6071428571428570953, 0.6130952380952381375, 0.6190476190476190688, 0.6250000000000000000, 0.6309523809523809312, 0.6369047619047618625, 0.6428571428571429047, 0.6488095238095238360, 0.6547619047619047672, 0.6607142857142856984, 0.6666666666666666297, 0.6726190476190476719, 0.6785714285714286031, 0.6845238095238095344, 0.6904761904761904656, 0.6964285714285713969, 0.7023809523809523281, 0.7083333333333333703, 0.7142857142857143016, 0.7202380952380952328, 0.7261904761904761640, 0.7321428571428570953, 0.7380952380952381375, 0.7440476190476190688, 0.7500000000000000000, 0.7559523809523809312, 0.7619047619047618625, 0.7678571428571429047, 0.7738095238095238360, 0.7797619047619047672, 0.7857142857142856984, 0.7916666666666666297, 0.7976190476190476719, 0.8035714285714286031, 0.8095238095238095344, 0.8154761904761904656, 0.8214285714285713969, 0.8273809523809523281, 0.8333333333333333703, 0.8392857142857143016, 0.8452380952380952328, 0.8511904761904761640, 0.8571428571428570953, 0.8630952380952381375, 0.8690476190476190688, 0.8750000000000000000, 0.8809523809523809312, 0.8869047619047618625, 0.8928571428571429047, 0.8988095238095238360, 0.9047619047619047672, 0.9107142857142856984, 0.9166666666666666297, 0.9226190476190476719, 0.9285714285714286031, 0.9345238095238095344, 0.9404761904761904656, 0.9464285714285713969, 0.9523809523809523281, 0.9583333333333333703, 0.9642857142857143016 ),
 .UNSPECIFIED. ) 
 GEOMETRIC_REPRESENTATION_ITEM ( )  RATIONAL_B_SPLINE_SURFACE ( (
 ( 1.000000000000000000, 0.9659258262890683122, 1.000000000000000000, 0.9659258262890683122, 1.000000000000000000, 0.9659258262890683122, 1.000000000000000000, 0.9659258262890683122, 1.000000000000000000, 0.9659258262890683122, 1.000000000000000000, 0.9659258262890683122, 1.000000000000000000, 0.9659258262890683122, 1.000000000000000000, 0.9659258262890683122, 1.000000000000000000, 0.9659258262890683122, 1.000000000000000000, 0.9659258262890683122, 1.000000000000000000, 0.9659258262890683122, 1.000000000000000000, 0.9659258262890683122, 1.000000000000000000, 0.9659258262890683122, 1.000000000000000000, 0.9659258262890683122, 1.000000000000000000, 0.9659258262890683122, 1.000000000000000000, 0.9659258262890683122, 1.000000000000000000, 0.9659258262890683122, 1.000000000000000000, 0.9659258262890683122, 1.000000000000000000, 0.9659258262890683122, 1.000000000000000000, 0.9659258262890683122, 1.000000000000000000, 0.9659258262890683122, 1.000000000000000000, 0.9659258262890683122, 1.000000000000000000, 0.9659258262890683122, 1.000000000000000000, 0.9659258262890683122, 1.000000000000000000, 0.9659258262890683122, 1.000000000000000000, 0.9659258262890683122, 1.000000000000000000, 0.9659258262890683122, 1.000000000000000000, 0.9659258262890683122, 1.000000000000000000, 0.9659258262890683122, 1.000000000000000000, 0.9659258262890683122, 1.000000000000000000, 0.9659258262890683122, 1.000000000000000000, 0.9659258262890683122, 1.000000000000000000, 0.9659258262890683122, 1.000000000000000000, 0.9659258262890683122, 1.000000000000000000, 0.9659258262890683122, 1.000000000000000000, 0.9659258262890683122, 1.000000000000000000, 0.9659258262890683122, 1.000000000000000000, 0.9659258262890683122, 1.000000000000000000, 0.9659258262890683122, 1.000000000000000000, 0.9659258262890683122, 1.000000000000000000, 0.9659258262890683122, 1.000000000000000000, 0.9659258262890683122, 1.000000000000000000, 0.9659258262890683122, 1.000000000000000000, 0.9659258262890683122, 1.000000000000000000, 0.9659258262890683122, 1.000000000000000000, 0.9659258262890683122, 1.000000000000000000, 0.9659258262890683122, 1.000000000000000000, 0.9659258262890683122, 1.000000000000000000, 0.9659258262890683122, 1.000000000000000000, 0.9659258262890683122, 1.000000000000000000, 0.9659258262890683122, 1.000000000000000000, 0.9659258262890683122, 1.000000000000000000, 0.9659258262890683122, 1.000000000000000000, 0.9659258262890683122, 1.000000000000000000, 0.9659258262890683122, 1.000000000000000000, 0.9659258262890683122, 1.000000000000000000, 0.9659258262890683122, 1.000000000000000000, 0.9659258262890683122, 1.000000000000000000, 0.9659258262890683122, 1.000000000000000000, 0.9659258262890683122, 1.000000000000000000, 0.9659258262890683122, 1.000000000000000000, 0.9659258262890683122, 1.000000000000000000, 0.9659258262890683122, 1.000000000000000000, 0.9659258262890683122, 1.000000000000000000, 0.9659258262890683122, 1.000000000000000000, 0.9659258262890683122, 1.000000000000000000, 0.9659258262890683122, 1.000000000000000000, 0.9659258262890683122, 1.000000000000000000, 0.9659258262890683122, 1.000000000000000000, 0.9659258262890683122, 1.000000000000000000, 0.9659258262890683122, 1.000000000000000000, 0.9659258262890683122, 1.000000000000000000, 0.9659258262890683122, 1.000000000000000000, 0.9659258262890683122, 1.000000000000000000, 0.9659258262890683122, 1.000000000000000000, 0.9659258262890683122, 1.000000000000000000, 0.9659258262890683122, 1.000000000000000000, 0.9659258262890683122, 1.000000000000000000, 0.9659258262890683122, 1.000000000000000000, 0.9659258262890683122, 1.000000000000000000, 0.9659258262890683122, 1.000000000000000000, 0.9659258262890683122, 1.000000000000000000, 0.9659258262890683122, 1.000000000000000000, 0.9659258262890683122, 1.000000000000000000, 0.9659258262890683122, 1.000000000000000000, 0.9659258262890683122, 1.000000000000000000, 0.9659258262890683122, 1.000000000000000000, 0.9659258262890683122, 1.000000000000000000, 0.9659258262890683122, 1.000000000000000000, 0.9659258262890683122, 1.000000000000000000, 0.9659258262890683122, 1.000000000000000000, 0.9659258262890683122, 1.000000000000000000, 0.9659258262890683122, 1.000000000000000000, 0.9659258262890683122, 1.000000000000000000, 0.9659258262890683122, 1.000000000000000000, 0.9659258262890683122, 1.000000000000000000, 0.9659258262890683122, 1.000000000000000000, 0.9659258262890683122, 1.000000000000000000, 0.9659258262890683122, 1.000000000000000000, 0.9659258262890683122, 1.000000000000000000, 0.9659258262890683122, 1.000000000000000000, 0.9659258262890683122, 1.000000000000000000, 0.9659258262890683122, 1.000000000000000000, 0.9659258262890683122, 1.000000000000000000, 0.9659258262890683122, 1.000000000000000000, 0.9659258262890683122, 1.000000000000000000, 0.9659258262890683122, 1.000000000000000000, 0.9659258262890683122, 1.000000000000000000, 0.9659258262890683122, 1.000000000000000000, 0.9659258262890683122, 1.000000000000000000, 0.9659258262890683122, 1.000000000000000000, 0.9659258262890683122, 1.000000000000000000, 0.9659258262890683122, 1.000000000000000000, 0.9659258262890683122, 1.000000000000000000, 0.9659258262890683122, 1.000000000000000000, 0.9659258262890683122, 1.000000000000000000, 0.9659258262890683122, 1.000000000000000000, 0.9659258262890683122, 1.000000000000000000, 0.9659258262890683122, 1.000000000000000000, 0.9659258262890683122, 1.000000000000000000, 0.9659258262890683122, 1.000000000000000000, 0.9659258262890683122, 1.000000000000000000, 0.9659258262890683122, 1.000000000000000000, 0.9659258262890683122, 1.000000000000000000, 0.9659258262890683122, 1.000000000000000000, 0.9659258262890683122, 1.000000000000000000, 0.9659258262890683122, 1.000000000000000000, 0.9659258262890683122, 1.000000000000000000, 0.9659258262890683122, 1.000000000000000000, 0.9659258262890683122, 1.000000000000000000, 0.9659258262890683122, 1.000000000000000000, 0.9659258262890683122, 1.000000000000000000, 0.9659258262890683122, 1.000000000000000000, 0.9659258262890683122, 1.000000000000000000, 0.9659258262890683122, 1.000000000000000000, 0.9659258262890683122, 1.000000000000000000, 0.9659258262890683122, 1.000000000000000000, 0.9659258262890683122, 1.000000000000000000, 0.9659258262890683122, 1.000000000000000000, 0.9659258262890683122, 1.000000000000000000, 0.9659258262890683122, 1.000000000000000000, 0.9659258262890683122, 1.000000000000000000, 0.9659258262890683122, 1.000000000000000000, 0.9659258262890683122, 1.000000000000000000, 0.9659258262890683122, 1.000000000000000000, 0.9659258262890683122, 1.000000000000000000, 0.9659258262890683122, 1.000000000000000000, 0.9659258262890683122, 1.000000000000000000, 0.9659258262890683122, 1.000000000000000000, 0.9659258262890683122, 1.000000000000000000, 0.9659258262890683122, 1.000000000000000000, 0.9659258262890683122, 1.000000000000000000, 0.9659258262890683122, 1.000000000000000000, 0.9659258262890683122, 1.000000000000000000, 0.9659258262890683122, 1.000000000000000000, 0.9659258262890683122, 1.000000000000000000, 0.9659258262890683122, 1.000000000000000000, 0.9659258262890683122, 1.000000000000000000, 0.9659258262890683122, 1.000000000000000000, 0.9659258262890683122, 1.000000000000000000, 0.9659258262890683122, 1.000000000000000000, 0.9659258262890683122, 1.000000000000000000),
 ( 1.000000000000000000, 0.9659258262890683122, 1.000000000000000000, 0.9659258262890683122, 1.000000000000000000, 0.9659258262890683122, 1.000000000000000000, 0.9659258262890683122, 1.000000000000000000, 0.9659258262890683122, 1.000000000000000000, 0.9659258262890683122, 1.000000000000000000, 0.9659258262890683122, 1.000000000000000000, 0.9659258262890683122, 1.000000000000000000, 0.9659258262890683122, 1.000000000000000000, 0.9659258262890683122, 1.000000000000000000, 0.9659258262890683122, 1.000000000000000000, 0.9659258262890683122, 1.000000000000000000, 0.9659258262890683122, 1.000000000000000000, 0.9659258262890683122, 1.000000000000000000, 0.9659258262890683122, 1.000000000000000000, 0.9659258262890683122, 1.000000000000000000, 0.9659258262890683122, 1.000000000000000000, 0.9659258262890683122, 1.000000000000000000, 0.9659258262890683122, 1.000000000000000000, 0.9659258262890683122, 1.000000000000000000, 0.9659258262890683122, 1.000000000000000000, 0.9659258262890683122, 1.000000000000000000, 0.9659258262890683122, 1.000000000000000000, 0.9659258262890683122, 1.000000000000000000, 0.9659258262890683122, 1.000000000000000000, 0.9659258262890683122, 1.000000000000000000, 0.9659258262890683122, 1.000000000000000000, 0.9659258262890683122, 1.000000000000000000, 0.9659258262890683122, 1.000000000000000000, 0.9659258262890683122, 1.000000000000000000, 0.9659258262890683122, 1.000000000000000000, 0.9659258262890683122, 1.000000000000000000, 0.9659258262890683122, 1.000000000000000000, 0.9659258262890683122, 1.000000000000000000, 0.9659258262890683122, 1.000000000000000000, 0.9659258262890683122, 1.000000000000000000, 0.9659258262890683122, 1.000000000000000000, 0.9659258262890683122, 1.000000000000000000, 0.9659258262890683122, 1.000000000000000000, 0.9659258262890683122, 1.000000000000000000, 0.9659258262890683122, 1.000000000000000000, 0.9659258262890683122, 1.000000000000000000, 0.9659258262890683122, 1.000000000000000000, 0.9659258262890683122, 1.000000000000000000, 0.9659258262890683122, 1.000000000000000000, 0.9659258262890683122, 1.000000000000000000, 0.9659258262890683122, 1.000000000000000000, 0.9659258262890683122, 1.000000000000000000, 0.9659258262890683122, 1.000000000000000000, 0.9659258262890683122, 1.000000000000000000, 0.9659258262890683122, 1.000000000000000000, 0.9659258262890683122, 1.000000000000000000, 0.9659258262890683122, 1.000000000000000000, 0.9659258262890683122, 1.000000000000000000, 0.9659258262890683122, 1.000000000000000000, 0.9659258262890683122, 1.000000000000000000, 0.9659258262890683122, 1.000000000000000000, 0.9659258262890683122, 1.000000000000000000, 0.9659258262890683122, 1.000000000000000000, 0.9659258262890683122, 1.000000000000000000, 0.9659258262890683122, 1.000000000000000000, 0.9659258262890683122, 1.000000000000000000, 0.9659258262890683122, 1.000000000000000000, 0.9659258262890683122, 1.000000000000000000, 0.9659258262890683122, 1.000000000000000000, 0.9659258262890683122, 1.000000000000000000, 0.9659258262890683122, 1.000000000000000000, 0.9659258262890683122, 1.000000000000000000, 0.9659258262890683122, 1.000000000000000000, 0.9659258262890683122, 1.000000000000000000, 0.9659258262890683122, 1.000000000000000000, 0.9659258262890683122, 1.000000000000000000, 0.9659258262890683122, 1.000000000000000000, 0.9659258262890683122, 1.000000000000000000, 0.9659258262890683122, 1.000000000000000000, 0.9659258262890683122, 1.000000000000000000, 0.9659258262890683122, 1.000000000000000000, 0.9659258262890683122, 1.000000000000000000, 0.9659258262890683122, 1.000000000000000000, 0.9659258262890683122, 1.000000000000000000, 0.9659258262890683122, 1.000000000000000000, 0.9659258262890683122, 1.000000000000000000, 0.9659258262890683122, 1.000000000000000000, 0.9659258262890683122, 1.000000000000000000, 0.9659258262890683122, 1.000000000000000000, 0.9659258262890683122, 1.000000000000000000, 0.9659258262890683122, 1.000000000000000000, 0.9659258262890683122, 1.000000000000000000, 0.9659258262890683122, 1.000000000000000000, 0.9659258262890683122, 1.000000000000000000, 0.9659258262890683122, 1.000000000000000000, 0.9659258262890683122, 1.000000000000000000, 0.9659258262890683122, 1.000000000000000000, 0.9659258262890683122, 1.000000000000000000, 0.9659258262890683122, 1.000000000000000000, 0.9659258262890683122, 1.000000000000000000, 0.9659258262890683122, 1.000000000000000000, 0.9659258262890683122, 1.000000000000000000, 0.9659258262890683122, 1.000000000000000000, 0.9659258262890683122, 1.000000000000000000, 0.9659258262890683122, 1.000000000000000000, 0.9659258262890683122, 1.000000000000000000, 0.9659258262890683122, 1.000000000000000000, 0.9659258262890683122, 1.000000000000000000, 0.9659258262890683122, 1.000000000000000000, 0.9659258262890683122, 1.000000000000000000, 0.9659258262890683122, 1.000000000000000000, 0.9659258262890683122, 1.000000000000000000, 0.9659258262890683122, 1.000000000000000000, 0.9659258262890683122, 1.000000000000000000, 0.9659258262890683122, 1.000000000000000000, 0.9659258262890683122, 1.000000000000000000, 0.9659258262890683122, 1.000000000000000000, 0.9659258262890683122, 1.000000000000000000, 0.9659258262890683122, 1.000000000000000000, 0.9659258262890683122, 1.000000000000000000, 0.9659258262890683122, 1.000000000000000000, 0.9659258262890683122, 1.000000000000000000, 0.9659258262890683122, 1.000000000000000000, 0.9659258262890683122, 1.000000000000000000, 0.9659258262890683122, 1.000000000000000000, 0.9659258262890683122, 1.000000000000000000, 0.9659258262890683122, 1.000000000000000000, 0.9659258262890683122, 1.000000000000000000, 0.9659258262890683122, 1.000000000000000000, 0.9659258262890683122, 1.000000000000000000, 0.9659258262890683122, 1.000000000000000000, 0.9659258262890683122, 1.000000000000000000, 0.9659258262890683122, 1.000000000000000000, 0.9659258262890683122, 1.000000000000000000, 0.9659258262890683122, 1.000000000000000000, 0.9659258262890683122, 1.000000000000000000, 0.9659258262890683122, 1.000000000000000000, 0.9659258262890683122, 1.000000000000000000, 0.9659258262890683122, 1.000000000000000000, 0.9659258262890683122, 1.000000000000000000, 0.9659258262890683122, 1.000000000000000000, 0.9659258262890683122, 1.000000000000000000, 0.9659258262890683122, 1.000000000000000000, 0.9659258262890683122, 1.000000000000000000, 0.9659258262890683122, 1.000000000000000000, 0.9659258262890683122, 1.000000000000000000, 0.9659258262890683122, 1.000000000000000000, 0.9659258262890683122, 1.000000000000000000, 0.9659258262890683122, 1.000000000000000000, 0.9659258262890683122, 1.000000000000000000, 0.9659258262890683122, 1.000000000000000000, 0.9659258262890683122, 1.000000000000000000, 0.9659258262890683122, 1.000000000000000000, 0.9659258262890683122, 1.000000000000000000, 0.9659258262890683122, 1.000000000000000000, 0.9659258262890683122, 1.000000000000000000, 0.9659258262890683122, 1.000000000000000000, 0.9659258262890683122, 1.000000000000000000, 0.9659258262890683122, 1.000000000000000000, 0.9659258262890683122, 1.000000000000000000, 0.9659258262890683122, 1.000000000000000000, 0.9659258262890683122, 1.000000000000000000, 0.9659258262890683122, 1.000000000000000000, 0.9659258262890683122, 1.000000000000000000, 0.9659258262890683122, 1.000000000000000000, 0.9659258262890683122, 1.000000000000000000) ) ) 
 REPRESENTATION_ITEM ( '' )  SURFACE ( )  );
#29497 = PRESENTATION_STYLE_ASSIGNMENT (( #61483 ) ) ;
#29498 = CARTESIAN_POINT ( 'NONE',  ( 13.43411237798105340, 45.58196800326374643, 12.81628187352647963 ) ) ;
#29499 = ORIENTED_EDGE ( 'NONE', *, *, #8806, .F. ) ;
#29500 = CARTESIAN_POINT ( 'NONE',  ( 4.559911319644449179, 62.23035201082150536, -9.422509992056141925 ) ) ;
#29501 = CARTESIAN_POINT ( 'NONE',  ( 10.00000000000000000, 37.87363466993041783, -12.81628187352647608 ) ) ;
#29502 = CARTESIAN_POINT ( 'NONE',  ( 7.361572987183169658, 4.967264484334119601, -9.846743663894592657 ) ) ;
#29503 = CARTESIAN_POINT ( 'NONE',  ( 15.44008868035555793, 41.39701867748817676, -9.422509992056140149 ) ) ;
#29504 = DIRECTION ( 'NONE',  ( 0.1478094111296180124, 0.000000000000000000, -0.9890158633619157147 ) ) ;
#29505 = CARTESIAN_POINT ( 'NONE',  ( 0.000000000000000000, 0.000000000000000000, 0.000000000000000000 ) ) ;
#29506 = CARTESIAN_POINT ( 'NONE',  ( 10.00000000000000178, 22.25893115100078745, 9.846743663894594434 ) ) ;
#29507 = EDGE_CURVE ( 'NONE', #58863, #27610, #48441, .T. ) ;
#29508 = CARTESIAN_POINT ( 'NONE',  ( 10.00000000000000178, 12.25893115100078568, 9.846743663894594434 ) ) ;
#29509 = CARTESIAN_POINT ( 'NONE',  ( 2.917880565312948704, 37.63708216824731068, 12.26659068614894643 ) ) ;
#29510 = CARTESIAN_POINT ( 'NONE',  ( 2.603489959281614308, 56.58210964143329846, 6.500000000000031086 ) ) ;
#29511 = EDGE_CURVE ( 'NONE', #17634, #54629, #21864, .T. ) ;
#29512 = FILL_AREA_STYLE_COLOUR ( '', #1930 ) ;
#29513 = CARTESIAN_POINT ( 'NONE',  ( -5.811454672277545974, -36.11427488547636955, -3.999999999998387956 ) ) ;
#29514 = ORIENTED_EDGE ( 'NONE', *, *, #73348, .F. ) ;
#29515 = CARTESIAN_POINT ( 'NONE',  ( -0.3689425029237898834, 66.17874883491396076, -10.36894250292378850 ) ) ;
#29516 = CARTESIAN_POINT ( 'NONE',  ( -4.164238869374099039, 66.80374883491396076, 8.674139862899312516E-16 ) ) ;
#29517 = CARTESIAN_POINT ( 'NONE',  ( 2.791683348922237240, 35.38393115100079456, -7.208316651077763204 ) ) ;
#29518 = VECTOR ( 'NONE', #72762, 1000.000000000000000 ) ;
#29519 = CARTESIAN_POINT ( 'NONE',  ( -1.099225684535947600, 44.54030133659708923, 6.408140936763237150 ) ) ;
#29520 = CARTESIAN_POINT ( 'NONE',  ( -4.431036607602414357, 14.49999999999999112, -14.33059365769922167 ) ) ;
#29522 = CARTESIAN_POINT ( 'NONE',  ( 17.08211943468705840, 5.137082168247300906, -12.26659068614894466 ) ) ;
#29521 = CARTESIAN_POINT ( 'NONE',  ( 2.120353041430647512, 4.078855811979330250E-16, -14.34413130794945523 ) ) ;
#29523 = CARTESIAN_POINT ( 'NONE',  ( 7.084665262690076126, 12.02201867748817143, -10.88017736071110164 ) ) ;
#29524 = CARTESIAN_POINT ( 'NONE',  ( -2.266590686148945544, 51.38708216824730357, -7.082119434687050408 ) ) ;
#29525 = CARTESIAN_POINT ( 'NONE',  ( 19.84674366389459621, 23.50893115100078390, 7.409399052514197653E-17 ) ) ;
#29526 = CARTESIAN_POINT ( 'NONE',  ( 0.000000000000000000, 0.000000000000000000, 0.000000000000000000 ) ) ;
#29527 = CARTESIAN_POINT ( 'NONE',  ( 14.92337183194729988, 29.34226448433411960, -8.527530157486177487 ) ) ;
#29529 = EDGE_CURVE ( 'NONE', #38580, #58843, #94922, .T. ) ;
#29528 = B_SPLINE_CURVE_WITH_KNOTS ( 'NONE', 3,
 ( #94619, #58082, #12103, #65083, #88586, #26132 ),
 .UNSPECIFIED., .F., .F.,
 ( 4, 2, 4 ),
 ( 0.000000000000000000, 0.0002605067024380892785, 0.0005210134048761785571 ),
 .UNSPECIFIED. ) ;
#29530 = CARTESIAN_POINT ( 'NONE',  ( -1.180296924652843193, 0.000000000000000000, -5.323975374878068934 ) ) ;
#29531 = CARTESIAN_POINT ( 'NONE',  ( -7.208316651077764980, 20.38393115100079100, -7.208316651077759651 ) ) ;
#29532 = VERTEX_POINT ( 'NONE', #71930 ) ;
#29533 = ORIENTED_EDGE ( 'NONE', *, *, #31434, .T. ) ;
#29534 = DIRECTION ( 'NONE',  ( -0.000000000000000000, 0.000000000000000000, 1.000000000000000000 ) ) ;
#29535 = ORIENTED_EDGE ( 'NONE', *, *, #87540, .T. ) ;
#29536 = CARTESIAN_POINT ( 'NONE',  ( 5.076628168052704559, 45.17559781766745175, -8.527530157486179263 ) ) ;
#29537 = CARTESIAN_POINT ( 'NONE',  ( -0.3689425029237881626, 17.42874883491397142, 10.36894250292379027 ) ) ;
#29539 = CARTESIAN_POINT ( 'NONE',  ( 17.96484262340118221, 39.93868534415484106, 7.964842623401181321 ) ) ;
#29538 = CARTESIAN_POINT ( 'NONE',  ( 17.96484262340118221, 29.93868534415484106, 7.964842623401181321 ) ) ;
#29541 = CARTESIAN_POINT ( 'NONE',  ( 10.00000000000000178, 20.37363466993042138, 12.81628187352647608 ) ) ;
#29540 = CARTESIAN_POINT ( 'NONE',  ( 7.361572987183169658, 64.96726448433412315, -9.846743663894592657 ) ) ;
#29542 = CARTESIAN_POINT ( 'NONE',  ( -0.8801773607111008646, 68.27201867748817676, 2.915334737309923430 ) ) ;
#29543 = CARTESIAN_POINT ( 'NONE',  ( -1.099225684535947600, 33.70696800326375353, -6.408140936763238038 ) ) ;
#29544 = VERTEX_POINT ( 'NONE', #80427 ) ;
#29545 = CARTESIAN_POINT ( 'NONE',  ( 10.00000000000000000, 49.75893115100078745, -9.846743663894594434 ) ) ;
#29546 = CARTESIAN_POINT ( 'NONE',  ( 7.084665262690076126, 9.105352010821503583, 10.88017736071109987 ) ) ;
#29547 = VERTEX_POINT ( 'NONE', #32939 ) ;
#29548 = CARTESIAN_POINT ( 'NONE',  ( 12.91533473730993009, 11.60535201082150714, -10.88017736071109987 ) ) ;
#29549 = B_SPLINE_CURVE_WITH_KNOTS ( 'NONE', 3,
 ( #62046, #85058, #39572, #15593 ),
 .UNSPECIFIED., .F., .F.,
 ( 4, 4 ),
 ( 4.336808689942017736E-18, 0.001060528352561992006 ),
 .UNSPECIFIED. ) ;
#29550 = ORIENTED_EDGE ( 'NONE', *, *, #8025, .F. ) ;
#29551 = CARTESIAN_POINT ( 'NONE',  ( 17.96484262340118221, 51.18868534415483396, -7.964842623401177768 ) ) ;
#29552 = CARTESIAN_POINT ( 'NONE',  ( 0.5774900079438590739, 52.64701867748817676, -5.440088680355550821 ) ) ;
#29553 = B_SPLINE_CURVE_WITH_KNOTS ( 'NONE', 3,
 ( #45981, #85449, #61947, #9447 ),
 .UNSPECIFIED., .F., .F.,
 ( 4, 4 ),
 ( 0.000000000000000000, 0.001036303429213364206 ),
 .UNSPECIFIED. ) ;
#29554 = CARTESIAN_POINT ( 'NONE',  ( 4.559911319644449179, 62.23035201082150536, -9.422509992056141925 ) ) ;
#29555 = PRESENTATION_STYLE_ASSIGNMENT (( #52565 ) ) ;
#29556 = CARTESIAN_POINT ( 'NONE',  ( 19.42250999205614548, 50.98035201082151247, -5.440088680355545492 ) ) ;
#29557 = CARTESIAN_POINT ( 'NONE',  ( -46.94000000000001194, 102.4632489371144146, 6.394394627235429951 ) ) ;
#29558 = ADVANCED_FACE ( 'NONE', ( #65403 ), #63440, .F. ) ;
#29559 = FILL_AREA_STYLE ('',( #37090 ) ) ;
#29560 = CARTESIAN_POINT ( 'NONE',  ( 7.361572987183169658, 24.96726448433412315, -9.846743663894592657 ) ) ;
#29561 = ORIENTED_EDGE ( 'NONE', *, *, #37719, .F. ) ;
#29562 = CARTESIAN_POINT ( 'NONE',  ( 0.000000000000000000, 70.00000000000000000, -5.000000000000000000 ) ) ;
#29563 = EDGE_CURVE ( 'NONE', #90631, #79877, #90367, .T. ) ;
#29564 =( NAMED_UNIT ( * ) PLANE_ANGLE_UNIT ( ) SI_UNIT ( $, .RADIAN. ) );
#29565 = CARTESIAN_POINT ( 'NONE',  ( 6.204703633549690345, 2.845415501580634388, 14.16423886937410082 ) ) ;
#29566 = CARTESIAN_POINT ( 'NONE',  ( 20.10493008474206178, 29.71697413083880335, 6.336235997365763595 ) ) ;
#29568 = CARTESIAN_POINT ( 'NONE',  ( 14.92337183194729633, 37.67559781766745175, 8.527530157486181039 ) ) ;
#29567 = DIRECTION ( 'NONE',  ( 0.000000000000000000, 1.000000000000000000, 0.000000000000000000 ) ) ;
#29569 = CARTESIAN_POINT ( 'NONE',  ( -0.8801773607111008646, 8.272018677488171434, 2.915334737309923430 ) ) ;
#29570 = LINE ( 'NONE', #35610, #67429 ) ;
#29571 = ORIENTED_EDGE ( 'NONE', *, *, #29507, .F. ) ;
#29572 = FACE_OUTER_BOUND ( 'NONE', #47853, .T. ) ;
#29573 = CARTESIAN_POINT ( 'NONE',  ( 14.92337183194729633, 42.67559781766745886, 8.527530157486181039 ) ) ;
#29574 = CYLINDRICAL_SURFACE ( 'NONE', #96257, 11.92686044187656513 ) ;
#29575 = CARTESIAN_POINT ( 'NONE',  ( 22.81628187352648496, 21.83196800326374643, -3.434112377981050290 ) ) ;
#29576 = CARTESIAN_POINT ( 'NONE',  ( 19.84674366389459621, 13.50893115100078568, 7.409399052514197653E-17 ) ) ;
#29577 = CARTESIAN_POINT ( 'NONE',  ( 0.2751277870542911397, 35.30223176428830811, 6.499999999999992006 ) ) ;
#29578 = CARTESIAN_POINT ( 'NONE',  ( 16.40814093676323893, 5.790301336597087456, 11.09922568453595026 ) ) ;
#29579 = DIRECTION ( 'NONE',  ( 0.000000000000000000, -0.000000000000000000, -1.000000000000000000 ) ) ;
#29580 = AXIS2_PLACEMENT_3D ( 'NONE', #69724, #61708, #1250 ) ;
#29581 = EDGE_CURVE ( 'NONE', #21351, #46284, #9907, .T. ) ;
#29582 = VERTEX_POINT ( 'NONE', #59382 ) ;
#29583 = ORIENTED_EDGE ( 'NONE', *, *, #84676, .T. ) ;
#29584 = CARTESIAN_POINT ( 'NONE',  ( 12.91533473730992121, 29.52201867748817321, 10.88017736071110164 ) ) ;
#29585 = CARTESIAN_POINT ( 'NONE',  ( 17.08211943468705840, 20.13708216824730357, -12.26659068614894466 ) ) ;
#29586 = CARTESIAN_POINT ( 'NONE',  ( 2.791683348922240793, 26.63393115100078745, 7.208316651077764092 ) ) ;
#29587 = CARTESIAN_POINT ( 'NONE',  ( 12.91533473730993009, 56.60535201082151247, -10.88017736071109987 ) ) ;
#29589 = DIRECTION ( 'NONE',  ( 0.6626200482157461602, 0.000000000000000000, -0.7489557207889945278 ) ) ;
#29588 = CARTESIAN_POINT ( 'NONE',  ( 21.09922568453595559, 42.04030133659708213, -6.408140936763230044 ) ) ;
#29590 = CARTESIAN_POINT ( 'NONE',  ( 19.42250999205614548, 10.98035201082150358, -5.440088680355545492 ) ) ;
#29591 = EDGE_CURVE ( 'NONE', #78512, #59678, #10784, .T. ) ;
#29592 = DIRECTION ( 'NONE',  ( -0.000000000000000000, -1.000000000000000000, -0.000000000000000000 ) ) ;
#29593 = CARTESIAN_POINT ( 'NONE',  ( 13.07661834287964986, 14.99999999999796252, 6.550615570657222442 ) ) ;
#29594 = CARTESIAN_POINT ( 'NONE',  ( 0.6178305044545838731, 14.74863466993041783, 9.382169495545420901 ) ) ;
#29595 = CARTESIAN_POINT ( 'NONE',  ( 6.565887622018943937, 5.165301336597086568, 12.81628187352647430 ) ) ;
#29596 = CARTESIAN_POINT ( 'NONE',  ( 17.20831665107776587, 22.88393115100078745, 7.208316651077764980 ) ) ;
#29597 = CARTESIAN_POINT ( 'NONE',  ( 10.88017736071110519, -14.43631465584515539, -2.602085213965210642E-15 ) ) ;
#29598 = CARTESIAN_POINT ( 'NONE',  ( 21.09922568453594849, 31.20696800326375353, 6.408140936763242479 ) ) ;
#29599 = CARTESIAN_POINT ( 'NONE',  ( 3.969999999999999751, 10.25000000000000000, -2.500000000000000000 ) ) ;
#29600 =( REPRESENTATION_RELATIONSHIP ('NONE','NONE', #61309, #53719 ) REPRESENTATION_RELATIONSHIP_WITH_TRANSFORMATION ( #15229 )SHAPE_REPRESENTATION_RELATIONSHIP( ) );
#29602 = CARTESIAN_POINT ( 'NONE',  ( 0.000000000000000000, 0.000000000000000000, 0.000000000000000000 ) ) ;
#29601 = CARTESIAN_POINT ( 'NONE',  ( 15.44008868035555793, 41.39701867748817676, -9.422509992056140149 ) ) ;
#29603 = CARTESIAN_POINT ( 'NONE',  ( 4.629999999999999893, 4.857171655774867594E-16, 4.000000000000000000 ) ) ;
#29604 = CARTESIAN_POINT ( 'NONE',  ( 4.559911319644449179, 67.23035201082150536, -9.422509992056141925 ) ) ;
#29605 = CARTESIAN_POINT ( 'NONE',  ( 0.5774900079438607392, 38.48035201082150536, 5.440088680355550821 ) ) ;
#29606 = CARTESIAN_POINT ( 'NONE',  ( 20.88017736071110875, 45.77201867748816966, -2.915334737309920765 ) ) ;
#29607 = CARTESIAN_POINT ( 'NONE',  ( 5.076628168052703671, 66.84226448433412315, 8.527530157486179263 ) ) ;
#29608 = CARTESIAN_POINT ( 'NONE',  ( -6.898461952320262824, 4.061641280801676772E-16, -12.75387089053318590 ) ) ;
#29609 = MECHANICAL_DESIGN_GEOMETRIC_PRESENTATION_REPRESENTATION (  '', ( #64713 ), #47166 ) ;
#29610 = CARTESIAN_POINT ( 'NONE',  ( 2.791683348922237240, 35.38393115100079456, -7.208316651077763204 ) ) ;
#29611 = CARTESIAN_POINT ( 'NONE',  ( 20.88017736071110875, 10.77201867748817143, -2.915334737309920765 ) ) ;
#29612 = CARTESIAN_POINT ( 'NONE',  ( 3.591859063236763294, 13.29030133659708746, -11.09922568453595026 ) ) ;
#29613 = EDGE_LOOP ( 'NONE', ( #59506, #55610, #30032, #77907, #53625, #16773 ) ) ;
#29614 = CARTESIAN_POINT ( 'NONE',  ( 15.44008868035555260, 29.73035201082150891, 9.422509992056143702 ) ) ;
#29615 = SURFACE_SIDE_STYLE ('',( #75627 ) ) ;
#29616 = CARTESIAN_POINT ( 'NONE',  ( 20.88017736071110875, 25.77201867748816966, -2.915334737309920765 ) ) ;
#29617 = CARTESIAN_POINT ( 'NONE',  ( 2.035157376598824452, 68.68868534415484817, 7.964842623401179544 ) ) ;
#29618 = CARTESIAN_POINT ( 'NONE',  ( 24.16423886937410614, 39.30374883491396787, 8.672049930838204340E-16 ) ) ;
#29619 = CARTESIAN_POINT ( 'NONE',  ( 0.1532563361054082862, 16.21726448433411960, 2.638427012816831674 ) ) ;
#29620 = CARTESIAN_POINT ( 'NONE',  ( 12.91533473730992121, 49.52201867748817676, 10.88017736071110164 ) ) ;
#29621 = CARTESIAN_POINT ( 'NONE',  ( 19.72487221294571214, 37.80223176428831522, -6.499999999999988454 ) ) ;
#29622 = CARTESIAN_POINT ( 'NONE',  ( 24.16423886937410614, 4.303748834913967869, 8.672049930838204340E-16 ) ) ;
#29623 = EDGE_CURVE ( 'NONE', #5095, #42806, #68350, .T. ) ;
#29624 = ORIENTED_EDGE ( 'NONE', *, *, #60493, .T. ) ;
#29625 = LINE ( 'NONE', #90135, #27379 ) ;
#29626 = CARTESIAN_POINT ( 'NONE',  ( 1.472469842513823179, 65.59226448433412315, -4.923371831947296329 ) ) ;
#29627 = VERTEX_POINT ( 'NONE', #75375 ) ;
#29628 = VECTOR ( 'NONE', #40431, 1000.000000000000000 ) ;
#29629 = CARTESIAN_POINT ( 'NONE',  ( 6.204703633549690345, 17.84541550158063217, 14.16423886937410082 ) ) ;
#29630 = CARTESIAN_POINT ( 'NONE',  ( 17.08211943468705840, 20.13708216824730357, -12.26659068614894466 ) ) ;
#29631 = CARTESIAN_POINT ( 'NONE',  ( 0.5774900079438607392, 63.48035201082149825, 5.440088680355550821 ) ) ;
#29632 = CARTESIAN_POINT ( 'NONE',  ( -4.164238869374098151, 66.59541550158060375, -3.795296366450310543 ) ) ;
#29633 = CARTESIAN_POINT ( 'NONE',  ( 21.09922568453594849, 1.206968003263753531, 6.408140936763242479 ) ) ;
#29634 = CARTESIAN_POINT ( 'NONE',  ( 10.00000000000000178, 47.25893115100078745, 9.846743663894594434 ) ) ;
#29635 = CARTESIAN_POINT ( 'NONE',  ( -11.16005593728303324, -52.90553718812902417, 4.000000000003606004 ) ) ;
#29637 = CARTESIAN_POINT ( 'NONE',  ( 3.591859063236761518, 19.95696800326375353, 11.09922568453594849 ) ) ;
#29636 = CARTESIAN_POINT ( 'NONE',  ( 15.44008868035555793, 46.39701867748817676, -9.422509992056140149 ) ) ;
#29638 = CARTESIAN_POINT ( 'NONE',  ( -4.164238869374099039, 11.80374883491396965, 8.674139862899312516E-16 ) ) ;
#29639 = CARTESIAN_POINT ( 'NONE',  ( 19.42250999205614193, 10.14701867748816966, 5.440088680355555262 ) ) ;
#29640 = AXIS2_PLACEMENT_3D ( 'NONE', #1495, #46961, #8969 ) ;
#29641 = CARTESIAN_POINT ( 'NONE',  ( -0.8801773607111009756, 18.06368534415484106, 1.068504757029289695E-15 ) ) ;
#29642 = SURFACE_STYLE_USAGE ( .BOTH. , #98185 ) ;
#29643 = CARTESIAN_POINT ( 'NONE',  ( 20.88017736071110519, 60.56368534415484106, 2.639326808657452039E-16 ) ) ;
#29644 = CARTESIAN_POINT ( 'NONE',  ( 16.40814093676324603, 47.45696800326375353, -11.09922568453594671 ) ) ;
#29645 = CARTESIAN_POINT ( 'NONE',  ( 9.846743663894590881, -26.28273551566587685, -2.638427012816833894 ) ) ;
#29646 = ORIENTED_EDGE ( 'NONE', *, *, #5217, .T. ) ;
#29647 = CARTESIAN_POINT ( 'NONE',  ( 0.000000000000000000, 15.00000000000000000, 0.000000000000000000 ) ) ;
#29648 = SURFACE_STYLE_FILL_AREA ( #67682 ) ;
#29649 = CARTESIAN_POINT ( 'NONE',  ( 12.63842701281683034, 32.46726448433412315, 9.846743663894596210 ) ) ;
#29650 = ORIENTED_EDGE ( 'NONE', *, *, #79964, .F. ) ;
#29651 = CARTESIAN_POINT ( 'NONE',  ( -0.1038446121089042773, 19.24302437010793199, -6.337995344473781323 ) ) ;
#29653 = CARTESIAN_POINT ( 'NONE',  ( 17.08211943468705130, 58.47041550158063927, 12.26659068614894998 ) ) ;
#29652 = CARTESIAN_POINT ( 'NONE',  ( 10.00000000000000000, 50.55374883491396787, -14.16423886937410082 ) ) ;
#29655 = CARTESIAN_POINT ( 'NONE',  ( 12.63842701281683922, 49.55059781766744464, -9.846743663894590881 ) ) ;
#29654 = CARTESIAN_POINT ( 'NONE',  ( 1.472469842513823179, 25.59226448433412315, -4.923371831947296329 ) ) ;
#29656 = CARTESIAN_POINT ( 'NONE',  ( 21.92686044187657401, 50.37045670184115664, -3.195792623639525765 ) ) ;
#29657 = LINE ( 'NONE', #69651, #12904 ) ;
#29658 = CARTESIAN_POINT ( 'NONE',  ( 7.084665262690076126, 62.02201867748816966, -10.88017736071110164 ) ) ;
#29659 = CIRCLE ( 'NONE', #93545, 6.999999999999995559 ) ;
#29660 = B_SPLINE_CURVE_WITH_KNOTS ( 'NONE', 3,
 ( #19786, #27778, #58263, #89274, #88778, #57780 ),
 .UNSPECIFIED., .F., .F.,
 ( 4, 2, 4 ),
 ( 0.0002800124554209686796, 0.0006862178066679820113, 0.001092423157914995235 ),
 .UNSPECIFIED. ) ;
#29661 = CARTESIAN_POINT ( 'NONE',  ( 6.408140936763243367, 15.79030133659708923, 11.09922568453594494 ) ) ;
#29662 = ORIENTED_EDGE ( 'NONE', *, *, #75684, .T. ) ;
#29663 = EDGE_CURVE ( 'NONE', #38633, #74198, #28403, .T. ) ;
#29664 = CARTESIAN_POINT ( 'NONE',  ( 20.36894250292379382, 38.67874883491396076, 10.36894250292379205 ) ) ;
#29665 = CARTESIAN_POINT ( 'NONE',  ( -2.816281873526473856, 29.12363466993041783, 9.499525473075851096E-16 ) ) ;
#29666 = ORIENTED_EDGE ( 'NONE', *, *, #71019, .F. ) ;
#29667 = CARTESIAN_POINT ( 'NONE',  ( -2.816281873526473856, 59.33196800326374643, 3.434112377981055619 ) ) ;
#29668 = CARTESIAN_POINT ( 'NONE',  ( 15.44008868035555793, 31.39701867748817676, -9.422509992056140149 ) ) ;
#29669 = CARTESIAN_POINT ( 'NONE',  ( 5.076628168052703671, 36.84226448433412315, 8.527530157486179263 ) ) ;
#29670 = CARTESIAN_POINT ( 'NONE',  ( 0.5774900079438607392, 28.48035201082150891, 5.440088680355550821 ) ) ;
#29671 = DIRECTION ( 'NONE',  ( -0.000000000000000000, -0.000000000000000000, -1.000000000000000000 ) ) ;
#29672 = FACE_OUTER_BOUND ( 'NONE', #68405, .T. ) ;
#29673 = CARTESIAN_POINT ( 'NONE',  ( 10.00000000000000178, 47.25893115100078745, 9.846743663894594434 ) ) ;
#29674 = CARTESIAN_POINT ( 'NONE',  ( 7.361572987183170547, 57.05059781766744464, 9.846743663894590881 ) ) ;
#29675 = AXIS2_PLACEMENT_3D ( 'NONE', #54190, #16208, #46691 ) ;
#29676 = ADVANCED_FACE ( 'NONE', ( #5906 ), #29377, .T. ) ;
#29678 = ORIENTED_EDGE ( 'NONE', *, *, #17411, .F. ) ;
#29677 = CARTESIAN_POINT ( 'NONE',  ( 12.99999999999999822, 75.00000000000000000, 6.500000000000000888 ) ) ;
#29679 = CARTESIAN_POINT ( 'NONE',  ( 4.469999999999999751, 36.75000000000000000, 4.000000000000000000 ) ) ;
#29680 = LINE ( 'NONE', #90685, #56216 ) ;
#29681 = CARTESIAN_POINT ( 'NONE',  ( 17.85158348494334746, 59.73726573380444194, -6.500000000000027534 ) ) ;
#29682 = EDGE_CURVE ( 'NONE', #75564, #55756, #37403, .T. ) ;
#29683 = CARTESIAN_POINT ( 'NONE',  ( 6.000000000000000000, 11.00000000000000000, -6.000000000000000000 ) ) ;
#29684 = CARTESIAN_POINT ( 'NONE',  ( 5.076628168052703671, 36.84226448433412315, 8.527530157486179263 ) ) ;
#29685 = EDGE_CURVE ( 'NONE', #97713, #67262, #43883, .T. ) ;
#29686 = CARTESIAN_POINT ( 'NONE',  ( 6.767445849361157784, 14.63606917768312954, 13.38662304974505624 ) ) ;
#29687 = DIRECTION ( 'NONE',  ( -1.000000000000000000, 5.782411586589362323E-17, 0.000000000000000000 ) ) ;
#29688 = ORIENTED_EDGE ( 'NONE', *, *, #66504, .F. ) ;
#29689 = CARTESIAN_POINT ( 'NONE',  ( 12.63842701281683922, 59.55059781766744464, -9.846743663894590881 ) ) ;
#29690 = FACE_OUTER_BOUND ( 'NONE', #93029, .T. ) ;
#29691 = CARTESIAN_POINT ( 'NONE',  ( 19.84674366389459621, 38.50893115100078745, 7.409399052514197653E-17 ) ) ;
#29692 = CARTESIAN_POINT ( 'NONE',  ( -4.164238869374099927, 32.01208216824730357, 3.795296366450308767 ) ) ;
#29693 = CARTESIAN_POINT ( 'NONE',  ( 0.1532563361054083140, 51.00893115100078745, 1.131784320476157264E-15 ) ) ;
#29694 = CARTESIAN_POINT ( 'NONE',  ( 19.38216949554541557, 47.24863466993041783, -9.382169495545420901 ) ) ;
#29696 = FILL_AREA_STYLE ('',( #51731 ) ) ;
#29695 = CARTESIAN_POINT ( 'NONE',  ( 38.04706783004212411, 12.00000000000001066, -7.000000000000000000 ) ) ;
#29697 = CARTESIAN_POINT ( 'NONE',  ( 1.472469842513823179, 0.5922644843341181575, -4.923371831947296329 ) ) ;
#29698 = SURFACE_SIDE_STYLE ('',( #14230 ) ) ;
#29699 = CARTESIAN_POINT ( 'NONE',  ( 17.20831665107776587, 42.88393115100077324, 7.208316651077764980 ) ) ;
#29700 = CARTESIAN_POINT ( 'NONE',  ( 0.5774900079438590739, 37.64701867748817676, -5.440088680355550821 ) ) ;
#29701 = COLOUR_RGB ( '', 0.08235294, 0.09019608, 0.10196078) ;
#29702 = CARTESIAN_POINT ( 'NONE',  ( 14.92337183194729988, 39.34226448433412315, -8.527530157486177487 ) ) ;
#29703 = DIRECTION ( 'NONE',  ( 0.000000000000000000, 0.000000000000000000, 1.000000000000000000 ) ) ;
#29704 = CIRCLE ( 'NONE', #74385, 11.99999999999999645 ) ;
#29705 = EDGE_CURVE ( 'NONE', #50542, #16647, #74229, .T. ) ;
#29706 = CARTESIAN_POINT ( 'NONE',  ( 15.44008868035555793, 46.39701867748817676, -9.422509992056140149 ) ) ;
#29707 = CIRCLE ( 'NONE', #80830, 14.49999999999999822 ) ;
#29708 = ORIENTED_EDGE ( 'NONE', *, *, #59796, .F. ) ;
#29709 = CARTESIAN_POINT ( 'NONE',  ( 0.6076426042653109150, 22.37576471608601381, -6.499999999999992006 ) ) ;
#29710 = CARTESIAN_POINT ( 'NONE',  ( 7.084665262690076126, 9.105352010821503583, 10.88017736071109987 ) ) ;
#29712 = CARTESIAN_POINT ( 'NONE',  ( 2.035157376598824452, 43.68868534415484106, 7.964842623401179544 ) ) ;
#29711 = CARTESIAN_POINT ( 'NONE',  ( 16.40814093676323893, 0.7903013365970867898, 11.09922568453595026 ) ) ;
#29713 = CARTESIAN_POINT ( 'NONE',  ( 0.2751277870542969683, 2.282175860852373894, -6.500000000000000888 ) ) ;
#29714 = ADVANCED_FACE ( 'NONE', ( #59878 ), #42916, .F. ) ;
#29715 = DIRECTION ( 'NONE',  ( -1.000000000000000000, -0.000000000000000000, -0.000000000000000000 ) ) ;
#29716 = CARTESIAN_POINT ( 'NONE',  ( 13.50171220565083807, 15.00000000000000711, 5.622479820943917517 ) ) ;
#29718 = CARTESIAN_POINT ( 'NONE',  ( -46.58287598127274975, 100.7776474196661525, 9.484240826427258853 ) ) ;
#29717 = CARTESIAN_POINT ( 'NONE',  ( 19.42250999205614193, 35.14701867748816966, 5.440088680355555262 ) ) ;
#29719 = CARTESIAN_POINT ( 'NONE',  ( 1.472469842513823179, 15.59226448433411960, -4.923371831947296329 ) ) ;
#29720 = CARTESIAN_POINT ( 'NONE',  ( 7.361572987183169658, 19.96726448433411960, -9.846743663894592657 ) ) ;
#29721 = FILL_AREA_STYLE ('',( #59730 ) ) ;
#29722 = CARTESIAN_POINT ( 'NONE',  ( -3.795296366450322534, 25.76208216824730357, -14.16423886937409904 ) ) ;
#29723 = CARTESIAN_POINT ( 'NONE',  ( 0.1532563361054100626, 60.80059781766744464, -2.638427012816831230 ) ) ;
#29724 = CARTESIAN_POINT ( 'NONE',  ( 10.00000000000000000, 60.55374883491397497, -14.16423886937410082 ) ) ;
#29725 = CARTESIAN_POINT ( 'NONE',  ( 20.15039907845753575, 35.60158574516643171, -6.262539305110076171 ) ) ;
#29726 = CARTESIAN_POINT ( 'NONE',  ( 24.16423886937410614, 19.30374883491397142, 8.672049930838204340E-16 ) ) ;
#29727 = CARTESIAN_POINT ( 'NONE',  ( 24.16423886937410614, 44.30374883491397497, 8.672049930838204340E-16 ) ) ;
#29728 = CARTESIAN_POINT ( 'NONE',  ( 12.91533473730992121, 4.522018677488169658, 10.88017736071110164 ) ) ;
#29729 = ORIENTED_EDGE ( 'NONE', *, *, #24423, .T. ) ;
#29730 = CARTESIAN_POINT ( 'NONE',  ( 19.84674366389459266, 18.71726448433411960, -2.638427012816827677 ) ) ;
#29731 = CARTESIAN_POINT ( 'NONE',  ( 0.5774900079438590739, 7.647018677488171434, -5.440088680355550821 ) ) ;
#29732 = CARTESIAN_POINT ( 'NONE',  ( 17.20831665107776587, 54.13393115100079456, -7.208316651077762316 ) ) ;
#29733 = CARTESIAN_POINT ( 'NONE',  ( 17.08211943468705130, 8.470415501580635720, 12.26659068614894998 ) ) ;
#29734 = CARTESIAN_POINT ( 'NONE',  ( -7.750000000000000000, 79.82179676972448590, 4.250000000000000000 ) ) ;
#29735 = CARTESIAN_POINT ( 'NONE',  ( 17.20831665107776587, 2.883931151000785231, 7.208316651077764980 ) ) ;
#29736 = CARTESIAN_POINT ( 'NONE',  ( -2.816281873526471635, 43.91530133659708923, -3.434112377981056508 ) ) ;
#29737 = CARTESIAN_POINT ( 'NONE',  ( 10.00000000000000178, 37.25893115100078745, 9.846743663894594434 ) ) ;
#29738 = ORIENTED_EDGE ( 'NONE', *, *, #40260, .F. ) ;
#29739 = CARTESIAN_POINT ( 'NONE',  ( 14.92337183194729633, 2.675597817667451750, 8.527530157486181039 ) ) ;
#29740 = CARTESIAN_POINT ( 'NONE',  ( 9.511402282543471642, -15.49422404099329498, -3.750000000000000000 ) ) ;
#29741 = FACE_OUTER_BOUND ( 'NONE', #68298, .T. ) ;
#29742 = CARTESIAN_POINT ( 'NONE',  ( 0.5774900079438607392, 8.480352010821505360, 5.440088680355550821 ) ) ;
#29743 = CARTESIAN_POINT ( 'NONE',  ( -2.266590686148945544, 51.38708216824730357, -7.082119434687050408 ) ) ;
#29744 = CARTESIAN_POINT ( 'NONE',  ( 20.88017736071110519, 45.56368534415484106, 2.639326808657452039E-16 ) ) ;
#29745 = CARTESIAN_POINT ( 'NONE',  ( 24.16423886937409904, 4.095415501580634832, 3.795296366450317205 ) ) ;
#29746 =( NAMED_UNIT ( * ) SI_UNIT ( $, .STERADIAN. ) SOLID_ANGLE_UNIT ( ) );
#29747 = CARTESIAN_POINT ( 'NONE',  ( 12.63842701281683034, 27.46726448433411250, 9.846743663894596210 ) ) ;
#29748 = CARTESIAN_POINT ( 'NONE',  ( 2.035157376598822676, 12.43868534415483751, -7.964842623401177768 ) ) ;
#29749 = CARTESIAN_POINT ( 'NONE',  ( 18.52753015748618282, 38.92559781766745175, -4.923371831947291888 ) ) ;
#29750 =( NAMED_UNIT ( * ) PLANE_ANGLE_UNIT ( ) SI_UNIT ( $, .RADIAN. ) );
#29751 = CARTESIAN_POINT ( 'NONE',  ( 14.92337183194729988, 49.34226448433411605, -8.527530157486177487 ) ) ;
#29752 = AXIS2_PLACEMENT_3D ( 'NONE', #11062, #72050, #3579 ) ;
#29753 = CARTESIAN_POINT ( 'NONE',  ( 20.88017736071110519, 35.56368534415484106, 2.639326808657452039E-16 ) ) ;
#29754 = ORIENTED_EDGE ( 'NONE', *, *, #55694, .T. ) ;
#29755 = CARTESIAN_POINT ( 'NONE',  ( 0.6178305044545818747, 63.49863466993043204, -9.382169495545419124 ) ) ;
#29756 = LINE ( 'NONE', #60264, #68435 ) ;
#29757 = CARTESIAN_POINT ( 'NONE',  ( 12.63842701281683034, 2.467264484334118269, 9.846743663894596210 ) ) ;
#29758 = CARTESIAN_POINT ( 'NONE',  ( -2.816281873526471635, 38.91530133659708213, -3.434112377981056508 ) ) ;
#29760 = CARTESIAN_POINT ( 'NONE',  ( 7.361572987183169658, 34.96726448433411605, -9.846743663894592657 ) ) ;
#29759 = CARTESIAN_POINT ( 'NONE',  ( 2.035157376598824452, 3.688685344154837953, 7.964842623401179544 ) ) ;
#29761 = CARTESIAN_POINT ( 'NONE',  ( 20.00000000000000711, 85.81090550034849684, 4.886738312308601451 ) ) ;
#29762 = DIRECTION ( 'NONE',  ( 0.000000000000000000, 1.000000000000000000, 0.000000000000000000 ) ) ;
#29763 = CARTESIAN_POINT ( 'NONE',  ( 24.16423886937409904, 34.09541550158064638, 3.795296366450317205 ) ) ;
#29764 = CARTESIAN_POINT ( 'NONE',  ( 17.08211943468705130, 43.47041550158063927, 12.26659068614894998 ) ) ;
#29765 = CARTESIAN_POINT ( 'NONE',  ( 10.00000000000000178, 52.25893115100078745, 9.846743663894594434 ) ) ;
#29766 = PRESENTATION_STYLE_ASSIGNMENT (( #7292 ) ) ;
#29767 = CARTESIAN_POINT ( 'NONE',  ( 12.91533473730992121, 39.52201867748817676, 10.88017736071110164 ) ) ;
#29768 = CARTESIAN_POINT ( 'NONE',  ( 7.361572987183170547, 7.050597817667451750, 9.846743663894590881 ) ) ;
#29769 = ORIENTED_EDGE ( 'NONE', *, *, #86431, .T. ) ;
#29770 = CARTESIAN_POINT ( 'NONE',  ( 6.565887622018943937, 55.16530133659709634, 12.81628187352647430 ) ) ;
#29771 = ORIENTED_EDGE ( 'NONE', *, *, #543, .T. ) ;
#29772 = CARTESIAN_POINT ( 'NONE',  ( 1.472469842513823179, 1.425597817667451528, 4.923371831947296329 ) ) ;
#29773 = PRESENTATION_LAYER_ASSIGNMENT (  '', '', ( #28134 ) ) ;
#29774 = ORIENTED_EDGE ( 'NONE', *, *, #31392, .T. ) ;
#29775 = CARTESIAN_POINT ( 'NONE',  ( -2.266590686148945544, 12.22041550158063394, 7.082119434687048631 ) ) ;
#29776 = CARTESIAN_POINT ( 'NONE',  ( 1.472469842513823179, 1.425597817667451528, 4.923371831947296329 ) ) ;
#29777 = CARTESIAN_POINT ( 'NONE',  ( 20.88017736071110519, 25.56368534415483751, 2.639326808657452039E-16 ) ) ;
#29778 = DIRECTION ( 'NONE',  ( -0.6776733583268385042, 0.7353630527936689809, 0.000000000000000000 ) ) ;
#29779 = EDGE_LOOP ( 'NONE', ( #82081, #69671, #60038, #26613 ) ) ;
#29780 =( BOUNDED_SURFACE ( )  B_SPLINE_SURFACE ( 1, 2, ( 
 ( #69975, #60978, #84968, #92951, #30477, #91491, #83989, #23011, #53479, #70466, #46475, #76971, #24486, #16486, #54949, #8484, #85466, #9464, #3453, #49918, #4443, #33422, #18448, #71932, #64417, #34909, #47942, #87912, #65405, #88416, #56449, #33910, #19426, #80429, #72910, #79442, #11925, #48443, #70968, #42429, #41950, #86935, #78448, #94924, #87426, #64898, #10453, #48930, #10940, #2972, #95931, #27411, #17956, #63442, #41464, #40470, #9964, #26423, #56924, #79921, #18943, #78942, #72413, #57902, #49420, #11430, #40961, #3940, #2488, #32941, #71458, #63921, #94432, #25476, #93949, #34409, #55958, #95426, #86458, #26922, #25947, #57419, #96927, #90369, #28881, #13904, #12411, #88909, #50906, #73399, #20420, #66394, #21907, #20914, #73898, #52383, #28405, #74887, #6892, #75377, #67894, #19916, #51403, #35405, #6385, #81890, #13402, #58900, #82887, #43400, #89398, #65898, #89888, #98415, #14403, #80916, #21405, #43885, #42918, #74381, #37405, #5429, #29871, #36403, #5908, #66896, #44874, #97415, #81401, #51900, #44389, #36901, #60373, #59384, #58391, #29379, #82382, #12903, #97918, #50407, #96428, #4927, #67390, #59880, #27902, #35898, #61850, #92357, #69865, #7400, #45884, #45375, #68882, #37898, #14904, #16368, #84862, #91369, #76374, #46849, #9348, #53874, #61361, #54835, #38878, #22895, #23884, #77344, #8855, #1876, #46368, #30361, #1386, #76857, #53367, #31840, #85348, #68390, #75879, #412, #39370, #62337, #92845, #54348, #24372, #16860, #98910, #7889, #60869, #30864, #83874, #15398, #47335, #77836, #38381, #91870, #39852, #70357, #32332, #90870, #23389, #22399, #84384, #15884, #52876, #83382, #8370, #69369, #889, #31350, #79808, #25357, #71340, #94313, #17840, #34283, #87792, #32822, #78330, #25838, #55340, #93337, #18334, #2858, #94808, #48814, #63319, #56810, #42308, #79321, #56334, #93828, #86828, #72781, #24857, #55842, #86336, #48323, #40352, #95300, #64297, #70853, #10831, #11801, #11311, #4317, #40839, #33312, #64783, #71820, #87307, #85847, #78831, #10341, #17360, #63806, #41351, #26803, #3327, #33792, #57299, #26310, #18826, #49795, #19307, #62837, #47830, #49307, #9852, #41831, #72297, #3828, #80302, #2366, #58270, #43282, #80798, #5790, #84129, #30607, #95809, #36281, #73777, #27287, #89282, #53611, #88786, #91622, #51282, #68628, #20296, #5306, #12294, #66778, #15641, #61112, #57787, #97299, #35783, #88293, #20793, #46123, #50794, #23138, #81768, #96806, #66272, #158, #13280, #35283, #28771, #59266, #89768, #76611, #43771, #73286, #45624, #74261, #65779, #15146, #34790, #42802, #19793, #12783, #22641 ),
 ( #53122, #81285, #38142, #65279, #28283, #58777, #4810, #83631, #76123, #96308, #7650, #50282, #27784, #1630, #86584, #63570, #70600, #77100, #63080, #2125, #92109, #32080, #9595, #69122, #94078, #16117, #653, #8127, #71093, #38621, #84614, #78092, #17115, #25116, #46601, #69610, #1131, #62580, #10099, #25599, #92596, #77586, #93084, #24615, #56092, #31102, #48074, #18093, #48570, #16613, #55081, #78587, #31593, #2619, #55598, #33074, #61596, #23640, #40596, #8613, #32585, #54100, #39121, #24119, #62088, #47090, #54589, #85103, #9102, #39616, #70105, #86093, #85601, #47598, #40099, #93581, #17604, #58033, #42078, #57544, #66030, #49071, #20547, #73035, #42551, #96559, #18578, #50544, #95557, #34046, #41093, #65031, #72540, #4570, #4073, #56579, #27046, #28033, #35031, #11558, #34536, #88043, #50051, #96056, #79069, #88540, #10583, #19555, #65533, #80556, #80055, #12050, #64543, #27540, #20042, #79574, #81038, #49545, #95050, #57054, #12545, #26558, #43047, #58528, #3588, #87556, #11073, #73526, #5054, #41594, #35537, #89036, #71590, #3102, #33556, #64054, #94566, #72061, #26084, #87069, #19066, #44518, #52513, #13033, #7533, #59026, #43527, #51032, #15033, #81526, #28532, #22038, #60009, #68023, #89532, #13534, #44017, #6522, #53001, #38024, #36540, #21537, #75017, #67528, #68518, #74023, #90998, #47, #91507, #59523, #37032, #22529, #74520, #45506, #98549, #76006, #30496, #5553, #83515, #21042, #45007, #66532, #60995, #67029, #51531, #90016, #36030, #97059, #52029, #82023, #6040, #30001, #29501, #97551, #29013, #82522, #14039, #60508, #98046, #90504, #83020, #14537, #75513, #7027, #37533, #23026, #92480, #53996, #62967, #76502, #542, #1519, #55482, #16003, #15532, #24999, #2007, #84987, #31965, #9983, #91993, #63463, #31477, #46013, #53498, #24005, #84503, #93472, #8016, #30989, #16996, #85487, #40486, #61488, #85983, #39502, #76990, #84008, #8985, #16503, #47475, #46980, #23524, #69991, #70984, #77975, #54477, #77474, #62466, #92971, #39985, #38513, #32472, #69011, #24503, #9482, #54965, #70487, #17494, #8503, #47959, #78469, #46491, #2506, #32959, #39006, #1017, #69501, #61980, #95943, #73411, #18462, #10954, #33438, #19444, #94939, #94449, #34425, #42444, #56939, #87441, #4939, #50423, #57434, #63935, #49933, #87927, #78958, #18957, #95443, #55975, #80931, #2990, #86476, #93964, #57919, #25490, #71475, #64917, #3954, #11939, #25962, #56463, #86949, #49434, #27426, #12424, #79455, #64432, #79938, #11445, #42930, #17975, #34921, #35419, #48459, #3470, #41963, #65418, #48947, #88429, #72926, #19929, #10469, #40977 ) ),
 .UNSPECIFIED., .F., .F., .T. ) 
 B_SPLINE_SURFACE_WITH_KNOTS ( ( 2, 2 ),
 ( 3, 2, 2, 2, 2, 2, 2, 2, 2, 2, 2, 2, 2, 2, 2, 2, 2, 2, 2, 2, 2, 2, 2, 2, 2, 2, 2, 2, 2, 2, 2, 2, 2, 2, 2, 2, 2, 2, 2, 2, 2, 2, 2, 2, 2, 2, 2, 2, 2, 2, 2, 2, 2, 2, 2, 2, 2, 2, 2, 2, 2, 2, 2, 2, 2, 2, 2, 2, 2, 2, 2, 2, 2, 2, 2, 2, 2, 2, 2, 2, 2, 2, 2, 2, 2, 2, 2, 2, 2, 2, 2, 2, 2, 2, 2, 2, 2, 2, 2, 2, 2, 2, 2, 2, 2, 2, 2, 2, 2, 2, 2, 2, 2, 2, 2, 2, 2, 2, 2, 2, 2, 2, 2, 2, 2, 2, 2, 2, 2, 2, 2, 2, 2, 2, 2, 2, 2, 2, 2, 2, 2, 2, 2, 2, 2, 2, 2, 2, 2, 2, 2, 2, 2, 2, 2, 2, 2, 2, 2, 2, 2, 2, 3 ),
 ( 0.000000000000000000, 1.000000000000000000 ),
 ( 0.000000000000000000, 0.005952380952380952051, 0.01190476190476190410, 0.01785714285714285615, 0.02380952380952380820, 0.02976190476190476025, 0.03571428571428571230, 0.04166666666666666435, 0.04761904761904761640, 0.05357142857142856845, 0.05952380952380952051, 0.06547619047619047949, 0.07142857142857142461, 0.07738095238095238360, 0.08333333333333332871, 0.08928571428571428770, 0.09523809523809523281, 0.1011904761904761918, 0.1071428571428571369, 0.1130952380952380959, 0.1190476190476190410, 0.1250000000000000000, 0.1309523809523809590, 0.1369047619047619180, 0.1428571428571428492, 0.1488095238095238082, 0.1547619047619047672, 0.1607142857142857262, 0.1666666666666666574, 0.1726190476190476164, 0.1785714285714285754, 0.1845238095238095344, 0.1904761904761904656, 0.1964285714285714246, 0.2023809523809523836, 0.2083333333333333426, 0.2142857142857142738, 0.2202380952380952328, 0.2261904761904761918, 0.2321428571428571508, 0.2380952380952380820, 0.2440476190476190410, 0.2500000000000000000, 0.2559523809523809312, 0.2619047619047619180, 0.2678571428571428492, 0.2738095238095238360, 0.2797619047619047672, 0.2857142857142856984, 0.2916666666666666852, 0.2976190476190476164, 0.3035714285714285476, 0.3095238095238095344, 0.3154761904761904656, 0.3214285714285714524, 0.3273809523809523836, 0.3333333333333333148, 0.3392857142857143016, 0.3452380952380952328, 0.3511904761904761640, 0.3571428571428571508, 0.3630952380952380820, 0.3690476190476190688, 0.3750000000000000000, 0.3809523809523809312, 0.3869047619047619180, 0.3928571428571428492, 0.3988095238095238360, 0.4047619047619047672, 0.4107142857142856984, 0.4166666666666666852, 0.4226190476190476164, 0.4285714285714285476, 0.4345238095238095344, 0.4404761904761904656, 0.4464285714285714524, 0.4523809523809523836, 0.4583333333333333148, 0.4642857142857143016, 0.4702380952380952328, 0.4761904761904761640, 0.4821428571428571508, 0.4880952380952380820, 0.4940476190476190688, 0.5000000000000000000, 0.5059523809523809312, 0.5119047619047618625, 0.5178571428571429047, 0.5238095238095238360, 0.5297619047619047672, 0.5357142857142856984, 0.5416666666666666297, 0.5476190476190476719, 0.5535714285714286031, 0.5595238095238095344, 0.5654761904761904656, 0.5714285714285713969, 0.5773809523809523281, 0.5833333333333333703, 0.5892857142857143016, 0.5952380952380952328, 0.6011904761904761640, 0.6071428571428570953, 0.6130952380952381375, 0.6190476190476190688, 0.6250000000000000000, 0.6309523809523809312, 0.6369047619047618625, 0.6428571428571429047, 0.6488095238095238360, 0.6547619047619047672, 0.6607142857142856984, 0.6666666666666666297, 0.6726190476190476719, 0.6785714285714286031, 0.6845238095238095344, 0.6904761904761904656, 0.6964285714285713969, 0.7023809523809523281, 0.7083333333333333703, 0.7142857142857143016, 0.7202380952380952328, 0.7261904761904761640, 0.7321428571428570953, 0.7380952380952381375, 0.7440476190476190688, 0.7500000000000000000, 0.7559523809523809312, 0.7619047619047618625, 0.7678571428571429047, 0.7738095238095238360, 0.7797619047619047672, 0.7857142857142856984, 0.7916666666666666297, 0.7976190476190476719, 0.8035714285714286031, 0.8095238095238095344, 0.8154761904761904656, 0.8214285714285713969, 0.8273809523809523281, 0.8333333333333333703, 0.8392857142857143016, 0.8452380952380952328, 0.8511904761904761640, 0.8571428571428570953, 0.8630952380952381375, 0.8690476190476190688, 0.8750000000000000000, 0.8809523809523809312, 0.8869047619047618625, 0.8928571428571429047, 0.8988095238095238360, 0.9047619047619047672, 0.9107142857142856984, 0.9166666666666666297, 0.9226190476190476719, 0.9285714285714286031, 0.9345238095238095344, 0.9404761904761904656, 0.9464285714285713969, 0.9523809523809523281, 0.9583333333333333703, 0.9642857142857143016 ),
 .UNSPECIFIED. ) 
 GEOMETRIC_REPRESENTATION_ITEM ( )  RATIONAL_B_SPLINE_SURFACE ( (
 ( 1.000000000000000000, 0.9659258262890683122, 1.000000000000000000, 0.9659258262890683122, 1.000000000000000000, 0.9659258262890683122, 1.000000000000000000, 0.9659258262890683122, 1.000000000000000000, 0.9659258262890683122, 1.000000000000000000, 0.9659258262890683122, 1.000000000000000000, 0.9659258262890683122, 1.000000000000000000, 0.9659258262890683122, 1.000000000000000000, 0.9659258262890683122, 1.000000000000000000, 0.9659258262890683122, 1.000000000000000000, 0.9659258262890683122, 1.000000000000000000, 0.9659258262890683122, 1.000000000000000000, 0.9659258262890683122, 1.000000000000000000, 0.9659258262890683122, 1.000000000000000000, 0.9659258262890683122, 1.000000000000000000, 0.9659258262890683122, 1.000000000000000000, 0.9659258262890683122, 1.000000000000000000, 0.9659258262890683122, 1.000000000000000000, 0.9659258262890683122, 1.000000000000000000, 0.9659258262890683122, 1.000000000000000000, 0.9659258262890683122, 1.000000000000000000, 0.9659258262890683122, 1.000000000000000000, 0.9659258262890683122, 1.000000000000000000, 0.9659258262890683122, 1.000000000000000000, 0.9659258262890683122, 1.000000000000000000, 0.9659258262890683122, 1.000000000000000000, 0.9659258262890683122, 1.000000000000000000, 0.9659258262890683122, 1.000000000000000000, 0.9659258262890683122, 1.000000000000000000, 0.9659258262890683122, 1.000000000000000000, 0.9659258262890683122, 1.000000000000000000, 0.9659258262890683122, 1.000000000000000000, 0.9659258262890683122, 1.000000000000000000, 0.9659258262890683122, 1.000000000000000000, 0.9659258262890683122, 1.000000000000000000, 0.9659258262890683122, 1.000000000000000000, 0.9659258262890683122, 1.000000000000000000, 0.9659258262890683122, 1.000000000000000000, 0.9659258262890683122, 1.000000000000000000, 0.9659258262890683122, 1.000000000000000000, 0.9659258262890683122, 1.000000000000000000, 0.9659258262890683122, 1.000000000000000000, 0.9659258262890683122, 1.000000000000000000, 0.9659258262890683122, 1.000000000000000000, 0.9659258262890683122, 1.000000000000000000, 0.9659258262890683122, 1.000000000000000000, 0.9659258262890683122, 1.000000000000000000, 0.9659258262890683122, 1.000000000000000000, 0.9659258262890683122, 1.000000000000000000, 0.9659258262890683122, 1.000000000000000000, 0.9659258262890683122, 1.000000000000000000, 0.9659258262890683122, 1.000000000000000000, 0.9659258262890683122, 1.000000000000000000, 0.9659258262890683122, 1.000000000000000000, 0.9659258262890683122, 1.000000000000000000, 0.9659258262890683122, 1.000000000000000000, 0.9659258262890683122, 1.000000000000000000, 0.9659258262890683122, 1.000000000000000000, 0.9659258262890683122, 1.000000000000000000, 0.9659258262890683122, 1.000000000000000000, 0.9659258262890683122, 1.000000000000000000, 0.9659258262890683122, 1.000000000000000000, 0.9659258262890683122, 1.000000000000000000, 0.9659258262890683122, 1.000000000000000000, 0.9659258262890683122, 1.000000000000000000, 0.9659258262890683122, 1.000000000000000000, 0.9659258262890683122, 1.000000000000000000, 0.9659258262890683122, 1.000000000000000000, 0.9659258262890683122, 1.000000000000000000, 0.9659258262890683122, 1.000000000000000000, 0.9659258262890683122, 1.000000000000000000, 0.9659258262890683122, 1.000000000000000000, 0.9659258262890683122, 1.000000000000000000, 0.9659258262890683122, 1.000000000000000000, 0.9659258262890683122, 1.000000000000000000, 0.9659258262890683122, 1.000000000000000000, 0.9659258262890683122, 1.000000000000000000, 0.9659258262890683122, 1.000000000000000000, 0.9659258262890683122, 1.000000000000000000, 0.9659258262890683122, 1.000000000000000000, 0.9659258262890683122, 1.000000000000000000, 0.9659258262890683122, 1.000000000000000000, 0.9659258262890683122, 1.000000000000000000, 0.9659258262890683122, 1.000000000000000000, 0.9659258262890683122, 1.000000000000000000, 0.9659258262890683122, 1.000000000000000000, 0.9659258262890683122, 1.000000000000000000, 0.9659258262890683122, 1.000000000000000000, 0.9659258262890683122, 1.000000000000000000, 0.9659258262890683122, 1.000000000000000000, 0.9659258262890683122, 1.000000000000000000, 0.9659258262890683122, 1.000000000000000000, 0.9659258262890683122, 1.000000000000000000, 0.9659258262890683122, 1.000000000000000000, 0.9659258262890683122, 1.000000000000000000, 0.9659258262890683122, 1.000000000000000000, 0.9659258262890683122, 1.000000000000000000, 0.9659258262890683122, 1.000000000000000000, 0.9659258262890683122, 1.000000000000000000, 0.9659258262890683122, 1.000000000000000000, 0.9659258262890683122, 1.000000000000000000, 0.9659258262890683122, 1.000000000000000000, 0.9659258262890683122, 1.000000000000000000, 0.9659258262890683122, 1.000000000000000000, 0.9659258262890683122, 1.000000000000000000, 0.9659258262890683122, 1.000000000000000000, 0.9659258262890683122, 1.000000000000000000, 0.9659258262890683122, 1.000000000000000000, 0.9659258262890683122, 1.000000000000000000, 0.9659258262890683122, 1.000000000000000000, 0.9659258262890683122, 1.000000000000000000, 0.9659258262890683122, 1.000000000000000000, 0.9659258262890683122, 1.000000000000000000, 0.9659258262890683122, 1.000000000000000000, 0.9659258262890683122, 1.000000000000000000, 0.9659258262890683122, 1.000000000000000000, 0.9659258262890683122, 1.000000000000000000, 0.9659258262890683122, 1.000000000000000000, 0.9659258262890683122, 1.000000000000000000, 0.9659258262890683122, 1.000000000000000000, 0.9659258262890683122, 1.000000000000000000, 0.9659258262890683122, 1.000000000000000000, 0.9659258262890683122, 1.000000000000000000, 0.9659258262890683122, 1.000000000000000000, 0.9659258262890683122, 1.000000000000000000, 0.9659258262890683122, 1.000000000000000000, 0.9659258262890683122, 1.000000000000000000, 0.9659258262890683122, 1.000000000000000000, 0.9659258262890683122, 1.000000000000000000, 0.9659258262890683122, 1.000000000000000000, 0.9659258262890683122, 1.000000000000000000, 0.9659258262890683122, 1.000000000000000000, 0.9659258262890683122, 1.000000000000000000, 0.9659258262890683122, 1.000000000000000000, 0.9659258262890683122, 1.000000000000000000, 0.9659258262890683122, 1.000000000000000000, 0.9659258262890683122, 1.000000000000000000, 0.9659258262890683122, 1.000000000000000000, 0.9659258262890683122, 1.000000000000000000, 0.9659258262890683122, 1.000000000000000000, 0.9659258262890683122, 1.000000000000000000, 0.9659258262890683122, 1.000000000000000000, 0.9659258262890683122, 1.000000000000000000, 0.9659258262890683122, 1.000000000000000000, 0.9659258262890683122, 1.000000000000000000, 0.9659258262890683122, 1.000000000000000000, 0.9659258262890683122, 1.000000000000000000, 0.9659258262890683122, 1.000000000000000000, 0.9659258262890683122, 1.000000000000000000, 0.9659258262890683122, 1.000000000000000000, 0.9659258262890683122, 1.000000000000000000, 0.9659258262890683122, 1.000000000000000000, 0.9659258262890683122, 1.000000000000000000, 0.9659258262890683122, 1.000000000000000000, 0.9659258262890683122, 1.000000000000000000, 0.9659258262890683122, 1.000000000000000000, 0.9659258262890683122, 1.000000000000000000, 0.9659258262890683122, 1.000000000000000000, 0.9659258262890683122, 1.000000000000000000, 0.9659258262890683122, 1.000000000000000000, 0.9659258262890683122, 1.000000000000000000, 0.9659258262890683122, 1.000000000000000000),
 ( 1.000000000000000000, 0.9659258262890683122, 1.000000000000000000, 0.9659258262890683122, 1.000000000000000000, 0.9659258262890683122, 1.000000000000000000, 0.9659258262890683122, 1.000000000000000000, 0.9659258262890683122, 1.000000000000000000, 0.9659258262890683122, 1.000000000000000000, 0.9659258262890683122, 1.000000000000000000, 0.9659258262890683122, 1.000000000000000000, 0.9659258262890683122, 1.000000000000000000, 0.9659258262890683122, 1.000000000000000000, 0.9659258262890683122, 1.000000000000000000, 0.9659258262890683122, 1.000000000000000000, 0.9659258262890683122, 1.000000000000000000, 0.9659258262890683122, 1.000000000000000000, 0.9659258262890683122, 1.000000000000000000, 0.9659258262890683122, 1.000000000000000000, 0.9659258262890683122, 1.000000000000000000, 0.9659258262890683122, 1.000000000000000000, 0.9659258262890683122, 1.000000000000000000, 0.9659258262890683122, 1.000000000000000000, 0.9659258262890683122, 1.000000000000000000, 0.9659258262890683122, 1.000000000000000000, 0.9659258262890683122, 1.000000000000000000, 0.9659258262890683122, 1.000000000000000000, 0.9659258262890683122, 1.000000000000000000, 0.9659258262890683122, 1.000000000000000000, 0.9659258262890683122, 1.000000000000000000, 0.9659258262890683122, 1.000000000000000000, 0.9659258262890683122, 1.000000000000000000, 0.9659258262890683122, 1.000000000000000000, 0.9659258262890683122, 1.000000000000000000, 0.9659258262890683122, 1.000000000000000000, 0.9659258262890683122, 1.000000000000000000, 0.9659258262890683122, 1.000000000000000000, 0.9659258262890683122, 1.000000000000000000, 0.9659258262890683122, 1.000000000000000000, 0.9659258262890683122, 1.000000000000000000, 0.9659258262890683122, 1.000000000000000000, 0.9659258262890683122, 1.000000000000000000, 0.9659258262890683122, 1.000000000000000000, 0.9659258262890683122, 1.000000000000000000, 0.9659258262890683122, 1.000000000000000000, 0.9659258262890683122, 1.000000000000000000, 0.9659258262890683122, 1.000000000000000000, 0.9659258262890683122, 1.000000000000000000, 0.9659258262890683122, 1.000000000000000000, 0.9659258262890683122, 1.000000000000000000, 0.9659258262890683122, 1.000000000000000000, 0.9659258262890683122, 1.000000000000000000, 0.9659258262890683122, 1.000000000000000000, 0.9659258262890683122, 1.000000000000000000, 0.9659258262890683122, 1.000000000000000000, 0.9659258262890683122, 1.000000000000000000, 0.9659258262890683122, 1.000000000000000000, 0.9659258262890683122, 1.000000000000000000, 0.9659258262890683122, 1.000000000000000000, 0.9659258262890683122, 1.000000000000000000, 0.9659258262890683122, 1.000000000000000000, 0.9659258262890683122, 1.000000000000000000, 0.9659258262890683122, 1.000000000000000000, 0.9659258262890683122, 1.000000000000000000, 0.9659258262890683122, 1.000000000000000000, 0.9659258262890683122, 1.000000000000000000, 0.9659258262890683122, 1.000000000000000000, 0.9659258262890683122, 1.000000000000000000, 0.9659258262890683122, 1.000000000000000000, 0.9659258262890683122, 1.000000000000000000, 0.9659258262890683122, 1.000000000000000000, 0.9659258262890683122, 1.000000000000000000, 0.9659258262890683122, 1.000000000000000000, 0.9659258262890683122, 1.000000000000000000, 0.9659258262890683122, 1.000000000000000000, 0.9659258262890683122, 1.000000000000000000, 0.9659258262890683122, 1.000000000000000000, 0.9659258262890683122, 1.000000000000000000, 0.9659258262890683122, 1.000000000000000000, 0.9659258262890683122, 1.000000000000000000, 0.9659258262890683122, 1.000000000000000000, 0.9659258262890683122, 1.000000000000000000, 0.9659258262890683122, 1.000000000000000000, 0.9659258262890683122, 1.000000000000000000, 0.9659258262890683122, 1.000000000000000000, 0.9659258262890683122, 1.000000000000000000, 0.9659258262890683122, 1.000000000000000000, 0.9659258262890683122, 1.000000000000000000, 0.9659258262890683122, 1.000000000000000000, 0.9659258262890683122, 1.000000000000000000, 0.9659258262890683122, 1.000000000000000000, 0.9659258262890683122, 1.000000000000000000, 0.9659258262890683122, 1.000000000000000000, 0.9659258262890683122, 1.000000000000000000, 0.9659258262890683122, 1.000000000000000000, 0.9659258262890683122, 1.000000000000000000, 0.9659258262890683122, 1.000000000000000000, 0.9659258262890683122, 1.000000000000000000, 0.9659258262890683122, 1.000000000000000000, 0.9659258262890683122, 1.000000000000000000, 0.9659258262890683122, 1.000000000000000000, 0.9659258262890683122, 1.000000000000000000, 0.9659258262890683122, 1.000000000000000000, 0.9659258262890683122, 1.000000000000000000, 0.9659258262890683122, 1.000000000000000000, 0.9659258262890683122, 1.000000000000000000, 0.9659258262890683122, 1.000000000000000000, 0.9659258262890683122, 1.000000000000000000, 0.9659258262890683122, 1.000000000000000000, 0.9659258262890683122, 1.000000000000000000, 0.9659258262890683122, 1.000000000000000000, 0.9659258262890683122, 1.000000000000000000, 0.9659258262890683122, 1.000000000000000000, 0.9659258262890683122, 1.000000000000000000, 0.9659258262890683122, 1.000000000000000000, 0.9659258262890683122, 1.000000000000000000, 0.9659258262890683122, 1.000000000000000000, 0.9659258262890683122, 1.000000000000000000, 0.9659258262890683122, 1.000000000000000000, 0.9659258262890683122, 1.000000000000000000, 0.9659258262890683122, 1.000000000000000000, 0.9659258262890683122, 1.000000000000000000, 0.9659258262890683122, 1.000000000000000000, 0.9659258262890683122, 1.000000000000000000, 0.9659258262890683122, 1.000000000000000000, 0.9659258262890683122, 1.000000000000000000, 0.9659258262890683122, 1.000000000000000000, 0.9659258262890683122, 1.000000000000000000, 0.9659258262890683122, 1.000000000000000000, 0.9659258262890683122, 1.000000000000000000, 0.9659258262890683122, 1.000000000000000000, 0.9659258262890683122, 1.000000000000000000, 0.9659258262890683122, 1.000000000000000000, 0.9659258262890683122, 1.000000000000000000, 0.9659258262890683122, 1.000000000000000000, 0.9659258262890683122, 1.000000000000000000, 0.9659258262890683122, 1.000000000000000000, 0.9659258262890683122, 1.000000000000000000, 0.9659258262890683122, 1.000000000000000000, 0.9659258262890683122, 1.000000000000000000, 0.9659258262890683122, 1.000000000000000000, 0.9659258262890683122, 1.000000000000000000, 0.9659258262890683122, 1.000000000000000000, 0.9659258262890683122, 1.000000000000000000, 0.9659258262890683122, 1.000000000000000000, 0.9659258262890683122, 1.000000000000000000, 0.9659258262890683122, 1.000000000000000000, 0.9659258262890683122, 1.000000000000000000, 0.9659258262890683122, 1.000000000000000000, 0.9659258262890683122, 1.000000000000000000, 0.9659258262890683122, 1.000000000000000000, 0.9659258262890683122, 1.000000000000000000, 0.9659258262890683122, 1.000000000000000000, 0.9659258262890683122, 1.000000000000000000, 0.9659258262890683122, 1.000000000000000000, 0.9659258262890683122, 1.000000000000000000, 0.9659258262890683122, 1.000000000000000000, 0.9659258262890683122, 1.000000000000000000, 0.9659258262890683122, 1.000000000000000000, 0.9659258262890683122, 1.000000000000000000, 0.9659258262890683122, 1.000000000000000000, 0.9659258262890683122, 1.000000000000000000, 0.9659258262890683122, 1.000000000000000000, 0.9659258262890683122, 1.000000000000000000, 0.9659258262890683122, 1.000000000000000000) ) ) 
 REPRESENTATION_ITEM ( '' )  SURFACE ( )  );
#29781 = PRESENTATION_LAYER_ASSIGNMENT (  '', '', ( #37808 ) ) ;
#29782 = CARTESIAN_POINT ( 'NONE',  ( 0.5774900079438607392, 28.48035201082150891, 5.440088680355550821 ) ) ;
#29783 = AXIS2_PLACEMENT_3D ( 'NONE', #12596, #34102, #66590 ) ;
#29784 =( BOUNDED_CURVE ( )  B_SPLINE_CURVE ( 2, ( #61512, #69036, #45535, #38541, #54993, #37559, #76032, #7565, #76 ),
 .UNSPECIFIED., .F., .F. ) 
 B_SPLINE_CURVE_WITH_KNOTS ( ( 3, 2, 2, 2, 3 ),
 ( 0.4391432315068939940, 0.4404761904761904656, 0.4464285714285714524, 0.4523809523809523836, 0.4537139113502488552 ),
 .UNSPECIFIED. ) 
 CURVE ( )  GEOMETRIC_REPRESENTATION_ITEM ( )  RATIONAL_B_SPLINE_CURVE ( ( 0.9881565478350728959, 0.9923695281211487584, 1.000000000000000000, 0.9659258262890683122, 1.000000000000000000, 0.9659258262890683122, 1.000000000000000000, 0.9923695281211487584, 0.9881565478350728959 ) ) 
 REPRESENTATION_ITEM ( '' )  );
#29785 = VERTEX_POINT ( 'NONE', #82380 ) ;
#29786 = CARTESIAN_POINT ( 'NONE',  ( 7.084665262690076126, 37.02201867748817676, -10.88017736071110164 ) ) ;
#29787 = DIRECTION ( 'NONE',  ( 0.000000000000000000, 1.000000000000000000, 0.000000000000000000 ) ) ;
#29788 = ORIENTED_EDGE ( 'NONE', *, *, #3169, .F. ) ;
#29789 = CARTESIAN_POINT ( 'NONE',  ( 6.565887622018943937, 13.08196800326374998, -12.81628187352647608 ) ) ;
#29790 = CARTESIAN_POINT ( 'NONE',  ( 20.88017736071110519, 65.56368534415483396, 2.639326808657452039E-16 ) ) ;
#29791 = CARTESIAN_POINT ( 'NONE',  ( 0.000000000000000000, 15.00000000000000000, 0.000000000000000000 ) ) ;
#29792 = EDGE_CURVE ( 'NONE', #16296, #13218, #49036, .T. ) ;
#29794 = DIRECTION ( 'NONE',  ( 0.000000000000000000, 1.000000000000000000, 0.000000000000000000 ) ) ;
#29793 = CARTESIAN_POINT ( 'NONE',  ( 20.88017736071110519, 15.56368534415483751, 2.639326808657452039E-16 ) ) ;
#29795 = CARTESIAN_POINT ( 'NONE',  ( 14.92337183194729988, 4.342264484334117824, -8.527530157486177487 ) ) ;
#29796 = CARTESIAN_POINT ( 'NONE',  ( 0.5774900079438590739, 37.64701867748817676, -5.440088680355550821 ) ) ;
#29797 = VECTOR ( 'NONE', #93897, 1000.000000000000000 ) ;
#29798 = EDGE_CURVE ( 'NONE', #38777, #5117, #82716, .T. ) ;
#29799 = ORIENTED_EDGE ( 'NONE', *, *, #8524, .T. ) ;
#29800 = CARTESIAN_POINT ( 'NONE',  ( 6.565887622018943937, 50.16530133659708213, 12.81628187352647430 ) ) ;
#29801 = CARTESIAN_POINT ( 'NONE',  ( 15.44008868035555793, 46.39701867748817676, -9.422509992056140149 ) ) ;
#29802 = CARTESIAN_POINT ( 'NONE',  ( -15.33206046421386759, 15.00000000000000000, -4.561284726668966449 ) ) ;
#29803 = CARTESIAN_POINT ( 'NONE',  ( -1.099225684535947600, 54.54030133659708923, 6.408140936763237150 ) ) ;
#29804 = CARTESIAN_POINT ( 'NONE',  ( 15.44008868035555793, 46.39701867748817676, -9.422509992056140149 ) ) ;
#29805 = EDGE_CURVE ( 'NONE', #156, #11511, #73007, .T. ) ;
#29806 = CARTESIAN_POINT ( 'NONE',  ( 0.6178305044545818747, -1.501365330069579951, -9.382169495545419124 ) ) ;
#29807 = FACE_OUTER_BOUND ( 'NONE', #90283, .T. ) ;
#29808 = CARTESIAN_POINT ( 'NONE',  ( 5.076628168052703671, 11.84226448433411960, 8.527530157486179263 ) ) ;
#29809 = CARTESIAN_POINT ( 'NONE',  ( 6.565887622018943937, 60.16530133659707502, 12.81628187352647430 ) ) ;
#29810 = CARTESIAN_POINT ( 'NONE',  ( 1.492507162822266809, 37.19955587570481015, -6.500000000000066613 ) ) ;
#29811 = CARTESIAN_POINT ( 'NONE',  ( 12.63842701281683922, 4.550597817667451750, -9.846743663894590881 ) ) ;
#29812 = CARTESIAN_POINT ( 'NONE',  ( -2.816281873526473856, 9.331968003263753531, 3.434112377981055619 ) ) ;
#29814 = CARTESIAN_POINT ( 'NONE',  ( 1.472469842513823179, 60.59226448433412315, -4.923371831947296329 ) ) ;
#29813 = FACE_OUTER_BOUND ( 'NONE', #39291, .T. ) ;
#29815 = CARTESIAN_POINT ( 'NONE',  ( -0.8801773607111008646, 33.27201867748817676, 2.915334737309923430 ) ) ;
#29816 = CARTESIAN_POINT ( 'NONE',  ( 12.63842701281683034, 47.46726448433412315, 9.846743663894596210 ) ) ;
#29817 =( LENGTH_UNIT ( ) NAMED_UNIT ( * ) SI_UNIT ( .MILLI., .METRE. ) );
#29818 = CARTESIAN_POINT ( 'NONE',  ( 5.076628168052703671, 21.84226448433411960, 8.527530157486179263 ) ) ;
#29819 = CARTESIAN_POINT ( 'NONE',  ( 14.92337183194729633, 12.67559781766745353, 8.527530157486181039 ) ) ;
#29821 = ORIENTED_EDGE ( 'NONE', *, *, #95041, .F. ) ;
#29820 = CARTESIAN_POINT ( 'NONE',  ( -1.099225684535947600, 8.706968003263753531, -6.408140936763238038 ) ) ;
#29822 = CARTESIAN_POINT ( 'NONE',  ( 10.00000000000000000, 64.75893115100078035, -9.846743663894594434 ) ) ;
#29823 = CARTESIAN_POINT ( 'NONE',  ( 6.033511671519392827, -36.04540650267304613, -2.499999999999998224 ) ) ;
#29824 = CARTESIAN_POINT ( 'NONE',  ( 15.44008868035555260, 4.730352010821505360, 9.422509992056143702 ) ) ;
#29825 = CARTESIAN_POINT ( 'NONE',  ( 10.00000000000000000, 44.75893115100078745, -9.846743663894594434 ) ) ;
#29826 = PRESENTATION_LAYER_ASSIGNMENT (  '', '', ( #39420 ) ) ;
#29827 = CARTESIAN_POINT ( 'NONE',  ( 0.2751277870542967463, 0.000000000000000000, 6.500000000000000888 ) ) ;
#29828 = CARTESIAN_POINT ( 'NONE',  ( 10.00000000000000000, 65.55374883491396076, -14.16423886937410082 ) ) ;
#29829 = DIRECTION ( 'NONE',  ( 1.000000000000000000, 0.000000000000000000, 0.000000000000000000 ) ) ;
#29830 = ADVANCED_FACE ( 'NONE', ( #24854 ), #8367, .T. ) ;
#29831 = CARTESIAN_POINT ( 'NONE',  ( 19.42250999205614193, 30.14701867748817321, 5.440088680355555262 ) ) ;
#29832 = CARTESIAN_POINT ( 'NONE',  ( 2.917880565312950480, 55.97041550158063217, -12.26659068614894821 ) ) ;
#29834 = CARTESIAN_POINT ( 'NONE',  ( 12.07856007377828078, 4.686601975994315497E-16, -8.022367888854837759 ) ) ;
#29833 = CARTESIAN_POINT ( 'NONE',  ( -0.8801773607110991993, 2.855352010821504471, -2.915334737309923874 ) ) ;
#29835 = CARTESIAN_POINT ( 'NONE',  ( 12.63842701281683922, 4.550597817667451750, -9.846743663894590881 ) ) ;
#29836 = CARTESIAN_POINT ( 'NONE',  ( 7.361572987183170547, 27.05059781766745175, 9.846743663894590881 ) ) ;
#29837 = CARTESIAN_POINT ( 'NONE',  ( 10.00000000000000178, 15.37363466993042138, 12.81628187352647608 ) ) ;
#29838 = CARTESIAN_POINT ( 'NONE',  ( 38.04706783004212411, 44.99999999999999289, 7.000000000000000000 ) ) ;
#29839 =( LENGTH_UNIT ( ) NAMED_UNIT ( * ) SI_UNIT ( .MILLI., .METRE. ) );
#29840 = CARTESIAN_POINT ( 'NONE',  ( 19.84674366389459266, 58.30059781766745886, 2.638427012816836559 ) ) ;
#29841 = DIRECTION ( 'NONE',  ( -0.000000000000000000, -1.000000000000000000, -0.000000000000000000 ) ) ;
#29842 = EDGE_CURVE ( 'NONE', #62099, #50486, #14739, .T. ) ;
#29843 = DIRECTION ( 'NONE',  ( 0.000000000000000000, 0.000000000000000000, 1.000000000000000000 ) ) ;
#29844 = CARTESIAN_POINT ( 'NONE',  ( -4.164238869374098151, 16.59541550158063927, -3.795296366450310543 ) ) ;
#29845 = CARTESIAN_POINT ( 'NONE',  ( 19.84674366389459266, 23.30059781766745530, 2.638427012816836559 ) ) ;
#29846 = FACE_OUTER_BOUND ( 'NONE', #66368, .T. ) ;
#29847 = ORIENTED_EDGE ( 'NONE', *, *, #6565, .F. ) ;
#29848 = CARTESIAN_POINT ( 'NONE',  ( 20.36894250292379738, 44.92874883491396787, -10.36894250292379027 ) ) ;
#29849 = CIRCLE ( 'NONE', #98573, 0.5000000000000004441 ) ;
#29850 = CARTESIAN_POINT ( 'NONE',  ( 17.20831665107776587, 14.13393115100078568, -7.208316651077762316 ) ) ;
#29852 = FACE_OUTER_BOUND ( 'NONE', #60650, .T. ) ;
#29851 = DIRECTION ( 'NONE',  ( 0.9995586998285053149, 0.02970531260815256758, 0.000000000000000000 ) ) ;
#29853 = CARTESIAN_POINT ( 'NONE',  ( 20.88017736071110875, 30.77201867748816966, -2.915334737309920765 ) ) ;
#29854 = CARTESIAN_POINT ( 'NONE',  ( 10.00000000000000178, 50.37363466993042493, 12.81628187352647608 ) ) ;
#29855 = CARTESIAN_POINT ( 'NONE',  ( 10.00000000000000178, 40.37363466993042493, 12.81628187352647608 ) ) ;
#29856 = CARTESIAN_POINT ( 'NONE',  ( 12.63842701281683034, 7.467264484334118713, 9.846743663894596210 ) ) ;
#29857 = ORIENTED_EDGE ( 'NONE', *, *, #37822, .F. ) ;
#29858 = LINE ( 'NONE', #8357, #68615 ) ;
#29859 = CARTESIAN_POINT ( 'NONE',  ( -2.266590686148945544, 37.22041550158063217, 7.082119434687048631 ) ) ;
#29860 = CARTESIAN_POINT ( 'NONE',  ( 2.917880565312948704, 12.63708216824730179, 12.26659068614894643 ) ) ;
#29861 = CARTESIAN_POINT ( 'NONE',  ( 10.00000000000000178, 9.313685344154839285, 10.88017736071110342 ) ) ;
#29862 =( GEOMETRIC_REPRESENTATION_CONTEXT ( 3 ) GLOBAL_UNCERTAINTY_ASSIGNED_CONTEXT ( ( #35142 ) ) GLOBAL_UNIT_ASSIGNED_CONTEXT ( ( #48010, #71031, #17048 ) ) REPRESENTATION_CONTEXT ( 'NONE', 'WORKASPACE' ) );
#29863 = CARTESIAN_POINT ( 'NONE',  ( 12.91533473730992121, 19.52201867748816611, 10.88017736071110164 ) ) ;
#29864 = DIRECTION ( 'NONE',  ( 0.000000000000000000, 1.000000000000000000, 0.000000000000000000 ) ) ;
#29865 = LINE ( 'NONE', #59378, #67135 ) ;
#29866 = CARTESIAN_POINT ( 'NONE',  ( 10.00000000000000178, 59.31368534415484106, 10.88017736071110342 ) ) ;
#29867 = CARTESIAN_POINT ( 'NONE',  ( 10.00000000000000178, 59.31368534415484106, 10.88017736071110342 ) ) ;
#29868 = CARTESIAN_POINT ( 'NONE',  ( 3.591859063236761518, 24.95696800326375353, 11.09922568453594849 ) ) ;
#29869 = CARTESIAN_POINT ( 'NONE',  ( -5.810213597521888040, 0.04962897357397404868, 13.56092647078866875 ) ) ;
#29870 = LINE ( 'NONE', #52875, #70704 ) ;
#29871 = CARTESIAN_POINT ( 'NONE',  ( 5.076628168052704559, 25.17559781766745175, -8.527530157486179263 ) ) ;
#29872 = CIRCLE ( 'NONE', #98584, 1.500000000000001332 ) ;
#29873 = AXIS2_PLACEMENT_3D ( 'NONE', #38088, #37094, #67593 ) ;
#29874 = CARTESIAN_POINT ( 'NONE',  ( -2.816281873526471635, 23.91530133659708568, -3.434112377981056508 ) ) ;
#29875 = CARTESIAN_POINT ( 'NONE',  ( 1.707155281725168061, 27.90189080397291477, 6.500000000000023093 ) ) ;
#29876 = CARTESIAN_POINT ( 'NONE',  ( 19.42250999205614193, 15.14701867748817143, 5.440088680355555262 ) ) ;
#29877 = CARTESIAN_POINT ( 'NONE',  ( 1.472469842513823179, 35.59226448433412315, -4.923371831947296329 ) ) ;
#29878 = CARTESIAN_POINT ( 'NONE',  ( 10.00000000000000178, 65.37363466993042493, 12.81628187352647608 ) ) ;
#29879 = CARTESIAN_POINT ( 'NONE',  ( 17.20831665107776587, 17.88393115100078745, 7.208316651077764980 ) ) ;
#29880 = CARTESIAN_POINT ( 'NONE',  ( -4.164238869374099927, 2.012082168247300906, 3.795296366450308767 ) ) ;
#29881 = CARTESIAN_POINT ( 'NONE',  ( -5.418184704451235234, 0.000000000000000000, -0.6173241701923803948 ) ) ;
#29882 = CARTESIAN_POINT ( 'NONE',  ( 20.88017736071110519, 30.56368534415484106, 2.639326808657452039E-16 ) ) ;
#29884 = CARTESIAN_POINT ( 'NONE',  ( 24.16423886937410614, 34.30374883491396787, 8.672049930838204340E-16 ) ) ;
#29883 = CARTESIAN_POINT ( 'NONE',  ( 20.15039907845753930, 70.00000000000000000, -6.262539305110068177 ) ) ;
#29885 = CARTESIAN_POINT ( 'NONE',  ( 19.84674366389459621, 48.50893115100078745, 7.409399052514197653E-17 ) ) ;
#29886 = CARTESIAN_POINT ( 'NONE',  ( 2.035157376598822676, 27.43868534415483396, -7.964842623401177768 ) ) ;
#29887 = EDGE_CURVE ( 'NONE', #3919, #5292, #77938, .T. ) ;
#29888 = CARTESIAN_POINT ( 'NONE',  ( 20.88017736071110875, 20.77201867748816611, -2.915334737309920765 ) ) ;
#29889 = ORIENTED_EDGE ( 'NONE', *, *, #38991, .T. ) ;
#29890 = CARTESIAN_POINT ( 'NONE',  ( 20.88017736071110519, 25.56368534415483751, 2.639326808657452039E-16 ) ) ;
#29891 = EDGE_CURVE ( 'NONE', #53231, #97016, #29056, .T. ) ;
#29892 = CARTESIAN_POINT ( 'NONE',  ( 13.43411237798106583, 42.66530133659707502, -12.81628187352647252 ) ) ;
#29893 = CARTESIAN_POINT ( 'NONE',  ( 17.96484262340118221, 44.93868534415483396, 7.964842623401181321 ) ) ;
#29894 = CARTESIAN_POINT ( 'NONE',  ( 12.91533473730992121, 34.52201867748817676, 10.88017736071110164 ) ) ;
#29895 = VERTEX_POINT ( 'NONE', #39367 ) ;
#29896 = CARTESIAN_POINT ( 'NONE',  ( 19.84674366389459266, 53.71726448433411605, -2.638427012816827677 ) ) ;
#29897 = CARTESIAN_POINT ( 'NONE',  ( 20.88017736071110164, 35.35535201082150536, 2.915334737309930979 ) ) ;
#29898 = DIRECTION ( 'NONE',  ( 0.2840153447039300283, 0.000000000000000000, -0.9588197348681908316 ) ) ;
#29899 = DIRECTION ( 'NONE',  ( 0.000000000000000000, 0.000000000000000000, 1.000000000000000000 ) ) ;
#29900 = CARTESIAN_POINT ( 'NONE',  ( 24.16423886937409904, 44.09541550158063927, 3.795296366450317205 ) ) ;
#29901 = CARTESIAN_POINT ( 'NONE',  ( 2.035157376598824452, 53.68868534415484817, 7.964842623401179544 ) ) ;
#29902 = CARTESIAN_POINT ( 'NONE',  ( 0.9408516040111476464, 52.46693863883976405, -6.499999999999953815 ) ) ;
#29903 = CARTESIAN_POINT ( 'NONE',  ( -3.750000000000000888, 1.019547802438465212, -4.000000000000000000 ) ) ;
#29904 = CARTESIAN_POINT ( 'NONE',  ( 14.92337183194729988, 59.34226448433412315, -8.527530157486177487 ) ) ;
#29905 = FACE_OUTER_BOUND ( 'NONE', #67448, .T. ) ;
#29906 = CARTESIAN_POINT ( 'NONE',  ( 2.791683348922237240, 30.38393115100078390, -7.208316651077763204 ) ) ;
#29907 = ORIENTED_EDGE ( 'NONE', *, *, #49448, .F. ) ;
#29908 = CARTESIAN_POINT ( 'NONE',  ( 7.361572987183169658, 34.96726448433411605, -9.846743663894592657 ) ) ;
#29909 = CARTESIAN_POINT ( 'NONE',  ( -12.81628187352647608, -20.87636533006957507, 3.903127820947815962E-15 ) ) ;
#29910 = CARTESIAN_POINT ( 'NONE',  ( 17.96484262340118221, 26.18868534415483396, -7.964842623401177768 ) ) ;
#29911 = CARTESIAN_POINT ( 'NONE',  ( 12.63842701281683922, 44.55059781766745175, -9.846743663894590881 ) ) ;
#29912 = CARTESIAN_POINT ( 'NONE',  ( 19.38216949554541202, 15.99863466993042138, 9.382169495545424454 ) ) ;
#29914 = CARTESIAN_POINT ( 'NONE',  ( 7.084665262690076126, 54.10535201082151247, 10.88017736071109987 ) ) ;
#29913 = CARTESIAN_POINT ( 'NONE',  ( 8.879999999999991900, 27.04366094290857347, -2.900000000000000799 ) ) ;
#29915 = CARTESIAN_POINT ( 'NONE',  ( 10.00000000000000178, 29.31368534415483751, 10.88017736071110342 ) ) ;
#29916 = CARTESIAN_POINT ( 'NONE',  ( 2.917880565312948704, 42.63708216824729647, 12.26659068614894643 ) ) ;
#29917 = ADVANCED_FACE ( 'NONE', ( #16365 ), #46846, .F. ) ;
#29918 = CARTESIAN_POINT ( 'NONE',  ( 0.2751277870542967463, 70.00000000000000000, -6.000000000000000000 ) ) ;
#29919 = ORIENTED_EDGE ( 'NONE', *, *, #22377, .T. ) ;
#29920 = CARTESIAN_POINT ( 'NONE',  ( -1.099225684535947600, 13.70696800326375353, -6.408140936763238038 ) ) ;
#29921 = CARTESIAN_POINT ( 'NONE',  ( 4.559911319644449179, 12.23035201082150536, -9.422509992056141925 ) ) ;
#29922 = EDGE_CURVE ( 'NONE', #12652, #52108, #10723, .T. ) ;
#29923 = CARTESIAN_POINT ( 'NONE',  ( 19.42250999205614548, 45.98035201082150536, -5.440088680355545492 ) ) ;
#29924 = DIRECTION ( 'NONE',  ( 0.000000000000000000, -0.000000000000000000, -1.000000000000000000 ) ) ;
#29925 = ORIENTED_EDGE ( 'NONE', *, *, #50734, .F. ) ;
#29926 = CARTESIAN_POINT ( 'NONE',  ( 10.00000000000000000, 61.81368534415484106, -10.88017736071110342 ) ) ;
#29927 = CARTESIAN_POINT ( 'NONE',  ( 10.00000000000000000, 34.75893115100078745, -9.846743663894594434 ) ) ;
#29928 = CARTESIAN_POINT ( 'NONE',  ( 0.1532563361054083140, 26.00893115100078745, 1.131784320476157264E-15 ) ) ;
#29929 = AXIS2_PLACEMENT_3D ( 'NONE', #91337, #39339, #69335 ) ;
#29930 = CARTESIAN_POINT ( 'NONE',  ( 14.92337183194729988, 14.34226448433411782, -8.527530157486177487 ) ) ;
#29931 = CARTESIAN_POINT ( 'NONE',  ( 13.78891971893209245, 14.49999999999999112, 5.904717858191670388 ) ) ;
#29933 = CARTESIAN_POINT ( 'NONE',  ( 21.09922568453594849, 36.20696800326375353, 6.408140936763242479 ) ) ;
#29932 = CARTESIAN_POINT ( 'NONE',  ( -6.030006457149878152, -39.79017371238850842, 2.750000000000000000 ) ) ;
#29936 = CARTESIAN_POINT ( 'NONE',  ( -46.44000000000001194, 93.00000000000000000, -9.000000000000000000 ) ) ;
#29935 = VECTOR ( 'NONE', #80368, 1000.000000000000114 ) ;
#29934 = CARTESIAN_POINT ( 'NONE',  ( 14.92337183194729988, 19.34226448433411960, -8.527530157486177487 ) ) ;
#29937 = CARTESIAN_POINT ( 'NONE',  ( 5.170517050971795037, -13.81852248048418375, -3.999999999999999112 ) ) ;
#29939 = EDGE_LOOP ( 'NONE', ( #20352, #75176, #64369, #39920 ) ) ;
#29938 = CARTESIAN_POINT ( 'NONE',  ( 0.1532563361054082862, 36.21726448433410894, 2.638427012816831674 ) ) ;
#29940 = VECTOR ( 'NONE', #83280, 1000.000000000000000 ) ;
#29941 = CARTESIAN_POINT ( 'NONE',  ( 2.815433093577117685, 0.3639308411966863388, -14.73340885523753307 ) ) ;
#29942 = CARTESIAN_POINT ( 'NONE',  ( 13.43411237798106583, 7.665301336597086568, -12.81628187352647252 ) ) ;
#29943 = EDGE_CURVE ( 'NONE', #31636, #30124, #61848, .T. ) ;
#29944 = CARTESIAN_POINT ( 'NONE',  ( -0.8801773607111008646, 48.27201867748816966, 2.915334737309923430 ) ) ;
#29945 = CARTESIAN_POINT ( 'NONE',  ( 20.36894250292379382, 28.67874883491396787, 10.36894250292379205 ) ) ;
#29946 = CARTESIAN_POINT ( 'NONE',  ( -9.286179496273216927, 88.06418697516217264, 4.851265792411716404 ) ) ;
#29947 = CARTESIAN_POINT ( 'NONE',  ( 17.08211943468705130, 33.47041550158063927, 12.26659068614894998 ) ) ;
#29948 = EDGE_CURVE ( 'NONE', #9403, #37993, #15968, .T. ) ;
#29949 = CARTESIAN_POINT ( 'NONE',  ( 22.26659068614895176, 49.72041550158063927, -7.082119434687042414 ) ) ;
#29950 = CARTESIAN_POINT ( 'NONE',  ( 20.36894250292379382, 3.678748834913967869, 10.36894250292379205 ) ) ;
#29952 = CARTESIAN_POINT ( 'NONE',  ( 17.39651004071842166, 32.93575266056828355, 6.499999999999998224 ) ) ;
#29951 = CARTESIAN_POINT ( 'NONE',  ( 20.36894250292379382, 28.67874883491396787, 10.36894250292379205 ) ) ;
#29953 = CARTESIAN_POINT ( 'NONE',  ( 20.88017736071110875, 50.77201867748817676, -2.915334737309920765 ) ) ;
#29954 = CARTESIAN_POINT ( 'NONE',  ( -11.25000000000000000, 10.32636696231598172, 3.014428414850140570 ) ) ;
#29955 = CARTESIAN_POINT ( 'NONE',  ( 19.84674366389459266, 33.71726448433410894, -2.638427012816827677 ) ) ;
#29957 = CARTESIAN_POINT ( 'NONE',  ( 12.63842701281683034, 47.46726448433412315, 9.846743663894596210 ) ) ;
#29956 = CARTESIAN_POINT ( 'NONE',  ( 0.000000000000000000, 0.000000000000000000, 6.000000000000000000 ) ) ;
#29958 = CARTESIAN_POINT ( 'NONE',  ( 12.91533473730992121, 29.52201867748817321, 10.88017736071110164 ) ) ;
#29959 = CARTESIAN_POINT ( 'NONE',  ( 16.40814093676324603, 52.45696800326375353, -11.09922568453594671 ) ) ;
#29960 = CARTESIAN_POINT ( 'NONE',  ( 7.361572987183170547, 67.05059781766746596, 9.846743663894590881 ) ) ;
#29961 = CARTESIAN_POINT ( 'NONE',  ( -9.399392868737642459, 15.00000000000000000, -11.04089732309485861 ) ) ;
#29962 = CARTESIAN_POINT ( 'NONE',  ( 14.92337183194729988, 24.34226448433411960, -8.527530157486177487 ) ) ;
#29963 = CARTESIAN_POINT ( 'NONE',  ( 6.565887622018943937, 45.16530133659708923, 12.81628187352647430 ) ) ;
#29964 = CARTESIAN_POINT ( 'NONE',  ( 7.082119434687047743, -19.86291783175269643, -12.26659068614894821 ) ) ;
#29965 = CARTESIAN_POINT ( 'NONE',  ( 17.96484262340118221, 44.93868534415483396, 7.964842623401181321 ) ) ;
#29966 = CARTESIAN_POINT ( 'NONE',  ( 10.00000000000000178, 52.25893115100078745, 9.846743663894594434 ) ) ;
#29967 = CARTESIAN_POINT ( 'NONE',  ( -4.164238869374098151, 46.59541550158063927, -3.795296366450310543 ) ) ;
#29968 = ORIENTED_EDGE ( 'NONE', *, *, #68437, .T. ) ;
#29969 = CARTESIAN_POINT ( 'NONE',  ( -2.266590686148945544, 1.387082168247301128, -7.082119434687050408 ) ) ;
#29970 = B_SPLINE_CURVE_WITH_KNOTS ( 'NONE', 3,
 ( #49278, #87761, #11277, #50765, #12753, #26277 ),
 .UNSPECIFIED., .F., .F.,
 ( 4, 2, 4 ),
 ( 3.409110551326300585E-05, 0.0004400426677350938610, 0.0008459942299569247906 ),
 .UNSPECIFIED. ) ;
#29971 = CARTESIAN_POINT ( 'NONE',  ( 19.42250999205614548, 65.98035201082151957, -5.440088680355545492 ) ) ;
#29972 = CARTESIAN_POINT ( 'NONE',  ( 2.035157376598824452, 68.68868534415484817, 7.964842623401179544 ) ) ;
#29973 = CARTESIAN_POINT ( 'NONE',  ( 10.00000000000000000, 65.55374883491396076, -14.16423886937410082 ) ) ;
#29974 = CARTESIAN_POINT ( 'NONE',  ( 0.6178305044545838731, -0.2513653300695798953, 9.382169495545420901 ) ) ;
#29975 = DIRECTION ( 'NONE',  ( 0.000000000000000000, 0.000000000000000000, 1.000000000000000000 ) ) ;
#29976 = CARTESIAN_POINT ( 'NONE',  ( 0.5774900079438590739, 52.64701867748817676, -5.440088680355550821 ) ) ;
#29977 = DIRECTION ( 'NONE',  ( -0.000000000000000000, -0.000000000000000000, 1.000000000000000000 ) ) ;
#29978 = DIRECTION ( 'NONE',  ( 0.000000000000000000, 0.000000000000000000, -1.000000000000000000 ) ) ;
#29979 = CARTESIAN_POINT ( 'NONE',  ( 10.00000000000000178, 30.37363466993042138, 12.81628187352647608 ) ) ;
#29980 = CARTESIAN_POINT ( 'NONE',  ( -2.266590686148945544, 46.38708216824730357, -7.082119434687050408 ) ) ;
#29981 = CARTESIAN_POINT ( 'NONE',  ( -5.204170427930421283E-15, 31.81368534415485172, -10.88017736071110342 ) ) ;
#29982 = CARTESIAN_POINT ( 'NONE',  ( 0.5774900079438590739, 7.647018677488171434, -5.440088680355550821 ) ) ;
#29983 = CARTESIAN_POINT ( 'NONE',  ( 20.88017736071110875, 25.77201867748816966, -2.915334737309920765 ) ) ;
#29984 = CARTESIAN_POINT ( 'NONE',  ( 5.076628168052703671, 56.84226448433412315, 8.527530157486179263 ) ) ;
#29985 = CARTESIAN_POINT ( 'NONE',  ( 0.6178305044545818747, 48.49863466993042493, -9.382169495545419124 ) ) ;
#29986 = DIRECTION ( 'NONE',  ( 0.000000000000000000, 0.000000000000000000, 1.000000000000000000 ) ) ;
#29987 = ORIENTED_EDGE ( 'NONE', *, *, #46442, .T. ) ;
#29988 = CARTESIAN_POINT ( 'NONE',  ( -0.8801773607110991993, 12.85535201082150358, -2.915334737309923874 ) ) ;
#29989 = CARTESIAN_POINT ( 'NONE',  ( 16.40814093676324603, 17.45696800326375353, -11.09922568453594671 ) ) ;
#29990 = FACE_OUTER_BOUND ( 'NONE', #6490, .T. ) ;
#29991 = CIRCLE ( 'NONE', #68339, 0.5000000000000027756 ) ;
#29992 = CARTESIAN_POINT ( 'NONE',  ( 18.52753015748617571, 53.09226448433412315, 4.923371831947298993 ) ) ;
#29993 = CARTESIAN_POINT ( 'NONE',  ( 0.5774900079438607392, 33.48035201082150536, 5.440088680355550821 ) ) ;
#29994 = CARTESIAN_POINT ( 'NONE',  ( 19.38216949554541202, 25.99863466993042138, 9.382169495545424454 ) ) ;
#29996 = CYLINDRICAL_SURFACE ( 'NONE', #92686, 15.00000000000000000 ) ;
#29995 = CARTESIAN_POINT ( 'NONE',  ( -0.8801773607111009756, 43.06368534415484106, 1.068504757029289695E-15 ) ) ;
#29997 = CARTESIAN_POINT ( 'NONE',  ( 0.000000000000000000, 15.00000000000000000, 0.000000000000000000 ) ) ;
#29998 = CARTESIAN_POINT ( 'NONE',  ( 22.81628187352647785, 46.62363466993041783, 6.195893100308588602E-16 ) ) ;
#29999 = ORIENTED_EDGE ( 'NONE', *, *, #72345, .F. ) ;
#30000 = CARTESIAN_POINT ( 'NONE',  ( 20.88017736071110519, 45.56368534415484106, 2.639326808657452039E-16 ) ) ;
#30001 = CARTESIAN_POINT ( 'NONE',  ( 13.43411237798106583, 37.66530133659708923, -12.81628187352647252 ) ) ;
#30002 = CARTESIAN_POINT ( 'NONE',  ( 20.88017736071110875, 40.77201867748818387, -2.915334737309920765 ) ) ;
#30003 = CARTESIAN_POINT ( 'NONE',  ( 0.000000000000000000, 14.49999999999999822, 0.000000000000000000 ) ) ;
#30004 = CIRCLE ( 'NONE', #22042, 9.999999999999994671 ) ;
#30005 = CARTESIAN_POINT ( 'NONE',  ( 1.472469842513823179, 65.59226448433412315, -4.923371831947296329 ) ) ;
#30006 = CARTESIAN_POINT ( 'NONE',  ( 19.84674366389459266, 23.71726448433412315, -2.638427012816827677 ) ) ;
#30007 = CARTESIAN_POINT ( 'NONE',  ( 18.52753015748618282, 8.925597817667451750, -4.923371831947291888 ) ) ;
#30008 = CARTESIAN_POINT ( 'NONE',  ( 19.05914839598886346, 39.96693863883975695, 6.499999999999922728 ) ) ;
#30009 = CARTESIAN_POINT ( 'NONE',  ( 20.36894250292379382, 38.67874883491396076, 10.36894250292379205 ) ) ;
#30010 = CARTESIAN_POINT ( 'NONE',  ( 12.25993886608605443, 0.5000000000000004441, -8.642563219313617040 ) ) ;
#30011 = ADVANCED_FACE ( 'NONE', ( #77341 ), #7887, .T. ) ;
#30012 = VECTOR ( 'NONE', #53603, 1000.000000000000000 ) ;
#30013 = CARTESIAN_POINT ( 'NONE',  ( 7.084665262690076126, 9.105352010821503583, 10.88017736071109987 ) ) ;
#30014 = CARTESIAN_POINT ( 'NONE',  ( -7.117921737451715636, -58.38558715620306572, -3.999999999999999112 ) ) ;
#30015 = AXIS2_PLACEMENT_3D ( 'NONE', #86729, #18231, #10727 ) ;
#30016 = ORIENTED_EDGE ( 'NONE', *, *, #88507, .T. ) ;
#30017 = CARTESIAN_POINT ( 'NONE',  ( 0.5774900079438590739, 2.647018677488171434, -5.440088680355550821 ) ) ;
#30018 = CARTESIAN_POINT ( 'NONE',  ( -4.164238869374099039, 61.80374883491397497, 8.674139862899312516E-16 ) ) ;
#30019 = CARTESIAN_POINT ( 'NONE',  ( 2.791683348922240793, 46.63393115100077324, 7.208316651077764092 ) ) ;
#30020 = CARTESIAN_POINT ( 'NONE',  ( 13.43411237798106583, 37.66530133659708923, -12.81628187352647252 ) ) ;
#30022 = CARTESIAN_POINT ( 'NONE',  ( -0.3689425029237881626, 2.428748834913967869, 10.36894250292379027 ) ) ;
#30021 = DIRECTION ( 'NONE',  ( -1.776356839400250780E-14, 0.000000000000000000, 1.000000000000000000 ) ) ;
#30023 = CARTESIAN_POINT ( 'NONE',  ( 4.559911319644449179, 7.230352010821504471, -9.422509992056141925 ) ) ;
#30024 = CARTESIAN_POINT ( 'NONE',  ( -0.3689425029237898834, 51.17874883491397497, -10.36894250292378850 ) ) ;
#30025 = CARTESIAN_POINT ( 'NONE',  ( 18.52753015748618282, 48.92559781766745886, -4.923371831947291888 ) ) ;
#30026 = DIRECTION ( 'NONE',  ( -0.6626200482157408311, 0.000000000000000000, 0.7489557207889990798 ) ) ;
#30027 = CARTESIAN_POINT ( 'NONE',  ( 19.84674366389459266, 23.30059781766745530, 2.638427012816836559 ) ) ;
#30028 = CARTESIAN_POINT ( 'NONE',  ( -7.208316651077756099, 11.63393115100078212, 7.208316651077766757 ) ) ;
#30029 = ORIENTED_EDGE ( 'NONE', *, *, #45642, .F. ) ;
#30030 = ORIENTED_EDGE ( 'NONE', *, *, #34970, .F. ) ;
#30031 = CARTESIAN_POINT ( 'NONE',  ( 1.354709868695638697, 14.63606900606171557, -14.93870011653155316 ) ) ;
#30032 = ORIENTED_EDGE ( 'NONE', *, *, #56947, .T. ) ;
#30033 = CARTESIAN_POINT ( 'NONE',  ( 5.076628168052703671, 56.84226448433412315, 8.527530157486179263 ) ) ;
#30034 = CARTESIAN_POINT ( 'NONE',  ( -4.164238869374099927, 22.01208216824730357, 3.795296366450308767 ) ) ;
#30036 = CARTESIAN_POINT ( 'NONE',  ( -0.8801773607110991993, 32.85535201082151247, -2.915334737309923874 ) ) ;
#30035 = CARTESIAN_POINT ( 'NONE',  ( 15.44008868035555260, 29.73035201082150891, 9.422509992056143702 ) ) ;
#30038 = CARTESIAN_POINT ( 'NONE',  ( 22.81628187352647785, 36.62363466993041783, 6.195893100308588602E-16 ) ) ;
#30037 = CARTESIAN_POINT ( 'NONE',  ( 14.92337183194729988, 64.34226448433412315, -8.527530157486177487 ) ) ;
#30039 = CARTESIAN_POINT ( 'NONE',  ( 2.917880565312948704, 2.637082168247300906, 12.26659068614894643 ) ) ;
#30040 = CARTESIAN_POINT ( 'NONE',  ( 19.42250999205614193, 65.14701867748817676, 5.440088680355555262 ) ) ;
#30041 = EDGE_CURVE ( 'NONE', #26237, #32664, #38379, .T. ) ;
#30042 = CARTESIAN_POINT ( 'NONE',  ( 21.09922568453595559, 32.04030133659708923, -6.408140936763230044 ) ) ;
#30043 = ORIENTED_EDGE ( 'NONE', *, *, #19506, .F. ) ;
#30044 = CARTESIAN_POINT ( 'NONE',  ( 17.20831665107776587, 44.13393115100078745, -7.208316651077762316 ) ) ;
#30045 = ADVANCED_FACE ( 'NONE', ( #45373 ), #30359, .F. ) ;
#30046 = CARTESIAN_POINT ( 'NONE',  ( -0.8801773607111009756, 13.06368534415483929, 1.068504757029289695E-15 ) ) ;
#30047 = ORIENTED_EDGE ( 'NONE', *, *, #16369, .F. ) ;
#30048 = CARTESIAN_POINT ( 'NONE',  ( -0.8801773607111008646, 18.27201867748817321, 2.915334737309923430 ) ) ;
#30049 = ORIENTED_EDGE ( 'NONE', *, *, #97151, .T. ) ;
#30050 = CARTESIAN_POINT ( 'NONE',  ( 10.00000000000000000, 66.81368534415484817, -10.88017736071110342 ) ) ;
#30051 = CARTESIAN_POINT ( 'NONE',  ( 0.5774900079438607392, 53.48035201082151247, 5.440088680355550821 ) ) ;
#30052 = VECTOR ( 'NONE', #78818, 1000.000000000000000 ) ;
#30053 =( LENGTH_UNIT ( ) NAMED_UNIT ( * ) SI_UNIT ( .MILLI., .METRE. ) );
#30054 = CARTESIAN_POINT ( 'NONE',  ( 20.88017736071110875, 55.77201867748816966, -2.915334737309920765 ) ) ;
#30055 = CARTESIAN_POINT ( 'NONE',  ( 17.35999999999999943, 33.99999999999997158, -9.500000000000000000 ) ) ;
#30056 = ORIENTED_EDGE ( 'NONE', *, *, #65937, .F. ) ;
#30057 = CARTESIAN_POINT ( 'NONE',  ( 10.00000000000000178, 42.25893115100078745, 9.846743663894594434 ) ) ;
#30058 = ORIENTED_EDGE ( 'NONE', *, *, #15576, .T. ) ;
#30059 = DIRECTION ( 'NONE',  ( -0.9832549075639539504, 0.000000000000000000, -0.1822355254921514123 ) ) ;
#30060 = SURFACE_STYLE_FILL_AREA ( #90568 ) ;
#30061 = B_SPLINE_CURVE_WITH_KNOTS ( 'NONE', 3,
 ( #30594, #14645, #38610, #24105, #61099, #60608 ),
 .UNSPECIFIED., .F., .F.,
 ( 4, 2, 4 ),
 ( 0.0002800187770386834392, 0.0006862241901302594451, 0.001092429603221835559 ),
 .UNSPECIFIED. ) ;
#30062 = CARTESIAN_POINT ( 'NONE',  ( 10.00000000000000000, 5.553748834913967869, -14.16423886937410082 ) ) ;
#30063 = TOROIDAL_SURFACE ( 'NONE', #52427, 2.899999999999999911, 0.1000000000000000056 ) ;
#30064 = VERTEX_POINT ( 'NONE', #41348 ) ;
#30065 = CARTESIAN_POINT ( 'NONE',  ( -28.92076923076924544, 88.65384615384614619, -9.500000000000000000 ) ) ;
#30066 = LINE ( 'NONE', #36608, #3497 ) ;
#30067 = CARTESIAN_POINT ( 'NONE',  ( 15.44008868035555260, 4.730352010821505360, 9.422509992056143702 ) ) ;
#30068 = DIRECTION ( 'NONE',  ( -0.000000000000000000, 0.000000000000000000, 1.000000000000000000 ) ) ;
#30070 = ORIENTED_EDGE ( 'NONE', *, *, #1938, .F. ) ;
#30069 = CARTESIAN_POINT ( 'NONE',  ( -2.816281873526473856, 39.12363466993041783, 9.499525473075851096E-16 ) ) ;
#30071 = CARTESIAN_POINT ( 'NONE',  ( 38.04706783004212411, 12.00000000000001066, 7.000000000000000000 ) ) ;
#30072 = CARTESIAN_POINT ( 'NONE',  ( 12.63842701281683034, 47.46726448433412315, 9.846743663894596210 ) ) ;
#30073 = CARTESIAN_POINT ( 'NONE',  ( 8.880000000000000782, -7.313785530894214126, -3.750000000000001776 ) ) ;
#30074 = CARTESIAN_POINT ( 'NONE',  ( 22.81628187352647785, 16.62363466993042138, 6.195893100308588602E-16 ) ) ;
#30076 = ADVANCED_FACE ( 'NONE', ( #33788 ), #47827, .T. ) ;
#30075 = CARTESIAN_POINT ( 'NONE',  ( 5.076628168052703671, 21.84226448433411960, 8.527530157486179263 ) ) ;
#30077 = VECTOR ( 'NONE', #52761, 1000.000000000000000 ) ;
#30078 = DIRECTION ( 'NONE',  ( 0.000000000000000000, -1.000000000000000000, 0.000000000000000000 ) ) ;
#30079 = CARTESIAN_POINT ( 'NONE',  ( 6.565887622018943937, 0.1653013365970866511, 12.81628187352647430 ) ) ;
#30080 = SURFACE_SIDE_STYLE ('',( #22606 ) ) ;
#30081 = VERTEX_POINT ( 'NONE', #25834 ) ;
#30082 = ORIENTED_EDGE ( 'NONE', *, *, #3545, .T. ) ;
#30083 = CARTESIAN_POINT ( 'NONE',  ( 0.5774900079438590739, 27.64701867748817676, -5.440088680355550821 ) ) ;
#30084 = CARTESIAN_POINT ( 'NONE',  ( 10.00000000000000000, 15.55374883491396787, -14.16423886937410082 ) ) ;
#30085 = CARTESIAN_POINT ( 'NONE',  ( 19.84674366389459266, 23.30059781766745530, 2.638427012816836559 ) ) ;
#30086 = CARTESIAN_POINT ( 'NONE',  ( 2.791683348922237240, 0.3839311510007847872, -7.208316651077763204 ) ) ;
#30088 = CARTESIAN_POINT ( 'NONE',  ( 14.22901244993685843, 2.270048298641524909E-16, -3.387263120971315988 ) ) ;
#30087 = CARTESIAN_POINT ( 'NONE',  ( 0.6178305044545838731, 34.74863466993042493, 9.382169495545420901 ) ) ;
#30089 = CARTESIAN_POINT ( 'NONE',  ( 12.91533473730993009, 16.60535201082150891, -10.88017736071109987 ) ) ;
#30090 = LINE ( 'NONE', #37126, #3904 ) ;
#30091 = CARTESIAN_POINT ( 'NONE',  ( 3.591859063236761518, 14.95696800326375531, 11.09922568453594849 ) ) ;
#30092 = CARTESIAN_POINT ( 'NONE',  ( 16.40814093676324603, 2.456968003263753531, -11.09922568453594671 ) ) ;
#30093 = CARTESIAN_POINT ( 'NONE',  ( 10.00000000000000000, 29.75893115100078745, -9.846743663894594434 ) ) ;
#30094 = CARTESIAN_POINT ( 'NONE',  ( 10.88017736071109987, -9.227981322511825013, -2.915334737309928315 ) ) ;
#30095 = CARTESIAN_POINT ( 'NONE',  ( 22.81628187352647785, 31.62363466993042138, 6.195893100308588602E-16 ) ) ;
#30096 = CARTESIAN_POINT ( 'NONE',  ( -46.94000000000001194, 93.00000000000000000, 9.000000000000000000 ) ) ;
#30098 = CARTESIAN_POINT ( 'NONE',  ( 13.07751017357376888, 15.00000000000000000, 6.263284095430594611 ) ) ;
#30097 = CARTESIAN_POINT ( 'NONE',  ( 7.084665262690076126, 34.10535201082151247, 10.88017736071109987 ) ) ;
#30099 = CARTESIAN_POINT ( 'NONE',  ( 0.6261916924966959286, 0.5000000000000002220, 6.500000000000003553 ) ) ;
#30100 = CARTESIAN_POINT ( 'NONE',  ( 17.84635730667656262, 28.63791097397319163, 6.500000000000019540 ) ) ;
#30101 = CARTESIAN_POINT ( 'NONE',  ( 4.559911319644449179, 42.23035201082151247, -9.422509992056141925 ) ) ;
#30102 = CARTESIAN_POINT ( 'NONE',  ( 20.88017736071110875, 50.77201867748817676, -2.915334737309920765 ) ) ;
#30103 = CARTESIAN_POINT ( 'NONE',  ( 7.361572987183169658, 64.96726448433412315, -9.846743663894592657 ) ) ;
#30104 = LINE ( 'NONE', #76112, #30012 ) ;
#30105 = UNCERTAINTY_MEASURE_WITH_UNIT (LENGTH_MEASURE( 1.000000000000000082E-05 ), #11867, 'distance_accuracy_value', 'NONE');
#30106 =( BOUNDED_SURFACE ( )  B_SPLINE_SURFACE ( 1, 2, ( 
 ( #98379, #31311, #52838, #37367, #854, #38349, #46332, #77306, #8820, #39334, #52350, #14367, #69828, #38838, #92319, #98873, #21872, #68844, #68355, #54311, #29342, #59843, #22857, #29835, #82847, #22364, #30328, #44836, #75341, #6856, #60343, #61323, #14869, #45341, #7361, #91331, #83838, #15363, #45848, #80135, #31802, #95641, #50131, #96142, #32295, #78295, #58110, #4656, #62799, #72623, #26642, #9310, #9812, #20126, #27127, #4156, #34623, #80638, #50630, #65122, #57138, #49625, #24337, #39818, #12134, #40314, #81121, #27625, #70819, #2334, #57629, #35117, #93300, #24824, #11645, #42637, #42158, #87634, #32789, #43124, #19148, #88126, #19638, #55300, #63286, #93793, #73114, #65616, #88619, #85811, #12622, #1351, #62300, #17324, #92807, #54797, #85313, #16822, #47297, #77799, #70323, #1838, #47797, #60088, #6121, #28118, #35627, #43615, #5635, #97146, #58618, #74102, #36113, #30085, #98634, #83100, #44097, #44606, #97636, #74608, #83603, #28617, #5136, #96641, #60592, #13119, #81610, #14628, #52112, #29586, #91087, #22614, #53091, #89119, #20630, #15117, #90590, #22117, #36627, #66112, #21627, #13616, #45093, #52597, #75599, #67111, #66619, #73612, #59104, #29101, #51119, #98125, #89613, #21126, #14122, #7111, #51625, #82105, #75101, #59603, #90099, #82604, #6608, #37121, #67617, #37615, #68109, #76579, #23607, #2094, #47565, #8099, #16584, #69582, #53582, #54073, #63054, #70078, #47060, #77558, #24589, #93551, #9074, #1102, #92564, #68602, #84095, #55052, #84588, #25084, #70568, #16087, #46574, #39587, #78063, #38595, #69093, #24090, #85571, #54558, #31565, #77073, #86066, #62060, #85075, #62551, #627, #8585, #39091, #1598, #93056, #32049, #31073, #17085, #32553, #9566, #61571, #40067, #55567, #45593, #76091, #7621, #38113, #130, #30579, #92082, #61084, #91594, #23110, #15611, #46095, #48540, #41063, #71064, #86556, #18060, #73011, #42527, #27022, #87038, #87528, #41565, #18548, #27513, #71560, #48043, #40566, #4543, #56062, #49518, #3072, #79039, #19530, #33528, #72032, #11531, #64516, #96030, #10067, #64023, #4050, #49040, #2589, #78555, #10552, #94535, #26054, #33044, #56543, #79544, #35005, #65508, #57522, #11044, #19042, #3559, #34019, #58006, #95022, #63539, #94049, #17577, #26530, #80027, #57027, #42052, #50027, #72516, #25570, #88018, #34512, #65005, #95532, #80529, #12028, #12516, #73500, #6999, #74992, #44492, #59003, #50518, #36509, #28509, #59982, #6495, #37003, #81998, #96532, #75487, #81500, #89505, #81015, #14011, #43018, #66004, #28986, #67499, #20017, #58503, #59493, #5026, #35511, #28007, #67002 ),
 ( #22010, #89013, #20520, #29474, #51504, #73999, #97524, #98020, #13509, #29974, #43991, #37504, #74493, #51005, #89992, #36005, #44980, #67996, #21508, #13005, #43500, #90476, #5525, #66508, #21016, #6017, #52006, #82495, #98521, #52484, #97033, #82992, #14510, #88515, #53966, #61950, #23975, #38976, #39951, #31934, #988, #77944, #69962, #9450, #31448, #69467, #77443, #17, #60479, #1481, #39472, #54935, #52973, #70454, #92451, #76958, #68980, #54448, #90968, #62434, #84957, #53466, #514, #60966, #15006, #1973, #30960, #22502, #83486, #30465, #46465, #61458, #92938, #45476, #8955, #16469, #24471, #83976, #47445, #46948, #8468, #68490, #75978, #22999, #85452, #16964, #15501, #7507, #38486, #45983, #91475, #15975, #37998, #76472, #7987, #91966, #23495, #84475, #78930, #64402, #64882, #26409, #63907, #87892, #11414, #80410, #79905, #11910, #94910, #87411, #93440, #56909, #9951, #25934, #10440, #94418, #40455, #86443, #95409, #2474, #70954, #72397, #56435, #17942, #10926, #41935, #86923, #72892, #18434, #49900, #48917, #24965, #33896, #40947, #19409, #42412, #41452, #32930, #55450, #3925, #55944, #47929, #33409, #79430, #18928, #71916, #32439, #49405, #63430, #34395, #26905, #17462, #3437, #57402, #62938, #85952, #78435, #93936, #25461, #48428, #71445, #2959, #74363, #13384, #21386, #42901, #6369, #66377, #28388, #66879, #20402, #43381, #28864, #4909, #20895, #59863, #65387, #80899, #43867, #82364, #34891, #73383, #5891, #95914, #57886, #35390, #81871, #27394, #97396, #51883, #97902, #65882, #81383, #90350, #36882, #96409, #36384, #58880, #12395, #12882, #21888, #59368, #89871, #13887, #44371, #52366, #74870, #89382, #51384, #88400, #27885, #67372, #73880, #82871, #29360, #5410, #35881, #14385, #44855, #58372, #88893, #4426, #19897, #50390, #50889, #96911, #16841, #61342, #15863, #92338, #37880, #83855, #7869, #394, #23861, #53854, #60850, #54326, #31819, #84840, #7381, #30844, #15379, #8350, #91853, #69347, #23368, #54816, #67876, #22876, #61830, #38364, #29854, #37386, #45356, #68373, #98892, #60357, #75861, #30343, #62316, #1368, #16348, #45863, #46348, #84362, #76354, #85327, #91349, #6875, #98397, #92823, #14887, #38858, #53347, #68862, #77322, #76835, #83364, #46830, #871, #31330, #24353, #75361, #90851, #22382, #52856, #8836, #39350, #69844, #17821, #9329, #94294, #86317, #18806, #3307, #94789, #40821, #55320, #34265, #40331, #48303, #39832, #71802, #70835, #62817, #78810, #33294, #79302, #2838, #3809, #10811, #17341, #33770, #41329, #32312, #71320, #48794, #64277, #25817, #26782, #49289, #86810, #64767, #56790 ) ),
 .UNSPECIFIED., .F., .F., .F. ) 
 B_SPLINE_SURFACE_WITH_KNOTS ( ( 2, 2 ),
 ( 3, 2, 2, 2, 2, 2, 2, 2, 2, 2, 2, 2, 2, 2, 2, 2, 2, 2, 2, 2, 2, 2, 2, 2, 2, 2, 2, 2, 2, 2, 2, 2, 2, 2, 2, 2, 2, 2, 2, 2, 2, 2, 2, 2, 2, 2, 2, 2, 2, 2, 2, 2, 2, 2, 2, 2, 2, 2, 2, 2, 2, 2, 2, 2, 2, 2, 2, 2, 2, 2, 2, 2, 2, 2, 2, 2, 2, 2, 2, 2, 2, 2, 2, 2, 2, 2, 2, 2, 2, 2, 2, 2, 2, 2, 2, 2, 2, 2, 2, 2, 2, 2, 2, 2, 2, 2, 2, 2, 2, 2, 2, 2, 2, 2, 2, 2, 2, 2, 2, 2, 2, 2, 2, 2, 2, 2, 2, 2, 2, 2, 2, 2, 2, 2, 2, 2, 2, 2, 2, 2, 2, 2, 2, 2, 2, 2, 2, 2, 2, 2, 2, 2, 2, 2, 2, 2, 2, 2, 2, 2, 2, 2, 3 ),
 ( 0.000000000000000000, 1.000000000000000000 ),
 ( 0.000000000000000000, 0.005952380952380952051, 0.01190476190476190410, 0.01785714285714285615, 0.02380952380952380820, 0.02976190476190476025, 0.03571428571428571230, 0.04166666666666666435, 0.04761904761904761640, 0.05357142857142856845, 0.05952380952380952051, 0.06547619047619047949, 0.07142857142857142461, 0.07738095238095238360, 0.08333333333333332871, 0.08928571428571428770, 0.09523809523809523281, 0.1011904761904761918, 0.1071428571428571369, 0.1130952380952380959, 0.1190476190476190410, 0.1250000000000000000, 0.1309523809523809590, 0.1369047619047619180, 0.1428571428571428492, 0.1488095238095238082, 0.1547619047619047672, 0.1607142857142857262, 0.1666666666666666574, 0.1726190476190476164, 0.1785714285714285754, 0.1845238095238095344, 0.1904761904761904656, 0.1964285714285714246, 0.2023809523809523836, 0.2083333333333333426, 0.2142857142857142738, 0.2202380952380952328, 0.2261904761904761918, 0.2321428571428571508, 0.2380952380952380820, 0.2440476190476190410, 0.2500000000000000000, 0.2559523809523809312, 0.2619047619047619180, 0.2678571428571428492, 0.2738095238095238360, 0.2797619047619047672, 0.2857142857142856984, 0.2916666666666666852, 0.2976190476190476164, 0.3035714285714285476, 0.3095238095238095344, 0.3154761904761904656, 0.3214285714285714524, 0.3273809523809523836, 0.3333333333333333148, 0.3392857142857143016, 0.3452380952380952328, 0.3511904761904761640, 0.3571428571428571508, 0.3630952380952380820, 0.3690476190476190688, 0.3750000000000000000, 0.3809523809523809312, 0.3869047619047619180, 0.3928571428571428492, 0.3988095238095238360, 0.4047619047619047672, 0.4107142857142856984, 0.4166666666666666852, 0.4226190476190476164, 0.4285714285714285476, 0.4345238095238095344, 0.4404761904761904656, 0.4464285714285714524, 0.4523809523809523836, 0.4583333333333333148, 0.4642857142857143016, 0.4702380952380952328, 0.4761904761904761640, 0.4821428571428571508, 0.4880952380952380820, 0.4940476190476190688, 0.5000000000000000000, 0.5059523809523809312, 0.5119047619047618625, 0.5178571428571429047, 0.5238095238095238360, 0.5297619047619047672, 0.5357142857142856984, 0.5416666666666666297, 0.5476190476190476719, 0.5535714285714286031, 0.5595238095238095344, 0.5654761904761904656, 0.5714285714285713969, 0.5773809523809523281, 0.5833333333333333703, 0.5892857142857143016, 0.5952380952380952328, 0.6011904761904761640, 0.6071428571428570953, 0.6130952380952381375, 0.6190476190476190688, 0.6250000000000000000, 0.6309523809523809312, 0.6369047619047618625, 0.6428571428571429047, 0.6488095238095238360, 0.6547619047619047672, 0.6607142857142856984, 0.6666666666666666297, 0.6726190476190476719, 0.6785714285714286031, 0.6845238095238095344, 0.6904761904761904656, 0.6964285714285713969, 0.7023809523809523281, 0.7083333333333333703, 0.7142857142857143016, 0.7202380952380952328, 0.7261904761904761640, 0.7321428571428570953, 0.7380952380952381375, 0.7440476190476190688, 0.7500000000000000000, 0.7559523809523809312, 0.7619047619047618625, 0.7678571428571429047, 0.7738095238095238360, 0.7797619047619047672, 0.7857142857142856984, 0.7916666666666666297, 0.7976190476190476719, 0.8035714285714286031, 0.8095238095238095344, 0.8154761904761904656, 0.8214285714285713969, 0.8273809523809523281, 0.8333333333333333703, 0.8392857142857143016, 0.8452380952380952328, 0.8511904761904761640, 0.8571428571428570953, 0.8630952380952381375, 0.8690476190476190688, 0.8750000000000000000, 0.8809523809523809312, 0.8869047619047618625, 0.8928571428571429047, 0.8988095238095238360, 0.9047619047619047672, 0.9107142857142856984, 0.9166666666666666297, 0.9226190476190476719, 0.9285714285714286031, 0.9345238095238095344, 0.9404761904761904656, 0.9464285714285713969, 0.9523809523809523281, 0.9583333333333333703, 0.9642857142857143016 ),
 .UNSPECIFIED. ) 
 GEOMETRIC_REPRESENTATION_ITEM ( )  RATIONAL_B_SPLINE_SURFACE ( (
 ( 1.000000000000000000, 0.9659258262890683122, 1.000000000000000000, 0.9659258262890683122, 1.000000000000000000, 0.9659258262890683122, 1.000000000000000000, 0.9659258262890683122, 1.000000000000000000, 0.9659258262890683122, 1.000000000000000000, 0.9659258262890683122, 1.000000000000000000, 0.9659258262890683122, 1.000000000000000000, 0.9659258262890683122, 1.000000000000000000, 0.9659258262890683122, 1.000000000000000000, 0.9659258262890683122, 1.000000000000000000, 0.9659258262890683122, 1.000000000000000000, 0.9659258262890683122, 1.000000000000000000, 0.9659258262890683122, 1.000000000000000000, 0.9659258262890683122, 1.000000000000000000, 0.9659258262890683122, 1.000000000000000000, 0.9659258262890683122, 1.000000000000000000, 0.9659258262890683122, 1.000000000000000000, 0.9659258262890683122, 1.000000000000000000, 0.9659258262890683122, 1.000000000000000000, 0.9659258262890683122, 1.000000000000000000, 0.9659258262890683122, 1.000000000000000000, 0.9659258262890683122, 1.000000000000000000, 0.9659258262890683122, 1.000000000000000000, 0.9659258262890683122, 1.000000000000000000, 0.9659258262890683122, 1.000000000000000000, 0.9659258262890683122, 1.000000000000000000, 0.9659258262890683122, 1.000000000000000000, 0.9659258262890683122, 1.000000000000000000, 0.9659258262890683122, 1.000000000000000000, 0.9659258262890683122, 1.000000000000000000, 0.9659258262890683122, 1.000000000000000000, 0.9659258262890683122, 1.000000000000000000, 0.9659258262890683122, 1.000000000000000000, 0.9659258262890683122, 1.000000000000000000, 0.9659258262890683122, 1.000000000000000000, 0.9659258262890683122, 1.000000000000000000, 0.9659258262890683122, 1.000000000000000000, 0.9659258262890683122, 1.000000000000000000, 0.9659258262890683122, 1.000000000000000000, 0.9659258262890683122, 1.000000000000000000, 0.9659258262890683122, 1.000000000000000000, 0.9659258262890683122, 1.000000000000000000, 0.9659258262890683122, 1.000000000000000000, 0.9659258262890683122, 1.000000000000000000, 0.9659258262890683122, 1.000000000000000000, 0.9659258262890683122, 1.000000000000000000, 0.9659258262890683122, 1.000000000000000000, 0.9659258262890683122, 1.000000000000000000, 0.9659258262890683122, 1.000000000000000000, 0.9659258262890683122, 1.000000000000000000, 0.9659258262890683122, 1.000000000000000000, 0.9659258262890683122, 1.000000000000000000, 0.9659258262890683122, 1.000000000000000000, 0.9659258262890683122, 1.000000000000000000, 0.9659258262890683122, 1.000000000000000000, 0.9659258262890683122, 1.000000000000000000, 0.9659258262890683122, 1.000000000000000000, 0.9659258262890683122, 1.000000000000000000, 0.9659258262890683122, 1.000000000000000000, 0.9659258262890683122, 1.000000000000000000, 0.9659258262890683122, 1.000000000000000000, 0.9659258262890683122, 1.000000000000000000, 0.9659258262890683122, 1.000000000000000000, 0.9659258262890683122, 1.000000000000000000, 0.9659258262890683122, 1.000000000000000000, 0.9659258262890683122, 1.000000000000000000, 0.9659258262890683122, 1.000000000000000000, 0.9659258262890683122, 1.000000000000000000, 0.9659258262890683122, 1.000000000000000000, 0.9659258262890683122, 1.000000000000000000, 0.9659258262890683122, 1.000000000000000000, 0.9659258262890683122, 1.000000000000000000, 0.9659258262890683122, 1.000000000000000000, 0.9659258262890683122, 1.000000000000000000, 0.9659258262890683122, 1.000000000000000000, 0.9659258262890683122, 1.000000000000000000, 0.9659258262890683122, 1.000000000000000000, 0.9659258262890683122, 1.000000000000000000, 0.9659258262890683122, 1.000000000000000000, 0.9659258262890683122, 1.000000000000000000, 0.9659258262890683122, 1.000000000000000000, 0.9659258262890683122, 1.000000000000000000, 0.9659258262890683122, 1.000000000000000000, 0.9659258262890683122, 1.000000000000000000, 0.9659258262890683122, 1.000000000000000000, 0.9659258262890683122, 1.000000000000000000, 0.9659258262890683122, 1.000000000000000000, 0.9659258262890683122, 1.000000000000000000, 0.9659258262890683122, 1.000000000000000000, 0.9659258262890683122, 1.000000000000000000, 0.9659258262890683122, 1.000000000000000000, 0.9659258262890683122, 1.000000000000000000, 0.9659258262890683122, 1.000000000000000000, 0.9659258262890683122, 1.000000000000000000, 0.9659258262890683122, 1.000000000000000000, 0.9659258262890683122, 1.000000000000000000, 0.9659258262890683122, 1.000000000000000000, 0.9659258262890683122, 1.000000000000000000, 0.9659258262890683122, 1.000000000000000000, 0.9659258262890683122, 1.000000000000000000, 0.9659258262890683122, 1.000000000000000000, 0.9659258262890683122, 1.000000000000000000, 0.9659258262890683122, 1.000000000000000000, 0.9659258262890683122, 1.000000000000000000, 0.9659258262890683122, 1.000000000000000000, 0.9659258262890683122, 1.000000000000000000, 0.9659258262890683122, 1.000000000000000000, 0.9659258262890683122, 1.000000000000000000, 0.9659258262890683122, 1.000000000000000000, 0.9659258262890683122, 1.000000000000000000, 0.9659258262890683122, 1.000000000000000000, 0.9659258262890683122, 1.000000000000000000, 0.9659258262890683122, 1.000000000000000000, 0.9659258262890683122, 1.000000000000000000, 0.9659258262890683122, 1.000000000000000000, 0.9659258262890683122, 1.000000000000000000, 0.9659258262890683122, 1.000000000000000000, 0.9659258262890683122, 1.000000000000000000, 0.9659258262890683122, 1.000000000000000000, 0.9659258262890683122, 1.000000000000000000, 0.9659258262890683122, 1.000000000000000000, 0.9659258262890683122, 1.000000000000000000, 0.9659258262890683122, 1.000000000000000000, 0.9659258262890683122, 1.000000000000000000, 0.9659258262890683122, 1.000000000000000000, 0.9659258262890683122, 1.000000000000000000, 0.9659258262890683122, 1.000000000000000000, 0.9659258262890683122, 1.000000000000000000, 0.9659258262890683122, 1.000000000000000000, 0.9659258262890683122, 1.000000000000000000, 0.9659258262890683122, 1.000000000000000000, 0.9659258262890683122, 1.000000000000000000, 0.9659258262890683122, 1.000000000000000000, 0.9659258262890683122, 1.000000000000000000, 0.9659258262890683122, 1.000000000000000000, 0.9659258262890683122, 1.000000000000000000, 0.9659258262890683122, 1.000000000000000000, 0.9659258262890683122, 1.000000000000000000, 0.9659258262890683122, 1.000000000000000000, 0.9659258262890683122, 1.000000000000000000, 0.9659258262890683122, 1.000000000000000000, 0.9659258262890683122, 1.000000000000000000, 0.9659258262890683122, 1.000000000000000000, 0.9659258262890683122, 1.000000000000000000, 0.9659258262890683122, 1.000000000000000000, 0.9659258262890683122, 1.000000000000000000, 0.9659258262890683122, 1.000000000000000000, 0.9659258262890683122, 1.000000000000000000, 0.9659258262890683122, 1.000000000000000000, 0.9659258262890683122, 1.000000000000000000, 0.9659258262890683122, 1.000000000000000000, 0.9659258262890683122, 1.000000000000000000, 0.9659258262890683122, 1.000000000000000000, 0.9659258262890683122, 1.000000000000000000, 0.9659258262890683122, 1.000000000000000000, 0.9659258262890683122, 1.000000000000000000, 0.9659258262890683122, 1.000000000000000000, 0.9659258262890683122, 1.000000000000000000, 0.9659258262890683122, 1.000000000000000000, 0.9659258262890683122, 1.000000000000000000, 0.9659258262890683122, 1.000000000000000000, 0.9659258262890683122, 1.000000000000000000),
 ( 1.000000000000000000, 0.9659258262890683122, 1.000000000000000000, 0.9659258262890683122, 1.000000000000000000, 0.9659258262890683122, 1.000000000000000000, 0.9659258262890683122, 1.000000000000000000, 0.9659258262890683122, 1.000000000000000000, 0.9659258262890683122, 1.000000000000000000, 0.9659258262890683122, 1.000000000000000000, 0.9659258262890683122, 1.000000000000000000, 0.9659258262890683122, 1.000000000000000000, 0.9659258262890683122, 1.000000000000000000, 0.9659258262890683122, 1.000000000000000000, 0.9659258262890683122, 1.000000000000000000, 0.9659258262890683122, 1.000000000000000000, 0.9659258262890683122, 1.000000000000000000, 0.9659258262890683122, 1.000000000000000000, 0.9659258262890683122, 1.000000000000000000, 0.9659258262890683122, 1.000000000000000000, 0.9659258262890683122, 1.000000000000000000, 0.9659258262890683122, 1.000000000000000000, 0.9659258262890683122, 1.000000000000000000, 0.9659258262890683122, 1.000000000000000000, 0.9659258262890683122, 1.000000000000000000, 0.9659258262890683122, 1.000000000000000000, 0.9659258262890683122, 1.000000000000000000, 0.9659258262890683122, 1.000000000000000000, 0.9659258262890683122, 1.000000000000000000, 0.9659258262890683122, 1.000000000000000000, 0.9659258262890683122, 1.000000000000000000, 0.9659258262890683122, 1.000000000000000000, 0.9659258262890683122, 1.000000000000000000, 0.9659258262890683122, 1.000000000000000000, 0.9659258262890683122, 1.000000000000000000, 0.9659258262890683122, 1.000000000000000000, 0.9659258262890683122, 1.000000000000000000, 0.9659258262890683122, 1.000000000000000000, 0.9659258262890683122, 1.000000000000000000, 0.9659258262890683122, 1.000000000000000000, 0.9659258262890683122, 1.000000000000000000, 0.9659258262890683122, 1.000000000000000000, 0.9659258262890683122, 1.000000000000000000, 0.9659258262890683122, 1.000000000000000000, 0.9659258262890683122, 1.000000000000000000, 0.9659258262890683122, 1.000000000000000000, 0.9659258262890683122, 1.000000000000000000, 0.9659258262890683122, 1.000000000000000000, 0.9659258262890683122, 1.000000000000000000, 0.9659258262890683122, 1.000000000000000000, 0.9659258262890683122, 1.000000000000000000, 0.9659258262890683122, 1.000000000000000000, 0.9659258262890683122, 1.000000000000000000, 0.9659258262890683122, 1.000000000000000000, 0.9659258262890683122, 1.000000000000000000, 0.9659258262890683122, 1.000000000000000000, 0.9659258262890683122, 1.000000000000000000, 0.9659258262890683122, 1.000000000000000000, 0.9659258262890683122, 1.000000000000000000, 0.9659258262890683122, 1.000000000000000000, 0.9659258262890683122, 1.000000000000000000, 0.9659258262890683122, 1.000000000000000000, 0.9659258262890683122, 1.000000000000000000, 0.9659258262890683122, 1.000000000000000000, 0.9659258262890683122, 1.000000000000000000, 0.9659258262890683122, 1.000000000000000000, 0.9659258262890683122, 1.000000000000000000, 0.9659258262890683122, 1.000000000000000000, 0.9659258262890683122, 1.000000000000000000, 0.9659258262890683122, 1.000000000000000000, 0.9659258262890683122, 1.000000000000000000, 0.9659258262890683122, 1.000000000000000000, 0.9659258262890683122, 1.000000000000000000, 0.9659258262890683122, 1.000000000000000000, 0.9659258262890683122, 1.000000000000000000, 0.9659258262890683122, 1.000000000000000000, 0.9659258262890683122, 1.000000000000000000, 0.9659258262890683122, 1.000000000000000000, 0.9659258262890683122, 1.000000000000000000, 0.9659258262890683122, 1.000000000000000000, 0.9659258262890683122, 1.000000000000000000, 0.9659258262890683122, 1.000000000000000000, 0.9659258262890683122, 1.000000000000000000, 0.9659258262890683122, 1.000000000000000000, 0.9659258262890683122, 1.000000000000000000, 0.9659258262890683122, 1.000000000000000000, 0.9659258262890683122, 1.000000000000000000, 0.9659258262890683122, 1.000000000000000000, 0.9659258262890683122, 1.000000000000000000, 0.9659258262890683122, 1.000000000000000000, 0.9659258262890683122, 1.000000000000000000, 0.9659258262890683122, 1.000000000000000000, 0.9659258262890683122, 1.000000000000000000, 0.9659258262890683122, 1.000000000000000000, 0.9659258262890683122, 1.000000000000000000, 0.9659258262890683122, 1.000000000000000000, 0.9659258262890683122, 1.000000000000000000, 0.9659258262890683122, 1.000000000000000000, 0.9659258262890683122, 1.000000000000000000, 0.9659258262890683122, 1.000000000000000000, 0.9659258262890683122, 1.000000000000000000, 0.9659258262890683122, 1.000000000000000000, 0.9659258262890683122, 1.000000000000000000, 0.9659258262890683122, 1.000000000000000000, 0.9659258262890683122, 1.000000000000000000, 0.9659258262890683122, 1.000000000000000000, 0.9659258262890683122, 1.000000000000000000, 0.9659258262890683122, 1.000000000000000000, 0.9659258262890683122, 1.000000000000000000, 0.9659258262890683122, 1.000000000000000000, 0.9659258262890683122, 1.000000000000000000, 0.9659258262890683122, 1.000000000000000000, 0.9659258262890683122, 1.000000000000000000, 0.9659258262890683122, 1.000000000000000000, 0.9659258262890683122, 1.000000000000000000, 0.9659258262890683122, 1.000000000000000000, 0.9659258262890683122, 1.000000000000000000, 0.9659258262890683122, 1.000000000000000000, 0.9659258262890683122, 1.000000000000000000, 0.9659258262890683122, 1.000000000000000000, 0.9659258262890683122, 1.000000000000000000, 0.9659258262890683122, 1.000000000000000000, 0.9659258262890683122, 1.000000000000000000, 0.9659258262890683122, 1.000000000000000000, 0.9659258262890683122, 1.000000000000000000, 0.9659258262890683122, 1.000000000000000000, 0.9659258262890683122, 1.000000000000000000, 0.9659258262890683122, 1.000000000000000000, 0.9659258262890683122, 1.000000000000000000, 0.9659258262890683122, 1.000000000000000000, 0.9659258262890683122, 1.000000000000000000, 0.9659258262890683122, 1.000000000000000000, 0.9659258262890683122, 1.000000000000000000, 0.9659258262890683122, 1.000000000000000000, 0.9659258262890683122, 1.000000000000000000, 0.9659258262890683122, 1.000000000000000000, 0.9659258262890683122, 1.000000000000000000, 0.9659258262890683122, 1.000000000000000000, 0.9659258262890683122, 1.000000000000000000, 0.9659258262890683122, 1.000000000000000000, 0.9659258262890683122, 1.000000000000000000, 0.9659258262890683122, 1.000000000000000000, 0.9659258262890683122, 1.000000000000000000, 0.9659258262890683122, 1.000000000000000000, 0.9659258262890683122, 1.000000000000000000, 0.9659258262890683122, 1.000000000000000000, 0.9659258262890683122, 1.000000000000000000, 0.9659258262890683122, 1.000000000000000000, 0.9659258262890683122, 1.000000000000000000, 0.9659258262890683122, 1.000000000000000000, 0.9659258262890683122, 1.000000000000000000, 0.9659258262890683122, 1.000000000000000000, 0.9659258262890683122, 1.000000000000000000, 0.9659258262890683122, 1.000000000000000000, 0.9659258262890683122, 1.000000000000000000, 0.9659258262890683122, 1.000000000000000000, 0.9659258262890683122, 1.000000000000000000, 0.9659258262890683122, 1.000000000000000000, 0.9659258262890683122, 1.000000000000000000, 0.9659258262890683122, 1.000000000000000000, 0.9659258262890683122, 1.000000000000000000, 0.9659258262890683122, 1.000000000000000000, 0.9659258262890683122, 1.000000000000000000, 0.9659258262890683122, 1.000000000000000000, 0.9659258262890683122, 1.000000000000000000) ) ) 
 REPRESENTATION_ITEM ( '' )  SURFACE ( )  );
#30107 = CARTESIAN_POINT ( 'NONE',  ( 12.63842701281683922, 54.55059781766745175, -9.846743663894590881 ) ) ;
#30109 = CARTESIAN_POINT ( 'NONE',  ( 8.502721643904074256, 0.04962896249296737394, -12.05657636697101331 ) ) ;
#30108 = CARTESIAN_POINT ( 'NONE',  ( 10.00000000000000178, 9.313685344154839285, 10.88017736071110342 ) ) ;
#30110 = CARTESIAN_POINT ( 'NONE',  ( 21.09922568453595559, 12.04030133659708746, -6.408140936763230044 ) ) ;
#30111 = ORIENTED_EDGE ( 'NONE', *, *, #35698, .F. ) ;
#30112 = CARTESIAN_POINT ( 'NONE',  ( 7.084665262690076126, 39.10535201082150536, 10.88017736071109987 ) ) ;
#30113 = CARTESIAN_POINT ( 'NONE',  ( -13.75801628063885040, 4.154966894009843400E-16, 4.578972376164368363 ) ) ;
#30114 = CARTESIAN_POINT ( 'NONE',  ( 2.035157376598822676, 27.43868534415483396, -7.964842623401177768 ) ) ;
#30115 = CARTESIAN_POINT ( 'NONE',  ( 17.20831665107776587, 7.883931151000784787, 7.208316651077764980 ) ) ;
#30116 = CARTESIAN_POINT ( 'NONE',  ( 20.36894250292379382, 33.67874883491396076, 10.36894250292379205 ) ) ;
#30117 = CARTESIAN_POINT ( 'NONE',  ( 7.361572987183169658, 29.96726448433411960, -9.846743663894592657 ) ) ;
#30118 = MECHANICAL_DESIGN_GEOMETRIC_PRESENTATION_REPRESENTATION (  '', ( #73151 ), #42911 ) ;
#30119 = CARTESIAN_POINT ( 'NONE',  ( -0.8801773607110991993, 47.85535201082150536, -2.915334737309923874 ) ) ;
#30120 = DIRECTION ( 'NONE',  ( 0.000000000000000000, 1.000000000000000000, 0.000000000000000000 ) ) ;
#30121 = EDGE_CURVE ( 'NONE', #83033, #26759, #23516, .T. ) ;
#30122 = CARTESIAN_POINT ( 'NONE',  ( -14.56332774647470174, 14.95077488074853456, -2.357028871694378580 ) ) ;
#30123 = CARTESIAN_POINT ( 'NONE',  ( 17.20831665107776587, 62.88393115100078745, 7.208316651077764980 ) ) ;
#30124 = VERTEX_POINT ( 'NONE', #87304 ) ;
#30125 = ORIENTED_EDGE ( 'NONE', *, *, #67305, .T. ) ;
#30126 = CARTESIAN_POINT ( 'NONE',  ( 13.79529636645030344, 23.26208216824730002, 14.16423886937410614 ) ) ;
#30127 = CARTESIAN_POINT ( 'NONE',  ( 20.36894250292379738, 19.92874883491396787, -10.36894250292379027 ) ) ;
#30128 = CARTESIAN_POINT ( 'NONE',  ( 2.035157376598824452, 63.68868534415484106, 7.964842623401179544 ) ) ;
#30129 = CARTESIAN_POINT ( 'NONE',  ( 7.084665262690076126, 2.022018677488171434, -10.88017736071110164 ) ) ;
#30130 = CARTESIAN_POINT ( 'NONE',  ( 0.1532563361054083140, 51.00893115100078745, 1.131784320476157264E-15 ) ) ;
#30131 = CARTESIAN_POINT ( 'NONE',  ( -11.48887051628074829, -88.22984412037166635, 4.000000000000000000 ) ) ;
#30133 = CARTESIAN_POINT ( 'NONE',  ( -1.099225684535947600, 13.70696800326375353, -6.408140936763238038 ) ) ;
#30132 = CARTESIAN_POINT ( 'NONE',  ( 12.91533473730992121, 49.52201867748817676, 10.88017736071110164 ) ) ;
#30134 = CARTESIAN_POINT ( 'NONE',  ( 22.26659068614895176, 19.72041550158063572, -7.082119434687042414 ) ) ;
#30135 = CARTESIAN_POINT ( 'NONE',  ( 7.084665262690076126, 14.10535201082150358, 10.88017736071109987 ) ) ;
#30136 = CARTESIAN_POINT ( 'NONE',  ( 0.5774900079438607392, 28.48035201082150891, 5.440088680355550821 ) ) ;
#30137 = CARTESIAN_POINT ( 'NONE',  ( 4.559911319644449179, 58.89701867748817676, 9.422509992056141925 ) ) ;
#30138 = CARTESIAN_POINT ( 'NONE',  ( -2.816281873526473856, 49.33196800326374643, 3.434112377981055619 ) ) ;
#30139 = CARTESIAN_POINT ( 'NONE',  ( -8.527530157486173934, -18.57440218233254470, 4.923371831947302546 ) ) ;
#30140 = EDGE_LOOP ( 'NONE', ( #54614, #27567, #73065, #21767 ) ) ;
#30141 = PLANE ( 'NONE',  #26794 ) ;
#30142 = CARTESIAN_POINT ( 'NONE',  ( 17.75000000000000355, 77.07179676972445748, -6.250000000000000000 ) ) ;
#30143 = DIRECTION ( 'NONE',  ( 0.000000000000000000, -1.000000000000000000, 0.000000000000000000 ) ) ;
#30144 = ORIENTED_EDGE ( 'NONE', *, *, #73617, .F. ) ;
#30145 = CARTESIAN_POINT ( 'NONE',  ( -7.750000000000000000, 0.000000000000000000, 4.000000000000000000 ) ) ;
#30147 = CARTESIAN_POINT ( 'NONE',  ( -4.164238869374099927, 67.01208216824728936, 3.795296366450308767 ) ) ;
#30146 = CARTESIAN_POINT ( 'NONE',  ( 6.204703633549690345, 57.84541550158063927, 14.16423886937410082 ) ) ;
#30149 = CARTESIAN_POINT ( 'NONE',  ( 12.63842701281683034, 62.46726448433410894, 9.846743663894596210 ) ) ;
#30148 = CARTESIAN_POINT ( 'NONE',  ( 10.00000000000000178, 17.25893115100078745, 9.846743663894594434 ) ) ;
#30150 = FACE_OUTER_BOUND ( 'NONE', #15652, .T. ) ;
#30151 = PRESENTATION_LAYER_ASSIGNMENT (  '', '', ( #71635 ) ) ;
#30152 = CARTESIAN_POINT ( 'NONE',  ( 19.80832241502127999, 44.75868815902068576, 6.499999999999992895 ) ) ;
#30153 =( GEOMETRIC_REPRESENTATION_CONTEXT ( 3 ) GLOBAL_UNCERTAINTY_ASSIGNED_CONTEXT ( ( #93212 ) ) GLOBAL_UNIT_ASSIGNED_CONTEXT ( ( #69301, #31281, #92291 ) ) REPRESENTATION_CONTEXT ( 'NONE', 'WORKASPACE' ) );
#30154 = EDGE_CURVE ( 'NONE', #86853, #40259, #37409, .T. ) ;
#30155 = B_SPLINE_CURVE_WITH_KNOTS ( 'NONE', 3,
 ( #38870, #69361, #60366, #76848, #90361, #21899 ),
 .UNSPECIFIED., .F., .F.,
 ( 4, 2, 4 ),
 ( 3.409110551494643978E-05, 0.0004400426677367921553, 0.0008459942299586379385 ),
 .UNSPECIFIED. ) ;
#30156 = CARTESIAN_POINT ( 'NONE',  ( -9.382169495545413795, 24.74863466993042493, 9.382169495545428006 ) ) ;
#30157 = VERTEX_POINT ( 'NONE', #17838 ) ;
#30158 = CARTESIAN_POINT ( 'NONE',  ( 20.36894250292379382, 33.67874883491396076, 10.36894250292379205 ) ) ;
#30159 = VERTEX_POINT ( 'NONE', #32819 ) ;
#30160 = EDGE_CURVE ( 'NONE', #37917, #22102, #55839, .T. ) ;
#30161 = CARTESIAN_POINT ( 'NONE',  ( 2.917880565312948704, 47.63708216824730357, 12.26659068614894643 ) ) ;
#30162 = ORIENTED_EDGE ( 'NONE', *, *, #87136, .T. ) ;
#30163 = CARTESIAN_POINT ( 'NONE',  ( 0.6178305044545838731, 59.74863466993041783, 9.382169495545420901 ) ) ;
#30164 = CARTESIAN_POINT ( 'NONE',  ( 7.084665262690076126, 22.02201867748817321, -10.88017736071110164 ) ) ;
#30165 = CARTESIAN_POINT ( 'NONE',  ( 10.00000000000000000, 54.75893115100078745, -9.846743663894594434 ) ) ;
#30166 = CARTESIAN_POINT ( 'NONE',  ( 12.91533473730993009, 26.60535201082150536, -10.88017736071109987 ) ) ;
#30167 = CARTESIAN_POINT ( 'NONE',  ( 13.34343830728399816, 0.3640475087720989045, 6.852200678592694771 ) ) ;
#30168 = CARTESIAN_POINT ( 'NONE',  ( -8.000000000000000000, 40.99999999999999289, 6.500000000000000888 ) ) ;
#30169 = CARTESIAN_POINT ( 'NONE',  ( 0.1532563361054083140, 56.00893115100078745, 1.131784320476157264E-15 ) ) ;
#30170 = CARTESIAN_POINT ( 'NONE',  ( 19.84674366389459266, 53.71726448433411605, -2.638427012816827677 ) ) ;
#30171 =( GEOMETRIC_REPRESENTATION_CONTEXT ( 3 ) GLOBAL_UNCERTAINTY_ASSIGNED_CONTEXT ( ( #87169 ) ) GLOBAL_UNIT_ASSIGNED_CONTEXT ( ( #814, #67816, #7808 ) ) REPRESENTATION_CONTEXT ( 'NONE', 'WORKASPACE' ) );
#30173 = ORIENTED_EDGE ( 'NONE', *, *, #56016, .T. ) ;
#30172 = DIRECTION ( 'NONE',  ( 0.000000000000000000, 0.000000000000000000, 1.000000000000000000 ) ) ;
#30174 = LINE ( 'NONE', #81698, #65426 ) ;
#30175 = DIRECTION ( 'NONE',  ( 0.000000000000000000, 0.000000000000000000, 1.000000000000000000 ) ) ;
#30176 = CYLINDRICAL_SURFACE ( 'NONE', #30768, 0.5000000000000004441 ) ;
#30177 = ORIENTED_EDGE ( 'NONE', *, *, #85707, .F. ) ;
#30178 = CARTESIAN_POINT ( 'NONE',  ( 19.67858290521088804, 89.00000000000000000, 5.461713021790605360 ) ) ;
#30179 = CARTESIAN_POINT ( 'NONE',  ( 7.361572987183170547, 37.05059781766744464, 9.846743663894590881 ) ) ;
#30180 = LINE ( 'NONE', #69189, #62771 ) ;
#30181 = CARTESIAN_POINT ( 'NONE',  ( 16.40814093676324603, 37.45696800326376064, -11.09922568453594671 ) ) ;
#30182 = DIRECTION ( 'NONE',  ( -0.000000000000000000, -1.000000000000000000, -0.000000000000000000 ) ) ;
#30183 = DIRECTION ( 'NONE',  ( 0.000000000000000000, 0.000000000000000000, -1.000000000000000000 ) ) ;
#30184 = VERTEX_POINT ( 'NONE', #10338 ) ;
#30185 = CIRCLE ( 'NONE', #84533, 0.2500000000000002220 ) ;
#30186 = DIRECTION ( 'NONE',  ( 0.000000000000000000, -1.000000000000000000, 0.000000000000000000 ) ) ;
#30187 = CARTESIAN_POINT ( 'NONE',  ( -0.03447792253739477564, 65.15514106990688958, 6.401564815979731371 ) ) ;
#30188 = CARTESIAN_POINT ( 'NONE',  ( 2.791683348922240793, 41.63393115100078745, 7.208316651077764092 ) ) ;
#30189 = CARTESIAN_POINT ( 'NONE',  ( -2.266590686148945544, 36.38708216824730357, -7.082119434687050408 ) ) ;
#30190 = CARTESIAN_POINT ( 'NONE',  ( 7.361572987183169658, 44.96726448433412315, -9.846743663894592657 ) ) ;
#30191 = CARTESIAN_POINT ( 'NONE',  ( -9.383795276901851778, 14.76930270348881002, 11.62679839395687864 ) ) ;
#30192 = CARTESIAN_POINT ( 'NONE',  ( 2.791683348922237240, 5.383931151000785675, -7.208316651077763204 ) ) ;
#30193 = CARTESIAN_POINT ( 'NONE',  ( -4.164238869374098151, 6.595415501580634832, -3.795296366450310543 ) ) ;
#30194 = CARTESIAN_POINT ( 'NONE',  ( 19.84674366389459621, 48.50893115100078745, 7.409399052514197653E-17 ) ) ;
#30196 = ADVANCED_FACE ( 'NONE', ( #40349 ), #93943, .T. ) ;
#30195 = CARTESIAN_POINT ( 'NONE',  ( 17.96484262340118221, 54.93868534415484106, 7.964842623401181321 ) ) ;
#30197 = CARTESIAN_POINT ( 'NONE',  ( 0.1532563361054083140, 46.00893115100079456, 1.131784320476157264E-15 ) ) ;
#30198 = DIRECTION ( 'NONE',  ( -1.000000000000000000, 0.000000000000000000, 0.000000000000000000 ) ) ;
#30199 = CARTESIAN_POINT ( 'NONE',  ( 17.96484262340118221, 39.93868534415484106, 7.964842623401181321 ) ) ;
#30200 = ORIENTED_EDGE ( 'NONE', *, *, #11057, .T. ) ;
#30201 = CARTESIAN_POINT ( 'NONE',  ( 6.741983435833431848, 0.04922511925147219497, 13.12218577464092917 ) ) ;
#30202 = CARTESIAN_POINT ( 'NONE',  ( -0.8801773607111009756, 33.06368534415484106, 1.068504757029289695E-15 ) ) ;
#30204 = CARTESIAN_POINT ( 'NONE',  ( 20.88017736071110875, 45.77201867748816966, -2.915334737309920765 ) ) ;
#30203 = CARTESIAN_POINT ( 'NONE',  ( 5.076628168052703671, 66.84226448433412315, 8.527530157486179263 ) ) ;
#30205 = CARTESIAN_POINT ( 'NONE',  ( -0.2418659066527647783, 48.09014588040356841, 6.114288769123054301 ) ) ;
#30206 = DIRECTION ( 'NONE',  ( 0.000000000000000000, 0.000000000000000000, 1.000000000000000000 ) ) ;
#30207 = MECHANICAL_DESIGN_GEOMETRIC_PRESENTATION_REPRESENTATION (  '', ( #9454 ), #4689 ) ;
#30209 = FACE_OUTER_BOUND ( 'NONE', #56388, .T. ) ;
#30208 = CARTESIAN_POINT ( 'NONE',  ( 20.88017736071110519, 40.56368534415484106, 2.639326808657452039E-16 ) ) ;
#30210 = CARTESIAN_POINT ( 'NONE',  ( 17.20831665107776587, 12.88393115100078390, 7.208316651077764980 ) ) ;
#30211 = CARTESIAN_POINT ( 'NONE',  ( 19.84674366389459621, 38.50893115100078745, 7.409399052514197653E-17 ) ) ;
#30212 = DIRECTION ( 'NONE',  ( -0.1132032137678971873, 0.000000000000000000, -0.9935718556765885667 ) ) ;
#30213 = CARTESIAN_POINT ( 'NONE',  ( -10.36894250292379205, 26.17874883491397497, -10.36894250292378672 ) ) ;
#30214 = CARTESIAN_POINT ( 'NONE',  ( -2.816281873526473856, -0.8763653300695799508, 9.499525473075851096E-16 ) ) ;
#30215 = CARTESIAN_POINT ( 'NONE',  ( 2.035157376598824452, 3.688685344154837953, 7.964842623401179544 ) ) ;
#30216 = CARTESIAN_POINT ( 'NONE',  ( 20.03447792253739124, 27.65514106990690735, -6.401564815979737588 ) ) ;
#30217 = CARTESIAN_POINT ( 'NONE',  ( -2.266590686148945544, 16.38708216824730357, -7.082119434687050408 ) ) ;
#30218 = CARTESIAN_POINT ( 'NONE',  ( -2.266590686148945544, 47.22041550158063927, 7.082119434687048631 ) ) ;
#30219 = FACE_OUTER_BOUND ( 'NONE', #91059, .T. ) ;
#30220 = ORIENTED_EDGE ( 'NONE', *, *, #96632, .F. ) ;
#30221 = CARTESIAN_POINT ( 'NONE',  ( 5.076628168052704559, 25.17559781766745175, -8.527530157486179263 ) ) ;
#30222 = CARTESIAN_POINT ( 'NONE',  ( 19.42250999205614548, 20.98035201082150891, -5.440088680355545492 ) ) ;
#30223 = CARTESIAN_POINT ( 'NONE',  ( 1.472469842513823179, 46.42559781766745175, 4.923371831947296329 ) ) ;
#30225 = CARTESIAN_POINT ( 'NONE',  ( 14.29730467489529389, 15.00000000000000000, 2.416004766803322656 ) ) ;
#30224 = CARTESIAN_POINT ( 'NONE',  ( 2.917880565312950480, 5.970415501580634832, -12.26659068614894821 ) ) ;
#30226 = UNCERTAINTY_MEASURE_WITH_UNIT (LENGTH_MEASURE( 1.000000000000000082E-05 ), #63751, 'distance_accuracy_value', 'NONE');
#30227 = CARTESIAN_POINT ( 'NONE',  ( 19.84674366389459266, 8.300597817667451750, 2.638427012816836559 ) ) ;
#30228 = CARTESIAN_POINT ( 'NONE',  ( 6.565887622018943937, 33.08196800326374643, -12.81628187352647608 ) ) ;
#30229 = CARTESIAN_POINT ( 'NONE',  ( 10.00000000000000178, 42.25893115100078745, 9.846743663894594434 ) ) ;
#30230 = VERTEX_POINT ( 'NONE', #16428 ) ;
#30231 = CARTESIAN_POINT ( 'NONE',  ( 14.92337183194729988, 9.342264484334119601, -8.527530157486177487 ) ) ;
#30232 = CARTESIAN_POINT ( 'NONE',  ( 11.40632470801588028, -69.21560994247100496, -4.000000000000000000 ) ) ;
#30233 = CARTESIAN_POINT ( 'NONE',  ( -14.29730467490344736, 15.00000000000000000, 2.416004766801328696 ) ) ;
#30234 = CARTESIAN_POINT ( 'NONE',  ( 13.79529636645031943, 55.34541550158062506, -14.16423886937409904 ) ) ;
#30235 = CARTESIAN_POINT ( 'NONE',  ( 20.88017736071110875, 45.77201867748816966, -2.915334737309920765 ) ) ;
#30236 = CARTESIAN_POINT ( 'NONE',  ( -2.266590686148945544, 2.220415501580634388, 7.082119434687048631 ) ) ;
#30237 = SURFACE_STYLE_USAGE ( .BOTH. , #15276 ) ;
#30238 = CARTESIAN_POINT ( 'NONE',  ( 2.791683348922240793, 36.63393115100078035, 7.208316651077764092 ) ) ;
#30239 = CARTESIAN_POINT ( 'NONE',  ( 17.96484262340118221, 9.938685344154837509, 7.964842623401181321 ) ) ;
#30240 = CARTESIAN_POINT ( 'NONE',  ( 1.472469842513823179, 35.59226448433412315, -4.923371831947296329 ) ) ;
#30241 = CARTESIAN_POINT ( 'NONE',  ( -0.1772112516523293435, 6.298283880980280717E-16, -4.084223281690102958 ) ) ;
#30242 = CARTESIAN_POINT ( 'NONE',  ( 2.791683348922237240, 55.38393115100078745, -7.208316651077763204 ) ) ;
#30243 = AXIS2_PLACEMENT_3D ( 'NONE', #43411, #13411, #89408 ) ;
#30244 = CARTESIAN_POINT ( 'NONE',  ( 15.44008868035555793, 46.39701867748817676, -9.422509992056140149 ) ) ;
#30245 = EDGE_CURVE ( 'NONE', #84144, #39231, #76242, .T. ) ;
#30246 = ORIENTED_EDGE ( 'NONE', *, *, #87706, .F. ) ;
#30247 = ORIENTED_EDGE ( 'NONE', *, *, #92595, .F. ) ;
#30248 = CARTESIAN_POINT ( 'NONE',  ( 16.40814093676324603, 52.45696800326375353, -11.09922568453594671 ) ) ;
#30249 = DIRECTION ( 'NONE',  ( -0.08715574274765112983, -0.9961946980917461003, 0.000000000000000000 ) ) ;
#30250 = CARTESIAN_POINT ( 'NONE',  ( 12.63842701281683034, 12.46726448433411782, 9.846743663894596210 ) ) ;
#30251 = CARTESIAN_POINT ( 'NONE',  ( -2.816281873526473856, 54.33196800326376064, 3.434112377981055619 ) ) ;
#30253 = CARTESIAN_POINT ( 'NONE',  ( 18.52753015748618282, 53.92559781766745175, -4.923371831947291888 ) ) ;
#30252 = CARTESIAN_POINT ( 'NONE',  ( 4.559911319644449179, 8.897018677488173211, 9.422509992056141925 ) ) ;
#30255 = EDGE_CURVE ( 'NONE', #42986, #98896, #1650, .T. ) ;
#30254 = CARTESIAN_POINT ( 'NONE',  ( 20.00000000000001066, 87.41133749857198154, 4.971011743019353446 ) ) ;
#30256 = EDGE_CURVE ( 'NONE', #83033, #96742, #33369, .T. ) ;
#30257 =( LENGTH_UNIT ( ) NAMED_UNIT ( * ) SI_UNIT ( .MILLI., .METRE. ) );
#30258 = CARTESIAN_POINT ( 'NONE',  ( -4.164238869374098151, 41.59541550158061796, -3.795296366450310543 ) ) ;
#30259 = CARTESIAN_POINT ( 'NONE',  ( 19.84674366389459266, 58.71726448433411605, -2.638427012816827677 ) ) ;
#30260 = CARTESIAN_POINT ( 'NONE',  ( 6.683977931330435496, -73.15273079452120442, -2.499999999999999556 ) ) ;
#30261 = CARTESIAN_POINT ( 'NONE',  ( 4.559911319644449179, 48.89701867748817676, 9.422509992056141925 ) ) ;
#30262 = CARTESIAN_POINT ( 'NONE',  ( 19.84674366389459266, 3.300597817667451750, 2.638427012816836559 ) ) ;
#30263 = AXIS2_PLACEMENT_3D ( 'NONE', #82846, #68843, #23351 ) ;
#30264 = CARTESIAN_POINT ( 'NONE',  ( -6.715867195167534831, 4.123781235506717606E-16, 12.85095824508322693 ) ) ;
#30265 = ORIENTED_EDGE ( 'NONE', *, *, #23455, .F. ) ;
#30266 = CARTESIAN_POINT ( 'NONE',  ( 13.43411237798106583, 57.66530133659708923, -12.81628187352647252 ) ) ;
#30267 = ORIENTED_EDGE ( 'NONE', *, *, #91561, .T. ) ;
#30268 = EDGE_CURVE ( 'NONE', #34211, #96219, #50485, .T. ) ;
#30269 = CARTESIAN_POINT ( 'NONE',  ( 12.63842701281683922, 4.550597817667451750, -9.846743663894590881 ) ) ;
#30270 = ORIENTED_EDGE ( 'NONE', *, *, #84933, .T. ) ;
#30271 = CARTESIAN_POINT ( 'NONE',  ( 6.204703633549690345, 15.76208216824730179, -14.16423886937410259 ) ) ;
#30272 = CARTESIAN_POINT ( 'NONE',  ( 2.791683348922240793, 26.63393115100078745, 7.208316651077764092 ) ) ;
#30273 = CARTESIAN_POINT ( 'NONE',  ( -0.8801773607110991993, 27.85535201082150181, -2.915334737309923874 ) ) ;
#30274 = VECTOR ( 'NONE', #28871, 1000.000000000000000 ) ;
#30275 = CARTESIAN_POINT ( 'NONE',  ( 4.469999999999999751, 10.00000000000000000, 3.750000000000000000 ) ) ;
#30276 = EDGE_LOOP ( 'NONE', ( #12174, #65186 ) ) ;
#30277 = CARTESIAN_POINT ( 'NONE',  ( -0.8801773607111009756, 23.06368534415484106, 1.068504757029289695E-15 ) ) ;
#30278 = ORIENTED_EDGE ( 'NONE', *, *, #94153, .F. ) ;
#30279 = DIRECTION ( 'NONE',  ( 0.000000000000000000, -1.000000000000000000, 0.000000000000000000 ) ) ;
#30280 = ORIENTED_EDGE ( 'NONE', *, *, #21359, .F. ) ;
#30281 = ADVANCED_FACE ( 'NONE', ( #24921 ), #91924, .F. ) ;
#30282 = VERTEX_POINT ( 'NONE', #93396 ) ;
#30283 = CARTESIAN_POINT ( 'NONE',  ( 13.43411237798105340, 15.58196800326374998, 12.81628187352647963 ) ) ;
#30284 = CARTESIAN_POINT ( 'NONE',  ( 0.2751277870542912507, 20.30223176428831167, 6.499999999999992006 ) ) ;
#30285 = CARTESIAN_POINT ( 'NONE',  ( 17.20831665107776587, 9.133931151000787452, -7.208316651077762316 ) ) ;
#30286 = FACE_OUTER_BOUND ( 'NONE', #89798, .T. ) ;
#30287 = CARTESIAN_POINT ( 'NONE',  ( 19.84674366389459621, 13.50893115100078568, 7.409399052514197653E-17 ) ) ;
#30288 = CARTESIAN_POINT ( 'NONE',  ( 2.035157376598822676, 32.43868534415483396, -7.964842623401177768 ) ) ;
#30289 = ORIENTED_EDGE ( 'NONE', *, *, #71498, .T. ) ;
#30290 = ORIENTED_EDGE ( 'NONE', *, *, #36622, .F. ) ;
#30291 = B_SPLINE_CURVE_WITH_KNOTS ( 'NONE', 3,
 ( #77418, #14984, #60943, #69942, #84937, #45455 ),
 .UNSPECIFIED., .F., .F.,
 ( 4, 2, 4 ),
 ( 0.0002800039672440423157, 0.0006862092354666148638, 0.001092414503689187249 ),
 .UNSPECIFIED. ) ;
#30292 = FACE_OUTER_BOUND ( 'NONE', #39680, .T. ) ;
#30293 = CARTESIAN_POINT ( 'NONE',  ( 7.084665262690076126, 42.02201867748816966, -10.88017736071110164 ) ) ;
#30294 = CARTESIAN_POINT ( 'NONE',  ( 21.09922568453594849, 56.20696800326375353, 6.408140936763242479 ) ) ;
#30295 = CARTESIAN_POINT ( 'NONE',  ( 4.559911319644449179, 63.89701867748817676, 9.422509992056141925 ) ) ;
#30296 = CARTESIAN_POINT ( 'NONE',  ( 6.565887622018943937, 3.081968003263753531, -12.81628187352647608 ) ) ;
#30297 = LINE ( 'NONE', #83316, #70643 ) ;
#30298 = AXIS2_PLACEMENT_3D ( 'NONE', #39656, #78628, #10139 ) ;
#30299 = CARTESIAN_POINT ( 'NONE',  ( 18.52753015748618282, 13.92559781766745175, -4.923371831947291888 ) ) ;
#30300 = CARTESIAN_POINT ( 'NONE',  ( 22.81628187352647785, 56.62363466993042493, 6.195893100308588602E-16 ) ) ;
#30301 = DIRECTION ( 'NONE',  ( -4.884981308350689409E-14, 0.000000000000000000, 1.000000000000000000 ) ) ;
#30302 = CARTESIAN_POINT ( 'NONE',  ( 18.52753015748618282, 8.925597817667451750, -4.923371831947291888 ) ) ;
#30303 = CARTESIAN_POINT ( 'NONE',  ( -2.816281873526473856, 14.33196800326375531, 3.434112377981055619 ) ) ;
#30305 = CARTESIAN_POINT ( 'NONE',  ( 19.84674366389459621, 63.50893115100078745, 7.409399052514197653E-17 ) ) ;
#30304 = DIRECTION ( 'NONE',  ( 0.9099612708765483227, 0.000000000000000000, -0.4146932426562279228 ) ) ;
#30306 = CARTESIAN_POINT ( 'NONE',  ( 20.88017736071110519, 30.56368534415484106, 2.639326808657452039E-16 ) ) ;
#30307 = CARTESIAN_POINT ( 'NONE',  ( 19.84674366389459266, 58.30059781766745886, 2.638427012816836559 ) ) ;
#30308 = DIRECTION ( 'NONE',  ( -0.000000000000000000, 0.000000000000000000, 1.000000000000000000 ) ) ;
#30309 = AXIS2_PLACEMENT_3D ( 'NONE', #33463, #52660, #90654 ) ;
#30310 = CARTESIAN_POINT ( 'NONE',  ( 10.00000000000000000, 19.75893115100078390, -9.846743663894594434 ) ) ;
#30311 = CARTESIAN_POINT ( 'NONE',  ( 17.20831665107776587, 4.133931151000785675, -7.208316651077762316 ) ) ;
#30312 = EDGE_CURVE ( 'NONE', #76776, #33114, #33823, .T. ) ;
#30314 = ORIENTED_EDGE ( 'NONE', *, *, #11238, .T. ) ;
#30313 = CARTESIAN_POINT ( 'NONE',  ( 0.6178305044545838731, 4.748634669930420493, 9.382169495545420901 ) ) ;
#30315 = CARTESIAN_POINT ( 'NONE',  ( 10.00000000000000000, 6.813685344154838397, -10.88017736071110342 ) ) ;
#30316 = CARTESIAN_POINT ( 'NONE',  ( -4.873787042390880231, -0.03417435944610275333, 13.39061984619915791 ) ) ;
#30317 = CARTESIAN_POINT ( 'NONE',  ( 5.113979357103554335, -17.50950876244569443, -2.750000000000804246 ) ) ;
#30318 = CARTESIAN_POINT ( 'NONE',  ( 10.00000000000000178, 9.313685344154839285, 10.88017736071110342 ) ) ;
#30319 = CARTESIAN_POINT ( 'NONE',  ( 1.472469842513823179, 50.59226448433411605, -4.923371831947296329 ) ) ;
#30320 = ORIENTED_EDGE ( 'NONE', *, *, #79405, .F. ) ;
#30321 = CARTESIAN_POINT ( 'NONE',  ( 19.05866839779140776, 65.95508385108959715, -6.499999999999956479 ) ) ;
#30322 = CARTESIAN_POINT ( 'NONE',  ( -4.164238869374098151, 66.59541550158060375, -3.795296366450310543 ) ) ;
#30323 = CARTESIAN_POINT ( 'NONE',  ( 0.8952175423694470613, 13.52576239577081019, 5.990408912944253927 ) ) ;
#30324 = CARTESIAN_POINT ( 'NONE',  ( 10.00000000000000178, 29.31368534415483751, 10.88017736071110342 ) ) ;
#30325 = CARTESIAN_POINT ( 'NONE',  ( 17.08211943468705840, 50.13708216824730357, -12.26659068614894466 ) ) ;
#30327 = DIRECTION ( 'NONE',  ( 0.000000000000000000, 1.000000000000000000, 0.000000000000000000 ) ) ;
#30326 = CARTESIAN_POINT ( 'NONE',  ( 0.5774900079438590739, 2.647018677488171434, -5.440088680355550821 ) ) ;
#30328 = CARTESIAN_POINT ( 'NONE',  ( 5.076628168052704559, 5.175597817667451750, -8.527530157486179263 ) ) ;
#30329 = AXIS2_PLACEMENT_3D ( 'NONE', #35246, #72747, #28245 ) ;
#30330 = CARTESIAN_POINT ( 'NONE',  ( 0.1532563361054100626, 25.80059781766744820, -2.638427012816831230 ) ) ;
#30331 = CARTESIAN_POINT ( 'NONE',  ( -2.816281873526471635, 13.91530133659708746, -3.434112377981056508 ) ) ;
#30332 = CARTESIAN_POINT ( 'NONE',  ( 19.72487221294570858, 26.86607318730131055, 6.500000000000000888 ) ) ;
#30333 =( LENGTH_UNIT ( ) NAMED_UNIT ( * ) SI_UNIT ( .MILLI., .METRE. ) );
#30334 = CARTESIAN_POINT ( 'NONE',  ( -4.164238869374099039, 11.80374883491396965, 8.674139862899312516E-16 ) ) ;
#30335 = CARTESIAN_POINT ( 'NONE',  ( 5.076628168052704559, 20.17559781766745175, -8.527530157486179263 ) ) ;
#30336 = DIRECTION ( 'NONE',  ( 1.000000000000000000, 0.000000000000000000, 0.000000000000000000 ) ) ;
#30337 = ORIENTED_EDGE ( 'NONE', *, *, #50212, .F. ) ;
#30338 = CARTESIAN_POINT ( 'NONE',  ( 22.26659068614894466, 58.88708216824729647, 7.082119434687054849 ) ) ;
#30339 = CARTESIAN_POINT ( 'NONE',  ( 17.20831665107776587, 9.133931151000787452, -7.208316651077762316 ) ) ;
#30341 = FACE_OUTER_BOUND ( 'NONE', #22319, .T. ) ;
#30340 = LINE ( 'NONE', #92820, #61069 ) ;
#30342 = CARTESIAN_POINT ( 'NONE',  ( 4.559911319644449179, 33.89701867748817676, 9.422509992056141925 ) ) ;
#30343 = CARTESIAN_POINT ( 'NONE',  ( 22.81628187352648496, 51.83196800326376064, -3.434112377981050290 ) ) ;
#30344 = CARTESIAN_POINT ( 'NONE',  ( 20.88017736071110164, 10.35535201082150714, 2.915334737309930979 ) ) ;
#30345 = CARTESIAN_POINT ( 'NONE',  ( 10.00000000000000000, 37.87363466993041783, -12.81628187352647608 ) ) ;
#30346 = CARTESIAN_POINT ( 'NONE',  ( -2.816281873526471635, 3.915301336597087456, -3.434112377981056508 ) ) ;
#30347 = CARTESIAN_POINT ( 'NONE',  ( 19.84674366389459621, 3.508931151000785231, 7.409399052514197653E-17 ) ) ;
#30348 = ORIENTED_EDGE ( 'NONE', *, *, #25272, .F. ) ;
#30349 = DIRECTION ( 'NONE',  ( 1.000000000000000000, 0.000000000000000000, 0.000000000000000000 ) ) ;
#30350 = CARTESIAN_POINT ( 'NONE',  ( -7.749999999999999112, -0.02153525003578424246, -4.000000000000000000 ) ) ;
#30351 = CARTESIAN_POINT ( 'NONE',  ( 2.917880565312950480, 40.97041550158063217, -12.26659068614894821 ) ) ;
#30352 = CARTESIAN_POINT ( 'NONE',  ( 10.00000000000000000, 15.55374883491396787, -14.16423886937410082 ) ) ;
#30353 = CARTESIAN_POINT ( 'NONE',  ( 7.084665262690076126, 9.105352010821503583, 10.88017736071109987 ) ) ;
#30354 = CARTESIAN_POINT ( 'NONE',  ( 20.88017736071110164, 30.35535201082151247, 2.915334737309930979 ) ) ;
#30355 = DIRECTION ( 'NONE',  ( -0.000000000000000000, -1.000000000000000000, -0.000000000000000000 ) ) ;
#30356 = CARTESIAN_POINT ( 'NONE',  ( 17.96484262340118221, 54.93868534415484106, 7.964842623401181321 ) ) ;
#30357 = CARTESIAN_POINT ( 'NONE',  ( 12.91533473730993009, 66.60535201082150536, -10.88017736071109987 ) ) ;
#30358 = CARTESIAN_POINT ( 'NONE',  ( -1.099225684535947600, 23.70696800326375708, -6.408140936763238038 ) ) ;
#30359 = PLANE ( 'NONE',  #9143 ) ;
#30360 = DIRECTION ( 'NONE',  ( 1.000000000000000000, -0.000000000000000000, 0.000000000000000000 ) ) ;
#30361 = CARTESIAN_POINT ( 'NONE',  ( 2.791683348922237240, 35.38393115100079456, -7.208316651077763204 ) ) ;
#30362 = EDGE_CURVE ( 'NONE', #23295, #20205, #36264, .T. ) ;
#30363 = CIRCLE ( 'NONE', #55937, 0.2500000000000002220 ) ;
#30364 = ADVANCED_FACE ( 'NONE', ( #86399 ), #13942, .T. ) ;
#30365 = CARTESIAN_POINT ( 'NONE',  ( -2.816281873526473856, 24.33196800326375353, 3.434112377981055619 ) ) ;
#30366 = CARTESIAN_POINT ( 'NONE',  ( 0.1532563361054100626, 5.800597817667452638, -2.638427012816831230 ) ) ;
#30368 = EDGE_CURVE ( 'NONE', #89066, #91549, #77398, .T. ) ;
#30367 = CARTESIAN_POINT ( 'NONE',  ( 17.96484262340118221, 4.938685344154837509, 7.964842623401181321 ) ) ;
#30369 = ADVANCED_FACE ( 'NONE', ( #39912 ), #31542, .T. ) ;
#30370 = CARTESIAN_POINT ( 'NONE',  ( 18.52753015748617571, 43.09226448433412315, 4.923371831947298993 ) ) ;
#30371 = CARTESIAN_POINT ( 'NONE',  ( 13.43411237798105340, 60.58196800326376064, 12.81628187352647963 ) ) ;
#30372 = CARTESIAN_POINT ( 'NONE',  ( 17.20831665107776587, 24.13393115100078035, -7.208316651077762316 ) ) ;
#30373 = CARTESIAN_POINT ( 'NONE',  ( -4.164238869374099927, 7.012082168247302683, 3.795296366450308767 ) ) ;
#30375 = DIRECTION ( 'NONE',  ( 1.000000000000000000, 2.081668171172167567E-14, 0.000000000000000000 ) ) ;
#30374 = AXIS2_PLACEMENT_3D ( 'NONE', #12405, #27896, #64412 ) ;
#30376 = CARTESIAN_POINT ( 'NONE',  ( -0.8801773607111009756, 28.06368534415484106, 1.068504757029289695E-15 ) ) ;
#30378 = CARTESIAN_POINT ( 'NONE',  ( -2.266590686148945544, 46.38708216824730357, -7.082119434687050408 ) ) ;
#30377 = CARTESIAN_POINT ( 'NONE',  ( 0.5774900079438590739, 17.64701867748817321, -5.440088680355550821 ) ) ;
#30379 = CIRCLE ( 'NONE', #9625, 0.09999999999999939493 ) ;
#30380 = CARTESIAN_POINT ( 'NONE',  ( 7.084665262690076126, 34.10535201082151247, 10.88017736071109987 ) ) ;
#30381 = CARTESIAN_POINT ( 'NONE',  ( 17.96484262340118221, 11.18868534415484106, -7.964842623401177768 ) ) ;
#30382 = VERTEX_POINT ( 'NONE', #9913 ) ;
#30383 = AXIS2_PLACEMENT_3D ( 'NONE', #1799, #63737, #15807 ) ;
#30384 = CARTESIAN_POINT ( 'NONE',  ( 2.035157376598822676, 32.43868534415483396, -7.964842623401177768 ) ) ;
#30385 = CARTESIAN_POINT ( 'NONE',  ( 6.565887622018943937, 50.16530133659708213, 12.81628187352647430 ) ) ;
#30386 = CARTESIAN_POINT ( 'NONE',  ( 0.5774900079438607392, 48.48035201082150536, 5.440088680355550821 ) ) ;
#30388 = CARTESIAN_POINT ( 'NONE',  ( 7.084665262690076126, 49.10535201082149825, 10.88017736071109987 ) ) ;
#30387 = FACE_OUTER_BOUND ( 'NONE', #32213, .T. ) ;
#30389 = EDGE_LOOP ( 'NONE', ( #69158, #97829, #96114, #81800, #5568, #78316 ) ) ;
#30390 = CARTESIAN_POINT ( 'NONE',  ( 2.035157376598822676, 52.43868534415483396, -7.964842623401177768 ) ) ;
#30391 = SURFACE_STYLE_USAGE ( .BOTH. , #52899 ) ;
#30392 = CARTESIAN_POINT ( 'NONE',  ( -3.750000000000000000, 10.25000000000000000, -2.500000000000000000 ) ) ;
#30393 = CARTESIAN_POINT ( 'NONE',  ( 2.917880565312950480, 45.97041550158063927, -12.26659068614894821 ) ) ;
#30394 = CARTESIAN_POINT ( 'NONE',  ( 1.472469842513823179, 1.425597817667451528, 4.923371831947296329 ) ) ;
#30395 = LINE ( 'NONE', #45402, #29072 ) ;
#30396 = CARTESIAN_POINT ( 'NONE',  ( 9.997910040112534702, 15.00000000000000000, 10.50199004140724490 ) ) ;
#30397 = CARTESIAN_POINT ( 'NONE',  ( 5.076628168052703671, 61.84226448433412315, 8.527530157486179263 ) ) ;
#30398 = CARTESIAN_POINT ( 'NONE',  ( -8.000000000000000000, 80.99999999999994316, -1.249999999999987121 ) ) ;
#30399 = CARTESIAN_POINT ( 'NONE',  ( 5.076628168052704559, 35.17559781766745175, -8.527530157486179263 ) ) ;
#30400 = EDGE_LOOP ( 'NONE', ( #51595, #23096, #4728, #84177 ) ) ;
#30401 = EDGE_CURVE ( 'NONE', #22141, #2391, #49110, .T. ) ;
#30402 = CARTESIAN_POINT ( 'NONE',  ( 7.361572987183169658, 29.96726448433411960, -9.846743663894592657 ) ) ;
#30403 = CARTESIAN_POINT ( 'NONE',  ( -6.408140936763232709, -10.04303199673624292, 11.09922568453595026 ) ) ;
#30404 = VECTOR ( 'NONE', #44620, 1000.000000000000227 ) ;
#30405 = CARTESIAN_POINT ( 'NONE',  ( 7.084665262690076126, 22.02201867748817321, -10.88017736071110164 ) ) ;
#30406 = CARTESIAN_POINT ( 'NONE',  ( 0.1532563361054100626, 35.80059781766745175, -2.638427012816831230 ) ) ;
#30407 = CARTESIAN_POINT ( 'NONE',  ( 22.81628187352647785, 26.62363466993042138, 6.195893100308588602E-16 ) ) ;
#30409 = CARTESIAN_POINT ( 'NONE',  ( 12.91533473730992121, 54.52201867748816255, 10.88017736071110164 ) ) ;
#30408 = DIRECTION ( 'NONE',  ( 0.000000000000000000, 1.000000000000000000, 0.000000000000000000 ) ) ;
#30411 = CARTESIAN_POINT ( 'NONE',  ( -0.8801773607111008646, 3.272018677488171434, 2.915334737309923430 ) ) ;
#30410 = CARTESIAN_POINT ( 'NONE',  ( 4.559911319644449179, 42.23035201082151247, -9.422509992056141925 ) ) ;
#30412 = CARTESIAN_POINT ( 'NONE',  ( 22.26659068614894466, 63.88708216824730357, 7.082119434687054849 ) ) ;
#30413 = EDGE_CURVE ( 'NONE', #5496, #32549, #49367, .T. ) ;
#30414 = CARTESIAN_POINT ( 'NONE',  ( 16.40814093676324603, 27.45696800326375708, -11.09922568453594671 ) ) ;
#30415 = DIRECTION ( 'NONE',  ( -0.000000000000000000, -1.000000000000000000, -0.000000000000000000 ) ) ;
#30416 = ORIENTED_EDGE ( 'NONE', *, *, #20390, .F. ) ;
#30417 = CARTESIAN_POINT ( 'NONE',  ( 22.81628187352647785, 21.41530133659708923, 3.434112377981063169 ) ) ;
#30418 = CARTESIAN_POINT ( 'NONE',  ( 7.084665262690076126, 19.10535201082150181, 10.88017736071109987 ) ) ;
#30419 = CARTESIAN_POINT ( 'NONE',  ( -0.8801773607111009756, 63.06368534415484106, 1.068504757029289695E-15 ) ) ;
#30420 = SURFACE_STYLE_USAGE ( .BOTH. , #13456 ) ;
#30421 = ORIENTED_EDGE ( 'NONE', *, *, #33005, .F. ) ;
#30422 = CARTESIAN_POINT ( 'NONE',  ( 7.084665262690076126, 52.02201867748816255, -10.88017736071110164 ) ) ;
#30423 = CARTESIAN_POINT ( 'NONE',  ( 5.076628168052704559, 40.17559781766745175, -8.527530157486179263 ) ) ;
#30424 = CARTESIAN_POINT ( 'NONE',  ( 1.472469842513823179, 30.59226448433411960, -4.923371831947296329 ) ) ;
#30425 = CARTESIAN_POINT ( 'NONE',  ( 12.63842701281683922, 14.55059781766744997, -9.846743663894590881 ) ) ;
#30427 = CARTESIAN_POINT ( 'NONE',  ( 19.38216949554541202, 40.99863466993042493, 9.382169495545424454 ) ) ;
#30426 = CARTESIAN_POINT ( 'NONE',  ( -9.159723438033276821, -0.03417435944610275333, 10.91613331444536250 ) ) ;
#30429 = FACE_OUTER_BOUND ( 'NONE', #90501, .T. ) ;
#30428 = CARTESIAN_POINT ( 'NONE',  ( 5.076628168052704559, 20.17559781766745175, -8.527530157486179263 ) ) ;
#30430 = DIRECTION ( 'NONE',  ( -0.9969173337331285190, 0.000000000000000000, 0.07845909572783862918 ) ) ;
#30431 = CARTESIAN_POINT ( 'NONE',  ( 7.361572987183169658, 34.96726448433411605, -9.846743663894592657 ) ) ;
#30432 = AXIS2_PLACEMENT_3D ( 'NONE', #4553, #96042, #57532 ) ;
#30433 = CARTESIAN_POINT ( 'NONE',  ( 20.24186590665277663, 16.76028685723174405, 6.114288769123035649 ) ) ;
#30434 = CARTESIAN_POINT ( 'NONE',  ( 3.591859063236761518, 9.956968003263753531, 11.09922568453594849 ) ) ;
#30435 = CARTESIAN_POINT ( 'NONE',  ( 12.91533473730993009, 46.60535201082150536, -10.88017736071109987 ) ) ;
#30436 = CARTESIAN_POINT ( 'NONE',  ( 17.08211943468705840, 30.13708216824730357, -12.26659068614894466 ) ) ;
#30437 = UNCERTAINTY_MEASURE_WITH_UNIT (LENGTH_MEASURE( 1.000000000000000082E-05 ), #9479, 'distance_accuracy_value', 'NONE');
#30438 = CARTESIAN_POINT ( 'NONE',  ( -14.89999999999999680, 98.49999999999998579, -8.525133428036873795 ) ) ;
#30439 = CARTESIAN_POINT ( 'NONE',  ( -4.164238869374099039, 26.80374883491397142, 8.674139862899312516E-16 ) ) ;
#30440 = VECTOR ( 'NONE', #37026, 1000.000000000000000 ) ;
#30441 = CARTESIAN_POINT ( 'NONE',  ( 17.08211943468705130, 63.47041550158063927, 12.26659068614894998 ) ) ;
#30442 = CARTESIAN_POINT ( 'NONE',  ( -0.3689425029237881626, 7.428748834913967869, 10.36894250292379027 ) ) ;
#30443 = CARTESIAN_POINT ( 'NONE',  ( 24.16423886937410614, 24.30374883491396787, 8.672049930838204340E-16 ) ) ;
#30444 = CARTESIAN_POINT ( 'NONE',  ( 0.5774900079438607392, 53.48035201082151247, 5.440088680355550821 ) ) ;
#30445 = CARTESIAN_POINT ( 'NONE',  ( -8.235571585149871865, 9.493033628982651351, -8.235571585149866536 ) ) ;
#30448 = AXIS2_PLACEMENT_3D ( 'NONE', #92153, #61152, #196 ) ;
#30447 = CARTESIAN_POINT ( 'NONE',  ( 17.20831665107776587, 42.88393115100077324, 7.208316651077764980 ) ) ;
#30446 = CARTESIAN_POINT ( 'NONE',  ( 18.18329248733322601, 62.60290668512021028, 6.499999999999960920 ) ) ;
#30449 = CARTESIAN_POINT ( 'NONE',  ( 4.559911319644449179, 23.89701867748817321, 9.422509992056141925 ) ) ;
#30450 = LINE ( 'NONE', #23481, #48935 ) ;
#30451 = CARTESIAN_POINT ( 'NONE',  ( 17.20831665107776587, 57.88393115100078745, 7.208316651077764980 ) ) ;
#30452 = EDGE_CURVE ( 'NONE', #39764, #20515, #44319, .T. ) ;
#30453 = CARTESIAN_POINT ( 'NONE',  ( 0.2751277870542967463, 69.50000000000000000, 6.500000000000000888 ) ) ;
#30454 = CARTESIAN_POINT ( 'NONE',  ( 1.472469842513823179, 31.42559781766745530, 4.923371831947296329 ) ) ;
#30455 = CARTESIAN_POINT ( 'NONE',  ( 21.09922568453595559, 52.04030133659708923, -6.408140936763230044 ) ) ;
#30456 = CARTESIAN_POINT ( 'NONE',  ( 10.36894250292379027, -1.321251165086033907, 10.36894250292378672 ) ) ;
#30457 = CARTESIAN_POINT ( 'NONE',  ( 14.92337183194729633, 42.67559781766745886, 8.527530157486181039 ) ) ;
#30458 = CARTESIAN_POINT ( 'NONE',  ( 7.361572987183170547, 52.05059781766745175, 9.846743663894590881 ) ) ;
#30459 = CARTESIAN_POINT ( 'NONE',  ( 2.917880565312950480, 35.97041550158063217, -12.26659068614894821 ) ) ;
#30460 = ORIENTED_EDGE ( 'NONE', *, *, #53184, .T. ) ;
#30461 = CARTESIAN_POINT ( 'NONE',  ( 10.00000000000000000, 5.553748834913967869, -14.16423886937410082 ) ) ;
#30462 = CARTESIAN_POINT ( 'NONE',  ( -0.8801773607111009756, 68.06368534415484817, 1.068504757029289695E-15 ) ) ;
#30463 = SURFACE_STYLE_USAGE ( .BOTH. , #24962 ) ;
#30464 = CARTESIAN_POINT ( 'NONE',  ( -4.164238869374098151, 56.59541550158063927, -3.795296366450310543 ) ) ;
#30465 = CARTESIAN_POINT ( 'NONE',  ( 19.38216949554541557, 12.24863466993041961, -9.382169495545420901 ) ) ;
#30466 = PLANE ( 'NONE',  #27341 ) ;
#30467 = CARTESIAN_POINT ( 'NONE',  ( 2.035157376598822676, 52.43868534415483396, -7.964842623401177768 ) ) ;
#30468 = CARTESIAN_POINT ( 'NONE',  ( -1.926860441876562247, 27.45379003517447813, -3.195792623639530650 ) ) ;
#30469 = CARTESIAN_POINT ( 'NONE',  ( -46.78604402846880106, 100.7423487049318140, -9.213902555517821114 ) ) ;
#30470 = CARTESIAN_POINT ( 'NONE',  ( -0.3689425029237881626, 67.42874883491396076, 10.36894250292379027 ) ) ;
#30471 = CARTESIAN_POINT ( 'NONE',  ( -7.964842623401179544, 32.43868534415485527, -7.964842623401174215 ) ) ;
#30472 = CARTESIAN_POINT ( 'NONE',  ( 19.42250999205614548, 15.98035201082150714, -5.440088680355545492 ) ) ;
#30473 = CARTESIAN_POINT ( 'NONE',  ( 20.88017736071110164, 30.35535201082151247, 2.915334737309930979 ) ) ;
#30474 = CARTESIAN_POINT ( 'NONE',  ( 5.076628168052704559, 55.17559781766745175, -8.527530157486179263 ) ) ;
#30475 = CARTESIAN_POINT ( 'NONE',  ( 5.076628168052704559, 60.17559781766745175, -8.527530157486179263 ) ) ;
#30476 = CARTESIAN_POINT ( 'NONE',  ( 0.6178305044545838731, 49.74863466993041072, 9.382169495545420901 ) ) ;
#30477 = CARTESIAN_POINT ( 'NONE',  ( 1.472469842513823179, 0.5922644843341181575, -4.923371831947296329 ) ) ;
#30478 = ORIENTED_EDGE ( 'NONE', *, *, #32742, .T. ) ;
#30479 = AXIS2_PLACEMENT_3D ( 'NONE', #83606, #15614, #46578 ) ;
#30480 = CARTESIAN_POINT ( 'NONE',  ( 20.88017736071110164, 15.35535201082150358, 2.915334737309930979 ) ) ;
#30481 = CARTESIAN_POINT ( 'NONE',  ( 10.00000000000000000, 12.87363466993042138, -12.81628187352647608 ) ) ;
#30482 = DIRECTION ( 'NONE',  ( 0.000000000000000000, 0.000000000000000000, 1.000000000000000000 ) ) ;
#30483 = EDGE_CURVE ( 'NONE', #65662, #48512, #36333, .T. ) ;
#30484 = STYLED_ITEM ( 'NONE', ( #40053 ), #79132 ) ;
#30485 = CARTESIAN_POINT ( 'NONE',  ( 14.92337183194729988, 44.34226448433412315, -8.527530157486177487 ) ) ;
#30486 = CARTESIAN_POINT ( 'NONE',  ( 4.559911319644449179, 32.23035201082150536, -9.422509992056141925 ) ) ;
#30487 = ADVANCED_FACE ( 'NONE', ( #64845 ), #26371, .F. ) ;
#30488 = CARTESIAN_POINT ( 'NONE',  ( 3.591859063236761518, 19.95696800326375353, 11.09922568453594849 ) ) ;
#30490 = DIRECTION ( 'NONE',  ( -0.000000000000000000, -0.000000000000000000, -1.000000000000000000 ) ) ;
#30489 = CARTESIAN_POINT ( 'NONE',  ( 20.88017736071110164, 45.35535201082149115, 2.915334737309930979 ) ) ;
#30491 = LINE ( 'NONE', #22034, #1857 ) ;
#30492 = CARTESIAN_POINT ( 'NONE',  ( 22.81628187352647785, 46.41530133659708213, 3.434112377981063169 ) ) ;
#30493 = ORIENTED_EDGE ( 'NONE', *, *, #26174, .T. ) ;
#30494 = CARTESIAN_POINT ( 'NONE',  ( 0.1532563361054083140, 66.00893115100079456, 1.131784320476157264E-15 ) ) ;
#30495 = CARTESIAN_POINT ( 'NONE',  ( 0.5774900079438607392, 48.48035201082150536, 5.440088680355550821 ) ) ;
#30496 = CARTESIAN_POINT ( 'NONE',  ( -1.099225684535947600, 34.54030133659708923, 6.408140936763237150 ) ) ;
#30497 = CARTESIAN_POINT ( 'NONE',  ( 7.361572987183169658, 9.967264484334119601, -9.846743663894592657 ) ) ;
#30498 = CARTESIAN_POINT ( 'NONE',  ( 22.26659068614894466, 43.88708216824729647, 7.082119434687054849 ) ) ;
#30499 = DIRECTION ( 'NONE',  ( -1.000000000000000000, 0.000000000000000000, 0.000000000000000000 ) ) ;
#30500 = CARTESIAN_POINT ( 'NONE',  ( 2.791683348922240793, 11.63393115100078568, 7.208316651077764092 ) ) ;
#30501 = CARTESIAN_POINT ( 'NONE',  ( 10.00000000000000178, 7.258931151000785675, 9.846743663894594434 ) ) ;
#30502 = CARTESIAN_POINT ( 'NONE',  ( -13.82671409943298357, 15.00000000000000000, 3.447387012295131115 ) ) ;
#30503 = CARTESIAN_POINT ( 'NONE',  ( 13.79529636645030344, 38.26208216824729647, 14.16423886937410614 ) ) ;
#30504 = DIRECTION ( 'NONE',  ( -0.000000000000000000, -1.000000000000000000, -0.000000000000000000 ) ) ;
#30505 = CARTESIAN_POINT ( 'NONE',  ( 0.5774900079438607392, 13.48035201082150358, 5.440088680355550821 ) ) ;
#30506 = CARTESIAN_POINT ( 'NONE',  ( 0.000000000000000000, 0.5000000000000004441, 0.000000000000000000 ) ) ;
#30507 = AXIS2_PLACEMENT_3D ( 'NONE', #84603, #14136, #77088 ) ;
#30508 = EDGE_LOOP ( 'NONE', ( #50956, #7420, #12297, #80227 ) ) ;
#30509 = ORIENTED_EDGE ( 'NONE', *, *, #80043, .T. ) ;
#30510 = CARTESIAN_POINT ( 'NONE',  ( 20.88017736071110164, 10.35535201082150714, 2.915334737309930979 ) ) ;
#30511 = CARTESIAN_POINT ( 'NONE',  ( -4.164238869374098151, 61.59541550158063217, -3.795296366450310543 ) ) ;
#30512 = CARTESIAN_POINT ( 'NONE',  ( 17.20831665107776587, 37.88393115100078745, 7.208316651077764980 ) ) ;
#30513 = CARTESIAN_POINT ( 'NONE',  ( 22.81628187352647785, 36.62363466993041783, 6.195893100308588602E-16 ) ) ;
#30515 = CARTESIAN_POINT ( 'NONE',  ( -4.164238869374099039, 1.803748834913967647, 8.674139862899312516E-16 ) ) ;
#30514 = DIRECTION ( 'NONE',  ( 0.000000000000000000, 1.000000000000000000, 0.000000000000000000 ) ) ;
#30516 = CARTESIAN_POINT ( 'NONE',  ( 2.035157376598824452, 23.68868534415484461, 7.964842623401179544 ) ) ;
#30517 = CARTESIAN_POINT ( 'NONE',  ( 2.035157376598824452, 8.688685344154839285, 7.964842623401179544 ) ) ;
#30518 = CARTESIAN_POINT ( 'NONE',  ( 19.84674366389459621, 43.50893115100078745, 7.409399052514197653E-17 ) ) ;
#30519 = DIRECTION ( 'NONE',  ( -0.000000000000000000, -0.000000000000000000, -1.000000000000000000 ) ) ;
#30520 = CARTESIAN_POINT ( 'NONE',  ( 1.472469842513823179, 25.59226448433412315, -4.923371831947296329 ) ) ;
#30521 = TOROIDAL_SURFACE ( 'NONE', #6549, 14.49999999999999822, 0.5000000000000000000 ) ;
#30522 = ADVANCED_FACE ( 'NONE', ( #49858 ), #66425, .T. ) ;
#30523 = CARTESIAN_POINT ( 'NONE',  ( -4.250000000000000000, 36.75000000000000000, 4.000000000000000000 ) ) ;
#30524 = CARTESIAN_POINT ( 'NONE',  ( 7.208316651077762316, 19.13393115100078745, -7.208316651077764980 ) ) ;
#30525 = VERTEX_POINT ( 'NONE', #96958 ) ;
#30526 = CARTESIAN_POINT ( 'NONE',  ( -5.171435456984247558, 0.000000000000000000, 1.730338099013940978 ) ) ;
#30527 = ORIENTED_EDGE ( 'NONE', *, *, #11281, .T. ) ;
#30528 = CARTESIAN_POINT ( 'NONE',  ( 5.076628168052703671, 61.84226448433412315, 8.527530157486179263 ) ) ;
#30530 = CARTESIAN_POINT ( 'NONE',  ( 10.00000000000000000, 31.81368534415483751, -10.88017736071110342 ) ) ;
#30529 = CARTESIAN_POINT ( 'NONE',  ( 2.035157376598824452, 28.68868534415484106, 7.964842623401179544 ) ) ;
#30532 = CARTESIAN_POINT ( 'NONE',  ( 13.43411237798106583, 27.66530133659708568, -12.81628187352647252 ) ) ;
#30531 = CARTESIAN_POINT ( 'NONE',  ( 19.84674366389459621, 58.50893115100078745, 7.409399052514197653E-17 ) ) ;
#30533 = CARTESIAN_POINT ( 'NONE',  ( 2.917880565312948704, 17.63708216824730357, 12.26659068614894643 ) ) ;
#30534 = DIRECTION ( 'NONE',  ( 0.000000000000000000, 0.000000000000000000, 1.000000000000000000 ) ) ;
#30535 = B_SPLINE_CURVE_WITH_KNOTS ( 'NONE', 3,
 ( #75617, #38132, #22633, #68620, #53113, #54091 ),
 .UNSPECIFIED., .F., .F.,
 ( 4, 2, 4 ),
 ( 5.553824967135426632E-18, 0.0002605067024380923143, 0.0005210134048761790992 ),
 .UNSPECIFIED. ) ;
#30536 = CARTESIAN_POINT ( 'NONE',  ( -1.099225684535947600, 43.70696800326375353, -6.408140936763238038 ) ) ;
#30537 = VERTEX_POINT ( 'NONE', #5940 ) ;
#30538 = CARTESIAN_POINT ( 'NONE',  ( 14.92337183194729988, 39.34226448433412315, -8.527530157486177487 ) ) ;
#30539 = CARTESIAN_POINT ( 'NONE',  ( 15.44008868035555260, 4.730352010821505360, 9.422509992056143702 ) ) ;
#30540 = ORIENTED_EDGE ( 'NONE', *, *, #74328, .F. ) ;
#30541 = CARTESIAN_POINT ( 'NONE',  ( 10.00000000000000178, 14.31368534415483929, 10.88017736071110342 ) ) ;
#30542 = ORIENTED_EDGE ( 'NONE', *, *, #67677, .F. ) ;
#30543 = CARTESIAN_POINT ( 'NONE',  ( 7.084665262690076126, 59.10535201082150536, 10.88017736071109987 ) ) ;
#30544 = CARTESIAN_POINT ( 'NONE',  ( -0.8801773607110991993, 52.85535201082151247, -2.915334737309923874 ) ) ;
#30545 = CARTESIAN_POINT ( 'NONE',  ( 4.559911319644449179, 63.89701867748817676, 9.422509992056141925 ) ) ;
#30546 = CARTESIAN_POINT ( 'NONE',  ( 12.91533473730992121, 49.52201867748817676, 10.88017736071110164 ) ) ;
#30547 =( GEOMETRIC_REPRESENTATION_CONTEXT ( 3 ) GLOBAL_UNCERTAINTY_ASSIGNED_CONTEXT ( ( #38134 ) ) GLOBAL_UNIT_ASSIGNED_CONTEXT ( ( #12870, #43369, #21372 ) ) REPRESENTATION_CONTEXT ( 'NONE', 'WORKASPACE' ) );
#30548 = CARTESIAN_POINT ( 'NONE',  ( 17.85999999999999588, 33.98752635800203592, 10.00000000000000000 ) ) ;
#30549 = CARTESIAN_POINT ( 'NONE',  ( -46.94000000000000483, 100.4746355719282320, 9.260812147861324561 ) ) ;
#30551 = VERTEX_POINT ( 'NONE', #5456 ) ;
#30550 = CARTESIAN_POINT ( 'NONE',  ( 8.862917522023083805, -7.247543382038870163, 4.000000000000000000 ) ) ;
#30552 = VECTOR ( 'NONE', #86916, 1000.000000000000000 ) ;
#30553 = CARTESIAN_POINT ( 'NONE',  ( 19.84674366389459266, 43.30059781766744464, 2.638427012816836559 ) ) ;
#30554 = ORIENTED_EDGE ( 'NONE', *, *, #52621, .T. ) ;
#30555 = CARTESIAN_POINT ( 'NONE',  ( -3.750000000000000000, 10.00000000000000000, -2.750000000000000000 ) ) ;
#30556 = CARTESIAN_POINT ( 'NONE',  ( -2.266590686148945544, 17.22041550158063572, 7.082119434687048631 ) ) ;
#30557 = CARTESIAN_POINT ( 'NONE',  ( 0.1957200283969098842, 35.25733960839543357, 6.499999999999991118 ) ) ;
#30559 = CARTESIAN_POINT ( 'NONE',  ( -0.8801773607110991993, 62.85535201082150536, -2.915334737309923874 ) ) ;
#30558 = CARTESIAN_POINT ( 'NONE',  ( 13.99999999999999822, 11.50000000000000000, -6.000000000000000000 ) ) ;
#30560 = CARTESIAN_POINT ( 'NONE',  ( -0.8801773607111008646, 13.27201867748817321, 2.915334737309923430 ) ) ;
#30561 = FILL_AREA_STYLE ('',( #47044 ) ) ;
#30563 = ORIENTED_EDGE ( 'NONE', *, *, #79610, .T. ) ;
#30562 = CARTESIAN_POINT ( 'NONE',  ( 16.40814093676323893, 45.79030133659708923, 11.09922568453595026 ) ) ;
#30564 = CARTESIAN_POINT ( 'NONE',  ( -11.92686044187656513, 4.688309369127514614, 3.903127820947815962E-15 ) ) ;
#30565 = CARTESIAN_POINT ( 'NONE',  ( 19.84674366389459266, 48.71726448433413026, -2.638427012816827677 ) ) ;
#30566 =( LENGTH_UNIT ( ) NAMED_UNIT ( * ) SI_UNIT ( .MILLI., .METRE. ) );
#30567 = CARTESIAN_POINT ( 'NONE',  ( 3.591859063236763294, 18.29030133659708568, -11.09922568453595026 ) ) ;
#30568 = CARTESIAN_POINT ( 'NONE',  ( 7.361572987183170547, 27.05059781766745175, 9.846743663894590881 ) ) ;
#30569 = ADVANCED_FACE ( 'NONE', ( #67921 ), #92018, .F. ) ;
#30570 = CARTESIAN_POINT ( 'NONE',  ( 7.684764310694881750, 14.63595249122788999, -12.88194075009936057 ) ) ;
#30571 = CARTESIAN_POINT ( 'NONE',  ( 18.52753015748617571, 18.09226448433411960, 4.923371831947298993 ) ) ;
#30572 = CARTESIAN_POINT ( 'NONE',  ( -2.816281873526473856, 14.33196800326375531, 3.434112377981055619 ) ) ;
#30573 = TOROIDAL_SURFACE ( 'NONE', #43348, 14.49999999999999822, 0.5000000000000000000 ) ;
#30574 = CARTESIAN_POINT ( 'NONE',  ( 10.00000000000000000, 4.758931151000784787, -9.846743663894594434 ) ) ;
#30575 = ORIENTED_EDGE ( 'NONE', *, *, #67635, .T. ) ;
#30576 = VERTEX_POINT ( 'NONE', #35928 ) ;
#30577 = CARTESIAN_POINT ( 'NONE',  ( 2.035157376598824452, 23.68868534415484461, 7.964842623401179544 ) ) ;
#30578 = CARTESIAN_POINT ( 'NONE',  ( 13.79529636645031943, 15.34541550158063750, -14.16423886937409904 ) ) ;
#30579 = CARTESIAN_POINT ( 'NONE',  ( 1.472469842513823179, 46.42559781766745175, 4.923371831947296329 ) ) ;
#30580 = CARTESIAN_POINT ( 'NONE',  ( 20.88017736071110519, 65.56368534415483396, 2.639326808657452039E-16 ) ) ;
#30581 = AXIS2_PLACEMENT_3D ( 'NONE', #75013, #6518, #45003 ) ;
#30583 = DIRECTION ( 'NONE',  ( 0.9636304532086229502, 0.000000000000000000, -0.2672383760782571227 ) ) ;
#30582 = CARTESIAN_POINT ( 'NONE',  ( -1.099225684535947600, 43.70696800326375353, -6.408140936763238038 ) ) ;
#30584 = CARTESIAN_POINT ( 'NONE',  ( 2.035157376598824452, 18.68868534415484106, 7.964842623401179544 ) ) ;
#30585 = LINE ( 'NONE', #7116, #90044 ) ;
#30586 = CARTESIAN_POINT ( 'NONE',  ( -1.099225684535947600, 9.540301336597087456, 6.408140936763237150 ) ) ;
#30587 = CARTESIAN_POINT ( 'NONE',  ( 10.00000000000000178, 32.25893115100078745, 9.846743663894594434 ) ) ;
#30588 = CARTESIAN_POINT ( 'NONE',  ( 10.88017736071109987, -14.22798132251182679, -2.915334737309928315 ) ) ;
#30589 = CARTESIAN_POINT ( 'NONE',  ( 19.38216949554541202, 35.99863466993041072, 9.382169495545424454 ) ) ;
#30590 = DIRECTION ( 'NONE',  ( -0.000000000000000000, 1.000000000000000000, -0.000000000000000000 ) ) ;
#30592 = CARTESIAN_POINT ( 'NONE',  ( 0.000000000000000000, 13.17686044187655270, 0.000000000000000000 ) ) ;
#30591 = CARTESIAN_POINT ( 'NONE',  ( 4.559911319644449179, 43.89701867748816966, 9.422509992056141925 ) ) ;
#30593 = PLANE ( 'NONE',  #37019 ) ;
#30594 = CARTESIAN_POINT ( 'NONE',  ( -0.1034006766853582671, 15.00000000000000000, 14.49963131601234956 ) ) ;
#30595 = CARTESIAN_POINT ( 'NONE',  ( 20.88017736071110875, 40.77201867748818387, -2.915334737309920765 ) ) ;
#30596 = CARTESIAN_POINT ( 'NONE',  ( 7.084665262690076126, 49.10535201082149825, 10.88017736071109987 ) ) ;
#30597 = CARTESIAN_POINT ( 'NONE',  ( 19.84674366389459621, 58.50893115100078745, 7.409399052514197653E-17 ) ) ;
#30598 = EDGE_CURVE ( 'NONE', #24464, #69208, #94463, .T. ) ;
#30599 = CARTESIAN_POINT ( 'NONE',  ( -0.8801773607110991993, 67.85535201082151957, -2.915334737309923874 ) ) ;
#30600 = EDGE_CURVE ( 'NONE', #7752, #74794, #29053, .T. ) ;
#30601 = CARTESIAN_POINT ( 'NONE',  ( 5.076628168052704559, 55.17559781766745175, -8.527530157486179263 ) ) ;
#30603 = FACE_OUTER_BOUND ( 'NONE', #91421, .T. ) ;
#30602 = CARTESIAN_POINT ( 'NONE',  ( 0.5774900079438590739, 7.647018677488171434, -5.440088680355550821 ) ) ;
#30604 = CARTESIAN_POINT ( 'NONE',  ( 19.38216949554541202, 5.998634669930420493, 9.382169495545424454 ) ) ;
#30605 = ORIENTED_EDGE ( 'NONE', *, *, #20806, .T. ) ;
#30606 = CARTESIAN_POINT ( 'NONE',  ( 0.5774900079438590739, 32.64701867748816966, -5.440088680355550821 ) ) ;
#30608 = DIRECTION ( 'NONE',  ( 0.9890158633619187123, 0.000000000000000000, -0.1478094111295981949 ) ) ;
#30607 = CARTESIAN_POINT ( 'NONE',  ( 17.20831665107776587, 57.88393115100078745, 7.208316651077764980 ) ) ;
#30609 = CARTESIAN_POINT ( 'NONE',  ( 0.5774900079438607392, 13.48035201082150358, 5.440088680355550821 ) ) ;
#30610 = CARTESIAN_POINT ( 'NONE',  ( 19.42250999205614193, 25.14701867748817321, 5.440088680355555262 ) ) ;
#30611 = CARTESIAN_POINT ( 'NONE',  ( 24.16423886937410614, 34.30374883491396787, 8.672049930838204340E-16 ) ) ;
#30612 = CARTESIAN_POINT ( 'NONE',  ( 7.361572987183170547, 22.05059781766745530, 9.846743663894590881 ) ) ;
#30613 = CARTESIAN_POINT ( 'NONE',  ( 4.559911319644449179, 52.23035201082151247, -9.422509992056141925 ) ) ;
#30614 = CARTESIAN_POINT ( 'NONE',  ( -19.89999999999999858, 98.99999999999998579, 8.000000000000000000 ) ) ;
#30615 = CARTESIAN_POINT ( 'NONE',  ( 18.52753015748617571, 58.09226448433411605, 4.923371831947298993 ) ) ;
#30616 = ORIENTED_EDGE ( 'NONE', *, *, #94013, .T. ) ;
#30617 = VERTEX_POINT ( 'NONE', #33941 ) ;
#30618 = TOROIDAL_SURFACE ( 'NONE', #89721, 18.53834841531100608, 7.000000000000000000 ) ;
#30619 = CARTESIAN_POINT ( 'NONE',  ( 22.26659068614895176, 39.72041550158063217, -7.082119434687042414 ) ) ;
#30620 = CARTESIAN_POINT ( 'NONE',  ( 20.36894250292379382, 28.67874883491396787, 10.36894250292379205 ) ) ;
#30621 = CARTESIAN_POINT ( 'NONE',  ( -0.8801773607111008646, 68.27201867748817676, 2.915334737309923430 ) ) ;
#30622 = CARTESIAN_POINT ( 'NONE',  ( 19.84674366389459621, 43.50893115100078745, 7.409399052514197653E-17 ) ) ;
#30623 = CARTESIAN_POINT ( 'NONE',  ( -9.543970587277799567, -28.01866822100916465, 4.000000000000000000 ) ) ;
#30625 = CARTESIAN_POINT ( 'NONE',  ( 10.00000000000000000, 12.87363466993042138, -12.81628187352647608 ) ) ;
#30624 = CARTESIAN_POINT ( 'NONE',  ( 10.00000000000000178, 49.31368534415484106, 10.88017736071110342 ) ) ;
#30626 = CARTESIAN_POINT ( 'NONE',  ( 13.79529636645031943, 35.34541550158063927, -14.16423886937409904 ) ) ;
#30627 = CARTESIAN_POINT ( 'NONE',  ( 10.00000000000000000, 11.81368534415483751, -10.88017736071110342 ) ) ;
#30628 = CARTESIAN_POINT ( 'NONE',  ( 7.084665262690076126, 32.02201867748816966, -10.88017736071110164 ) ) ;
#30629 = CARTESIAN_POINT ( 'NONE',  ( 21.92686044187656691, 4.953790035174471917, 3.195792623639537755 ) ) ;
#30630 = CARTESIAN_POINT ( 'NONE',  ( 0.5774900079438590739, 52.64701867748817676, -5.440088680355550821 ) ) ;
#30631 = CARTESIAN_POINT ( 'NONE',  ( 21.09922568453595559, 47.04030133659708923, -6.408140936763230044 ) ) ;
#30632 = CARTESIAN_POINT ( 'NONE',  ( -2.638427012816824124, -22.94940218233254470, 9.846743663894596210 ) ) ;
#30633 = ORIENTED_EDGE ( 'NONE', *, *, #47623, .T. ) ;
#30634 = DIRECTION ( 'NONE',  ( 1.000000000000000000, 0.000000000000000000, 0.000000000000000000 ) ) ;
#30635 = VERTEX_POINT ( 'NONE', #12933 ) ;
#30636 = ORIENTED_EDGE ( 'NONE', *, *, #57231, .T. ) ;
#30637 = DIRECTION ( 'NONE',  ( 0.000000000000000000, 0.000000000000000000, 1.000000000000000000 ) ) ;
#30639 = CARTESIAN_POINT ( 'NONE',  ( 17.08211943468705130, 63.47041550158063927, 12.26659068614894998 ) ) ;
#30638 = CARTESIAN_POINT ( 'NONE',  ( 17.08211943468705130, 53.47041550158063217, 12.26659068614894998 ) ) ;
#30641 = CARTESIAN_POINT ( 'NONE',  ( 7.361572987183170547, 57.05059781766744464, 9.846743663894590881 ) ) ;
#30640 = CARTESIAN_POINT ( 'NONE',  ( 2.791683348922240793, 21.63393115100078745, 7.208316651077764092 ) ) ;
#30642 = CARTESIAN_POINT ( 'NONE',  ( -19.64999999999999858, 0.000000000000000000, -7.750000000000000000 ) ) ;
#30643 = EDGE_CURVE ( 'NONE', #8562, #45049, #25980, .T. ) ;
#30644 = CARTESIAN_POINT ( 'NONE',  ( 17.20831665107776587, 9.133931151000787452, -7.208316651077762316 ) ) ;
#30645 = VECTOR ( 'NONE', #13210, 1000.000000000000000 ) ;
#30646 = VECTOR ( 'NONE', #96336, 1000.000000000000000 ) ;
#30647 = CARTESIAN_POINT ( 'NONE',  ( -2.816281873526473856, 4.331968003263754419, 3.434112377981055619 ) ) ;
#30648 = CARTESIAN_POINT ( 'NONE',  ( -6.408140936763246032, 23.29030133659709634, -11.09922568453594316 ) ) ;
#30649 = VERTEX_POINT ( 'NONE', #57934 ) ;
#30650 = AXIS2_PLACEMENT_3D ( 'NONE', #68909, #60894, #23416 ) ;
#30651 = CARTESIAN_POINT ( 'NONE',  ( 24.16423886937409904, 29.09541550158063572, 3.795296366450317205 ) ) ;
#30652 = CIRCLE ( 'NONE', #32291, 0.1000000000000001166 ) ;
#30653 = CARTESIAN_POINT ( 'NONE',  ( -2.266590686148945544, 37.22041550158063217, 7.082119434687048631 ) ) ;
#30654 = VERTEX_POINT ( 'NONE', #42458 ) ;
#30655 = CARTESIAN_POINT ( 'NONE',  ( 22.81628187352647785, 51.62363466993042493, 6.195893100308588602E-16 ) ) ;
#30656 = CARTESIAN_POINT ( 'NONE',  ( 12.91533473730993009, 26.60535201082150536, -10.88017736071109987 ) ) ;
#30657 = CARTESIAN_POINT ( 'NONE',  ( 0.1532563361054100626, 50.80059781766745175, -2.638427012816831230 ) ) ;
#30658 = CARTESIAN_POINT ( 'NONE',  ( 12.91533473730992121, 29.52201867748817321, 10.88017736071110164 ) ) ;
#30659 = MECHANICAL_DESIGN_GEOMETRIC_PRESENTATION_REPRESENTATION (  '', ( #61006 ), #9992 ) ;
#30660 = DIRECTION ( 'NONE',  ( 0.000000000000000000, 1.000000000000000000, 0.000000000000000000 ) ) ;
#30661 = CARTESIAN_POINT ( 'NONE',  ( -6.732636091893172470, -88.11213685669366669, 2.750000000000000444 ) ) ;
#30662 = CARTESIAN_POINT ( 'NONE',  ( 19.84674366389459621, 58.50893115100078745, 7.409399052514197653E-17 ) ) ;
#30663 = CARTESIAN_POINT ( 'NONE',  ( 14.92337183194729633, 47.67559781766745175, 8.527530157486181039 ) ) ;
#30664 = CARTESIAN_POINT ( 'NONE',  ( -13.75801628063875803, 4.618045246005505222E-16, -4.578972376164643698 ) ) ;
#30665 = B_SPLINE_CURVE_WITH_KNOTS ( 'NONE', 3,
 ( #28472, #27968, #21469, #13977, #43462, #65468 ),
 .UNSPECIFIED., .F., .F.,
 ( 4, 2, 4 ),
 ( 0.000000000000000000, 0.0002605067024380854296, 0.0005210134048761708592 ),
 .UNSPECIFIED. ) ;
#30666 = CARTESIAN_POINT ( 'NONE',  ( -14.29730467489530632, 4.415605380435452030E-16, -2.416004766803409254 ) ) ;
#30667 = CARTESIAN_POINT ( 'NONE',  ( 0.1532563361054082862, 1.217264484334117824, 2.638427012816831674 ) ) ;
#30668 = CARTESIAN_POINT ( 'NONE',  ( -10.00000000000000000, 82.00000000000000000, -9.500000000000000000 ) ) ;
#30669 = ORIENTED_EDGE ( 'NONE', *, *, #5107, .F. ) ;
#30670 = CARTESIAN_POINT ( 'NONE',  ( 19.67858290521089160, 88.19931278102706074, 5.461713021790606248 ) ) ;
#30671 = CARTESIAN_POINT ( 'NONE',  ( 0.1532563361054082862, 26.21726448433411605, 2.638427012816831674 ) ) ;
#30672 = FACE_OUTER_BOUND ( 'NONE', #9997, .T. ) ;
#30673 = CARTESIAN_POINT ( 'NONE',  ( 16.40814093676323893, 35.79030133659708923, 11.09922568453595026 ) ) ;
#30674 = DIRECTION ( 'NONE',  ( 0.000000000000000000, 1.000000000000000000, -0.000000000000000000 ) ) ;
#30675 = CARTESIAN_POINT ( 'NONE',  ( -10.58171042697183850, 14.76984967302771601, 10.54749450092394625 ) ) ;
#30676 = ORIENTED_EDGE ( 'NONE', *, *, #96432, .F. ) ;
#30677 = LINE ( 'NONE', #69678, #98713 ) ;
#30678 = CARTESIAN_POINT ( 'NONE',  ( -13.82192141328815715, 4.664367351173465489E-16, 4.382292601468585680 ) ) ;
#30679 = CARTESIAN_POINT ( 'NONE',  ( 18.52753015748617571, 58.09226448433411605, 4.923371831947298993 ) ) ;
#30680 = CARTESIAN_POINT ( 'NONE',  ( 22.26659068614894466, 28.88708216824730357, 7.082119434687054849 ) ) ;
#30681 = CARTESIAN_POINT ( 'NONE',  ( 17.20831665107776587, 62.88393115100078745, 7.208316651077764980 ) ) ;
#30682 = CARTESIAN_POINT ( 'NONE',  ( 20.15039907845753575, 36.74884699246889141, 6.262539305110075283 ) ) ;
#30683 = CARTESIAN_POINT ( 'NONE',  ( 2.791683348922237240, 10.38393115100078390, -7.208316651077763204 ) ) ;
#30684 = CARTESIAN_POINT ( 'NONE',  ( -2.266590686148945544, 2.220415501580634388, 7.082119434687048631 ) ) ;
#30685 = CARTESIAN_POINT ( 'NONE',  ( 0.1532563361054100626, 45.80059781766745886, -2.638427012816831230 ) ) ;
#30686 = CARTESIAN_POINT ( 'NONE',  ( -0.8801773607111009756, 48.06368534415484817, 1.068504757029289695E-15 ) ) ;
#30687 = ADVANCED_FACE ( 'NONE', ( #26950 ), #4954, .T. ) ;
#30688 = CARTESIAN_POINT ( 'NONE',  ( 0.7577696756376512965, 0.2301502180066073988, -14.92139465029747747 ) ) ;
#30689 = TOROIDAL_SURFACE ( 'NONE', #414, 14.49999999999999822, 0.5000000000000000000 ) ;
#30690 = CARTESIAN_POINT ( 'NONE',  ( 12.91533473730993009, 61.60535201082150536, -10.88017736071109987 ) ) ;
#30691 = ORIENTED_EDGE ( 'NONE', *, *, #26619, .T. ) ;
#30692 = DIRECTION ( 'NONE',  ( -4.618527782440651208E-14, 0.000000000000000000, 1.000000000000000000 ) ) ;
#30693 = CARTESIAN_POINT ( 'NONE',  ( 20.88017736071110875, 30.77201867748816966, -2.915334737309920765 ) ) ;
#30695 = CARTESIAN_POINT ( 'NONE',  ( 20.88017736071110164, 60.35535201082151957, 2.915334737309930979 ) ) ;
#30694 = CARTESIAN_POINT ( 'NONE',  ( 10.00000000000000000, 64.75893115100078035, -9.846743663894594434 ) ) ;
#30696 = PRESENTATION_STYLE_ASSIGNMENT (( #75220 ) ) ;
#30697 = CARTESIAN_POINT ( 'NONE',  ( 18.04007052943773104, 14.00257860105348762, -5.767676674365834977 ) ) ;
#30698 = FILL_AREA_STYLE ('',( #69215 ) ) ;
#30700 = CARTESIAN_POINT ( 'NONE',  ( 20.00000000000000711, 98.59912998021083297, -4.500000000000001776 ) ) ;
#30699 = CARTESIAN_POINT ( 'NONE',  ( 4.559911319644449179, 33.89701867748817676, 9.422509992056141925 ) ) ;
#30701 = CARTESIAN_POINT ( 'NONE',  ( 14.92337183194729633, 17.67559781766745175, 8.527530157486181039 ) ) ;
#30702 = CARTESIAN_POINT ( 'NONE',  ( 12.63842701281683034, 32.46726448433412315, 9.846743663894596210 ) ) ;
#30703 = PLANE ( 'NONE',  #98482 ) ;
#30704 = CARTESIAN_POINT ( 'NONE',  ( -10.36894250292378317, 22.42874883491397853, 10.36894250292379560 ) ) ;
#30705 = CARTESIAN_POINT ( 'NONE',  ( 7.361572987183169658, 59.96726448433410894, -9.846743663894592657 ) ) ;
#30706 = CARTESIAN_POINT ( 'NONE',  ( 13.79529636645031943, 65.34541550158063217, -14.16423886937409904 ) ) ;
#30707 = CARTESIAN_POINT ( 'NONE',  ( 20.15039907845753220, 27.62777174578613071, -6.262539305110077947 ) ) ;
#30708 = CARTESIAN_POINT ( 'NONE',  ( 24.16423886937410614, 24.51208216824730002, -3.795296366450302550 ) ) ;
#30709 = CARTESIAN_POINT ( 'NONE',  ( -4.164238869374099927, 52.01208216824729647, 3.795296366450308767 ) ) ;
#30710 = AXIS2_PLACEMENT_3D ( 'NONE', #66100, #29090, #37602 ) ;
#30711 = CARTESIAN_POINT ( 'NONE',  ( 2.791683348922240793, 16.63393115100078745, 7.208316651077764092 ) ) ;
#30712 = CARTESIAN_POINT ( 'NONE',  ( 0.5774900079438590739, 2.647018677488170990, -5.440088680355550821 ) ) ;
#30713 = ORIENTED_EDGE ( 'NONE', *, *, #37166, .F. ) ;
#30714 = CARTESIAN_POINT ( 'NONE',  ( 19.84674366389459266, 23.30059781766745530, 2.638427012816836559 ) ) ;
#30715 = EDGE_CURVE ( 'NONE', #52108, #12652, #40920, .T. ) ;
#30716 = CARTESIAN_POINT ( 'NONE',  ( 4.559911319644449179, 22.23035201082150536, -9.422509992056141925 ) ) ;
#30717 = CARTESIAN_POINT ( 'NONE',  ( -2.816281873526471635, -1.084698663402913210, -3.434112377981056508 ) ) ;
#30719 = CARTESIAN_POINT ( 'NONE',  ( 1.821158202401527593, 6.166888798595236310, 6.499999999999993783 ) ) ;
#30718 = CARTESIAN_POINT ( 'NONE',  ( 10.00000000000000178, 13.05374883491396787, 14.16423886937410082 ) ) ;
#30720 = CARTESIAN_POINT ( 'NONE',  ( 2.062412797813223616E-17, 1.639999999999999014, 0.000000000000000000 ) ) ;
#30721 = VECTOR ( 'NONE', #7825, 1000.000000000000000 ) ;
#30722 = AXIS2_PLACEMENT_3D ( 'NONE', #4143, #73100, #27114 ) ;
#30723 = CARTESIAN_POINT ( 'NONE',  ( 14.92337183194729633, 7.675597817667451750, 8.527530157486181039 ) ) ;
#30724 = CARTESIAN_POINT ( 'NONE',  ( 22.81628187352647785, 41.62363466993042493, 6.195893100308588602E-16 ) ) ;
#30725 = CARTESIAN_POINT ( 'NONE',  ( 1.472469842513823179, 46.42559781766745175, 4.923371831947296329 ) ) ;
#30726 = ORIENTED_EDGE ( 'NONE', *, *, #66459, .F. ) ;
#30727 = CARTESIAN_POINT ( 'NONE',  ( 14.92337183194729633, 22.67559781766745175, 8.527530157486181039 ) ) ;
#30728 = CARTESIAN_POINT ( 'NONE',  ( 11.44533173451573660, -77.48526441101033413, -3.750000000000000000 ) ) ;
#30729 = CARTESIAN_POINT ( 'NONE',  ( -12.25993886608593364, 0.5000000000000004441, -8.642563219313787570 ) ) ;
#30730 = CARTESIAN_POINT ( 'NONE',  ( 24.16423886937410614, 59.51208216824728936, -3.795296366450302550 ) ) ;
#30731 = CARTESIAN_POINT ( 'NONE',  ( -0.8801773607111009756, 58.06368534415484106, 1.068504757029289695E-15 ) ) ;
#30732 = CARTESIAN_POINT ( 'NONE',  ( 6.879999999999995453, 70.25000000000000000, 6.500000000000000888 ) ) ;
#30733 = CARTESIAN_POINT ( 'NONE',  ( 18.52753015748617571, 38.09226448433412315, 4.923371831947298993 ) ) ;
#30734 = CARTESIAN_POINT ( 'NONE',  ( 2.035157376598824452, 8.688685344154839285, 7.964842623401179544 ) ) ;
#30735 = CARTESIAN_POINT ( 'NONE',  ( 10.00000000000000000, 44.75893115100078745, -9.846743663894594434 ) ) ;
#30736 = CARTESIAN_POINT ( 'NONE',  ( 5.428133280998942212, 0.000000000000000000, 0.5226697871167882425 ) ) ;
#30737 = CARTESIAN_POINT ( 'NONE',  ( 19.84674366389459621, 53.50893115100078745, 7.409399052514197653E-17 ) ) ;
#30738 = CARTESIAN_POINT ( 'NONE',  ( -0.8801773607110991993, 52.85535201082151247, -2.915334737309923874 ) ) ;
#30739 = AXIS2_PLACEMENT_3D ( 'NONE', #71785, #60950, #40806 ) ;
#30740 = ORIENTED_EDGE ( 'NONE', *, *, #56486, .F. ) ;
#30741 = ORIENTED_EDGE ( 'NONE', *, *, #70598, .F. ) ;
#30742 = DIRECTION ( 'NONE',  ( 0.6246950475544237324, 0.7808688094430306093, 0.000000000000000000 ) ) ;
#30743 = PLANE ( 'NONE',  #81195 ) ;
#30744 = CARTESIAN_POINT ( 'NONE',  ( 19.84674366389459621, 3.508931151000785231, 7.409399052514197653E-17 ) ) ;
#30745 = CARTESIAN_POINT ( 'NONE',  ( 0.6178305044545838731, 54.74863466993042493, 9.382169495545420901 ) ) ;
#30747 = CARTESIAN_POINT ( 'NONE',  ( 7.361572987183170547, 47.05059781766745175, 9.846743663894590881 ) ) ;
#30746 = CARTESIAN_POINT ( 'NONE',  ( 20.88017736071110519, 5.563685344154838397, 2.639326808657452039E-16 ) ) ;
#30748 = DIRECTION ( 'NONE',  ( 0.3665012267242945265, 0.000000000000000000, 0.9304175679820255729 ) ) ;
#30749 = CARTESIAN_POINT ( 'NONE',  ( -0.3689425029237898834, 31.17874883491396787, -10.36894250292378850 ) ) ;
#30750 = CARTESIAN_POINT ( 'NONE',  ( 22.26659068614894466, 58.88708216824729647, 7.082119434687054849 ) ) ;
#30751 = CARTESIAN_POINT ( 'NONE',  ( 14.92337183194729633, 52.67559781766745175, 8.527530157486181039 ) ) ;
#30752 = CARTESIAN_POINT ( 'NONE',  ( -0.8801773607110991993, 52.85535201082151247, -2.915334737309923874 ) ) ;
#30753 = CARTESIAN_POINT ( 'NONE',  ( 2.035157376598822676, 67.43868534415484817, -7.964842623401177768 ) ) ;
#30754 = VECTOR ( 'NONE', #81464, 999.9999999999998863 ) ;
#30755 = ADVANCED_FACE ( 'NONE', ( #79955 ), #19458, .T. ) ;
#30756 = VERTEX_POINT ( 'NONE', #65929 ) ;
#30757 = CARTESIAN_POINT ( 'NONE',  ( 19.38216949554541202, 55.99863466993041072, 9.382169495545424454 ) ) ;
#30758 = EDGE_LOOP ( 'NONE', ( #87066, #78968, #89034, #33842 ) ) ;
#30759 = CARTESIAN_POINT ( 'NONE',  ( 1.472469842513823179, 6.425597817667451750, 4.923371831947296329 ) ) ;
#30760 = ORIENTED_EDGE ( 'NONE', *, *, #28453, .F. ) ;
#30761 = CARTESIAN_POINT ( 'NONE',  ( 20.36894250292379738, 24.92874883491396787, -10.36894250292379027 ) ) ;
#30762 = CARTESIAN_POINT ( 'NONE',  ( 14.92337183194729988, 19.34226448433411960, -8.527530157486177487 ) ) ;
#30763 = CARTESIAN_POINT ( 'NONE',  ( 20.88017736071110519, 35.56368534415484106, 2.639326808657452039E-16 ) ) ;
#30764 = ADVANCED_FACE ( 'NONE', ( #18478, #41978 ), #96457, .F. ) ;
#30765 =( NAMED_UNIT ( * ) SI_UNIT ( $, .STERADIAN. ) SOLID_ANGLE_UNIT ( ) );
#30766 = ORIENTED_EDGE ( 'NONE', *, *, #86264, .F. ) ;
#30767 = CARTESIAN_POINT ( 'NONE',  ( 4.559911319644449179, 22.23035201082150536, -9.422509992056141925 ) ) ;
#30768 = AXIS2_PLACEMENT_3D ( 'NONE', #61652, #98221, #90190 ) ;
#30769 = ORIENTED_EDGE ( 'NONE', *, *, #39054, .F. ) ;
#30770 = CARTESIAN_POINT ( 'NONE',  ( 2.035157376598824452, 38.68868534415483396, 7.964842623401179544 ) ) ;
#30771 = CARTESIAN_POINT ( 'NONE',  ( 1.821158202401528481, 66.16688879859523809, 6.500000000000007105 ) ) ;
#30772 = EDGE_CURVE ( 'NONE', #89406, #96102, #72939, .T. ) ;
#30773 = SURFACE_SIDE_STYLE ('',( #21446 ) ) ;
#30774 = ORIENTED_EDGE ( 'NONE', *, *, #29581, .F. ) ;
#30775 = CARTESIAN_POINT ( 'NONE',  ( 10.00000000000000000, 22.87363466993042138, -12.81628187352647608 ) ) ;
#30776 = LINE ( 'NONE', #53789, #84513 ) ;
#30777 = CARTESIAN_POINT ( 'NONE',  ( 7.361572987183170547, 7.050597817667451750, 9.846743663894590881 ) ) ;
#30778 = FILL_AREA_STYLE_COLOUR ( '', #68934 ) ;
#30779 = CARTESIAN_POINT ( 'NONE',  ( 13.34343830728399283, 0.5000000000000004441, 6.852200678592689442 ) ) ;
#30780 = CARTESIAN_POINT ( 'NONE',  ( 12.63842701281683034, 12.46726448433411782, 9.846743663894596210 ) ) ;
#30781 = CARTESIAN_POINT ( 'NONE',  ( 0.5774900079438607392, 33.48035201082150536, 5.440088680355550821 ) ) ;
#30782 = COLOUR_RGB ( '', 0.31764706, 0.68627451, 0.89019608) ;
#30783 = VERTEX_POINT ( 'NONE', #27440 ) ;
#30784 = ORIENTED_EDGE ( 'NONE', *, *, #39699, .T. ) ;
#30785 = CARTESIAN_POINT ( 'NONE',  ( -0.8801773607111009756, 63.06368534415484106, 1.068504757029289695E-15 ) ) ;
#30786 = CARTESIAN_POINT ( 'NONE',  ( -46.94000000000016826, 103.2691844435149733, -6.361973263950634561 ) ) ;
#30787 = CARTESIAN_POINT ( 'NONE',  ( 22.81628187352647785, 61.41530133659709634, 3.434112377981063169 ) ) ;
#30788 = CARTESIAN_POINT ( 'NONE',  ( 19.42250999205614193, 65.14701867748817676, 5.440088680355555262 ) ) ;
#30789 = AXIS2_PLACEMENT_3D ( 'NONE', #67713, #82701, #52207 ) ;
#30790 = MECHANICAL_DESIGN_GEOMETRIC_PRESENTATION_REPRESENTATION (  '', ( #16402 ), #48357 ) ;
#30791 = CARTESIAN_POINT ( 'NONE',  ( 0.6178305044545838731, -0.2513653300695798953, 9.382169495545420901 ) ) ;
#30793 =( NAMED_UNIT ( * ) SI_UNIT ( $, .STERADIAN. ) SOLID_ANGLE_UNIT ( ) );
#30792 = COLOUR_RGB ( '', 0.08235294, 0.09019608, 0.10196078) ;
#30794 = B_SPLINE_CURVE_WITH_KNOTS ( 'NONE', 3,
 ( #32804, #18312, #41811, #63299, #10319, #87774 ),
 .UNSPECIFIED., .F., .F.,
 ( 4, 2, 4 ),
 ( 3.409110551419719510E-05, 0.0004400426677360445436, 0.0008459942299578918990 ),
 .UNSPECIFIED. ) ;
#30795 = B_SPLINE_CURVE_WITH_KNOTS ( 'NONE', 3,
 ( #15, #512, #54932, #84473, #93437, #1970 ),
 .UNSPECIFIED., .F., .F.,
 ( 4, 2, 4 ),
 ( 0.0002800075630655414352, 0.0006862128664597091660, 0.001092418169853877005 ),
 .UNSPECIFIED. ) ;
#30796 = CARTESIAN_POINT ( 'NONE',  ( 19.84674366389459266, 28.30059781766745886, 2.638427012816836559 ) ) ;
#30797 = CARTESIAN_POINT ( 'NONE',  ( 22.81628187352647785, 51.62363466993042493, 6.195893100308588602E-16 ) ) ;
#30798 = CARTESIAN_POINT ( 'NONE',  ( -0.000000000000000000, 78.62409777033050773, 9.230451250305735655 ) ) ;
#30799 = CARTESIAN_POINT ( 'NONE',  ( 19.84674366389459266, 23.71726448433412315, -2.638427012816827677 ) ) ;
#30800 = MECHANICAL_DESIGN_GEOMETRIC_PRESENTATION_REPRESENTATION (  '', ( #18047 ), #56302 ) ;
#30801 = CARTESIAN_POINT ( 'NONE',  ( 13.43411237798105340, 15.58196800326374998, 12.81628187352647963 ) ) ;
#30803 = CARTESIAN_POINT ( 'NONE',  ( -6.982525766850298687, -88.11956318484570261, -2.750000000000000444 ) ) ;
#30802 =( NAMED_UNIT ( * ) SI_UNIT ( $, .STERADIAN. ) SOLID_ANGLE_UNIT ( ) );
#30804 = CARTESIAN_POINT ( 'NONE',  ( 12.91533473730992121, 34.52201867748817676, 10.88017736071110164 ) ) ;
#30805 = CARTESIAN_POINT ( 'NONE',  ( 0.1532563361054082862, 66.21726448433413736, 2.638427012816831674 ) ) ;
#30806 = SURFACE_SIDE_STYLE ('',( #9296 ) ) ;
#30807 = CARTESIAN_POINT ( 'NONE',  ( 0.1532563361054100626, 20.80059781766744464, -2.638427012816831230 ) ) ;
#30808 = CARTESIAN_POINT ( 'NONE',  ( 2.791683348922237240, 5.383931151000785675, -7.208316651077763204 ) ) ;
#30809 = CARTESIAN_POINT ( 'NONE',  ( 4.559911319644449179, 18.89701867748817321, 9.422509992056141925 ) ) ;
#30810 = EDGE_CURVE ( 'NONE', #53420, #52573, #18570, .T. ) ;
#30811 = CARTESIAN_POINT ( 'NONE',  ( 13.43411237798105340, 20.58196800326374643, 12.81628187352647963 ) ) ;
#30812 = CARTESIAN_POINT ( 'NONE',  ( 14.92337183194729633, 57.67559781766745886, 8.527530157486181039 ) ) ;
#30813 = CARTESIAN_POINT ( 'NONE',  ( 5.429204171141014612, -28.64228857766720537, -2.499999999999999112 ) ) ;
#30815 = EDGE_CURVE ( 'NONE', #11994, #34811, #53875, .T. ) ;
#30814 = CARTESIAN_POINT ( 'NONE',  ( 2.035157376598822676, 7.438685344154837509, -7.964842623401177768 ) ) ;
#30816 = CARTESIAN_POINT ( 'NONE',  ( 19.84674366389459266, 43.71726448433410894, -2.638427012816827677 ) ) ;
#30817 = EDGE_LOOP ( 'NONE', ( #46295, #32752, #5052, #318, #52787, #83077 ) ) ;
#30818 = CARTESIAN_POINT ( 'NONE',  ( 5.114679605280758601, -17.52310038230844924, 2.750000000000000000 ) ) ;
#30819 = CARTESIAN_POINT ( 'NONE',  ( -0.8801773607110991993, 17.85535201082150536, -2.915334737309923874 ) ) ;
#30820 = LINE ( 'NONE', #91325, #83875 ) ;
#30821 = CARTESIAN_POINT ( 'NONE',  ( 17.96484262340118221, 29.93868534415484106, 7.964842623401181321 ) ) ;
#30822 =( GEOMETRIC_REPRESENTATION_CONTEXT ( 3 ) GLOBAL_UNCERTAINTY_ASSIGNED_CONTEXT ( ( #32194 ) ) GLOBAL_UNIT_ASSIGNED_CONTEXT ( ( #66925, #89918, #19943 ) ) REPRESENTATION_CONTEXT ( 'NONE', 'WORKASPACE' ) );
#30824 = FACE_OUTER_BOUND ( 'NONE', #56994, .T. ) ;
#30823 = CARTESIAN_POINT ( 'NONE',  ( -2.266590686148945544, 62.22041550158063927, 7.082119434687048631 ) ) ;
#30825 = CARTESIAN_POINT ( 'NONE',  ( 19.42250999205614548, 5.980352010821504471, -5.440088680355545492 ) ) ;
#30826 = CARTESIAN_POINT ( 'NONE',  ( 2.791683348922237240, 25.38393115100078390, -7.208316651077763204 ) ) ;
#30827 = CARTESIAN_POINT ( 'NONE',  ( -2.816281873526473856, 9.331968003263753531, 3.434112377981055619 ) ) ;
#30828 = CARTESIAN_POINT ( 'NONE',  ( -46.88208652658967424, 103.4388194638874694, 6.247021903621933880 ) ) ;
#30829 = CARTESIAN_POINT ( 'NONE',  ( 0.4400000000000020006, 1.019547802438468986, -3.750000000000000000 ) ) ;
#30830 =( GEOMETRIC_REPRESENTATION_CONTEXT ( 3 ) GLOBAL_UNCERTAINTY_ASSIGNED_CONTEXT ( ( #80431 ) ) GLOBAL_UNIT_ASSIGNED_CONTEXT ( ( #77688, #18679, #63172 ) ) REPRESENTATION_CONTEXT ( 'NONE', 'WORKASPACE' ) );
#30831 = CARTESIAN_POINT ( 'NONE',  ( 9.519554572442881835, -3.083623444479279201E-15, 11.10344954678186369 ) ) ;
#30832 = CARTESIAN_POINT ( 'NONE',  ( -8.159336008669392015, -4.163137246823999327, -3.750000000000000000 ) ) ;
#30833 = CARTESIAN_POINT ( 'NONE',  ( -4.164238869374098151, 11.59541550158063217, -3.795296366450310543 ) ) ;
#30834 = AXIS2_PLACEMENT_3D ( 'NONE', #86403, #41896, #18889 ) ;
#30835 = CARTESIAN_POINT ( 'NONE',  ( 7.361572987183170547, 32.05059781766745175, 9.846743663894590881 ) ) ;
#30836 = CARTESIAN_POINT ( 'NONE',  ( -6.732636091893168029, -88.11213685669366669, 4.000000000000000000 ) ) ;
#30837 = VERTEX_POINT ( 'NONE', #81429 ) ;
#30838 = EDGE_CURVE ( 'NONE', #71952, #5095, #63413, .T. ) ;
#30839 = CARTESIAN_POINT ( 'NONE',  ( 6.204703633549690345, 47.84541550158064638, 14.16423886937410082 ) ) ;
#30840 = CARTESIAN_POINT ( 'NONE',  ( 10.00000000000000178, 12.25893115100078568, 9.846743663894594434 ) ) ;
#30842 = FACE_OUTER_BOUND ( 'NONE', #67074, .T. ) ;
#30841 = DIRECTION ( 'NONE',  ( -0.9426414910921805390, 0.000000000000000000, 0.3338068592337649076 ) ) ;
#30843 = CARTESIAN_POINT ( 'NONE',  ( 20.88017736071110875, 40.77201867748818387, -2.915334737309920765 ) ) ;
#30844 = CARTESIAN_POINT ( 'NONE',  ( 6.565887622018943937, 48.08196800326375353, -12.81628187352647608 ) ) ;
#30845 = CARTESIAN_POINT ( 'NONE',  ( 17.96484262340118221, 14.93868534415483751, 7.964842623401181321 ) ) ;
#30846 = CARTESIAN_POINT ( 'NONE',  ( 22.81628187352647785, 51.41530133659708923, 3.434112377981063169 ) ) ;
#30847 = CARTESIAN_POINT ( 'NONE',  ( 1.472469842513823179, 61.42559781766745175, 4.923371831947296329 ) ) ;
#30848 = FILL_AREA_STYLE_COLOUR ( '', #49022 ) ;
#30850 = EDGE_LOOP ( 'NONE', ( #70940, #74394, #81581, #59648 ) ) ;
#30849 = ADVANCED_FACE ( 'NONE', ( #18971 ), #48962, .F. ) ;
#30851 = FACE_OUTER_BOUND ( 'NONE', #70276, .T. ) ;
#30852 = CARTESIAN_POINT ( 'NONE',  ( -10.97324858046188467, 15.00000000000000711, -9.670892530813352650 ) ) ;
#30853 = CARTESIAN_POINT ( 'NONE',  ( 2.917880565312950480, 45.97041550158063927, -12.26659068614894821 ) ) ;
#30854 = CARTESIAN_POINT ( 'NONE',  ( 22.26659068614895176, 14.72041550158063572, -7.082119434687042414 ) ) ;
#30855 = CARTESIAN_POINT ( 'NONE',  ( 20.88017736071110519, 25.56368534415483751, 2.639326808657452039E-16 ) ) ;
#30856 = CARTESIAN_POINT ( 'NONE',  ( 19.42250999205614193, 30.14701867748817321, 5.440088680355555262 ) ) ;
#30857 = FACE_BOUND ( 'NONE', #91961, .T. ) ;
#30858 = PLANE ( 'NONE',  #43214 ) ;
#30859 = CARTESIAN_POINT ( 'NONE',  ( 19.84674366389459266, 3.300597817667451750, 2.638427012816836559 ) ) ;
#30860 = CARTESIAN_POINT ( 'NONE',  ( 12.91533473730992121, 59.52201867748816966, 10.88017736071110164 ) ) ;
#30861 = CARTESIAN_POINT ( 'NONE',  ( -2.816281873526471635, 28.91530133659708213, -3.434112377981056508 ) ) ;
#30862 = CARTESIAN_POINT ( 'NONE',  ( 5.419894505350511871, 0.3639313574487206271, 13.98659156302465156 ) ) ;
#30863 = CARTESIAN_POINT ( 'NONE',  ( -11.92686044187656869, 2.453790035174480355, -3.195792623639521768 ) ) ;
#30864 = CARTESIAN_POINT ( 'NONE',  ( 17.20831665107776587, 39.13393115100079456, -7.208316651077762316 ) ) ;
#30865 = CARTESIAN_POINT ( 'NONE',  ( 17.96484262340118221, 9.938685344154837509, 7.964842623401181321 ) ) ;
#30866 = CARTESIAN_POINT ( 'NONE',  ( 16.40814093676324603, 12.45696800326375353, -11.09922568453594671 ) ) ;
#30867 = AXIS2_PLACEMENT_3D ( 'NONE', #43387, #12399, #95919 ) ;
#30868 = CARTESIAN_POINT ( 'NONE',  ( 19.84674366389459266, 3.717264484334118713, -2.638427012816827677 ) ) ;
#30869 = CARTESIAN_POINT ( 'NONE',  ( 17.96484262340118221, 14.93868534415483751, 7.964842623401181321 ) ) ;
#30870 = CARTESIAN_POINT ( 'NONE',  ( 17.20831665107776587, 44.13393115100078745, -7.208316651077762316 ) ) ;
#30871 = CARTESIAN_POINT ( 'NONE',  ( 22.81628187352647785, 61.62363466993041783, 6.195893100308588602E-16 ) ) ;
#30872 = CIRCLE ( 'NONE', #29294, 15.00000000000000000 ) ;
#30873 = CARTESIAN_POINT ( 'NONE',  ( 19.84674366389459266, 33.30059781766744464, 2.638427012816836559 ) ) ;
#30874 = CARTESIAN_POINT ( 'NONE',  ( -0.3689425029237881626, 17.42874883491397142, 10.36894250292379027 ) ) ;
#30875 = CARTESIAN_POINT ( 'NONE',  ( 2.035157376598824452, 33.68868534415484106, 7.964842623401179544 ) ) ;
#30876 = CARTESIAN_POINT ( 'NONE',  ( 17.96484262340118221, 14.93868534415483751, 7.964842623401181321 ) ) ;
#30877 = CIRCLE ( 'NONE', #81969, 14.49999999999999822 ) ;
#30878 = CARTESIAN_POINT ( 'NONE',  ( 17.96484262340118221, 26.18868534415483396, -7.964842623401177768 ) ) ;
#30879 = CARTESIAN_POINT ( 'NONE',  ( 12.91533473730993009, 21.60535201082150536, -10.88017736071109987 ) ) ;
#30880 = ORIENTED_EDGE ( 'NONE', *, *, #97594, .T. ) ;
#30881 = CARTESIAN_POINT ( 'NONE',  ( 12.91533473730992121, 44.52201867748816966, 10.88017736071110164 ) ) ;
#30882 = CARTESIAN_POINT ( 'NONE',  ( -1.099225684535947600, 64.54030133659709634, 6.408140936763237150 ) ) ;
#30883 = EDGE_CURVE ( 'NONE', #13031, #70888, #57065, .T. ) ;
#30884 = CARTESIAN_POINT ( 'NONE',  ( 4.559911319644449179, 42.23035201082151247, -9.422509992056141925 ) ) ;
#30885 = CARTESIAN_POINT ( 'NONE',  ( -0.8801773607110991993, 57.85535201082149825, -2.915334737309923874 ) ) ;
#30886 = ORIENTED_EDGE ( 'NONE', *, *, #67539, .F. ) ;
#30887 =( BOUNDED_CURVE ( )  B_SPLINE_CURVE ( 2, ( #17466, #71448, #11420, #56440, #78439, #85956, #55949, #40952, #2963 ),
 .UNSPECIFIED., .F., .F. ) 
 B_SPLINE_CURVE_WITH_KNOTS ( ( 3, 2, 2, 2, 3 ),
 ( 0.7972837940830885817, 0.7976190476190476719, 0.8035714285714286031, 0.8095238095238095344, 0.8098590630597686246 ),
 .UNSPECIFIED. ) 
 CURVE ( )  GEOMETRIC_REPRESENTATION_ITEM ( )  RATIONAL_B_SPLINE_CURVE ( ( 0.9963778908391764944, 0.9980808541467923733, 1.000000000000000000, 0.9659258262890683122, 1.000000000000000000, 0.9659258262890683122, 1.000000000000000000, 0.9980808541467922623, 0.9963778908391764944 ) ) 
 REPRESENTATION_ITEM ( '' )  );
#30888 = CARTESIAN_POINT ( 'NONE',  ( 20.88017736071110164, 50.35535201082151247, 2.915334737309930979 ) ) ;
#30889 = CARTESIAN_POINT ( 'NONE',  ( 6.575338752131433040, -50.90849809618014632, 3.750000000000000000 ) ) ;
#30890 = B_SPLINE_CURVE_WITH_KNOTS ( 'NONE', 3,
 ( #90773, #22297, #68778, #45276, #91264, #6789 ),
 .UNSPECIFIED., .F., .F.,
 ( 4, 2, 4 ),
 ( -2.009308255746759193E-05, 0.0003744380149044889881, 0.0007689691123664455646 ),
 .UNSPECIFIED. ) ;
#30891 = FILL_AREA_STYLE ('',( #62867 ) ) ;
#30892 = CARTESIAN_POINT ( 'NONE',  ( -2.266590686148945544, 51.38708216824730357, -7.082119434687050408 ) ) ;
#30893 = CARTESIAN_POINT ( 'NONE',  ( -0.8801773607110991993, 67.85535201082151957, -2.915334737309923874 ) ) ;
#30894 = CARTESIAN_POINT ( 'NONE',  ( 18.72515096720571037, 55.05509018479936145, 6.499999999999982236 ) ) ;
#30895 = CARTESIAN_POINT ( 'NONE',  ( -13.96521320569119595, 0.04922511925147229905, -4.755935267939353395 ) ) ;
#30896 = CARTESIAN_POINT ( 'NONE',  ( 18.52753015748618282, 38.92559781766745175, -4.923371831947291888 ) ) ;
#30897 = ORIENTED_EDGE ( 'NONE', *, *, #84820, .F. ) ;
#30898 = CARTESIAN_POINT ( 'NONE',  ( 0.1532563361054083140, 41.00893115100078745, 1.131784320476157264E-15 ) ) ;
#30899 = CARTESIAN_POINT ( 'NONE',  ( 20.88017736071110164, 45.35535201082149115, 2.915334737309930979 ) ) ;
#30900 = CARTESIAN_POINT ( 'NONE',  ( 5.076628168052704559, 35.17559781766745175, -8.527530157486179263 ) ) ;
#30902 = CARTESIAN_POINT ( 'NONE',  ( 7.084665262690076126, 57.02201867748817676, -10.88017736071110164 ) ) ;
#30901 = DIRECTION ( 'NONE',  ( 0.000000000000000000, 1.000000000000000000, 0.000000000000000000 ) ) ;
#30904 = CARTESIAN_POINT ( 'NONE',  ( 10.00000000000000178, 65.37363466993042493, 12.81628187352647608 ) ) ;
#30903 = CARTESIAN_POINT ( 'NONE',  ( 10.00000000000000178, 44.31368534415484106, 10.88017736071110342 ) ) ;
#30905 = CARTESIAN_POINT ( 'NONE',  ( -4.164238869374099039, 61.80374883491397497, 8.674139862899312516E-16 ) ) ;
#30906 = CARTESIAN_POINT ( 'NONE',  ( 19.38216949554541557, 17.24863466993041783, -9.382169495545420901 ) ) ;
#30907 = CARTESIAN_POINT ( 'NONE',  ( 19.72487221294571214, 22.80223176428831877, -6.499999999999988454 ) ) ;
#30908 = ORIENTED_EDGE ( 'NONE', *, *, #39884, .F. ) ;
#30909 = CARTESIAN_POINT ( 'NONE',  ( 3.591859063236761518, 14.95696800326375531, 11.09922568453594849 ) ) ;
#30910 = CARTESIAN_POINT ( 'NONE',  ( -0.8801773607110991993, 22.85535201082150181, -2.915334737309923874 ) ) ;
#30911 = CARTESIAN_POINT ( 'NONE',  ( 20.88017736071110875, 60.77201867748817676, -2.915334737309920765 ) ) ;
#30912 = ADVANCED_FACE ( 'NONE', ( #33962 ), #48985, .T. ) ;
#30913 = VERTEX_POINT ( 'NONE', #71980 ) ;
#30914 = CARTESIAN_POINT ( 'NONE',  ( 12.63842701281683034, 2.467264484334118269, 9.846743663894596210 ) ) ;
#30915 = CARTESIAN_POINT ( 'NONE',  ( 0.1532563361054083140, 46.00893115100079456, 1.131784320476157264E-15 ) ) ;
#30916 = CARTESIAN_POINT ( 'NONE',  ( 19.84674366389459266, 43.71726448433410894, -2.638427012816827677 ) ) ;
#30917 = CARTESIAN_POINT ( 'NONE',  ( 12.63842701281683034, 32.46726448433412315, 9.846743663894596210 ) ) ;
#30919 = CARTESIAN_POINT ( 'NONE',  ( 6.565887622018943937, 43.08196800326374643, -12.81628187352647608 ) ) ;
#30918 = DIRECTION ( 'NONE',  ( 0.3007057995042831666, 0.000000000000000000, -0.9537169507482237130 ) ) ;
#30921 = CYLINDRICAL_SURFACE ( 'NONE', #48311, 0.5000000000000004441 ) ;
#30920 = CARTESIAN_POINT ( 'NONE',  ( 2.791683348922240793, 11.63393115100078568, 7.208316651077764092 ) ) ;
#30922 = CARTESIAN_POINT ( 'NONE',  ( 20.15039907845753220, 45.60158574516643881, -6.262539305110077947 ) ) ;
#30924 = ORIENTED_EDGE ( 'NONE', *, *, #89439, .T. ) ;
#30923 = CARTESIAN_POINT ( 'NONE',  ( 1.472469842513823179, 50.59226448433411605, -4.923371831947296329 ) ) ;
#30925 = CARTESIAN_POINT ( 'NONE',  ( 0.2751277870542967463, 0.000000000000000000, 6.500000000000000888 ) ) ;
#30926 = CARTESIAN_POINT ( 'NONE',  ( -1.099225684535947600, 8.706968003263753531, -6.408140936763238038 ) ) ;
#30927 = EDGE_CURVE ( 'NONE', #11366, #339, #5152, .T. ) ;
#30928 = CARTESIAN_POINT ( 'NONE',  ( 15.44008868035555260, 49.73035201082150536, 9.422509992056143702 ) ) ;
#30930 = EDGE_CURVE ( 'NONE', #92377, #19902, #94484, .T. ) ;
#30929 = CARTESIAN_POINT ( 'NONE',  ( 2.917880565312948704, 37.63708216824731068, 12.26659068614894643 ) ) ;
#30931 = CARTESIAN_POINT ( 'NONE',  ( -10.29676451088645095, 12.55750643096800445, -4.707860652926549427 ) ) ;
#30932 = CARTESIAN_POINT ( 'NONE',  ( 19.65543155966242139, 92.23967373577187345, 5.359767647080724728 ) ) ;
#30933 = VECTOR ( 'NONE', #57916, 1000.000000000000000 ) ;
#30934 = CARTESIAN_POINT ( 'NONE',  ( -4.164238869374099039, 31.80374883491396432, 8.674139862899312516E-16 ) ) ;
#30935 = CARTESIAN_POINT ( 'NONE',  ( 13.79529636645031943, 65.34541550158063217, -14.16423886937409904 ) ) ;
#30936 = CARTESIAN_POINT ( 'NONE',  ( 6.204703633549690345, 5.762082168247301794, -14.16423886937410259 ) ) ;
#30938 = FACE_OUTER_BOUND ( 'NONE', #31677, .T. ) ;
#30937 = CARTESIAN_POINT ( 'NONE',  ( -0.3689425029237881626, 22.42874883491397142, 10.36894250292379027 ) ) ;
#30939 = CARTESIAN_POINT ( 'NONE',  ( 19.42250999205614193, 65.14701867748817676, 5.440088680355555262 ) ) ;
#30940 = CARTESIAN_POINT ( 'NONE',  ( -0.1503990784575242878, 29.24884699246888786, -6.262539305110083276 ) ) ;
#30942 = CARTESIAN_POINT ( 'NONE',  ( 18.52753015748617571, 43.09226448433412315, 4.923371831947298993 ) ) ;
#30941 = DIRECTION ( 'NONE',  ( 5.818595309480553908E-17, 1.000000000000000000, 0.000000000000000000 ) ) ;
#30943 = ORIENTED_EDGE ( 'NONE', *, *, #45390, .F. ) ;
#30944 = CARTESIAN_POINT ( 'NONE',  ( 7.084665262690076126, 24.10535201082150181, 10.88017736071109987 ) ) ;
#30945 = CARTESIAN_POINT ( 'NONE',  ( 20.32896413005680714, 55.57879003517447103, -5.963430220938276349 ) ) ;
#30946 = CARTESIAN_POINT ( 'NONE',  ( 2.791683348922240793, 66.63393115100079456, 7.208316651077764092 ) ) ;
#30947 = CARTESIAN_POINT ( 'NONE',  ( -0.9940297508538862292, 0.000000000000000000, 14.21528771620248932 ) ) ;
#30948 = CARTESIAN_POINT ( 'NONE',  ( 5.076628168052704559, 40.17559781766745175, -8.527530157486179263 ) ) ;
#30949 = CARTESIAN_POINT ( 'NONE',  ( 10.00000000000000178, 60.37363466993041783, 12.81628187352647608 ) ) ;
#30950 = CARTESIAN_POINT ( 'NONE',  ( -3.795296366450300773, -7.154584498419361616, 14.16423886937410437 ) ) ;
#30951 = CARTESIAN_POINT ( 'NONE',  ( 18.52753015748618282, 38.92559781766745175, -4.923371831947291888 ) ) ;
#30952 = CARTESIAN_POINT ( 'NONE',  ( 5.076628168052703671, 46.84226448433412315, 8.527530157486179263 ) ) ;
#30953 = CARTESIAN_POINT ( 'NONE',  ( 22.26659068614895176, 44.72041550158063927, -7.082119434687042414 ) ) ;
#30955 = EDGE_CURVE ( 'NONE', #72980, #43200, #3027, .T. ) ;
#30954 = ORIENTED_EDGE ( 'NONE', *, *, #41014, .F. ) ;
#30956 = CARTESIAN_POINT ( 'NONE',  ( 6.204703633549690345, 7.845415501580634832, 14.16423886937410082 ) ) ;
#30957 = CARTESIAN_POINT ( 'NONE',  ( 15.44008868035555793, 61.39701867748817676, -9.422509992056140149 ) ) ;
#30958 = FACE_OUTER_BOUND ( 'NONE', #65546, .T. ) ;
#30959 = CARTESIAN_POINT ( 'NONE',  ( 17.08211943468705840, 60.13708216824729647, -12.26659068614894466 ) ) ;
#30960 = CARTESIAN_POINT ( 'NONE',  ( 22.81628187352647785, 11.62363466993042138, 6.195893100308588602E-16 ) ) ;
#30961 = CARTESIAN_POINT ( 'NONE',  ( 21.92686044187656336, 1.979976035794174472, 3.195792623639536423 ) ) ;
#30962 = CARTESIAN_POINT ( 'NONE',  ( 12.63842701281683034, 2.467264484334118269, 9.846743663894596210 ) ) ;
#30963 = EDGE_CURVE ( 'NONE', #82286, #40665, #41013, .T. ) ;
#30964 = CARTESIAN_POINT ( 'NONE',  ( -0.8218345515130114354, 14.95077488074853456, 14.72992491912909152 ) ) ;
#30965 = CARTESIAN_POINT ( 'NONE',  ( -46.94000000000247752, 100.6180954154858398, -9.128675877383326309 ) ) ;
#30966 = CARTESIAN_POINT ( 'NONE',  ( 0.6178305044545838731, 29.74863466993042138, 9.382169495545420901 ) ) ;
#30967 = CARTESIAN_POINT ( 'NONE',  ( 20.36894250292379738, 59.92874883491397497, -10.36894250292379027 ) ) ;
#30968 = CARTESIAN_POINT ( 'NONE',  ( 3.999999999999999112, 23.03999999999999915, 4.898587196589411843E-16 ) ) ;
#30969 = CARTESIAN_POINT ( 'NONE',  ( -0.8801773607111008646, 28.27201867748817321, 2.915334737309923430 ) ) ;
#30970 = CARTESIAN_POINT ( 'NONE',  ( 19.42250999205614548, 30.98035201082150536, -5.440088680355545492 ) ) ;
#30971 = CARTESIAN_POINT ( 'NONE',  ( 2.791683348922237240, 55.38393115100078745, -7.208316651077763204 ) ) ;
#30972 = CARTESIAN_POINT ( 'NONE',  ( 19.84674366389459266, 48.30059781766745175, 2.638427012816836559 ) ) ;
#30973 = CARTESIAN_POINT ( 'NONE',  ( 22.81628187352647785, 56.41530133659708213, 3.434112377981063169 ) ) ;
#30974 = DIRECTION ( 'NONE',  ( -1.000000000000000000, -0.000000000000000000, 0.000000000000000000 ) ) ;
#30975 = ORIENTED_EDGE ( 'NONE', *, *, #4099, .F. ) ;
#30976 = CARTESIAN_POINT ( 'NONE',  ( 0.5774900079438590739, 12.64701867748817143, -5.440088680355550821 ) ) ;
#30977 = CARTESIAN_POINT ( 'NONE',  ( 22.81628187352648496, 16.83196800326374998, -3.434112377981050290 ) ) ;
#30978 = DIRECTION ( 'NONE',  ( -0.000000000000000000, -1.000000000000000000, -0.000000000000000000 ) ) ;
#30979 = CARTESIAN_POINT ( 'NONE',  ( 19.84674366389459266, 48.30059781766745175, 2.638427012816836559 ) ) ;
#30980 = CARTESIAN_POINT ( 'NONE',  ( -0.8801773607111008646, 43.27201867748817676, 2.915334737309923430 ) ) ;
#30981 = CARTESIAN_POINT ( 'NONE',  ( 6.565887622018943937, 18.08196800326375708, -12.81628187352647608 ) ) ;
#30983 = CYLINDRICAL_SURFACE ( 'NONE', #40029, 15.00000000000000000 ) ;
#30982 = CARTESIAN_POINT ( 'NONE',  ( 12.91533473730992121, 44.52201867748816966, 10.88017736071110164 ) ) ;
#30984 = DIRECTION ( 'NONE',  ( 1.000000000000000000, 1.465447498185264965E-15, 0.000000000000000000 ) ) ;
#30985 = ORIENTED_EDGE ( 'NONE', *, *, #87380, .T. ) ;
#30986 = CARTESIAN_POINT ( 'NONE',  ( 0.1532563361054100626, 60.80059781766744464, -2.638427012816831230 ) ) ;
#30987 = FACE_OUTER_BOUND ( 'NONE', #93511, .T. ) ;
#30988 = CARTESIAN_POINT ( 'NONE',  ( 17.96484262340118221, 44.93868534415483396, 7.964842623401181321 ) ) ;
#30990 = CARTESIAN_POINT ( 'NONE',  ( 24.16423886937409904, 9.095415501580633943, 3.795296366450317205 ) ) ;
#30989 = CARTESIAN_POINT ( 'NONE',  ( 13.43411237798105340, 45.58196800326374643, 12.81628187352647963 ) ) ;
#30991 = CARTESIAN_POINT ( 'NONE',  ( 1.472469842513823179, 5.592264484334118713, -4.923371831947296329 ) ) ;
#30992 = CARTESIAN_POINT ( 'NONE',  ( 2.791683348922240793, 61.63393115100079456, 7.208316651077764092 ) ) ;
#30993 = CARTESIAN_POINT ( 'NONE',  ( 0.1532563361054100626, 10.80059781766745175, -2.638427012816831230 ) ) ;
#30994 = DIRECTION ( 'NONE',  ( -1.000000000000000000, 0.000000000000000000, -0.000000000000000000 ) ) ;
#30995 = CARTESIAN_POINT ( 'NONE',  ( -0.3689425029237898834, 41.17874883491397497, -10.36894250292378850 ) ) ;
#30996 = ADVANCED_BREP_SHAPE_REPRESENTATION ( '', ( #41283, #27931 ), #96613 ) ;
#30997 = CARTESIAN_POINT ( 'NONE',  ( 17.96484262340118221, 6.188685344154836621, -7.964842623401177768 ) ) ;
#30998 = EDGE_CURVE ( 'NONE', #73080, #45005, #61851, .T. ) ;
#30999 = CARTESIAN_POINT ( 'NONE',  ( 17.96484262340118221, 4.938685344154837509, 7.964842623401181321 ) ) ;
#31000 = CARTESIAN_POINT ( 'NONE',  ( 4.020549461440701577, 0.000000000000000000, 3.684154808197116271 ) ) ;
#31001 = ORIENTED_EDGE ( 'NONE', *, *, #84512, .T. ) ;
#31002 = EDGE_LOOP ( 'NONE', ( #90982, #80496, #13679, #67311 ) ) ;
#31003 = CARTESIAN_POINT ( 'NONE',  ( 4.559911319644449179, 3.897018677488171434, 9.422509992056141925 ) ) ;
#31004 = CARTESIAN_POINT ( 'NONE',  ( 0.5774900079438607392, 8.480352010821505360, 5.440088680355550821 ) ) ;
#31005 = CARTESIAN_POINT ( 'NONE',  ( 5.076628168052704559, 40.17559781766745175, -8.527530157486179263 ) ) ;
#31006 = CARTESIAN_POINT ( 'NONE',  ( 10.00000000000000000, 32.87363466993042493, -12.81628187352647608 ) ) ;
#31007 = SURFACE_STYLE_USAGE ( .BOTH. , #25012 ) ;
#31010 = CARTESIAN_POINT ( 'NONE',  ( 20.36894250292379382, 8.678748834913967869, 10.36894250292379205 ) ) ;
#31009 = CARTESIAN_POINT ( 'NONE',  ( 6.879999999999995453, 43.00000000000000000, 4.250000000000000000 ) ) ;
#31008 = MECHANICAL_DESIGN_GEOMETRIC_PRESENTATION_REPRESENTATION (  '', ( #40649 ), #80544 ) ;
#31011 = CARTESIAN_POINT ( 'NONE',  ( 20.88017736071110164, 25.35535201082150891, 2.915334737309930979 ) ) ;
#31012 = CARTESIAN_POINT ( 'NONE',  ( 2.917880565312950480, 65.97041550158063217, -12.26659068614894821 ) ) ;
#31013 = CARTESIAN_POINT ( 'NONE',  ( 7.361572987183169658, 39.96726448433411605, -9.846743663894592657 ) ) ;
#31014 = CARTESIAN_POINT ( 'NONE',  ( 18.72515096720571037, 45.05509018479935435, 6.499999999999982236 ) ) ;
#31015 = CARTESIAN_POINT ( 'NONE',  ( 18.52753015748617571, 23.09226448433411960, 4.923371831947298993 ) ) ;
#31016 = CIRCLE ( 'NONE', #56503, 0.5000000000000000000 ) ;
#31017 = CARTESIAN_POINT ( 'NONE',  ( 6.408140936763243367, -39.20969866340291077, 11.09922568453594494 ) ) ;
#31018 = ORIENTED_EDGE ( 'NONE', *, *, #86712, .F. ) ;
#31019 = EDGE_LOOP ( 'NONE', ( #96242, #15216, #23201, #50305 ) ) ;
#31020 = CARTESIAN_POINT ( 'NONE',  ( 7.361572987183169658, 59.96726448433410894, -9.846743663894592657 ) ) ;
#31022 = CARTESIAN_POINT ( 'NONE',  ( 17.96484262340118221, 41.18868534415484106, -7.964842623401177768 ) ) ;
#31021 = CARTESIAN_POINT ( 'NONE',  ( 10.00000000000000000, 26.81368534415484106, -10.88017736071110342 ) ) ;
#31024 = CARTESIAN_POINT ( 'NONE',  ( -2.816281873526473856, 24.33196800326375353, 3.434112377981055619 ) ) ;
#31023 = CARTESIAN_POINT ( 'NONE',  ( 4.559911319644449179, 7.230352010821504471, -9.422509992056141925 ) ) ;
#31025 = CARTESIAN_POINT ( 'NONE',  ( 22.26659068614895176, 14.72041550158063572, -7.082119434687042414 ) ) ;
#31026 = EDGE_CURVE ( 'NONE', #98109, #66548, #83726, .T. ) ;
#31027 = CARTESIAN_POINT ( 'NONE',  ( -1.099225684535947600, 39.54030133659708923, 6.408140936763237150 ) ) ;
#31028 = ORIENTED_EDGE ( 'NONE', *, *, #29922, .T. ) ;
#31029 = CARTESIAN_POINT ( 'NONE',  ( 19.84674366389459621, 43.50893115100078745, 7.409399052514197653E-17 ) ) ;
#31030 = CARTESIAN_POINT ( 'NONE',  ( 17.96484262340118221, 26.18868534415483396, -7.964842623401177768 ) ) ;
#31031 = VERTEX_POINT ( 'NONE', #79975 ) ;
#31032 = CARTESIAN_POINT ( 'NONE',  ( 20.88017736071110164, 20.35535201082150891, 2.915334737309930979 ) ) ;
#31033 = ORIENTED_EDGE ( 'NONE', *, *, #18908, .T. ) ;
#31034 = CARTESIAN_POINT ( 'NONE',  ( 19.42250999205614548, 55.98035201082150536, -5.440088680355545492 ) ) ;
#31035 = DIRECTION ( 'NONE',  ( 0.000000000000000000, 0.000000000000000000, -1.000000000000000000 ) ) ;
#31036 = CARTESIAN_POINT ( 'NONE',  ( 10.00000000000000000, 66.81368534415484817, -10.88017736071110342 ) ) ;
#31037 = CARTESIAN_POINT ( 'NONE',  ( 1.472469842513823179, 6.425597817667451750, 4.923371831947296329 ) ) ;
#31038 = ADVANCED_FACE ( 'NONE', ( #72462 ), #90538, .T. ) ;
#31039 = CARTESIAN_POINT ( 'NONE',  ( 20.88017736071110519, 50.56368534415484106, 2.639326808657452039E-16 ) ) ;
#31040 = CARTESIAN_POINT ( 'NONE',  ( 4.838527690343618737, 14.49999999999999822, -14.19819177887726624 ) ) ;
#31041 = AXIS2_PLACEMENT_3D ( 'NONE', #62343, #77350, #47837 ) ;
#31042 = CARTESIAN_POINT ( 'NONE',  ( 2.603489959281592991, 11.58210964143329313, 6.500000000000006217 ) ) ;
#31044 = ORIENTED_EDGE ( 'NONE', *, *, #57243, .T. ) ;
#31043 = FACE_OUTER_BOUND ( 'NONE', #42380, .T. ) ;
#31045 = ADVANCED_FACE ( 'NONE', ( #56011 ), #97767, .T. ) ;
#31046 = CARTESIAN_POINT ( 'NONE',  ( 17.20831665107776587, 44.13393115100078745, -7.208316651077762316 ) ) ;
#31047 = ORIENTED_EDGE ( 'NONE', *, *, #81064, .F. ) ;
#31048 = VERTEX_POINT ( 'NONE', #93430 ) ;
#31049 = LINE ( 'NONE', #606, #98592 ) ;
#31051 = EDGE_CURVE ( 'NONE', #86750, #47321, #29872, .T. ) ;
#31050 = FACE_OUTER_BOUND ( 'NONE', #15560, .T. ) ;
#31052 = CARTESIAN_POINT ( 'NONE',  ( -4.164238869374099039, 16.80374883491396787, 8.674139862899312516E-16 ) ) ;
#31053 = CARTESIAN_POINT ( 'NONE',  ( 5.056330833731640162, 15.00000000000000000, 13.58983143750701394 ) ) ;
#31055 = CARTESIAN_POINT ( 'NONE',  ( 0.5774900079438607392, 58.48035201082151247, 5.440088680355550821 ) ) ;
#31054 = CARTESIAN_POINT ( 'NONE',  ( 19.72487221294570858, 10.71833443783938655, -6.500000000000000888 ) ) ;
#31056 = CARTESIAN_POINT ( 'NONE',  ( 12.91533473730992121, 14.52201867748817143, 10.88017736071110164 ) ) ;
#31057 = CARTESIAN_POINT ( 'NONE',  ( 2.603489959281590771, 66.58210964143327715, 6.500000000000003553 ) ) ;
#31058 = VERTEX_POINT ( 'NONE', #40936 ) ;
#31059 = CARTESIAN_POINT ( 'NONE',  ( 12.63842701281683034, 2.467264484334118269, 9.846743663894596210 ) ) ;
#31060 = CARTESIAN_POINT ( 'NONE',  ( 19.84674366389459266, 3.717264484334118713, -2.638427012816827677 ) ) ;
#31061 = B_SPLINE_CURVE_WITH_KNOTS ( 'NONE', 3,
 ( #5250, #36224, #5738, #97249, #49256, #50225 ),
 .UNSPECIFIED., .F., .F.,
 ( 4, 2, 4 ),
 ( 3.409110551496096809E-05, 0.0004400426677367859211, 0.0008459942299586109419 ),
 .UNSPECIFIED. ) ;
#31062 = CARTESIAN_POINT ( 'NONE',  ( -2.816281873526473856, 34.12363466993042493, 9.499525473075851096E-16 ) ) ;
#31063 = CARTESIAN_POINT ( 'NONE',  ( 12.63842701281683034, 27.46726448433411250, 9.846743663894596210 ) ) ;
#31064 = DIRECTION ( 'NONE',  ( 1.000000000000000000, 0.000000000000000000, 0.000000000000000000 ) ) ;
#31065 = CARTESIAN_POINT ( 'NONE',  ( -2.816281873526473856, 9.123634669930421381, 9.499525473075851096E-16 ) ) ;
#31066 = DIRECTION ( 'NONE',  ( 1.000000000000000000, 0.000000000000000000, 0.000000000000000000 ) ) ;
#31067 = CARTESIAN_POINT ( 'NONE',  ( 19.84674366389459266, 8.300597817667451750, 2.638427012816836559 ) ) ;
#31068 = B_SPLINE_CURVE_WITH_KNOTS ( 'NONE', 3,
 ( #49931, #88427, #80439, #11937 ),
 .UNSPECIFIED., .F., .F.,
 ( 4, 4 ),
 ( 6.234190775262425670E-17, 0.001060528352561999378 ),
 .UNSPECIFIED. ) ;
#31069 = VERTEX_POINT ( 'NONE', #57393 ) ;
#31070 = AXIS2_PLACEMENT_3D ( 'NONE', #19021, #80004, #65983 ) ;
#31071 = CARTESIAN_POINT ( 'NONE',  ( 7.084665262690076126, 27.02201867748817676, -10.88017736071110164 ) ) ;
#31072 = CARTESIAN_POINT ( 'NONE',  ( 24.16423886937410614, 24.51208216824730002, -3.795296366450302550 ) ) ;
#31073 = CARTESIAN_POINT ( 'NONE',  ( 18.52753015748618282, 43.92559781766745175, -4.923371831947291888 ) ) ;
#31074 = CARTESIAN_POINT ( 'NONE',  ( 4.559911319644449179, 67.23035201082150536, -9.422509992056141925 ) ) ;
#31076 = DIRECTION ( 'NONE',  ( 0.000000000000000000, 1.000000000000000000, 0.000000000000000000 ) ) ;
#31075 = CARTESIAN_POINT ( 'NONE',  ( 0.6178305044545818747, 43.49863466993042493, -9.382169495545419124 ) ) ;
#31077 = CARTESIAN_POINT ( 'NONE',  ( 17.96484262340118221, 29.93868534415484106, 7.964842623401181321 ) ) ;
#31078 = CIRCLE ( 'NONE', #86973, 1.249999999999987121 ) ;
#31079 = EDGE_CURVE ( 'NONE', #75433, #1023, #87403, .T. ) ;
#31080 = DIRECTION ( 'NONE',  ( 0.08715574274765140739, 0.9961946980917462113, 0.000000000000000000 ) ) ;
#31081 = CARTESIAN_POINT ( 'NONE',  ( 6.565887622018943937, 10.16530133659708746, 12.81628187352647430 ) ) ;
#31082 = CARTESIAN_POINT ( 'NONE',  ( 21.09922568453594849, 6.206968003263753531, 6.408140936763242479 ) ) ;
#31083 = CARTESIAN_POINT ( 'NONE',  ( 7.361572987183170547, 32.05059781766745175, 9.846743663894590881 ) ) ;
#31084 = CARTESIAN_POINT ( 'NONE',  ( -10.88017736071109987, 8.272018677488171434, 2.915334737309934532 ) ) ;
#31085 = CARTESIAN_POINT ( 'NONE',  ( 13.43411237798106583, 47.66530133659709634, -12.81628187352647252 ) ) ;
#31086 = CARTESIAN_POINT ( 'NONE',  ( 17.39651004071842166, 22.93575266056828355, 6.499999999999998224 ) ) ;
#31088 = CARTESIAN_POINT ( 'NONE',  ( -3.420591144908390113, 14.49999999999999112, -14.60477854057966063 ) ) ;
#31087 = CARTESIAN_POINT ( 'NONE',  ( 20.88017736071110875, 50.77201867748817676, -2.915334737309920765 ) ) ;
#31089 =( NAMED_UNIT ( * ) PLANE_ANGLE_UNIT ( ) SI_UNIT ( $, .RADIAN. ) );
#31090 = CARTESIAN_POINT ( 'NONE',  ( 12.91533473730993009, 66.60535201082150536, -10.88017736071109987 ) ) ;
#31091 = CARTESIAN_POINT ( 'NONE',  ( 2.035157376598822676, 37.43868534415484106, -7.964842623401177768 ) ) ;
#31092 = CARTESIAN_POINT ( 'NONE',  ( 19.42250999205614193, 40.14701867748817676, 5.440088680355555262 ) ) ;
#31093 = CARTESIAN_POINT ( 'NONE',  ( 0.1532563361054082862, 66.21726448433413736, 2.638427012816831674 ) ) ;
#31094 = AXIS2_PLACEMENT_3D ( 'NONE', #96786, #73756, #81265 ) ;
#31095 = CARTESIAN_POINT ( 'NONE',  ( 20.88017736071110519, 65.56368534415483396, 2.639326808657452039E-16 ) ) ;
#31096 = CARTESIAN_POINT ( 'NONE',  ( 14.92337183194729988, 49.34226448433411605, -8.527530157486177487 ) ) ;
#31098 = DIRECTION ( 'NONE',  ( 0.000000000000000000, 0.000000000000000000, 1.000000000000000000 ) ) ;
#31097 = CARTESIAN_POINT ( 'NONE',  ( 12.91533473730992121, 14.52201867748817143, 10.88017736071110164 ) ) ;
#31099 = CARTESIAN_POINT ( 'NONE',  ( 0.6178305044545818747, 8.498634669930421381, -9.382169495545419124 ) ) ;
#31100 = EDGE_LOOP ( 'NONE', ( #65320, #35393, #91619, #18846, #44533, #67014 ) ) ;
#31101 = CARTESIAN_POINT ( 'NONE',  ( 20.88017736071110875, 40.77201867748818387, -2.915334737309920765 ) ) ;
#31103 = DIRECTION ( 'NONE',  ( 0.9366721892483971246, -0.000000000000000000, 0.3502073812594687086 ) ) ;
#31102 = CARTESIAN_POINT ( 'NONE',  ( 19.38216949554541557, 7.248634669930421381, -9.382169495545420901 ) ) ;
#31104 = CARTESIAN_POINT ( 'NONE',  ( 20.88017736071110164, 15.35535201082150358, 2.915334737309930979 ) ) ;
#31105 = CARTESIAN_POINT ( 'NONE',  ( -0.8801773607111009756, 33.06368534415484106, 1.068504757029289695E-15 ) ) ;
#31106 = CARTESIAN_POINT ( 'NONE',  ( 6.204703633549690345, 32.84541550158063927, 14.16423886937410082 ) ) ;
#31107 = CARTESIAN_POINT ( 'NONE',  ( 7.361572987183170547, 27.05059781766745175, 9.846743663894590881 ) ) ;
#31108 = CARTESIAN_POINT ( 'NONE',  ( -0.8801773607110991993, 57.85535201082149825, -2.915334737309923874 ) ) ;
#31109 = CARTESIAN_POINT ( 'NONE',  ( 10.00000000000000178, 8.053748834913967869, 14.16423886937410082 ) ) ;
#31110 = PRESENTATION_LAYER_ASSIGNMENT (  '', '', ( #8781 ) ) ;
#31111 = UNCERTAINTY_MEASURE_WITH_UNIT (LENGTH_MEASURE( 1.000000000000000082E-05 ), #85113, 'distance_accuracy_value', 'NONE');
#31112 = CARTESIAN_POINT ( 'NONE',  ( 5.076628168052704559, 60.17559781766745175, -8.527530157486179263 ) ) ;
#31113 = ORIENTED_EDGE ( 'NONE', *, *, #87848, .T. ) ;
#31114 = EDGE_LOOP ( 'NONE', ( #63518, #24716, #90287, #43567 ) ) ;
#31115 = CARTESIAN_POINT ( 'NONE',  ( -4.164238869374098151, 41.59541550158061796, -3.795296366450310543 ) ) ;
#31116 = CARTESIAN_POINT ( 'NONE',  ( 20.36894250292379738, 39.92874883491396787, -10.36894250292379027 ) ) ;
#31117 = CARTESIAN_POINT ( 'NONE',  ( 5.076628168052703671, 6.842264484334118713, 8.527530157486179263 ) ) ;
#31118 = CARTESIAN_POINT ( 'NONE',  ( 18.52753015748617571, 58.09226448433411605, 4.923371831947298993 ) ) ;
#31119 = CARTESIAN_POINT ( 'NONE',  ( -11.62817260217089199, -77.84151128241060746, 4.000000000000001776 ) ) ;
#31121 = CARTESIAN_POINT ( 'NONE',  ( -2.816281873526471635, 23.91530133659708568, -3.434112377981056508 ) ) ;
#31120 = CARTESIAN_POINT ( 'NONE',  ( 10.00000000000000178, 64.31368534415483396, 10.88017736071110342 ) ) ;
#31122 = CARTESIAN_POINT ( 'NONE',  ( 22.26659068614894466, 23.88708216824730357, 7.082119434687054849 ) ) ;
#31123 = CARTESIAN_POINT ( 'NONE',  ( 12.91533473730992121, 19.52201867748816611, 10.88017736071110164 ) ) ;
#31124 = CARTESIAN_POINT ( 'NONE',  ( 10.00000000000000000, 31.81368534415483751, -10.88017736071110342 ) ) ;
#31125 = CARTESIAN_POINT ( 'NONE',  ( 3.000000000000000444, 22.11937003968011695, 3.673940397442059868E-16 ) ) ;
#31126 = CARTESIAN_POINT ( 'NONE',  ( 0.5774900079438607392, 53.48035201082151247, 5.440088680355550821 ) ) ;
#31127 = CARTESIAN_POINT ( 'NONE',  ( 2.638427012816835227, -7.532735515665882176, 9.846743663894590881 ) ) ;
#31128 = ADVANCED_FACE ( 'NONE', ( #41442 ), #11901, .F. ) ;
#31129 = ORIENTED_EDGE ( 'NONE', *, *, #3195, .F. ) ;
#31130 = CARTESIAN_POINT ( 'NONE',  ( 14.16722289976690163, 14.49999999999999112, -4.928467845925561974 ) ) ;
#31131 = TOROIDAL_SURFACE ( 'NONE', #29481, 1.000000000000000000, 0.5000000000000000000 ) ;
#31132 = ORIENTED_EDGE ( 'NONE', *, *, #74382, .T. ) ;
#31133 = DIRECTION ( 'NONE',  ( 0.000000000000000000, -1.000000000000000000, 0.000000000000000000 ) ) ;
#31134 = ORIENTED_EDGE ( 'NONE', *, *, #62317, .F. ) ;
#31136 = CARTESIAN_POINT ( 'NONE',  ( 6.204703633549690345, 60.76208216824730357, -14.16423886937410259 ) ) ;
#31135 = CARTESIAN_POINT ( 'NONE',  ( 10.00000000000000178, 58.05374883491397497, 14.16423886937410082 ) ) ;
#31138 = CARTESIAN_POINT ( 'NONE',  ( 17.20831665107776587, 57.88393115100078745, 7.208316651077764980 ) ) ;
#31137 = CARTESIAN_POINT ( 'NONE',  ( 0.1532563361054083140, 31.00893115100078390, 1.131784320476157264E-15 ) ) ;
#31139 =( NAMED_UNIT ( * ) SI_UNIT ( $, .STERADIAN. ) SOLID_ANGLE_UNIT ( ) );
#31140 = EDGE_CURVE ( 'NONE', #189, #62655, #19401, .T. ) ;
#31141 = CARTESIAN_POINT ( 'NONE',  ( -2.393480905993287777, 14.49999999999999112, 14.80781041047755409 ) ) ;
#31142 = CARTESIAN_POINT ( 'NONE',  ( 0.1532563361054083140, 11.00893115100078568, 1.131784320476157264E-15 ) ) ;
#31144 = CARTESIAN_POINT ( 'NONE',  ( 6.565887622018943937, 5.165301336597086568, 12.81628187352647430 ) ) ;
#31143 = VECTOR ( 'NONE', #25302, 1000.000000000000000 ) ;
#31145 = CARTESIAN_POINT ( 'NONE',  ( 6.408140936763243367, 20.79030133659709634, 11.09922568453594494 ) ) ;
#31146 = ORIENTED_EDGE ( 'NONE', *, *, #26467, .T. ) ;
#31147 = CARTESIAN_POINT ( 'NONE',  ( -4.164238869374098151, 41.59541550158061796, -3.795296366450310543 ) ) ;
#31148 = CARTESIAN_POINT ( 'NONE',  ( 2.917880565312948704, 37.63708216824731068, 12.26659068614894643 ) ) ;
#31149 = EDGE_LOOP ( 'NONE', ( #80204, #68907, #61485, #84516 ) ) ;
#31150 = CARTESIAN_POINT ( 'NONE',  ( 13.43411237798106583, 57.66530133659708923, -12.81628187352647252 ) ) ;
#31151 = CARTESIAN_POINT ( 'NONE',  ( 20.88017736071110875, 30.77201867748816966, -2.915334737309920765 ) ) ;
#31152 = CARTESIAN_POINT ( 'NONE',  ( 2.791683348922240793, 46.63393115100077324, 7.208316651077764092 ) ) ;
#31153 = CARTESIAN_POINT ( 'NONE',  ( 10.00000000000000178, 29.31368534415483751, 10.88017736071110342 ) ) ;
#31154 = CARTESIAN_POINT ( 'NONE',  ( -14.62617646268089899, 0.5000000000000004441, 3.327906561566782440 ) ) ;
#31155 = CARTESIAN_POINT ( 'NONE',  ( 17.20831665107776587, 54.13393115100079456, -7.208316651077762316 ) ) ;
#31156 = CARTESIAN_POINT ( 'NONE',  ( 2.791683348922237240, 55.38393115100078745, -7.208316651077763204 ) ) ;
#31157 = LINE ( 'NONE', #46182, #50488 ) ;
#31158 = EDGE_CURVE ( 'NONE', #84056, #55863, #71902, .T. ) ;
#31159 = TOROIDAL_SURFACE ( 'NONE', #16834, 14.49999999999999822, 0.5000000000000000000 ) ;
#31160 = DIRECTION ( 'NONE',  ( 0.000000000000000000, 0.000000000000000000, 1.000000000000000000 ) ) ;
#31161 = CARTESIAN_POINT ( 'NONE',  ( 5.076628168052703671, 1.842264484334118047, 8.527530157486179263 ) ) ;
#31162 = CARTESIAN_POINT ( 'NONE',  ( -8.606322355891206755, 3.940577227621431661E-16, -11.66967075398818743 ) ) ;
#31163 = VERTEX_POINT ( 'NONE', #40444 ) ;
#31164 = FACE_OUTER_BOUND ( 'NONE', #65184, .T. ) ;
#31165 = CARTESIAN_POINT ( 'NONE',  ( 1.472469842513823179, 30.59226448433411960, -4.923371831947296329 ) ) ;
#31166 = B_SPLINE_CURVE_WITH_KNOTS ( 'NONE', 3,
 ( #46556, #30557, #91574, #75083, #53560, #23589 ),
 .UNSPECIFIED., .F., .F.,
 ( 4, 2, 4 ),
 ( 0.000000000000000000, 0.0002701661927229427628, 0.0005403323854458855257 ),
 .UNSPECIFIED. ) ;
#31168 = ADVANCED_FACE ( 'NONE', ( #72880 ), #55436, .T. ) ;
#31167 = PLANE ( 'NONE',  #97991 ) ;
#31169 = CARTESIAN_POINT ( 'NONE',  ( 22.81628187352647785, 36.62363466993041783, 6.195893100308588602E-16 ) ) ;
#31170 = CARTESIAN_POINT ( 'NONE',  ( -3.530007528296587704, -1.230351260576522110, 2.750000000000000000 ) ) ;
#31171 = ORIENTED_EDGE ( 'NONE', *, *, #15058, .T. ) ;
#31172 = CARTESIAN_POINT ( 'NONE',  ( 11.36220558718861717, 15.00000000000000000, -9.008345252845218809 ) ) ;
#31173 = CARTESIAN_POINT ( 'NONE',  ( -11.36220558719268325, 15.00000000000000000, -9.008345252852777207 ) ) ;
#31174 = CARTESIAN_POINT ( 'NONE',  ( 18.52753015748618282, 58.92559781766745886, -4.923371831947291888 ) ) ;
#31175 = CARTESIAN_POINT ( 'NONE',  ( 24.16423886937410614, 39.51208216824731068, -3.795296366450302550 ) ) ;
#31176 = CARTESIAN_POINT ( 'NONE',  ( 12.63842701281683922, 54.55059781766745175, -9.846743663894590881 ) ) ;
#31177 = CARTESIAN_POINT ( 'NONE',  ( 21.92686044187656336, 36.97997603579418069, 3.195792623639536423 ) ) ;
#31178 = CARTESIAN_POINT ( 'NONE',  ( 19.84674366389459621, 13.50893115100078568, 7.409399052514197653E-17 ) ) ;
#31179 = CARTESIAN_POINT ( 'NONE',  ( 0.6178305044545838731, 54.74863466993042493, 9.382169495545420901 ) ) ;
#31180 = SURFACE_STYLE_USAGE ( .BOTH. , #29698 ) ;
#31181 = STYLED_ITEM ( 'NONE', ( #58071 ), #52588 ) ;
#31182 = CARTESIAN_POINT ( 'NONE',  ( 12.63842701281683034, 62.46726448433410894, 9.846743663894596210 ) ) ;
#31183 = CARTESIAN_POINT ( 'NONE',  ( 15.44008868035555260, 49.73035201082150536, 9.422509992056143702 ) ) ;
#31184 = CARTESIAN_POINT ( 'NONE',  ( 5.679566525937524979, -28.64346213795363738, -2.750000000000000888 ) ) ;
#31185 = TOROIDAL_SURFACE ( 'NONE', #87084, 14.49999999999999822, 0.5000000000000000000 ) ;
#31186 = CARTESIAN_POINT ( 'NONE',  ( -0.8801773607111008646, 58.27201867748816966, 2.915334737309923430 ) ) ;
#31187 = ORIENTED_EDGE ( 'NONE', *, *, #32, .F. ) ;
#31188 = CARTESIAN_POINT ( 'NONE',  ( 0.000000000000000000, 0.5000000000000004441, 0.000000000000000000 ) ) ;
#31189 = CARTESIAN_POINT ( 'NONE',  ( -0.8801773607110991993, 32.85535201082151247, -2.915334737309923874 ) ) ;
#31191 = CARTESIAN_POINT ( 'NONE',  ( 15.44008868035555793, 56.39701867748817676, -9.422509992056140149 ) ) ;
#31190 = CARTESIAN_POINT ( 'NONE',  ( 10.00000000000000178, 5.373634669930420493, 12.81628187352647608 ) ) ;
#31192 = CARTESIAN_POINT ( 'NONE',  ( 1.046131998949919373, 15.73810908735719494, 6.500000000000002665 ) ) ;
#31193 = LINE ( 'NONE', #69214, #84294 ) ;
#31194 = CARTESIAN_POINT ( 'NONE',  ( 8.731067818237042033, 4.537123368507811172, 8.731067818237033151 ) ) ;
#31196 = DIRECTION ( 'NONE',  ( 0.000000000000000000, 0.000000000000000000, 1.000000000000000000 ) ) ;
#31195 = CARTESIAN_POINT ( 'NONE',  ( 17.96484262340118221, 46.18868534415484106, -7.964842623401177768 ) ) ;
#31197 = CARTESIAN_POINT ( 'NONE',  ( 0.1532563361054083140, 36.00893115100078745, 1.131784320476157264E-15 ) ) ;
#31198 = SURFACE_SIDE_STYLE ('',( #23733 ) ) ;
#31199 = CARTESIAN_POINT ( 'NONE',  ( 10.36894250292378850, 14.92874883491396254, -10.36894250292379027 ) ) ;
#31200 = CARTESIAN_POINT ( 'NONE',  ( 19.84674366389459266, 63.71726448433412315, -2.638427012816827677 ) ) ;
#31201 = CARTESIAN_POINT ( 'NONE',  ( 19.42250999205614548, 10.98035201082150536, -5.440088680355545492 ) ) ;
#31202 = DIRECTION ( 'NONE',  ( -0.000000000000000000, -0.000000000000000000, -1.000000000000000000 ) ) ;
#31203 = CARTESIAN_POINT ( 'NONE',  ( -2.266590686148945544, 22.22041550158063572, 7.082119434687048631 ) ) ;
#31204 = CARTESIAN_POINT ( 'NONE',  ( -4.164238869374099039, 61.80374883491397497, 8.674139862899312516E-16 ) ) ;
#31205 = CARTESIAN_POINT ( 'NONE',  ( 7.361572987183170547, 22.05059781766745530, 9.846743663894590881 ) ) ;
#31206 = CARTESIAN_POINT ( 'NONE',  ( 19.80427997160308351, 32.75733960839544068, -6.500000000000010658 ) ) ;
#31207 = VERTEX_POINT ( 'NONE', #42404 ) ;
#31208 = CARTESIAN_POINT ( 'NONE',  ( 10.00000000000000178, 27.25893115100078390, 9.846743663894594434 ) ) ;
#31209 = CARTESIAN_POINT ( 'NONE',  ( 20.88017736071110164, 30.35535201082151247, 2.915334737309930979 ) ) ;
#31210 = CARTESIAN_POINT ( 'NONE',  ( 14.92337183194729633, 57.67559781766745886, 8.527530157486181039 ) ) ;
#31212 = DIRECTION ( 'NONE',  ( -1.000000000000000000, 0.000000000000000000, 0.000000000000000000 ) ) ;
#31211 = CARTESIAN_POINT ( 'NONE',  ( 24.16423886937410614, 4.512082168247300906, -3.795296366450302550 ) ) ;
#31213 = FACE_OUTER_BOUND ( 'NONE', #30276, .T. ) ;
#31214 = AXIS2_PLACEMENT_3D ( 'NONE', #527, #91978, #15514 ) ;
#31215 = CARTESIAN_POINT ( 'NONE',  ( 7.361572987183170547, 12.05059781766744997, 9.846743663894590881 ) ) ;
#31216 = CARTESIAN_POINT ( 'NONE',  ( 21.09922568453594849, 36.20696800326375353, 6.408140936763242479 ) ) ;
#31217 = CARTESIAN_POINT ( 'NONE',  ( 5.076628168052704559, 40.17559781766745175, -8.527530157486179263 ) ) ;
#31218 = ORIENTED_EDGE ( 'NONE', *, *, #53839, .F. ) ;
#31219 = CARTESIAN_POINT ( 'NONE',  ( 2.791683348922240793, 21.63393115100078745, 7.208316651077764092 ) ) ;
#31220 = DIRECTION ( 'NONE',  ( 0.000000000000000000, 0.000000000000000000, 1.000000000000000000 ) ) ;
#31221 = CARTESIAN_POINT ( 'NONE',  ( -0.3689425029237881626, 52.42874883491396076, 10.36894250292379027 ) ) ;
#31222 = CARTESIAN_POINT ( 'NONE',  ( 20.88017736071110164, 55.35535201082149825, 2.915334737309930979 ) ) ;
#31223 = CARTESIAN_POINT ( 'NONE',  ( 19.42250999205614193, 55.14701867748817676, 5.440088680355555262 ) ) ;
#31224 = CARTESIAN_POINT ( 'NONE',  ( 2.791683348922240793, 41.63393115100078745, 7.208316651077764092 ) ) ;
#31225 = CARTESIAN_POINT ( 'NONE',  ( 12.91533473730993009, 6.605352010821504471, -10.88017736071109987 ) ) ;
#31226 = CARTESIAN_POINT ( 'NONE',  ( -5.999999999999994671, 41.24999999999999289, 6.250000000000000000 ) ) ;
#31227 = CARTESIAN_POINT ( 'NONE',  ( 14.92337183194729988, 44.34226448433412315, -8.527530157486177487 ) ) ;
#31228 = CARTESIAN_POINT ( 'NONE',  ( 20.88017736071110875, 45.77201867748816966, -2.915334737309920765 ) ) ;
#31229 = CARTESIAN_POINT ( 'NONE',  ( 14.92337183194729988, 4.342264484334117824, -8.527530157486177487 ) ) ;
#31230 = UNCERTAINTY_MEASURE_WITH_UNIT (LENGTH_MEASURE( 1.000000000000000082E-05 ), #91765, 'distance_accuracy_value', 'NONE');
#31231 = VERTEX_POINT ( 'NONE', #32427 ) ;
#31232 = VERTEX_POINT ( 'NONE', #17452 ) ;
#31233 = CARTESIAN_POINT ( 'NONE',  ( -0.1503990784575287842, 28.10158574516642815, 6.262539305110075283 ) ) ;
#31234 = AXIS2_PLACEMENT_3D ( 'NONE', #26647, #19644, #20636 ) ;
#31235 = LINE ( 'NONE', #7282, #20532 ) ;
#31236 = CARTESIAN_POINT ( 'NONE',  ( 18.52753015748617571, 28.09226448433411960, 4.923371831947298993 ) ) ;
#31237 = CARTESIAN_POINT ( 'NONE',  ( 13.43411237798105340, 50.58196800326375353, 12.81628187352647963 ) ) ;
#31239 = CARTESIAN_POINT ( 'NONE',  ( 18.52753015748617571, 48.09226448433412315, 4.923371831947298993 ) ) ;
#31238 = CARTESIAN_POINT ( 'NONE',  ( 12.91533473730992121, 14.52201867748817143, 10.88017736071110164 ) ) ;
#31240 = CARTESIAN_POINT ( 'NONE',  ( 6.138934250732054565, 15.00000000000000000, -14.77128574976607389 ) ) ;
#31241 = CARTESIAN_POINT ( 'NONE',  ( 24.16423886937409904, 29.09541550158063572, 3.795296366450317205 ) ) ;
#31242 = CARTESIAN_POINT ( 'NONE',  ( -4.164238869374098151, 56.59541550158063927, -3.795296366450310543 ) ) ;
#31243 = CARTESIAN_POINT ( 'NONE',  ( 0.1532563361054100626, 55.80059781766745175, -2.638427012816831230 ) ) ;
#31244 = CARTESIAN_POINT ( 'NONE',  ( 18.00000000000000000, 77.37581971779007972, 4.190584158845563678 ) ) ;
#31245 = CARTESIAN_POINT ( 'NONE',  ( 0.5774900079438590739, 57.64701867748817676, -5.440088680355550821 ) ) ;
#31246 = CARTESIAN_POINT ( 'NONE',  ( 19.84674366389459266, 18.30059781766745175, 2.638427012816836559 ) ) ;
#31247 = CARTESIAN_POINT ( 'NONE',  ( -3.586264863366058098, -2.711807932106036212, 3.749999999999797939 ) ) ;
#31248 = EDGE_LOOP ( 'NONE', ( #81452, #89092, #97120, #22777 ) ) ;
#31249 = CARTESIAN_POINT ( 'NONE',  ( 5.451370222425311773, 0.000000000000000000, 0.1427491530890473426 ) ) ;
#31250 = ORIENTED_EDGE ( 'NONE', *, *, #32879, .T. ) ;
#31251 = CARTESIAN_POINT ( 'NONE',  ( 10.00000000000000178, 12.25893115100078568, 9.846743663894594434 ) ) ;
#31252 = ORIENTED_EDGE ( 'NONE', *, *, #91835, .T. ) ;
#31253 = VECTOR ( 'NONE', #11270, 1000.000000000000000 ) ;
#31254 = CARTESIAN_POINT ( 'NONE',  ( 13.79529636645031943, 25.34541550158063572, -14.16423886937409904 ) ) ;
#31255 = CARTESIAN_POINT ( 'NONE',  ( 7.361572987183170547, 27.05059781766745175, 9.846743663894590881 ) ) ;
#31256 = CARTESIAN_POINT ( 'NONE',  ( -0.8801773607110991993, 37.85535201082151247, -2.915334737309923874 ) ) ;
#31257 = EDGE_CURVE ( 'NONE', #18488, #11195, #13966, .T. ) ;
#31258 = FILL_AREA_STYLE ('',( #15793 ) ) ;
#31259 = VERTEX_POINT ( 'NONE', #56426 ) ;
#31260 = CARTESIAN_POINT ( 'NONE',  ( 10.00000000000000000, 31.81368534415483751, -10.88017736071110342 ) ) ;
#31261 = CARTESIAN_POINT ( 'NONE',  ( 12.21238578216004633, 15.00000000000000711, 8.049595036947206239 ) ) ;
#31262 = AXIS2_PLACEMENT_3D ( 'NONE', #75274, #29276, #14297 ) ;
#31263 = VERTEX_POINT ( 'NONE', #86912 ) ;
#31264 = CARTESIAN_POINT ( 'NONE',  ( 2.035157376598822676, 37.43868534415484106, -7.964842623401177768 ) ) ;
#31265 = EDGE_LOOP ( 'NONE', ( #51065, #50815, #41804, #69719 ) ) ;
#31266 = CARTESIAN_POINT ( 'NONE',  ( -2.816281873526473856, 14.12363466993041961, 9.499525473075851096E-16 ) ) ;
#31267 = CARTESIAN_POINT ( 'NONE',  ( 5.076628168052703671, 11.84226448433411960, 8.527530157486179263 ) ) ;
#31268 = SURFACE_STYLE_FILL_AREA ( #76779 ) ;
#31269 = LINE ( 'NONE', #54268, #60652 ) ;
#31270 = CARTESIAN_POINT ( 'NONE',  ( 1.472469842513823179, 21.42559781766745175, 4.923371831947296329 ) ) ;
#31271 = CARTESIAN_POINT ( 'NONE',  ( 4.559911319644449179, 33.89701867748817676, 9.422509992056141925 ) ) ;
#31272 = CIRCLE ( 'NONE', #48835, 6.999999999999999112 ) ;
#31274 = ORIENTED_EDGE ( 'NONE', *, *, #27212, .T. ) ;
#31273 = CIRCLE ( 'NONE', #55264, 15.00000000000000000 ) ;
#31275 = VERTEX_POINT ( 'NONE', #94900 ) ;
#31276 = EDGE_CURVE ( 'NONE', #7752, #82423, #93924, .T. ) ;
#31277 = LINE ( 'NONE', #61777, #34329 ) ;
#31278 = CARTESIAN_POINT ( 'NONE',  ( 10.00000000000000178, 59.31368534415484106, 10.88017736071110342 ) ) ;
#31279 = DIRECTION ( 'NONE',  ( 0.000000000000000000, 1.000000000000000000, 0.000000000000000000 ) ) ;
#31280 = VECTOR ( 'NONE', #96443, 1000.000000000000000 ) ;
#31281 =( NAMED_UNIT ( * ) PLANE_ANGLE_UNIT ( ) SI_UNIT ( $, .RADIAN. ) );
#31282 = CARTESIAN_POINT ( 'NONE',  ( 17.96484262340118221, 61.18868534415482685, -7.964842623401177768 ) ) ;
#31283 = ADVANCED_FACE ( 'NONE', ( #55933 ), #18422, .T. ) ;
#31284 = CARTESIAN_POINT ( 'NONE',  ( 16.40814093676323893, 5.790301336597087456, 11.09922568453595026 ) ) ;
#31285 = VERTEX_POINT ( 'NONE', #48417 ) ;
#31286 = FACE_OUTER_BOUND ( 'NONE', #11265, .T. ) ;
#31287 = CARTESIAN_POINT ( 'NONE',  ( 0.1532563361054082862, 36.21726448433410894, 2.638427012816831674 ) ) ;
#31288 = CARTESIAN_POINT ( 'NONE',  ( 6.565887622018943937, 50.16530133659708213, 12.81628187352647430 ) ) ;
#31289 = CARTESIAN_POINT ( 'NONE',  ( 7.361572987183169658, 14.96726448433411960, -9.846743663894592657 ) ) ;
#31290 = CARTESIAN_POINT ( 'NONE',  ( 6.565887622018943937, 20.16530133659708213, 12.81628187352647430 ) ) ;
#31292 = CARTESIAN_POINT ( 'NONE',  ( -7.072466555035560098, -84.40185515922217974, -2.750000000000000000 ) ) ;
#31291 = CARTESIAN_POINT ( 'NONE',  ( 14.43100913236850502, 4.664102659404345836E-16, -1.412789942453164693 ) ) ;
#31293 = CARTESIAN_POINT ( 'NONE',  ( -0.8801773607110991993, 37.85535201082151247, -2.915334737309923874 ) ) ;
#31294 = CARTESIAN_POINT ( 'NONE',  ( 14.92337183194729988, 59.34226448433412315, -8.527530157486177487 ) ) ;
#31295 = CARTESIAN_POINT ( 'NONE',  ( 12.60589901313219663, 0.3639308464568737356, 8.129656208642145998 ) ) ;
#31296 = CARTESIAN_POINT ( 'NONE',  ( 0.1532563361054083140, 16.00893115100078390, 1.131784320476157264E-15 ) ) ;
#31297 = CARTESIAN_POINT ( 'NONE',  ( 0.1532563361054083140, 6.008931151000784787, 1.131784320476157264E-15 ) ) ;
#31298 = CARTESIAN_POINT ( 'NONE',  ( 10.00000000000000178, 14.31368534415483751, 10.88017736071110342 ) ) ;
#31299 = CARTESIAN_POINT ( 'NONE',  ( 19.38216949554541202, 15.99863466993042138, 9.382169495545424454 ) ) ;
#31300 = SURFACE_SIDE_STYLE ('',( #16319 ) ) ;
#31301 = CARTESIAN_POINT ( 'NONE',  ( 0.1532563361054083140, 66.00893115100079456, 1.131784320476157264E-15 ) ) ;
#31302 = CARTESIAN_POINT ( 'NONE',  ( 4.380000000000000782, 0.09385850580201696158, -2.750000000000000000 ) ) ;
#31303 = CARTESIAN_POINT ( 'NONE',  ( 19.42250999205614193, 25.14701867748817321, 5.440088680355555262 ) ) ;
#31304 = CARTESIAN_POINT ( 'NONE',  ( 10.00000000000000178, 47.25893115100078745, 9.846743663894594434 ) ) ;
#31305 = CARTESIAN_POINT ( 'NONE',  ( 6.757645195922957093, -58.31151720878640532, 2.750000000000000444 ) ) ;
#31306 = CARTESIAN_POINT ( 'NONE',  ( -0.8801773607111009756, 13.06368534415483929, 1.068504757029289695E-15 ) ) ;
#31307 = CARTESIAN_POINT ( 'NONE',  ( -7.771322705631588335, 4.175205849424987664E-16, 12.24159072199911868 ) ) ;
#31308 = CARTESIAN_POINT ( 'NONE',  ( 2.035157376598822676, 27.43868534415483396, -7.964842623401177768 ) ) ;
#31310 = CARTESIAN_POINT ( 'NONE',  ( -0.1503990784575328643, 70.00000000000000000, 6.262539305110068177 ) ) ;
#31309 = CARTESIAN_POINT ( 'NONE',  ( 20.88017736071110519, 5.563685344154838397, 2.639326808657452039E-16 ) ) ;
#31311 = CARTESIAN_POINT ( 'NONE',  ( 7.361572987183169658, -0.03273551566588185635, -9.846743663894592657 ) ) ;
#31312 = EDGE_CURVE ( 'NONE', #57285, #21583, #77167, .T. ) ;
#31313 = CARTESIAN_POINT ( 'NONE',  ( 5.076628168052703671, 26.84226448433411960, 8.527530157486179263 ) ) ;
#31314 = CARTESIAN_POINT ( 'NONE',  ( 22.81628187352647785, 6.415301336597088344, 3.434112377981063169 ) ) ;
#31315 = CARTESIAN_POINT ( 'NONE',  ( 18.00000000000000355, 77.07179676972445748, -4.250000000000000000 ) ) ;
#31316 = VECTOR ( 'NONE', #24605, 1000.000000000000000 ) ;
#31317 = ADVANCED_FACE ( 'NONE', ( #33885 ), #21908, .T. ) ;
#31318 = CARTESIAN_POINT ( 'NONE',  ( 0.1532563361054083140, 66.00893115100079456, 1.131784320476157264E-15 ) ) ;
#31319 = FACE_OUTER_BOUND ( 'NONE', #4600, .T. ) ;
#31320 = SURFACE_STYLE_USAGE ( .BOTH. , #83845 ) ;
#31321 = CARTESIAN_POINT ( 'NONE',  ( 6.204703633549690345, 7.845415501580634832, 14.16423886937410082 ) ) ;
#31322 = CARTESIAN_POINT ( 'NONE',  ( 2.791683348922240793, 36.63393115100078035, 7.208316651077764092 ) ) ;
#31323 = CARTESIAN_POINT ( 'NONE',  ( -15.00000000000000000, 83.99999999999998579, 7.750000000000000000 ) ) ;
#31324 = ORIENTED_EDGE ( 'NONE', *, *, #88395, .T. ) ;
#31325 = CARTESIAN_POINT ( 'NONE',  ( 24.16423886937409904, 49.09541550158063217, 3.795296366450317205 ) ) ;
#31326 = CARTESIAN_POINT ( 'NONE',  ( 7.361572987183170547, 22.05059781766745530, 9.846743663894590881 ) ) ;
#31328 = CARTESIAN_POINT ( 'NONE',  ( 10.00000000000000178, 70.00000000000000000, 0.000000000000000000 ) ) ;
#31327 = SURFACE_STYLE_FILL_AREA ( #77319 ) ;
#31329 = CARTESIAN_POINT ( 'NONE',  ( 12.91533473730992121, 39.52201867748817676, 10.88017736071110164 ) ) ;
#31330 = CARTESIAN_POINT ( 'NONE',  ( 22.81628187352647785, 56.41530133659708213, 3.434112377981063169 ) ) ;
#31331 = CARTESIAN_POINT ( 'NONE',  ( 7.084665262690076126, 24.10535201082150181, 10.88017736071109987 ) ) ;
#31332 = CARTESIAN_POINT ( 'NONE',  ( 16.40814093676324603, 52.45696800326375353, -11.09922568453594671 ) ) ;
#31333 = CARTESIAN_POINT ( 'NONE',  ( 0.1532563361054082862, 66.21726448433413736, 2.638427012816831674 ) ) ;
#31334 = CARTESIAN_POINT ( 'NONE',  ( 14.92337183194729633, 2.675597817667451750, 8.527530157486181039 ) ) ;
#31335 = ORIENTED_EDGE ( 'NONE', *, *, #29323, .T. ) ;
#31336 = CARTESIAN_POINT ( 'NONE',  ( 10.82078848414219330, -0.03417435944610275333, -11.78082904627298433 ) ) ;
#31337 = DIRECTION ( 'NONE',  ( 1.000000000000000000, 0.000000000000000000, -0.000000000000000000 ) ) ;
#31338 = CARTESIAN_POINT ( 'NONE',  ( 17.08211943468705840, 60.13708216824729647, -12.26659068614894466 ) ) ;
#31339 = CARTESIAN_POINT ( 'NONE',  ( 10.00000000000000178, 18.05374883491396787, 14.16423886937410082 ) ) ;
#31340 = CARTESIAN_POINT ( 'NONE',  ( 17.96484262340118221, 16.18868534415483396, -7.964842623401177768 ) ) ;
#31341 = CARTESIAN_POINT ( 'NONE',  ( 19.42250999205614193, 40.14701867748817676, 5.440088680355555262 ) ) ;
#31342 = DIRECTION ( 'NONE',  ( 0.000000000000000000, 1.000000000000000000, 0.000000000000000000 ) ) ;
#31343 = DIRECTION ( 'NONE',  ( 0.000000000000000000, 0.000000000000000000, 1.000000000000000000 ) ) ;
#31344 = CARTESIAN_POINT ( 'NONE',  ( 15.44008868035555260, 64.73035201082151957, 9.422509992056143702 ) ) ;
#31345 = CARTESIAN_POINT ( 'NONE',  ( 10.00000000000000000, 66.81368534415484817, -10.88017736071110342 ) ) ;
#31346 = CARTESIAN_POINT ( 'NONE',  ( 22.81628187352648496, 21.83196800326374643, -3.434112377981050290 ) ) ;
#31347 = DIRECTION ( 'NONE',  ( -1.000000000000000000, 0.000000000000000000, 0.000000000000000000 ) ) ;
#31348 = CARTESIAN_POINT ( 'NONE',  ( 19.72487221294570858, 70.00000000000000000, 6.000000000000000000 ) ) ;
#31349 = CARTESIAN_POINT ( 'NONE',  ( 14.92337183194729988, 9.342264484334119601, -8.527530157486177487 ) ) ;
#31350 = CARTESIAN_POINT ( 'NONE',  ( 19.84674366389459266, 43.30059781766744464, 2.638427012816836559 ) ) ;
#31351 = CARTESIAN_POINT ( 'NONE',  ( 20.88017736071110164, 10.35535201082150714, 2.915334737309930979 ) ) ;
#31352 = VECTOR ( 'NONE', #87278, 1000.000000000000000 ) ;
#31353 = STYLED_ITEM ( 'NONE', ( #68790 ), #17764 ) ;
#31354 = B_SPLINE_CURVE_WITH_KNOTS ( 'NONE', 3,
 ( #8334, #22363, #23843, #84823, #16330, #46813 ),
 .UNSPECIFIED., .F., .F.,
 ( 4, 2, 4 ),
 ( 3.409110551494637202E-05, 0.0004400426677367937816, 0.0008459942299586411911 ),
 .UNSPECIFIED. ) ;
#31355 = CARTESIAN_POINT ( 'NONE',  ( 21.09922568453594849, 31.20696800326375353, 6.408140936763242479 ) ) ;
#31356 = CARTESIAN_POINT ( 'NONE',  ( 5.076628168052704559, 5.175597817667451750, -8.527530157486179263 ) ) ;
#31357 = DIRECTION ( 'NONE',  ( 1.000000000000000000, 0.000000000000000000, 0.000000000000000000 ) ) ;
#31358 = MECHANICAL_DESIGN_GEOMETRIC_PRESENTATION_REPRESENTATION (  '', ( #33000 ), #48912 ) ;
#31359 = CARTESIAN_POINT ( 'NONE',  ( 14.92337183194729988, 54.34226448433412315, -8.527530157486177487 ) ) ;
#31360 = CARTESIAN_POINT ( 'NONE',  ( 18.52753015748618282, 28.92559781766745175, -4.923371831947291888 ) ) ;
#31361 = CARTESIAN_POINT ( 'NONE',  ( 6.204703633549690345, 17.84541550158063217, 14.16423886937410082 ) ) ;
#31362 = CARTESIAN_POINT ( 'NONE',  ( 2.035157376598822676, 37.43868534415484106, -7.964842623401177768 ) ) ;
#31363 = CARTESIAN_POINT ( 'NONE',  ( 12.91533473730992121, 9.522018677488171434, 10.88017736071110164 ) ) ;
#31364 = CARTESIAN_POINT ( 'NONE',  ( 7.084665262690076126, 29.10535201082150181, 10.88017736071109987 ) ) ;
#31365 = CARTESIAN_POINT ( 'NONE',  ( 12.91533473730992121, 24.52201867748816966, 10.88017736071110164 ) ) ;
#31366 = ORIENTED_EDGE ( 'NONE', *, *, #37731, .T. ) ;
#31367 = CARTESIAN_POINT ( 'NONE',  ( 16.40814093676323893, 35.79030133659708923, 11.09922568453595026 ) ) ;
#31368 = CARTESIAN_POINT ( 'NONE',  ( 4.559911319644449179, 37.23035201082150536, -9.422509992056141925 ) ) ;
#31369 = VERTEX_POINT ( 'NONE', #66867 ) ;
#31370 = FACE_OUTER_BOUND ( 'NONE', #67060, .T. ) ;
#31371 = EDGE_CURVE ( 'NONE', #55012, #31523, #39532, .T. ) ;
#31372 = VECTOR ( 'NONE', #51958, 1000.000000000000114 ) ;
#31373 = CARTESIAN_POINT ( 'NONE',  ( 19.42250999205614193, 45.14701867748817676, 5.440088680355555262 ) ) ;
#31374 = ORIENTED_EDGE ( 'NONE', *, *, #78458, .F. ) ;
#31375 = CARTESIAN_POINT ( 'NONE',  ( 20.88017736071110519, 45.56368534415484106, 2.639326808657452039E-16 ) ) ;
#31376 = FACE_OUTER_BOUND ( 'NONE', #40674, .T. ) ;
#31377 =( LENGTH_UNIT ( ) NAMED_UNIT ( * ) SI_UNIT ( .MILLI., .METRE. ) );
#31378 = CARTESIAN_POINT ( 'NONE',  ( 24.16423886937410614, 54.51208216824730357, -3.795296366450302550 ) ) ;
#31379 = CARTESIAN_POINT ( 'NONE',  ( 2.035157376598822676, 62.43868534415483396, -7.964842623401177768 ) ) ;
#31380 = DIRECTION ( 'NONE',  ( -0.9969173337331274087, 0.000000000000000000, -0.07845909572785238206 ) ) ;
#31381 = CARTESIAN_POINT ( 'NONE',  ( -4.787136363774555647, -17.54594992866424974, -4.000000000000000000 ) ) ;
#31382 = CARTESIAN_POINT ( 'NONE',  ( 1.472469842513823179, 30.59226448433411960, -4.923371831947296329 ) ) ;
#31383 = ORIENTED_EDGE ( 'NONE', *, *, #7055, .F. ) ;
#31384 = CARTESIAN_POINT ( 'NONE',  ( 14.92337183194729633, 37.67559781766745175, 8.527530157486181039 ) ) ;
#31385 = CARTESIAN_POINT ( 'NONE',  ( 7.084665262690076126, 37.02201867748817676, -10.88017736071110164 ) ) ;
#31386 = CARTESIAN_POINT ( 'NONE',  ( 14.92337183194729988, 39.34226448433412315, -8.527530157486177487 ) ) ;
#31387 = CARTESIAN_POINT ( 'NONE',  ( 10.00000000000000178, 20.37363466993042138, 12.81628187352647608 ) ) ;
#31389 = CARTESIAN_POINT ( 'NONE',  ( -7.750000000000000000, 40.74999999999999289, 3.750000000000000000 ) ) ;
#31388 = CARTESIAN_POINT ( 'NONE',  ( 7.084665262690076126, 67.02201867748817676, -10.88017736071110164 ) ) ;
#31390 = CARTESIAN_POINT ( 'NONE',  ( 2.035157376598822676, 42.43868534415483396, -7.964842623401177768 ) ) ;
#31391 = CARTESIAN_POINT ( 'NONE',  ( 24.16423886937409904, 59.09541550158063217, 3.795296366450317205 ) ) ;
#31392 = EDGE_CURVE ( 'NONE', #33199, #87437, #77837, .T. ) ;
#31393 = CARTESIAN_POINT ( 'NONE',  ( 6.565887622018943937, 18.08196800326375708, -12.81628187352647608 ) ) ;
#31394 = CARTESIAN_POINT ( 'NONE',  ( 18.95386800104996183, 23.23810908735726599, -6.499999999999988454 ) ) ;
#31395 = ORIENTED_EDGE ( 'NONE', *, *, #97920, .F. ) ;
#31396 = CARTESIAN_POINT ( 'NONE',  ( 10.00000000000000178, 15.37363466993042138, 12.81628187352647608 ) ) ;
#31397 = CARTESIAN_POINT ( 'NONE',  ( 4.559911319644449179, 27.23035201082150536, -9.422509992056141925 ) ) ;
#31398 = CIRCLE ( 'NONE', #61737, 14.49999999999999822 ) ;
#31399 = CARTESIAN_POINT ( 'NONE',  ( 7.084665262690076126, 67.02201867748817676, -10.88017736071110164 ) ) ;
#31400 = ADVANCED_FACE ( 'NONE', ( #90340 ), #21374, .T. ) ;
#31401 = ORIENTED_EDGE ( 'NONE', *, *, #37851, .F. ) ;
#31402 = CARTESIAN_POINT ( 'NONE',  ( 0.1532563361054100626, 5.800597817667452638, -2.638427012816831230 ) ) ;
#31403 = CARTESIAN_POINT ( 'NONE',  ( 1.472469842513823179, 46.42559781766745175, 4.923371831947296329 ) ) ;
#31404 = CARTESIAN_POINT ( 'NONE',  ( 19.84674366389459621, 38.50893115100078745, 7.409399052514197653E-17 ) ) ;
#31405 = FILL_AREA_STYLE_COLOUR ( '', #84250 ) ;
#31406 = CARTESIAN_POINT ( 'NONE',  ( 1.472469842513823179, 31.42559781766745530, 4.923371831947296329 ) ) ;
#31407 = DIRECTION ( 'NONE',  ( 0.000000000000000000, 0.000000000000000000, -1.000000000000000000 ) ) ;
#31408 = LINE ( 'NONE', #76433, #6945 ) ;
#31410 = LINE ( 'NONE', #46910, #3645 ) ;
#31409 = CARTESIAN_POINT ( 'NONE',  ( 0.1532563361054100626, 15.80059781766745353, -2.638427012816831230 ) ) ;
#31411 = DIRECTION ( 'NONE',  ( 0.7253743710122867450, 0.000000000000000000, -0.6883545756937550220 ) ) ;
#31413 = ORIENTED_EDGE ( 'NONE', *, *, #6577, .T. ) ;
#31412 = CARTESIAN_POINT ( 'NONE',  ( 17.20831665107776587, 42.88393115100077324, 7.208316651077764980 ) ) ;
#31414 = CARTESIAN_POINT ( 'NONE',  ( 11.49638213510182005, 14.95077488074853811, -9.245501498401928586 ) ) ;
#31415 = CARTESIAN_POINT ( 'NONE',  ( 19.38216949554541557, 12.24863466993041961, -9.382169495545420901 ) ) ;
#31416 = CARTESIAN_POINT ( 'NONE',  ( 15.44008868035555793, 56.39701867748817676, -9.422509992056140149 ) ) ;
#31417 = AXIS2_PLACEMENT_3D ( 'NONE', #14222, #21728, #91188 ) ;
#31418 = CARTESIAN_POINT ( 'NONE',  ( 13.79529636645030344, 48.26208216824728936, 14.16423886937410614 ) ) ;
#31419 = CARTESIAN_POINT ( 'NONE',  ( 7.361572987183169658, -0.03273551566588185635, -9.846743663894592657 ) ) ;
#31420 = CARTESIAN_POINT ( 'NONE',  ( 20.00000000000000711, 98.59912998021083297, 5.000000000000000888 ) ) ;
#31421 = CARTESIAN_POINT ( 'NONE',  ( 6.204703633549690345, 42.84541550158063217, 14.16423886937410082 ) ) ;
#31422 = CARTESIAN_POINT ( 'NONE',  ( 2.917880565312950480, 65.97041550158063217, -12.26659068614894821 ) ) ;
#31423 = CARTESIAN_POINT ( 'NONE',  ( 24.16423886937409904, 24.09541550158063927, 3.795296366450317205 ) ) ;
#31425 = LINE ( 'NONE', #38465, #86099 ) ;
#31424 = CARTESIAN_POINT ( 'NONE',  ( 6.204703633549690345, 20.76208216824730357, -14.16423886937410259 ) ) ;
#31426 = DIRECTION ( 'NONE',  ( 1.000000000000000000, -0.000000000000000000, -0.000000000000000000 ) ) ;
#31428 = CARTESIAN_POINT ( 'NONE',  ( 17.20831665107776587, 39.13393115100079456, -7.208316651077762316 ) ) ;
#31427 = CARTESIAN_POINT ( 'NONE',  ( 4.130000000000000782, 1.019547802438464545, 2.500000000000000000 ) ) ;
#31429 = VECTOR ( 'NONE', #48833, 1000.000000000000000 ) ;
#31430 = CARTESIAN_POINT ( 'NONE',  ( 10.00000000000000000, 26.81368534415484106, -10.88017736071110342 ) ) ;
#31431 = CARTESIAN_POINT ( 'NONE',  ( 20.15039907845753220, 55.60158574516643171, -6.262539305110077947 ) ) ;
#31432 = DIRECTION ( 'NONE',  ( 0.000000000000000000, 1.000000000000000000, -0.000000000000000000 ) ) ;
#31433 = CARTESIAN_POINT ( 'NONE',  ( 19.67862543671680697, 89.79758947439231065, -5.461907810393946683 ) ) ;
#31434 = EDGE_CURVE ( 'NONE', #93127, #29027, #34715, .T. ) ;
#31435 = CARTESIAN_POINT ( 'NONE',  ( 18.52753015748617571, 38.09226448433412315, 4.923371831947298993 ) ) ;
#31437 = CARTESIAN_POINT ( 'NONE',  ( 22.81628187352647785, 51.41530133659708923, 3.434112377981063169 ) ) ;
#31436 = AXIS2_PLACEMENT_3D ( 'NONE', #87011, #48020, #10042 ) ;
#31438 = CARTESIAN_POINT ( 'NONE',  ( 3.469446951953614189E-15, -11.94625116508602680, 14.16423886937410259 ) ) ;
#31439 = VECTOR ( 'NONE', #74137, 1000.000000000000000 ) ;
#31440 = CARTESIAN_POINT ( 'NONE',  ( 19.84674366389459266, 38.71726448433412315, -2.638427012816827677 ) ) ;
#31441 = CARTESIAN_POINT ( 'NONE',  ( 19.84674366389459266, 58.30059781766745886, 2.638427012816836559 ) ) ;
#31442 = CARTESIAN_POINT ( 'NONE',  ( 22.26659068614894466, 33.88708216824730357, 7.082119434687054849 ) ) ;
#31443 = VECTOR ( 'NONE', #18536, 1000.000000000000000 ) ;
#31444 = ORIENTED_EDGE ( 'NONE', *, *, #70473, .T. ) ;
#31445 = CARTESIAN_POINT ( 'NONE',  ( 2.917880565312950480, 10.97041550158063572, -12.26659068614894821 ) ) ;
#31446 = DIRECTION ( 'NONE',  ( 0.000000000000000000, 0.000000000000000000, 1.000000000000000000 ) ) ;
#31447 = CARTESIAN_POINT ( 'NONE',  ( 10.00000000000000178, 4.313685344154837509, 10.88017736071110342 ) ) ;
#31448 = CARTESIAN_POINT ( 'NONE',  ( 21.09922568453595559, 7.040301336597086568, -6.408140936763230044 ) ) ;
#31449 = CARTESIAN_POINT ( 'NONE',  ( -13.40508947812159235, 3.877950237245923868E-16, -5.527528931046294502 ) ) ;
#31450 = CARTESIAN_POINT ( 'NONE',  ( 12.63842701281683922, 4.550597817667451750, -9.846743663894590881 ) ) ;
#31451 = FACE_OUTER_BOUND ( 'NONE', #15574, .T. ) ;
#31452 = DIRECTION ( 'NONE',  ( 0.000000000000000000, 0.000000000000000000, 1.000000000000000000 ) ) ;
#31453 = CARTESIAN_POINT ( 'NONE',  ( 2.603489959281581889, 30.43575266056827999, -6.499999999999995559 ) ) ;
#31454 = CARTESIAN_POINT ( 'NONE',  ( -0.3689425029237898834, 61.17874883491396076, -10.36894250292378850 ) ) ;
#31455 = DIRECTION ( 'NONE',  ( 1.257568779154408793E-17, 1.000000000000000000, -0.000000000000000000 ) ) ;
#31456 = CARTESIAN_POINT ( 'NONE',  ( 4.559911319644449179, 23.89701867748817321, 9.422509992056141925 ) ) ;
#31457 = CARTESIAN_POINT ( 'NONE',  ( 17.96484262340118221, 19.93868534415484106, 7.964842623401181321 ) ) ;
#31458 = CARTESIAN_POINT ( 'NONE',  ( 0.1532563361054082862, 61.21726448433412315, 2.638427012816831674 ) ) ;
#31459 = CARTESIAN_POINT ( 'NONE',  ( 17.20831665107776587, 52.88393115100078035, 7.208316651077764980 ) ) ;
#31460 = CLOSED_SHELL ( 'NONE', ( #88095, #35899, #80504, #60408, #92137, #93951, #2542, #16519, #50908, #1544, #41186, #25541, #4539, #44265, #31520, #84439, #20796, #27198, #19319, #43564, #5885, #84507, #45129, #15530, #82972, #48485, #21724, #10088, #31849, #90071 ) ) ;
#31461 = CARTESIAN_POINT ( 'NONE',  ( -45.03864103619531534, 105.4358411858499380, -5.309474494509486497 ) ) ;
#31462 = CARTESIAN_POINT ( 'NONE',  ( -5.419894505350674407, 15.00000000000000000, 13.98659156302455031 ) ) ;
#31463 = ORIENTED_EDGE ( 'NONE', *, *, #69537, .F. ) ;
#31464 = CARTESIAN_POINT ( 'NONE',  ( 12.91533473730993009, 26.60535201082150536, -10.88017736071109987 ) ) ;
#31465 = CARTESIAN_POINT ( 'NONE',  ( 22.81628187352647785, 21.62363466993041783, 6.195893100308588602E-16 ) ) ;
#31466 = LINE ( 'NONE', #69979, #56078 ) ;
#31467 = COLOUR_RGB ( '', 0.09019608, 0.27058824, 0.51372549) ;
#31468 = CARTESIAN_POINT ( 'NONE',  ( 19.84674366389459266, 63.30059781766745886, 2.638427012816836559 ) ) ;
#31469 = CARTESIAN_POINT ( 'NONE',  ( -0.8801773607111008646, 53.27201867748816966, 2.915334737309923430 ) ) ;
#31470 = CARTESIAN_POINT ( 'NONE',  ( 13.43411237798105340, 25.58196800326374998, 12.81628187352647963 ) ) ;
#31472 = CARTESIAN_POINT ( 'NONE',  ( 6.880000000000009663, 40.99999999999999289, -6.500000000000000888 ) ) ;
#31471 = CARTESIAN_POINT ( 'NONE',  ( 15.44008868035555260, 59.73035201082151247, 9.422509992056143702 ) ) ;
#31473 = CARTESIAN_POINT ( 'NONE',  ( 0.2751277870542911397, 50.30223176428831522, 6.499999999999992006 ) ) ;
#31474 = ORIENTED_EDGE ( 'NONE', *, *, #50023, .T. ) ;
#31475 = CARTESIAN_POINT ( 'NONE',  ( -0.8801773607111009756, 48.06368534415484817, 1.068504757029289695E-15 ) ) ;
#31476 = CARTESIAN_POINT ( 'NONE',  ( 17.96484262340118221, 49.93868534415484106, 7.964842623401181321 ) ) ;
#31478 = CARTESIAN_POINT ( 'NONE',  ( 20.36894250292379738, 14.92874883491396432, -10.36894250292379027 ) ) ;
#31477 = CARTESIAN_POINT ( 'NONE',  ( -2.816281873526473856, 44.12363466993042493, 9.499525473075851096E-16 ) ) ;
#31479 = CARTESIAN_POINT ( 'NONE',  ( 14.92337183194729633, 62.67559781766745886, 8.527530157486181039 ) ) ;
#31480 = CARTESIAN_POINT ( 'NONE',  ( 7.361572987183169658, 24.96726448433412315, -9.846743663894592657 ) ) ;
#31481 = DIRECTION ( 'NONE',  ( -1.000000000000000000, 0.000000000000000000, 0.000000000000000000 ) ) ;
#31482 = CARTESIAN_POINT ( 'NONE',  ( -0.3689425029237898834, 61.17874883491396076, -10.36894250292378850 ) ) ;
#31483 = VERTEX_POINT ( 'NONE', #73373 ) ;
#31484 = CARTESIAN_POINT ( 'NONE',  ( 15.44008868035555260, 4.730352010821504471, 9.422509992056143702 ) ) ;
#31485 = EDGE_CURVE ( 'NONE', #20205, #79142, #52356, .T. ) ;
#31486 = CARTESIAN_POINT ( 'NONE',  ( 12.91533473730992121, 4.522018677488169658, 10.88017736071110164 ) ) ;
#31487 = CARTESIAN_POINT ( 'NONE',  ( 1.472469842513823179, 16.42559781766745175, 4.923371831947296329 ) ) ;
#31488 = VECTOR ( 'NONE', #76730, 1000.000000000000000 ) ;
#31489 = ORIENTED_EDGE ( 'NONE', *, *, #92124, .F. ) ;
#31490 = CARTESIAN_POINT ( 'NONE',  ( 15.44008868035555793, 6.397018677488171434, -9.422509992056140149 ) ) ;
#31491 = CARTESIAN_POINT ( 'NONE',  ( 15.44008868035555260, 14.73035201082150536, 9.422509992056143702 ) ) ;
#31492 = CARTESIAN_POINT ( 'NONE',  ( 0.1532563361054100626, 45.80059781766745886, -2.638427012816831230 ) ) ;
#31493 = CARTESIAN_POINT ( 'NONE',  ( 16.40814093676323893, 40.79030133659708923, 11.09922568453595026 ) ) ;
#31494 = CARTESIAN_POINT ( 'NONE',  ( -18.89999999999999503, 92.00000000000000000, 7.750000000000000000 ) ) ;
#31496 = CARTESIAN_POINT ( 'NONE',  ( -0.3689425029237898834, 26.17874883491396432, -10.36894250292378850 ) ) ;
#31495 = CARTESIAN_POINT ( 'NONE',  ( -10.31693093662791405, 89.21683745891327533, -5.695017665641882054 ) ) ;
#31497 = CARTESIAN_POINT ( 'NONE',  ( 10.00000000000000000, 21.81368534415484106, -10.88017736071110342 ) ) ;
#31498 = CARTESIAN_POINT ( 'NONE',  ( 24.16423886937409904, 64.09541550158064638, 3.795296366450317205 ) ) ;
#31499 = CIRCLE ( 'NONE', #53849, 15.00000000000000000 ) ;
#31500 = EDGE_CURVE ( 'NONE', #43409, #42048, #74860, .T. ) ;
#31501 = CARTESIAN_POINT ( 'NONE',  ( 2.791683348922237240, 45.38393115100079456, -7.208316651077763204 ) ) ;
#31502 = CARTESIAN_POINT ( 'NONE',  ( 10.58840669699852199, -98.14374106289703548, 4.000000000000000000 ) ) ;
#31503 = CARTESIAN_POINT ( 'NONE',  ( 18.52753015748617571, 28.09226448433411960, 4.923371831947298993 ) ) ;
#31504 = CARTESIAN_POINT ( 'NONE',  ( 1.472469842513823179, 1.425597817667451528, 4.923371831947296329 ) ) ;
#31505 = CARTESIAN_POINT ( 'NONE',  ( -3.434112377981047626, -39.83469866340291787, 12.81628187352647963 ) ) ;
#31506 = TOROIDAL_SURFACE ( 'NONE', #50637, 14.49999999999999822, 0.5000000000000000000 ) ;
#31507 = ORIENTED_EDGE ( 'NONE', *, *, #61311, .T. ) ;
#31508 = CARTESIAN_POINT ( 'NONE',  ( 10.00000000000000000, 1.813685344154837731, -10.88017736071110342 ) ) ;
#31509 = CARTESIAN_POINT ( 'NONE',  ( 0.1532563361054082862, 1.217264484334117824, 2.638427012816831674 ) ) ;
#31510 = EDGE_CURVE ( 'NONE', #25131, #28832, #70300, .T. ) ;
#31511 = ORIENTED_EDGE ( 'NONE', *, *, #79843, .T. ) ;
#31512 = CARTESIAN_POINT ( 'NONE',  ( 19.84674366389459266, 63.30059781766745886, 2.638427012816836559 ) ) ;
#31514 = CARTESIAN_POINT ( 'NONE',  ( -0.8801773607111008646, 43.27201867748817676, 2.915334737309923430 ) ) ;
#31513 = CARTESIAN_POINT ( 'NONE',  ( 7.084665262690076126, 37.02201867748817676, -10.88017736071110164 ) ) ;
#31516 = CARTESIAN_POINT ( 'NONE',  ( 19.38216949554541202, 25.99863466993042138, 9.382169495545424454 ) ) ;
#31515 = CARTESIAN_POINT ( 'NONE',  ( 20.88017736071110519, 5.563685344154837509, 2.639326808657452039E-16 ) ) ;
#31517 = CARTESIAN_POINT ( 'NONE',  ( 22.26659068614894466, 13.88708216824730179, 7.082119434687054849 ) ) ;
#31518 = VECTOR ( 'NONE', #73093, 1000.000000000000000 ) ;
#31519 = CIRCLE ( 'NONE', #47584, 0.5000000000000004441 ) ;
#31520 = ADVANCED_FACE ( 'NONE', ( #28378 ), #4899, .T. ) ;
#31521 = ORIENTED_EDGE ( 'NONE', *, *, #37520, .T. ) ;
#31522 = CARTESIAN_POINT ( 'NONE',  ( 21.09922568453594849, 46.20696800326376064, 6.408140936763242479 ) ) ;
#31523 = VERTEX_POINT ( 'NONE', #67362 ) ;
#31524 = CARTESIAN_POINT ( 'NONE',  ( 0.1532563361054100626, 40.80059781766745886, -2.638427012816831230 ) ) ;
#31525 = CARTESIAN_POINT ( 'NONE',  ( 7.084665262690076126, 19.10535201082150181, 10.88017736071109987 ) ) ;
#31526 = EDGE_CURVE ( 'NONE', #65924, #65919, #57877, .T. ) ;
#31527 = CARTESIAN_POINT ( 'NONE',  ( 0.5774900079438607392, 18.48035201082150536, 5.440088680355550821 ) ) ;
#31528 = ORIENTED_EDGE ( 'NONE', *, *, #81256, .F. ) ;
#31529 = CARTESIAN_POINT ( 'NONE',  ( 19.42250999205614193, 60.14701867748817676, 5.440088680355555262 ) ) ;
#31530 = DIRECTION ( 'NONE',  ( 0.000000000000000000, -1.000000000000000000, -0.000000000000000000 ) ) ;
#31531 = CARTESIAN_POINT ( 'NONE',  ( 0.1532563361054100626, 5.800597817667452638, -2.638427012816831230 ) ) ;
#31532 = CARTESIAN_POINT ( 'NONE',  ( 17.96484262340118221, 64.93868534415483396, 7.964842623401181321 ) ) ;
#31533 = FILL_AREA_STYLE_COLOUR ( '', #36299 ) ;
#31534 = CARTESIAN_POINT ( 'NONE',  ( 2.603489959281591659, 10.43575266056827644, -6.500000000000006217 ) ) ;
#31536 = ORIENTED_EDGE ( 'NONE', *, *, #79405, .T. ) ;
#31535 = CARTESIAN_POINT ( 'NONE',  ( 5.076628168052703671, 1.842264484334118047, 8.527530157486179263 ) ) ;
#31537 = CARTESIAN_POINT ( 'NONE',  ( 1.472469842513823179, 40.59226448433411605, -4.923371831947296329 ) ) ;
#31538 = ORIENTED_EDGE ( 'NONE', *, *, #12207, .F. ) ;
#31539 = VERTEX_POINT ( 'NONE', #27386 ) ;
#31540 = CARTESIAN_POINT ( 'NONE',  ( 10.00000000000000178, 67.25893115100079456, 9.846743663894594434 ) ) ;
#31541 = DIRECTION ( 'NONE',  ( 0.000000000000000000, -1.000000000000000000, 0.000000000000000000 ) ) ;
#31542 = TOROIDAL_SURFACE ( 'NONE', #92224, 3.750000000000001776, 0.2500000000000000000 ) ;
#31543 = CARTESIAN_POINT ( 'NONE',  ( 3.591859063236761518, 59.95696800326375353, 11.09922568453594849 ) ) ;
#31544 = CARTESIAN_POINT ( 'NONE',  ( 2.917880565312950480, 0.9704155015806342766, -12.26659068614894821 ) ) ;
#31545 = CARTESIAN_POINT ( 'NONE',  ( 24.16423886937410614, 24.51208216824730002, -3.795296366450302550 ) ) ;
#31546 = VECTOR ( 'NONE', #89234, 1000.000000000000000 ) ;
#31547 = DIRECTION ( 'NONE',  ( 1.000000000000000000, 1.049065152435174162E-16, 0.000000000000000000 ) ) ;
#31548 = CARTESIAN_POINT ( 'NONE',  ( 18.72515096720569616, 10.05509018479935968, 6.500000000000001776 ) ) ;
#31549 = CARTESIAN_POINT ( 'NONE',  ( 20.88017736071110519, 20.56368534415484106, 2.639326808657452039E-16 ) ) ;
#31550 = DIRECTION ( 'NONE',  ( -0.000000000000000000, -0.000000000000000000, -1.000000000000000000 ) ) ;
#31551 = ORIENTED_EDGE ( 'NONE', *, *, #64028, .F. ) ;
#31552 = CARTESIAN_POINT ( 'NONE',  ( 2.791683348922240793, 6.633931151000785675, 7.208316651077764092 ) ) ;
#31553 = CARTESIAN_POINT ( 'NONE',  ( 22.81628187352647785, 36.62363466993041783, 6.195893100308588602E-16 ) ) ;
#31554 = CARTESIAN_POINT ( 'NONE',  ( 19.84674366389459266, 28.71726448433411960, -2.638427012816827677 ) ) ;
#31555 = DIRECTION ( 'NONE',  ( -0.4461978131098006117, 0.000000000000000000, -0.8949343616020291048 ) ) ;
#31556 = EDGE_CURVE ( 'NONE', #6459, #10733, #39602, .T. ) ;
#31557 = CARTESIAN_POINT ( 'NONE',  ( 16.40814093676323893, 10.79030133659708923, 11.09922568453595026 ) ) ;
#31558 = PLANE ( 'NONE',  #68137 ) ;
#31559 = AXIS2_PLACEMENT_3D ( 'NONE', #95070, #81059, #65051 ) ;
#31560 = CARTESIAN_POINT ( 'NONE',  ( 0.1532563361054082862, 6.217264484334118713, 2.638427012816831674 ) ) ;
#31561 = ORIENTED_EDGE ( 'NONE', *, *, #56250, .T. ) ;
#31562 = ORIENTED_EDGE ( 'NONE', *, *, #34474, .T. ) ;
#31563 = CARTESIAN_POINT ( 'NONE',  ( 4.559911319644449179, 28.89701867748817321, 9.422509992056141925 ) ) ;
#31564 = CARTESIAN_POINT ( 'NONE',  ( 17.08211943468705840, 30.13708216824730357, -12.26659068614894466 ) ) ;
#31565 = CARTESIAN_POINT ( 'NONE',  ( 1.472469842513823179, 41.42559781766745886, 4.923371831947296329 ) ) ;
#31566 = CARTESIAN_POINT ( 'NONE',  ( 0.5774900079438607392, 68.48035201082150536, 5.440088680355550821 ) ) ;
#31568 = CARTESIAN_POINT ( 'NONE',  ( -6.841090228438033272, -58.65898919720570603, -2.750000000000000444 ) ) ;
#31567 = CARTESIAN_POINT ( 'NONE',  ( 22.81628187352647785, 56.41530133659708213, 3.434112377981063169 ) ) ;
#31569 = CARTESIAN_POINT ( 'NONE',  ( 12.91533473730993009, 26.60535201082150536, -10.88017736071109987 ) ) ;
#31570 = PRESENTATION_STYLE_ASSIGNMENT (( #92570 ) ) ;
#31571 = CARTESIAN_POINT ( 'NONE',  ( 6.565887622018943937, 3.081968003263753531, -12.81628187352647608 ) ) ;
#31572 = CARTESIAN_POINT ( 'NONE',  ( 5.076628168052703671, 36.84226448433412315, 8.527530157486179263 ) ) ;
#31573 = B_SPLINE_CURVE_WITH_KNOTS ( 'NONE', 3,
 ( #73131, #58126, #13631, #58637, #89137, #95659 ),
 .UNSPECIFIED., .F., .F.,
 ( 4, 2, 4 ),
 ( 0.0002800075630785946873, 0.0006862128664728985939, 0.001092418169867202500 ),
 .UNSPECIFIED. ) ;
#31574 = CARTESIAN_POINT ( 'NONE',  ( 5.440088680355549045, 1.397018677488176541, -9.422509992056141925 ) ) ;
#31575 = CARTESIAN_POINT ( 'NONE',  ( 3.591859063236761518, 49.95696800326375353, 11.09922568453594849 ) ) ;
#31576 = LINE ( 'NONE', #8595, #77128 ) ;
#31578 = CARTESIAN_POINT ( 'NONE',  ( 66.76470751278411342, 40.99999999999997868, 9.500000000000000000 ) ) ;
#31577 = CARTESIAN_POINT ( 'NONE',  ( 20.88017736071110875, 55.77201867748816966, -2.915334737309920765 ) ) ;
#31579 = VECTOR ( 'NONE', #47683, 1000.000000000000000 ) ;
#31580 = DIRECTION ( 'NONE',  ( 1.000000000000000000, 1.257402221000611116E-16, -0.000000000000000000 ) ) ;
#31581 = VECTOR ( 'NONE', #42700, 1000.000000000000000 ) ;
#31582 = CARTESIAN_POINT ( 'NONE',  ( 20.88017736071110164, 60.35535201082151957, 2.915334737309930979 ) ) ;
#31583 = CARTESIAN_POINT ( 'NONE',  ( 19.42250999205614193, 60.14701867748817676, 5.440088680355555262 ) ) ;
#31584 = CARTESIAN_POINT ( 'NONE',  ( -6.898461952320240620, 15.00000000000000000, -12.75387089053316636 ) ) ;
#31585 = PLANE ( 'NONE',  #42803 ) ;
#31586 = CARTESIAN_POINT ( 'NONE',  ( -0.8801773607111009756, 8.063685344154837509, 1.068504757029289695E-15 ) ) ;
#31587 = CARTESIAN_POINT ( 'NONE',  ( 17.20831665107776587, 54.13393115100079456, -7.208316651077762316 ) ) ;
#31589 = DIRECTION ( 'NONE',  ( -1.000000000000000000, 0.000000000000000000, 0.000000000000000000 ) ) ;
#31588 = CARTESIAN_POINT ( 'NONE',  ( 7.084665262690076126, 27.02201867748817676, -10.88017736071110164 ) ) ;
#31590 = CARTESIAN_POINT ( 'NONE',  ( 13.43411237798105340, 30.58196800326374998, 12.81628187352647963 ) ) ;
#31591 = ORIENTED_EDGE ( 'NONE', *, *, #86174, .F. ) ;
#31592 = CARTESIAN_POINT ( 'NONE',  ( -0.8801773607111008646, 43.27201867748817676, 2.915334737309923430 ) ) ;
#31594 = DIRECTION ( 'NONE',  ( -0.000000000000000000, -0.000000000000000000, 1.000000000000000000 ) ) ;
#31593 = CARTESIAN_POINT ( 'NONE',  ( -1.099225684535947600, 8.706968003263753531, -6.408140936763238038 ) ) ;
#31595 = CARTESIAN_POINT ( 'NONE',  ( 17.96484262340118221, 9.938685344154837509, 7.964842623401181321 ) ) ;
#31596 = CARTESIAN_POINT ( 'NONE',  ( 20.88017736071110519, 35.56368534415484106, 2.639326808657452039E-16 ) ) ;
#31597 = CARTESIAN_POINT ( 'NONE',  ( 6.204703633549690345, 35.76208216824729647, -14.16423886937410259 ) ) ;
#31598 = CARTESIAN_POINT ( 'NONE',  ( 19.84674366389459621, 23.50893115100078390, 7.409399052514197653E-17 ) ) ;
#31599 = CARTESIAN_POINT ( 'NONE',  ( 15.44008868035555260, 64.73035201082151957, 9.422509992056143702 ) ) ;
#31600 = CARTESIAN_POINT ( 'NONE',  ( 1.274849032794324932, 32.55509018479936145, -6.500000000000021316 ) ) ;
#31601 = CARTESIAN_POINT ( 'NONE',  ( 2.917880565312948704, 17.63708216824730357, 12.26659068614894643 ) ) ;
#31602 = EDGE_CURVE ( 'NONE', #59678, #62057, #80888, .T. ) ;
#31603 = FILL_AREA_STYLE ('',( #93094 ) ) ;
#31604 = CARTESIAN_POINT ( 'NONE',  ( 7.361572987183169658, 59.96726448433410894, -9.846743663894592657 ) ) ;
#31606 = ORIENTED_EDGE ( 'NONE', *, *, #67066, .F. ) ;
#31605 = EDGE_CURVE ( 'NONE', #11363, #95826, #10832, .T. ) ;
#31607 = ORIENTED_EDGE ( 'NONE', *, *, #16116, .F. ) ;
#31608 = CARTESIAN_POINT ( 'NONE',  ( 22.26659068614895176, 29.72041550158063572, -7.082119434687042414 ) ) ;
#31609 = CARTESIAN_POINT ( 'NONE',  ( 2.917880565312948704, 32.63708216824730357, 12.26659068614894643 ) ) ;
#31610 = CARTESIAN_POINT ( 'NONE',  ( 0.1532563361054100626, 5.800597817667452638, -2.638427012816831230 ) ) ;
#31611 = CARTESIAN_POINT ( 'NONE',  ( -2.816281873526473856, 9.331968003263753531, 3.434112377981055619 ) ) ;
#31612 = CARTESIAN_POINT ( 'NONE',  ( 1.472469842513823179, 65.59226448433412315, -4.923371831947296329 ) ) ;
#31613 = CARTESIAN_POINT ( 'NONE',  ( -9.793382739396090386, -28.00152668697614189, 3.750000000000000000 ) ) ;
#31615 = CARTESIAN_POINT ( 'NONE',  ( -2.816281873526473856, 19.33196800326375708, 3.434112377981055619 ) ) ;
#31614 = CARTESIAN_POINT ( 'NONE',  ( 17.96484262340118221, 66.18868534415483396, -7.964842623401177768 ) ) ;
#31616 = CARTESIAN_POINT ( 'NONE',  ( -2.266590686148945544, 31.38708216824730002, -7.082119434687050408 ) ) ;
#31617 = CARTESIAN_POINT ( 'NONE',  ( -0.8801773607111009756, 33.06368534415484106, 1.068504757029289695E-15 ) ) ;
#31618 = EDGE_CURVE ( 'NONE', #44682, #1372, #81375, .T. ) ;
#31619 = CARTESIAN_POINT ( 'NONE',  ( 15.44008868035555260, 29.73035201082150891, 9.422509992056143702 ) ) ;
#31620 = CARTESIAN_POINT ( 'NONE',  ( 21.92686044187657401, 5.370456701841137992, -3.195792623639525765 ) ) ;
#31621 = CARTESIAN_POINT ( 'NONE',  ( -0.8801773607110991993, 57.85535201082149825, -2.915334737309923874 ) ) ;
#31622 = CARTESIAN_POINT ( 'NONE',  ( 9.846743663894594434, -6.491068848999207219, -2.168404344971008868E-15 ) ) ;
#31623 = ORIENTED_EDGE ( 'NONE', *, *, #90876, .F. ) ;
#31624 = LINE ( 'NONE', #93114, #69917 ) ;
#31625 = ORIENTED_EDGE ( 'NONE', *, *, #20709, .T. ) ;
#31626 = DIRECTION ( 'NONE',  ( -0.000000000000000000, -1.000000000000000000, -0.000000000000000000 ) ) ;
#31627 = ORIENTED_EDGE ( 'NONE', *, *, #90184, .F. ) ;
#31628 = CARTESIAN_POINT ( 'NONE',  ( -0.3689425029237881626, 2.428748834913967869, 10.36894250292379027 ) ) ;
#31630 = CARTESIAN_POINT ( 'NONE',  ( 24.16423886937410614, 59.51208216824728936, -3.795296366450302550 ) ) ;
#31629 = CARTESIAN_POINT ( 'NONE',  ( 10.00000000000000000, 60.55374883491397497, -14.16423886937410082 ) ) ;
#31632 = CARTESIAN_POINT ( 'NONE',  ( 2.791683348922240793, 66.63393115100079456, 7.208316651077764092 ) ) ;
#31631 = CARTESIAN_POINT ( 'NONE',  ( 5.076628168052704559, 40.17559781766745175, -8.527530157486179263 ) ) ;
#31633 = EDGE_CURVE ( 'NONE', #90793, #83574, #43370, .T. ) ;
#31634 = CYLINDRICAL_SURFACE ( 'NONE', #40690, 0.2500000000000002220 ) ;
#31635 = CARTESIAN_POINT ( 'NONE',  ( 10.00000000000000178, 10.37363466993041961, 12.81628187352647608 ) ) ;
#31636 = VERTEX_POINT ( 'NONE', #16336 ) ;
#31637 = CARTESIAN_POINT ( 'NONE',  ( 20.36894250292379382, 43.67874883491397497, 10.36894250292379205 ) ) ;
#31638 = EDGE_CURVE ( 'NONE', #15080, #14929, #73046, .T. ) ;
#31639 = CARTESIAN_POINT ( 'NONE',  ( 10.00000000000000000, 45.55374883491397497, -14.16423886937410082 ) ) ;
#31640 = ORIENTED_EDGE ( 'NONE', *, *, #8766, .F. ) ;
#31641 = CARTESIAN_POINT ( 'NONE',  ( 20.88017736071110875, 20.77201867748816611, -2.915334737309920765 ) ) ;
#31642 = CARTESIAN_POINT ( 'NONE',  ( 10.00000000000000000, 57.87363466993042493, -12.81628187352647608 ) ) ;
#31643 = VECTOR ( 'NONE', #4598, 1000.000000000000000 ) ;
#31644 = CARTESIAN_POINT ( 'NONE',  ( 12.91533473730992121, 24.52201867748816966, 10.88017736071110164 ) ) ;
#31645 = CARTESIAN_POINT ( 'NONE',  ( 19.84674366389459266, 53.71726448433411605, -2.638427012816827677 ) ) ;
#31646 = CARTESIAN_POINT ( 'NONE',  ( 0.5774900079438590739, 37.64701867748817676, -5.440088680355550821 ) ) ;
#31647 = CARTESIAN_POINT ( 'NONE',  ( -1.926860441876562025, 64.47997603579416648, -3.195792623639529761 ) ) ;
#31648 = CARTESIAN_POINT ( 'NONE',  ( 0.1532563361054100626, 50.80059781766745175, -2.638427012816831230 ) ) ;
#31649 = DIRECTION ( 'NONE',  ( -1.000000000000000000, 0.000000000000000000, 0.000000000000000000 ) ) ;
#31650 = CARTESIAN_POINT ( 'NONE',  ( 10.00000000000000000, 31.81368534415483751, -10.88017736071110342 ) ) ;
#31651 = VECTOR ( 'NONE', #20301, 1000.000000000000000 ) ;
#31652 = EDGE_CURVE ( 'NONE', #50813, #68545, #14876, .T. ) ;
#31653 = CIRCLE ( 'NONE', #44435, 14.49999999999999822 ) ;
#31655 = ORIENTED_EDGE ( 'NONE', *, *, #73462, .T. ) ;
#31654 = CARTESIAN_POINT ( 'NONE',  ( -0.1503990784575247319, 37.22266099184918176, -6.262539305110083276 ) ) ;
#31656 = CARTESIAN_POINT ( 'NONE',  ( 7.361572987183170547, 2.050597817667451750, 9.846743663894590881 ) ) ;
#31657 = CARTESIAN_POINT ( 'NONE',  ( -4.010449548135202491, -13.83555390988819767, 2.500000000000001332 ) ) ;
#31658 = ORIENTED_EDGE ( 'NONE', *, *, #37056, .F. ) ;
#31659 = CARTESIAN_POINT ( 'NONE',  ( 8.742110228303776154, -4.148858702909789642, 4.000000000000000000 ) ) ;
#31660 = CARTESIAN_POINT ( 'NONE',  ( 1.472469842513823179, 35.59226448433412315, -4.923371831947296329 ) ) ;
#31661 = CARTESIAN_POINT ( 'NONE',  ( 0.9940297508537879745, 15.00000000000000000, -14.21528771620249820 ) ) ;
#31662 = CARTESIAN_POINT ( 'NONE',  ( -45.94000000000000483, 92.50000000000000000, 9.000000000000000000 ) ) ;
#31663 = ORIENTED_EDGE ( 'NONE', *, *, #91354, .T. ) ;
#31664 = DIRECTION ( 'NONE',  ( 1.000000000000000000, 0.000000000000000000, -0.000000000000000000 ) ) ;
#31665 = DIRECTION ( 'NONE',  ( 0.000000000000000000, 0.000000000000000000, 1.000000000000000000 ) ) ;
#31666 = CARTESIAN_POINT ( 'NONE',  ( 0.1532563361054083140, 51.00893115100078745, 1.131784320476157264E-15 ) ) ;
#31667 = CARTESIAN_POINT ( 'NONE',  ( 2.917880565312948704, 52.63708216824730357, 12.26659068614894643 ) ) ;
#31668 = CARTESIAN_POINT ( 'NONE',  ( 18.52753015748618282, 53.92559781766745175, -4.923371831947291888 ) ) ;
#31669 = FACE_OUTER_BOUND ( 'NONE', #11997, .T. ) ;
#31670 = CARTESIAN_POINT ( 'NONE',  ( 18.52753015748617571, 18.09226448433411960, 4.923371831947298993 ) ) ;
#31671 = CARTESIAN_POINT ( 'NONE',  ( 16.40814093676323893, 50.79030133659708923, 11.09922568453595026 ) ) ;
#31672 = CARTESIAN_POINT ( 'NONE',  ( 0.1532563361054100626, 55.80059781766745175, -2.638427012816831230 ) ) ;
#31673 = CARTESIAN_POINT ( 'NONE',  ( 19.42250999205614548, 50.98035201082151247, -5.440088680355545492 ) ) ;
#31674 = CARTESIAN_POINT ( 'NONE',  ( 7.361572987183169658, 49.96726448433410894, -9.846743663894592657 ) ) ;
#31675 = DIRECTION ( 'NONE',  ( 1.000000000000000000, 0.000000000000000000, 0.000000000000000000 ) ) ;
#31676 = CARTESIAN_POINT ( 'NONE',  ( 20.88017736071110875, 55.77201867748816966, -2.915334737309920765 ) ) ;
#31677 = EDGE_LOOP ( 'NONE', ( #3032, #26227, #11016, #50884 ) ) ;
#31678 = DIRECTION ( 'NONE',  ( 0.01646788341559294114, 0.9998643952135761737, 0.000000000000000000 ) ) ;
#31679 = CARTESIAN_POINT ( 'NONE',  ( 7.084665262690076126, 29.10535201082150181, 10.88017736071109987 ) ) ;
#31681 = CARTESIAN_POINT ( 'NONE',  ( 15.44008868035555793, 61.39701867748817676, -9.422509992056140149 ) ) ;
#31680 = CARTESIAN_POINT ( 'NONE',  ( 0.6178305044545838731, 19.74863466993042138, 9.382169495545420901 ) ) ;
#31682 = CARTESIAN_POINT ( 'NONE',  ( 19.42250999205614193, 65.14701867748817676, 5.440088680355555262 ) ) ;
#31683 = CARTESIAN_POINT ( 'NONE',  ( 18.52753015748617571, 13.09226448433411960, 4.923371831947298993 ) ) ;
#31684 = CARTESIAN_POINT ( 'NONE',  ( 0.4195498155886419056, 0.4999999999999970579, -9.500000000000000000 ) ) ;
#31686 = CARTESIAN_POINT ( 'NONE',  ( -0.03743638938522819704, 54.25197528031017669, -6.399506433553964868 ) ) ;
#31685 = CARTESIAN_POINT ( 'NONE',  ( 12.91533473730993009, 56.60535201082151247, -10.88017736071109987 ) ) ;
#31687 = EDGE_CURVE ( 'NONE', #36285, #20560, #93571, .T. ) ;
#31688 = VECTOR ( 'NONE', #77331, 1000.000000000000000 ) ;
#31689 = CARTESIAN_POINT ( 'NONE',  ( 2.791683348922237240, 35.38393115100079456, -7.208316651077763204 ) ) ;
#31690 = CARTESIAN_POINT ( 'NONE',  ( 5.076628168052704559, 5.175597817667451750, -8.527530157486179263 ) ) ;
#31691 = CARTESIAN_POINT ( 'NONE',  ( -2.915334737309934532, -32.97798132251182324, -10.88017736071109987 ) ) ;
#31692 = CARTESIAN_POINT ( 'NONE',  ( -1.099225684535947600, 14.54030133659708568, 6.408140936763237150 ) ) ;
#31693 = CARTESIAN_POINT ( 'NONE',  ( 10.00000000000000178, 9.313685344154839285, 10.88017736071110342 ) ) ;
#31694 = FACE_OUTER_BOUND ( 'NONE', #59181, .T. ) ;
#31695 = EDGE_CURVE ( 'NONE', #54251, #51712, #61330, .T. ) ;
#31696 = CARTESIAN_POINT ( 'NONE',  ( 22.26659068614894466, 28.88708216824730357, 7.082119434687054849 ) ) ;
#31697 = CARTESIAN_POINT ( 'NONE',  ( 10.00000000000000000, 60.55374883491397497, -14.16423886937410082 ) ) ;
#31698 = CARTESIAN_POINT ( 'NONE',  ( 0.1532563361054100626, 35.80059781766745175, -2.638427012816831230 ) ) ;
#31699 = CARTESIAN_POINT ( 'NONE',  ( 17.20831665107776587, 24.13393115100078035, -7.208316651077762316 ) ) ;
#31700 = CARTESIAN_POINT ( 'NONE',  ( 10.00000000000000178, 14.31368534415483751, 10.88017736071110342 ) ) ;
#31701 = VERTEX_POINT ( 'NONE', #75849 ) ;
#31702 = CARTESIAN_POINT ( 'NONE',  ( 14.92337183194729988, 34.34226448433411605, -8.527530157486177487 ) ) ;
#31703 = CARTESIAN_POINT ( 'NONE',  ( 0.5774900079438607392, 23.48035201082150536, 5.440088680355550821 ) ) ;
#31704 = CARTESIAN_POINT ( 'NONE',  ( 18.52753015748617571, 63.09226448433412315, 4.923371831947298993 ) ) ;
#31706 = DIRECTION ( 'NONE',  ( -0.000000000000000000, -0.000000000000000000, -1.000000000000000000 ) ) ;
#31705 = CARTESIAN_POINT ( 'NONE',  ( -4.164238869374098151, 1.595415501580634388, -3.795296366450310543 ) ) ;
#31707 = CARTESIAN_POINT ( 'NONE',  ( 6.689969769698871360, 0.000000000000000000, 12.58200319823975022 ) ) ;
#31708 = CARTESIAN_POINT ( 'NONE',  ( 0.1532563361054083140, 11.00893115100078568, 1.131784320476157264E-15 ) ) ;
#31709 = CARTESIAN_POINT ( 'NONE',  ( -2.816281873526473856, 39.12363466993041783, 9.499525473075851096E-16 ) ) ;
#31710 = CARTESIAN_POINT ( 'NONE',  ( 0.1532563361054082862, 61.21726448433412315, 2.638427012816831674 ) ) ;
#31711 = ORIENTED_EDGE ( 'NONE', *, *, #83558, .F. ) ;
#31712 = CARTESIAN_POINT ( 'NONE',  ( 10.00000000000000000, 19.75893115100078390, -9.846743663894594434 ) ) ;
#31713 = CARTESIAN_POINT ( 'NONE',  ( 8.630000000000000782, 1.019547802438459216, -4.000000000000000000 ) ) ;
#31714 = CARTESIAN_POINT ( 'NONE',  ( -46.48928645636213730, 103.2957187381727238, -6.397878122524045530 ) ) ;
#31715 = CARTESIAN_POINT ( 'NONE',  ( -2.266590686148945544, 52.22041550158064638, 7.082119434687048631 ) ) ;
#31716 = CARTESIAN_POINT ( 'NONE',  ( -0.8801773607110991993, 52.85535201082151247, -2.915334737309923874 ) ) ;
#31717 = CARTESIAN_POINT ( 'NONE',  ( 13.79529636645030344, 3.262082168247301350, 14.16423886937410614 ) ) ;
#31718 = CARTESIAN_POINT ( 'NONE',  ( 15.44008868035555793, 61.39701867748817676, -9.422509992056140149 ) ) ;
#31719 = CARTESIAN_POINT ( 'NONE',  ( 10.00000000000000178, 42.25893115100078745, 9.846743663894594434 ) ) ;
#31720 = CARTESIAN_POINT ( 'NONE',  ( 17.96484262340118221, 24.93868534415484461, 7.964842623401181321 ) ) ;
#31721 = CARTESIAN_POINT ( 'NONE',  ( 2.791683348922240793, 46.63393115100077324, 7.208316651077764092 ) ) ;
#31722 = CARTESIAN_POINT ( 'NONE',  ( -0.8801773607111009756, 43.06368534415484106, 1.068504757029289695E-15 ) ) ;
#31723 = VECTOR ( 'NONE', #55867, 1000.000000000000000 ) ;
#31724 = DIRECTION ( 'NONE',  ( 0.000000000000000000, -0.000000000000000000, 1.000000000000000000 ) ) ;
#31725 = TOROIDAL_SURFACE ( 'NONE', #49281, 14.49999999999999822, 0.5000000000000000000 ) ;
#31727 = ORIENTED_EDGE ( 'NONE', *, *, #78519, .T. ) ;
#31726 = EDGE_CURVE ( 'NONE', #56575, #13765, #9178, .T. ) ;
#31728 = EDGE_LOOP ( 'NONE', ( #19214, #11349, #3511, #74790, #60299, #65876 ) ) ;
#31729 = DIRECTION ( 'NONE',  ( 0.000000000000000000, 0.000000000000000000, 1.000000000000000000 ) ) ;
#31730 = CARTESIAN_POINT ( 'NONE',  ( 17.08211943468705130, 3.470415501580634388, 12.26659068614894998 ) ) ;
#31731 = CARTESIAN_POINT ( 'NONE',  ( 17.20831665107776587, 47.88393115100078745, 7.208316651077764980 ) ) ;
#31732 = CARTESIAN_POINT ( 'NONE',  ( 5.076628168052703671, 21.84226448433411960, 8.527530157486179263 ) ) ;
#31733 = CARTESIAN_POINT ( 'NONE',  ( 3.591859063236761518, 59.95696800326375353, 11.09922568453594849 ) ) ;
#31735 = CARTESIAN_POINT ( 'NONE',  ( 7.361572987183169658, 54.96726448433413026, -9.846743663894592657 ) ) ;
#31734 = CARTESIAN_POINT ( 'NONE',  ( 12.91533473730993009, 16.60535201082150891, -10.88017736071109987 ) ) ;
#31736 = DIRECTION ( 'NONE',  ( -0.9996573249755573709, 0.000000000000000000, 0.02617694830786938473 ) ) ;
#31737 = CARTESIAN_POINT ( 'NONE',  ( 17.08211943468705840, 45.13708216824730357, -12.26659068614894466 ) ) ;
#31738 = EDGE_CURVE ( 'NONE', #41155, #91322, #85848, .T. ) ;
#31739 = CARTESIAN_POINT ( 'NONE',  ( 2.917880565312948704, 57.63708216824731068, 12.26659068614894643 ) ) ;
#31740 = CARTESIAN_POINT ( 'NONE',  ( 1.274849032794292736, 67.55509018479936856, -6.499999999999977796 ) ) ;
#31741 = DIRECTION ( 'NONE',  ( -0.000000000000000000, -1.000000000000000000, -0.000000000000000000 ) ) ;
#31742 = CARTESIAN_POINT ( 'NONE',  ( 7.084665262690076126, 52.02201867748816255, -10.88017736071110164 ) ) ;
#31743 = CARTESIAN_POINT ( 'NONE',  ( 1.472469842513823179, 21.42559781766745175, 4.923371831947296329 ) ) ;
#31744 = CARTESIAN_POINT ( 'NONE',  ( -5.811454672275934819, -36.11427488548928011, 4.000000000000000000 ) ) ;
#31745 = ORIENTED_EDGE ( 'NONE', *, *, #24698, .F. ) ;
#31746 = CARTESIAN_POINT ( 'NONE',  ( -1.354709868695410657, 0.5000000000000004441, -14.93870011653153362 ) ) ;
#31747 =( BOUNDED_SURFACE ( )  B_SPLINE_SURFACE ( 1, 2, ( 
 ( #94875, #3394, #24927, #78893, #18396, #16926, #47894, #26376, #87376, #85913, #9918, #56875, #1448, #40421, #31899, #54900, #85415, #80372, #58840, #88363, #97360, #5852, #19858, #50352, #36343, #66336, #96376, #66839, #12361, #27848, #89832, #27359, #59329, #88854, #80863, #58335, #96873, #42378, #42867, #73351, #4876, #28350, #20362, #65350, #11872, #79874, #35354, #28829, #65846, #50857, #12846, #81350, #73843, #43345, #11378, #72360, #5372, #20857, #89347, #51348, #72854, #41898, #81832, #13347, #34360, #34856, #95878, #43831, #74327, #3892, #64851, #95370, #26869, #57365, #87860, #7344, #69314, #13848, #31296, #52819, #61305, #37844, #14346, #53817, #53314, #21852, #22839, #59820, #98856, #68335, #83327, #14853, #52332, #38334, #68827, #90314, #30310, #74831, #358, #836, #15347, #30807, #6335, #45831, #82826, #45325, #29818, #75822, #75324, #37351, #84329, #98360, #60327, #91816, #23337, #90817, #60811, #22347, #61796, #91310, #76317, #92304, #15829, #67335, #76802, #8319, #38823, #51840, #82327, #97860, #85793, #88110, #25303, #65102, #80118, #47783, #87617, #84809, #32772, #70307, #65598, #27112, #19130, #8803, #40294, #11626, #42142, #2319, #4636, #95623, #54294, #57611, #47282, #19619, #50113, #80623, #12117, #62285, #42619, #70802, #16315, #77291, #1335, #92789, #93283, #54784, #85300, #39806, #1823, #24807, #55284, #52579, #88599, #75581, #51103, #28599, #37102, #98106, #89597, #37595, #51605, #74590, #29568, #96126, #96623, #36609, #67096, #50613, #43106, #35608, #73593, #66094, #29084, #21609, #34204, #81558, #36065, #97094, #90050, #51569, #57209, #41746, #71735, #43557, #98077, #28565, #74054, #6072, #89564, #67061, #82055, #52547, #64211, #66566, #14073, #19220, #13564, #64695, #29536, #74555, #36572, #56727, #72215, #3746, #60042, #87218, #97586, #90539, #21573, #79726, #49224, #29046, #59555, #82556, #11226, #44553, #75048, #6557, #87705, #95207, #37067, #67565, #22072, #14571, #3245, #33712, #94727, #18741, #26712, #49702, #76531, #39533, #75547, #91034, #7571, #62011, #98585, #38546, #23556, #84536, #47012, #85022, #62501, #77022, #61516, #76038, #84040, #45540, #69041, #24538, #15071, #575, #15561, #9015, #30033, #91541, #39037, #83549, #54025, #7063, #69531, #92511, #70025, #68550, #23058, #1549, #31994, #81, #16033, #31020, #53033, #53527, #93004, #54998, #46046, #92026, #85516, #60542, #30528, #54509, #22564, #61029, #46522, #8536, #1045, #31512, #41993, #93996, #86510, #72457, #3500, #33470, #3990, #48487, #63966, #57464, #63494, #95475, #25997, #25519, #56492, #86981, #3021, #78989, #10495 ),
 ( #10988, #64462, #11476, #47992, #56007, #34455, #18986, #78503, #18491, #41007, #55514, #18006, #17027, #47506, #71508, #48979, #87472, #49464, #10016, #26470, #9514, #40014, #86013, #94968, #79488, #78007, #2040, #41508, #33957, #32501, #56969, #79970, #62999, #93503, #17526, #40517, #71014, #2536, #32990, #65946, #5471, #36447, #50451, #96473, #20460, #12946, #66939, #66439, #73444, #57949, #87957, #58437, #13954, #35943, #27945, #20959, #28447, #13442, #58944, #67441, #80468, #88952, #89931, #50950, #81445, #80958, #44428, #89445, #51446, #72954, #88456, #12457, #74932, #34950, #43929, #6432, #21447, #95973, #42963, #74427, #51944, #82429, #4970, #29416, #11967, #91905, #45413, #29912, #61887, #53909, #92392, #77380, #8893, #91412, #46406, #39409, #925, #69903, #22938, #54386, #59921, #6938, #22441, #8409, #14446, #53406, #38424, #450, #31387, #23917, #1423, #23430, #76412, #52913, #16411, #90409, #15443, #46889, #21951, #37445, #14944, #38916, #44916, #45923, #68922, #61395, #52430, #82928, #75424, #84418, #7927, #75918, #98951, #37939, #15915, #67936, #68429, #69404, #30407, #98456, #60910, #9894, #86868, #1915, #40884, #92879, #18376, #79364, #26352, #62879, #40398, #79850, #64341, #24904, #48855, #41393, #32374, #70893, #31875, #85390, #93871, #25398, #3372, #16903, #55387, #17402, #95346, #26844, #42354, #81806, #42842, #21328, #59309, #73326, #4851, #89807, #58816, #50835, #51817, #35326, #81328, #13825, #50325, #82303, #12823, #65820, #43322, #20833, #65325, #27825, #58311, #88827, #51322, #5349, #88339, #72829, #34332, #28325, #44306, #13325, #43809, #74304, #5829, #36323, #66816, #64828, #57340, #97338, #19352, #49836, #80348, #95850, #11845, #4367, #27333, #57830, #19836, #70282, #3254, #54758, #85773, #64221, #25767, #93259, #24783, #40270, #48249, #56261, #17283, #10267, #86754, #18259, #47760, #78258, #48736, #79242, #10755, #94737, #56736, #46773, #35708, #36204, #96230, #4242, #87718, #18752, #88212, #43698, #35200, #57712, #50718, #65704, #12711, #27709, #97230, #11235, #19720, #58700, #65207, #27211, #11727, #74185, #88704, #50209, #72225, #19232, #49713, #5716, #3755, #80720, #66702, #66196, #26725, #95218, #12216, #42724, #96728, #57220, #58193, #20214, #81211, #34712, #80223, #20717, #43205, #51208, #28697, #59189, #73696, #28204, #49236, #89204, #79738, #81692, #13205, #41755, #42240, #72706, #95727, #13700, #67701, #83183, #45182, #15197, #83682, #209, #37697, #22203, #59685, #6695, #29187, #98213, #61166, #97724, #60180, #37213, #45679, #44185, #44687, #68195, #67198, #14708, #89695, #98716, #53176 ) ),
 .UNSPECIFIED., .F., .F., .F. ) 
 B_SPLINE_SURFACE_WITH_KNOTS ( ( 2, 2 ),
 ( 3, 2, 2, 2, 2, 2, 2, 2, 2, 2, 2, 2, 2, 2, 2, 2, 2, 2, 2, 2, 2, 2, 2, 2, 2, 2, 2, 2, 2, 2, 2, 2, 2, 2, 2, 2, 2, 2, 2, 2, 2, 2, 2, 2, 2, 2, 2, 2, 2, 2, 2, 2, 2, 2, 2, 2, 2, 2, 2, 2, 2, 2, 2, 2, 2, 2, 2, 2, 2, 2, 2, 2, 2, 2, 2, 2, 2, 2, 2, 2, 2, 2, 2, 2, 2, 2, 2, 2, 2, 2, 2, 2, 2, 2, 2, 2, 2, 2, 2, 2, 2, 2, 2, 2, 2, 2, 2, 2, 2, 2, 2, 2, 2, 2, 2, 2, 2, 2, 2, 2, 2, 2, 2, 2, 2, 2, 2, 2, 2, 2, 2, 2, 2, 2, 2, 2, 2, 2, 2, 2, 2, 2, 2, 2, 2, 2, 2, 2, 2, 2, 2, 2, 2, 2, 2, 2, 2, 2, 2, 2, 2, 2, 3 ),
 ( 0.000000000000000000, 1.000000000000000000 ),
 ( 0.000000000000000000, 0.005952380952380952051, 0.01190476190476190410, 0.01785714285714285615, 0.02380952380952380820, 0.02976190476190476025, 0.03571428571428571230, 0.04166666666666666435, 0.04761904761904761640, 0.05357142857142856845, 0.05952380952380952051, 0.06547619047619047949, 0.07142857142857142461, 0.07738095238095238360, 0.08333333333333332871, 0.08928571428571428770, 0.09523809523809523281, 0.1011904761904761918, 0.1071428571428571369, 0.1130952380952380959, 0.1190476190476190410, 0.1250000000000000000, 0.1309523809523809590, 0.1369047619047619180, 0.1428571428571428492, 0.1488095238095238082, 0.1547619047619047672, 0.1607142857142857262, 0.1666666666666666574, 0.1726190476190476164, 0.1785714285714285754, 0.1845238095238095344, 0.1904761904761904656, 0.1964285714285714246, 0.2023809523809523836, 0.2083333333333333426, 0.2142857142857142738, 0.2202380952380952328, 0.2261904761904761918, 0.2321428571428571508, 0.2380952380952380820, 0.2440476190476190410, 0.2500000000000000000, 0.2559523809523809312, 0.2619047619047619180, 0.2678571428571428492, 0.2738095238095238360, 0.2797619047619047672, 0.2857142857142856984, 0.2916666666666666852, 0.2976190476190476164, 0.3035714285714285476, 0.3095238095238095344, 0.3154761904761904656, 0.3214285714285714524, 0.3273809523809523836, 0.3333333333333333148, 0.3392857142857143016, 0.3452380952380952328, 0.3511904761904761640, 0.3571428571428571508, 0.3630952380952380820, 0.3690476190476190688, 0.3750000000000000000, 0.3809523809523809312, 0.3869047619047619180, 0.3928571428571428492, 0.3988095238095238360, 0.4047619047619047672, 0.4107142857142856984, 0.4166666666666666852, 0.4226190476190476164, 0.4285714285714285476, 0.4345238095238095344, 0.4404761904761904656, 0.4464285714285714524, 0.4523809523809523836, 0.4583333333333333148, 0.4642857142857143016, 0.4702380952380952328, 0.4761904761904761640, 0.4821428571428571508, 0.4880952380952380820, 0.4940476190476190688, 0.5000000000000000000, 0.5059523809523809312, 0.5119047619047618625, 0.5178571428571429047, 0.5238095238095238360, 0.5297619047619047672, 0.5357142857142856984, 0.5416666666666666297, 0.5476190476190476719, 0.5535714285714286031, 0.5595238095238095344, 0.5654761904761904656, 0.5714285714285713969, 0.5773809523809523281, 0.5833333333333333703, 0.5892857142857143016, 0.5952380952380952328, 0.6011904761904761640, 0.6071428571428570953, 0.6130952380952381375, 0.6190476190476190688, 0.6250000000000000000, 0.6309523809523809312, 0.6369047619047618625, 0.6428571428571429047, 0.6488095238095238360, 0.6547619047619047672, 0.6607142857142856984, 0.6666666666666666297, 0.6726190476190476719, 0.6785714285714286031, 0.6845238095238095344, 0.6904761904761904656, 0.6964285714285713969, 0.7023809523809523281, 0.7083333333333333703, 0.7142857142857143016, 0.7202380952380952328, 0.7261904761904761640, 0.7321428571428570953, 0.7380952380952381375, 0.7440476190476190688, 0.7500000000000000000, 0.7559523809523809312, 0.7619047619047618625, 0.7678571428571429047, 0.7738095238095238360, 0.7797619047619047672, 0.7857142857142856984, 0.7916666666666666297, 0.7976190476190476719, 0.8035714285714286031, 0.8095238095238095344, 0.8154761904761904656, 0.8214285714285713969, 0.8273809523809523281, 0.8333333333333333703, 0.8392857142857143016, 0.8452380952380952328, 0.8511904761904761640, 0.8571428571428570953, 0.8630952380952381375, 0.8690476190476190688, 0.8750000000000000000, 0.8809523809523809312, 0.8869047619047618625, 0.8928571428571429047, 0.8988095238095238360, 0.9047619047619047672, 0.9107142857142856984, 0.9166666666666666297, 0.9226190476190476719, 0.9285714285714286031, 0.9345238095238095344, 0.9404761904761904656, 0.9464285714285713969, 0.9523809523809523281, 0.9583333333333333703, 0.9642857142857143016 ),
 .UNSPECIFIED. ) 
 GEOMETRIC_REPRESENTATION_ITEM ( )  RATIONAL_B_SPLINE_SURFACE ( (
 ( 1.000000000000000000, 0.9659258262890683122, 1.000000000000000000, 0.9659258262890683122, 1.000000000000000000, 0.9659258262890683122, 1.000000000000000000, 0.9659258262890683122, 1.000000000000000000, 0.9659258262890683122, 1.000000000000000000, 0.9659258262890683122, 1.000000000000000000, 0.9659258262890683122, 1.000000000000000000, 0.9659258262890683122, 1.000000000000000000, 0.9659258262890683122, 1.000000000000000000, 0.9659258262890683122, 1.000000000000000000, 0.9659258262890683122, 1.000000000000000000, 0.9659258262890683122, 1.000000000000000000, 0.9659258262890683122, 1.000000000000000000, 0.9659258262890683122, 1.000000000000000000, 0.9659258262890683122, 1.000000000000000000, 0.9659258262890683122, 1.000000000000000000, 0.9659258262890683122, 1.000000000000000000, 0.9659258262890683122, 1.000000000000000000, 0.9659258262890683122, 1.000000000000000000, 0.9659258262890683122, 1.000000000000000000, 0.9659258262890683122, 1.000000000000000000, 0.9659258262890683122, 1.000000000000000000, 0.9659258262890683122, 1.000000000000000000, 0.9659258262890683122, 1.000000000000000000, 0.9659258262890683122, 1.000000000000000000, 0.9659258262890683122, 1.000000000000000000, 0.9659258262890683122, 1.000000000000000000, 0.9659258262890683122, 1.000000000000000000, 0.9659258262890683122, 1.000000000000000000, 0.9659258262890683122, 1.000000000000000000, 0.9659258262890683122, 1.000000000000000000, 0.9659258262890683122, 1.000000000000000000, 0.9659258262890683122, 1.000000000000000000, 0.9659258262890683122, 1.000000000000000000, 0.9659258262890683122, 1.000000000000000000, 0.9659258262890683122, 1.000000000000000000, 0.9659258262890683122, 1.000000000000000000, 0.9659258262890683122, 1.000000000000000000, 0.9659258262890683122, 1.000000000000000000, 0.9659258262890683122, 1.000000000000000000, 0.9659258262890683122, 1.000000000000000000, 0.9659258262890683122, 1.000000000000000000, 0.9659258262890683122, 1.000000000000000000, 0.9659258262890683122, 1.000000000000000000, 0.9659258262890683122, 1.000000000000000000, 0.9659258262890683122, 1.000000000000000000, 0.9659258262890683122, 1.000000000000000000, 0.9659258262890683122, 1.000000000000000000, 0.9659258262890683122, 1.000000000000000000, 0.9659258262890683122, 1.000000000000000000, 0.9659258262890683122, 1.000000000000000000, 0.9659258262890683122, 1.000000000000000000, 0.9659258262890683122, 1.000000000000000000, 0.9659258262890683122, 1.000000000000000000, 0.9659258262890683122, 1.000000000000000000, 0.9659258262890683122, 1.000000000000000000, 0.9659258262890683122, 1.000000000000000000, 0.9659258262890683122, 1.000000000000000000, 0.9659258262890683122, 1.000000000000000000, 0.9659258262890683122, 1.000000000000000000, 0.9659258262890683122, 1.000000000000000000, 0.9659258262890683122, 1.000000000000000000, 0.9659258262890683122, 1.000000000000000000, 0.9659258262890683122, 1.000000000000000000, 0.9659258262890683122, 1.000000000000000000, 0.9659258262890683122, 1.000000000000000000, 0.9659258262890683122, 1.000000000000000000, 0.9659258262890683122, 1.000000000000000000, 0.9659258262890683122, 1.000000000000000000, 0.9659258262890683122, 1.000000000000000000, 0.9659258262890683122, 1.000000000000000000, 0.9659258262890683122, 1.000000000000000000, 0.9659258262890683122, 1.000000000000000000, 0.9659258262890683122, 1.000000000000000000, 0.9659258262890683122, 1.000000000000000000, 0.9659258262890683122, 1.000000000000000000, 0.9659258262890683122, 1.000000000000000000, 0.9659258262890683122, 1.000000000000000000, 0.9659258262890683122, 1.000000000000000000, 0.9659258262890683122, 1.000000000000000000, 0.9659258262890683122, 1.000000000000000000, 0.9659258262890683122, 1.000000000000000000, 0.9659258262890683122, 1.000000000000000000, 0.9659258262890683122, 1.000000000000000000, 0.9659258262890683122, 1.000000000000000000, 0.9659258262890683122, 1.000000000000000000, 0.9659258262890683122, 1.000000000000000000, 0.9659258262890683122, 1.000000000000000000, 0.9659258262890683122, 1.000000000000000000, 0.9659258262890683122, 1.000000000000000000, 0.9659258262890683122, 1.000000000000000000, 0.9659258262890683122, 1.000000000000000000, 0.9659258262890683122, 1.000000000000000000, 0.9659258262890683122, 1.000000000000000000, 0.9659258262890683122, 1.000000000000000000, 0.9659258262890683122, 1.000000000000000000, 0.9659258262890683122, 1.000000000000000000, 0.9659258262890683122, 1.000000000000000000, 0.9659258262890683122, 1.000000000000000000, 0.9659258262890683122, 1.000000000000000000, 0.9659258262890683122, 1.000000000000000000, 0.9659258262890683122, 1.000000000000000000, 0.9659258262890683122, 1.000000000000000000, 0.9659258262890683122, 1.000000000000000000, 0.9659258262890683122, 1.000000000000000000, 0.9659258262890683122, 1.000000000000000000, 0.9659258262890683122, 1.000000000000000000, 0.9659258262890683122, 1.000000000000000000, 0.9659258262890683122, 1.000000000000000000, 0.9659258262890683122, 1.000000000000000000, 0.9659258262890683122, 1.000000000000000000, 0.9659258262890683122, 1.000000000000000000, 0.9659258262890683122, 1.000000000000000000, 0.9659258262890683122, 1.000000000000000000, 0.9659258262890683122, 1.000000000000000000, 0.9659258262890683122, 1.000000000000000000, 0.9659258262890683122, 1.000000000000000000, 0.9659258262890683122, 1.000000000000000000, 0.9659258262890683122, 1.000000000000000000, 0.9659258262890683122, 1.000000000000000000, 0.9659258262890683122, 1.000000000000000000, 0.9659258262890683122, 1.000000000000000000, 0.9659258262890683122, 1.000000000000000000, 0.9659258262890683122, 1.000000000000000000, 0.9659258262890683122, 1.000000000000000000, 0.9659258262890683122, 1.000000000000000000, 0.9659258262890683122, 1.000000000000000000, 0.9659258262890683122, 1.000000000000000000, 0.9659258262890683122, 1.000000000000000000, 0.9659258262890683122, 1.000000000000000000, 0.9659258262890683122, 1.000000000000000000, 0.9659258262890683122, 1.000000000000000000, 0.9659258262890683122, 1.000000000000000000, 0.9659258262890683122, 1.000000000000000000, 0.9659258262890683122, 1.000000000000000000, 0.9659258262890683122, 1.000000000000000000, 0.9659258262890683122, 1.000000000000000000, 0.9659258262890683122, 1.000000000000000000, 0.9659258262890683122, 1.000000000000000000, 0.9659258262890683122, 1.000000000000000000, 0.9659258262890683122, 1.000000000000000000, 0.9659258262890683122, 1.000000000000000000, 0.9659258262890683122, 1.000000000000000000, 0.9659258262890683122, 1.000000000000000000, 0.9659258262890683122, 1.000000000000000000, 0.9659258262890683122, 1.000000000000000000, 0.9659258262890683122, 1.000000000000000000, 0.9659258262890683122, 1.000000000000000000, 0.9659258262890683122, 1.000000000000000000, 0.9659258262890683122, 1.000000000000000000, 0.9659258262890683122, 1.000000000000000000, 0.9659258262890683122, 1.000000000000000000, 0.9659258262890683122, 1.000000000000000000, 0.9659258262890683122, 1.000000000000000000, 0.9659258262890683122, 1.000000000000000000, 0.9659258262890683122, 1.000000000000000000, 0.9659258262890683122, 1.000000000000000000, 0.9659258262890683122, 1.000000000000000000, 0.9659258262890683122, 1.000000000000000000, 0.9659258262890683122, 1.000000000000000000, 0.9659258262890683122, 1.000000000000000000, 0.9659258262890683122, 1.000000000000000000),
 ( 1.000000000000000000, 0.9659258262890683122, 1.000000000000000000, 0.9659258262890683122, 1.000000000000000000, 0.9659258262890683122, 1.000000000000000000, 0.9659258262890683122, 1.000000000000000000, 0.9659258262890683122, 1.000000000000000000, 0.9659258262890683122, 1.000000000000000000, 0.9659258262890683122, 1.000000000000000000, 0.9659258262890683122, 1.000000000000000000, 0.9659258262890683122, 1.000000000000000000, 0.9659258262890683122, 1.000000000000000000, 0.9659258262890683122, 1.000000000000000000, 0.9659258262890683122, 1.000000000000000000, 0.9659258262890683122, 1.000000000000000000, 0.9659258262890683122, 1.000000000000000000, 0.9659258262890683122, 1.000000000000000000, 0.9659258262890683122, 1.000000000000000000, 0.9659258262890683122, 1.000000000000000000, 0.9659258262890683122, 1.000000000000000000, 0.9659258262890683122, 1.000000000000000000, 0.9659258262890683122, 1.000000000000000000, 0.9659258262890683122, 1.000000000000000000, 0.9659258262890683122, 1.000000000000000000, 0.9659258262890683122, 1.000000000000000000, 0.9659258262890683122, 1.000000000000000000, 0.9659258262890683122, 1.000000000000000000, 0.9659258262890683122, 1.000000000000000000, 0.9659258262890683122, 1.000000000000000000, 0.9659258262890683122, 1.000000000000000000, 0.9659258262890683122, 1.000000000000000000, 0.9659258262890683122, 1.000000000000000000, 0.9659258262890683122, 1.000000000000000000, 0.9659258262890683122, 1.000000000000000000, 0.9659258262890683122, 1.000000000000000000, 0.9659258262890683122, 1.000000000000000000, 0.9659258262890683122, 1.000000000000000000, 0.9659258262890683122, 1.000000000000000000, 0.9659258262890683122, 1.000000000000000000, 0.9659258262890683122, 1.000000000000000000, 0.9659258262890683122, 1.000000000000000000, 0.9659258262890683122, 1.000000000000000000, 0.9659258262890683122, 1.000000000000000000, 0.9659258262890683122, 1.000000000000000000, 0.9659258262890683122, 1.000000000000000000, 0.9659258262890683122, 1.000000000000000000, 0.9659258262890683122, 1.000000000000000000, 0.9659258262890683122, 1.000000000000000000, 0.9659258262890683122, 1.000000000000000000, 0.9659258262890683122, 1.000000000000000000, 0.9659258262890683122, 1.000000000000000000, 0.9659258262890683122, 1.000000000000000000, 0.9659258262890683122, 1.000000000000000000, 0.9659258262890683122, 1.000000000000000000, 0.9659258262890683122, 1.000000000000000000, 0.9659258262890683122, 1.000000000000000000, 0.9659258262890683122, 1.000000000000000000, 0.9659258262890683122, 1.000000000000000000, 0.9659258262890683122, 1.000000000000000000, 0.9659258262890683122, 1.000000000000000000, 0.9659258262890683122, 1.000000000000000000, 0.9659258262890683122, 1.000000000000000000, 0.9659258262890683122, 1.000000000000000000, 0.9659258262890683122, 1.000000000000000000, 0.9659258262890683122, 1.000000000000000000, 0.9659258262890683122, 1.000000000000000000, 0.9659258262890683122, 1.000000000000000000, 0.9659258262890683122, 1.000000000000000000, 0.9659258262890683122, 1.000000000000000000, 0.9659258262890683122, 1.000000000000000000, 0.9659258262890683122, 1.000000000000000000, 0.9659258262890683122, 1.000000000000000000, 0.9659258262890683122, 1.000000000000000000, 0.9659258262890683122, 1.000000000000000000, 0.9659258262890683122, 1.000000000000000000, 0.9659258262890683122, 1.000000000000000000, 0.9659258262890683122, 1.000000000000000000, 0.9659258262890683122, 1.000000000000000000, 0.9659258262890683122, 1.000000000000000000, 0.9659258262890683122, 1.000000000000000000, 0.9659258262890683122, 1.000000000000000000, 0.9659258262890683122, 1.000000000000000000, 0.9659258262890683122, 1.000000000000000000, 0.9659258262890683122, 1.000000000000000000, 0.9659258262890683122, 1.000000000000000000, 0.9659258262890683122, 1.000000000000000000, 0.9659258262890683122, 1.000000000000000000, 0.9659258262890683122, 1.000000000000000000, 0.9659258262890683122, 1.000000000000000000, 0.9659258262890683122, 1.000000000000000000, 0.9659258262890683122, 1.000000000000000000, 0.9659258262890683122, 1.000000000000000000, 0.9659258262890683122, 1.000000000000000000, 0.9659258262890683122, 1.000000000000000000, 0.9659258262890683122, 1.000000000000000000, 0.9659258262890683122, 1.000000000000000000, 0.9659258262890683122, 1.000000000000000000, 0.9659258262890683122, 1.000000000000000000, 0.9659258262890683122, 1.000000000000000000, 0.9659258262890683122, 1.000000000000000000, 0.9659258262890683122, 1.000000000000000000, 0.9659258262890683122, 1.000000000000000000, 0.9659258262890683122, 1.000000000000000000, 0.9659258262890683122, 1.000000000000000000, 0.9659258262890683122, 1.000000000000000000, 0.9659258262890683122, 1.000000000000000000, 0.9659258262890683122, 1.000000000000000000, 0.9659258262890683122, 1.000000000000000000, 0.9659258262890683122, 1.000000000000000000, 0.9659258262890683122, 1.000000000000000000, 0.9659258262890683122, 1.000000000000000000, 0.9659258262890683122, 1.000000000000000000, 0.9659258262890683122, 1.000000000000000000, 0.9659258262890683122, 1.000000000000000000, 0.9659258262890683122, 1.000000000000000000, 0.9659258262890683122, 1.000000000000000000, 0.9659258262890683122, 1.000000000000000000, 0.9659258262890683122, 1.000000000000000000, 0.9659258262890683122, 1.000000000000000000, 0.9659258262890683122, 1.000000000000000000, 0.9659258262890683122, 1.000000000000000000, 0.9659258262890683122, 1.000000000000000000, 0.9659258262890683122, 1.000000000000000000, 0.9659258262890683122, 1.000000000000000000, 0.9659258262890683122, 1.000000000000000000, 0.9659258262890683122, 1.000000000000000000, 0.9659258262890683122, 1.000000000000000000, 0.9659258262890683122, 1.000000000000000000, 0.9659258262890683122, 1.000000000000000000, 0.9659258262890683122, 1.000000000000000000, 0.9659258262890683122, 1.000000000000000000, 0.9659258262890683122, 1.000000000000000000, 0.9659258262890683122, 1.000000000000000000, 0.9659258262890683122, 1.000000000000000000, 0.9659258262890683122, 1.000000000000000000, 0.9659258262890683122, 1.000000000000000000, 0.9659258262890683122, 1.000000000000000000, 0.9659258262890683122, 1.000000000000000000, 0.9659258262890683122, 1.000000000000000000, 0.9659258262890683122, 1.000000000000000000, 0.9659258262890683122, 1.000000000000000000, 0.9659258262890683122, 1.000000000000000000, 0.9659258262890683122, 1.000000000000000000, 0.9659258262890683122, 1.000000000000000000, 0.9659258262890683122, 1.000000000000000000, 0.9659258262890683122, 1.000000000000000000, 0.9659258262890683122, 1.000000000000000000, 0.9659258262890683122, 1.000000000000000000, 0.9659258262890683122, 1.000000000000000000, 0.9659258262890683122, 1.000000000000000000, 0.9659258262890683122, 1.000000000000000000, 0.9659258262890683122, 1.000000000000000000, 0.9659258262890683122, 1.000000000000000000, 0.9659258262890683122, 1.000000000000000000, 0.9659258262890683122, 1.000000000000000000, 0.9659258262890683122, 1.000000000000000000, 0.9659258262890683122, 1.000000000000000000, 0.9659258262890683122, 1.000000000000000000, 0.9659258262890683122, 1.000000000000000000, 0.9659258262890683122, 1.000000000000000000, 0.9659258262890683122, 1.000000000000000000, 0.9659258262890683122, 1.000000000000000000, 0.9659258262890683122, 1.000000000000000000, 0.9659258262890683122, 1.000000000000000000) ) ) 
 REPRESENTATION_ITEM ( '' )  SURFACE ( )  );
#31748 = ORIENTED_EDGE ( 'NONE', *, *, #61362, .T. ) ;
#31749 = CARTESIAN_POINT ( 'NONE',  ( 0.1532563361054083140, 16.00893115100078390, 1.131784320476157264E-15 ) ) ;
#31750 = VERTEX_POINT ( 'NONE', #85317 ) ;
#31751 = CARTESIAN_POINT ( 'NONE',  ( 22.26659068614894466, 13.88708216824730179, 7.082119434687054849 ) ) ;
#31752 = CARTESIAN_POINT ( 'NONE',  ( 19.84674366389459621, 18.50893115100078745, 7.409399052514197653E-17 ) ) ;
#31753 = CARTESIAN_POINT ( 'NONE',  ( 12.91533473730992121, 44.52201867748816966, 10.88017736071110164 ) ) ;
#31754 = DIRECTION ( 'NONE',  ( 0.000000000000000000, 0.000000000000000000, -1.000000000000000000 ) ) ;
#31755 = ORIENTED_EDGE ( 'NONE', *, *, #91797, .T. ) ;
#31756 = CARTESIAN_POINT ( 'NONE',  ( 12.91533473730993009, 36.60535201082151247, -10.88017736071109987 ) ) ;
#31757 = ADVANCED_FACE ( 'NONE', ( #91842 ), #77310, .T. ) ;
#31758 = VERTEX_POINT ( 'NONE', #45851 ) ;
#31759 = CARTESIAN_POINT ( 'NONE',  ( 10.00000000000000178, 13.05374883491396787, 14.16423886937410082 ) ) ;
#31760 = ORIENTED_EDGE ( 'NONE', *, *, #36308, .T. ) ;
#31761 = EDGE_CURVE ( 'NONE', #31031, #65562, #90605, .T. ) ;
#31762 = VERTEX_POINT ( 'NONE', #30332 ) ;
#31763 = CARTESIAN_POINT ( 'NONE',  ( 19.38216949554541557, 12.24863466993041961, -9.382169495545420901 ) ) ;
#31764 = CARTESIAN_POINT ( 'NONE',  ( 14.92337183194729988, 14.34226448433411782, -8.527530157486177487 ) ) ;
#31765 = DIRECTION ( 'NONE',  ( -0.000000000000000000, -0.000000000000000000, 1.000000000000000000 ) ) ;
#31766 = CARTESIAN_POINT ( 'NONE',  ( 2.815433093577122126, 0.5000000000000004441, -14.73340885523749932 ) ) ;
#31767 = CARTESIAN_POINT ( 'NONE',  ( 2.791683348922237240, 15.38393115100078212, -7.208316651077763204 ) ) ;
#31768 = CARTESIAN_POINT ( 'NONE',  ( 17.96484262340118221, 36.18868534415484106, -7.964842623401177768 ) ) ;
#31769 = ORIENTED_EDGE ( 'NONE', *, *, #15084, .F. ) ;
#31770 = EDGE_LOOP ( 'NONE', ( #31250, #21570, #30058, #28712 ) ) ;
#31771 = CARTESIAN_POINT ( 'NONE',  ( 3.969999999999999751, 36.75000000000000000, 3.750000000000000000 ) ) ;
#31772 = CARTESIAN_POINT ( 'NONE',  ( -0.8801773607111008646, 58.27201867748816966, 2.915334737309923430 ) ) ;
#31773 = DIRECTION ( 'NONE',  ( -1.000000000000000000, 0.000000000000000000, 0.000000000000000000 ) ) ;
#31774 = CARTESIAN_POINT ( 'NONE',  ( 7.084665262690076126, 62.02201867748816966, -10.88017736071110164 ) ) ;
#31775 = CARTESIAN_POINT ( 'NONE',  ( 16.40814093676324603, 17.45696800326375353, -11.09922568453594671 ) ) ;
#31776 = DIRECTION ( 'NONE',  ( -0.9762960071199316969, 0.000000000000000000, -0.2164396139381103423 ) ) ;
#31777 = CARTESIAN_POINT ( 'NONE',  ( 19.84674366389459266, 33.30059781766744464, 2.638427012816836559 ) ) ;
#31778 = CARTESIAN_POINT ( 'NONE',  ( 6.565887622018943937, 58.08196800326376064, -12.81628187352647608 ) ) ;
#31779 = CARTESIAN_POINT ( 'NONE',  ( 5.679567480639522437, -28.64348288259103725, -3.750000000000000000 ) ) ;
#31780 = CARTESIAN_POINT ( 'NONE',  ( 2.791683348922240793, 21.63393115100078745, 7.208316651077764092 ) ) ;
#31781 = CARTESIAN_POINT ( 'NONE',  ( -2.816281873526473856, 24.33196800326375353, 3.434112377981055619 ) ) ;
#31783 = DIRECTION ( 'NONE',  ( 0.000000000000000000, 0.000000000000000000, -1.000000000000000000 ) ) ;
#31782 = DIRECTION ( 'NONE',  ( 5.782411586589362323E-17, 1.000000000000000000, -0.000000000000000000 ) ) ;
#31784 = CARTESIAN_POINT ( 'NONE',  ( 10.00000000000000000, 46.81368534415484106, -10.88017736071110342 ) ) ;
#31785 = CARTESIAN_POINT ( 'NONE',  ( 18.52753015748617571, 63.09226448433412315, 4.923371831947298993 ) ) ;
#31786 = DIRECTION ( 'NONE',  ( -0.8141155183563145714, 0.000000000000000000, -0.5807029557109463225 ) ) ;
#31787 = CARTESIAN_POINT ( 'NONE',  ( 1.472469842513823179, 26.42559781766745175, 4.923371831947296329 ) ) ;
#31788 = CARTESIAN_POINT ( 'NONE',  ( 20.88017736071110164, 15.35535201082150358, 2.915334737309930979 ) ) ;
#31789 = CARTESIAN_POINT ( 'NONE',  ( 21.09922568453595559, 17.04030133659708923, -6.408140936763230044 ) ) ;
#31790 = STYLED_ITEM ( 'NONE', ( #60682 ), #72135 ) ;
#31791 = SURFACE_SIDE_STYLE ('',( #72252 ) ) ;
#31792 = CARTESIAN_POINT ( 'NONE',  ( -10.94840535726592634, 89.72140148746893829, 6.176821657850954495 ) ) ;
#31793 = CARTESIAN_POINT ( 'NONE',  ( 17.96484262340118221, 26.18868534415483396, -7.964842623401177768 ) ) ;
#31794 = ORIENTED_EDGE ( 'NONE', *, *, #26747, .T. ) ;
#31795 = DIRECTION ( 'NONE',  ( 0.9752498888222641549, -0.2211055276381879986, 3.469446951953568040E-15 ) ) ;
#31797 = CARTESIAN_POINT ( 'NONE',  ( 2.035157376598822676, 17.43868534415483751, -7.964842623401177768 ) ) ;
#31796 = CARTESIAN_POINT ( 'NONE',  ( 19.84674366389459621, 23.50893115100078390, 7.409399052514197653E-17 ) ) ;
#31798 = CARTESIAN_POINT ( 'NONE',  ( 18.72515096720568550, 20.05509018479935790, 6.500000000000015099 ) ) ;
#31799 = CARTESIAN_POINT ( 'NONE',  ( 4.559911319644449179, 33.89701867748817676, 9.422509992056141925 ) ) ;
#31800 = EDGE_CURVE ( 'NONE', #64703, #81191, #54229, .T. ) ;
#31801 = CARTESIAN_POINT ( 'NONE',  ( 20.88017736071110164, 5.355352010821503583, 2.915334737309930979 ) ) ;
#31802 = CARTESIAN_POINT ( 'NONE',  ( 18.52753015748617571, 8.092264484334117824, 4.923371831947298993 ) ) ;
#31803 = CARTESIAN_POINT ( 'NONE',  ( 0.1532563361054083140, 41.00893115100078745, 1.131784320476157264E-15 ) ) ;
#31804 = LINE ( 'NONE', #62302, #36126 ) ;
#31805 = DIRECTION ( 'NONE',  ( 1.000000000000000000, 0.000000000000000000, 0.000000000000000000 ) ) ;
#31806 = ADVANCED_FACE ( 'NONE', ( #98881 ), #60837, .F. ) ;
#31807 = CARTESIAN_POINT ( 'NONE',  ( 7.361572987183169658, 64.96726448433412315, -9.846743663894592657 ) ) ;
#31808 = CARTESIAN_POINT ( 'NONE',  ( 0.000000000000000000, 14.49999999999999822, 0.000000000000000000 ) ) ;
#31809 = CARTESIAN_POINT ( 'NONE',  ( -9.793405416354234561, -28.00185549905096849, -3.750000000000000000 ) ) ;
#31810 = CARTESIAN_POINT ( 'NONE',  ( -2.266590686148945544, 22.22041550158063572, 7.082119434687048631 ) ) ;
#31811 = CARTESIAN_POINT ( 'NONE',  ( 12.63842701281683922, 34.55059781766745886, -9.846743663894590881 ) ) ;
#31812 = CARTESIAN_POINT ( 'NONE',  ( 11.36220558718863138, 4.417444789370043464E-16, -9.008345252845243678 ) ) ;
#31813 = EDGE_LOOP ( 'NONE', ( #97633, #15702, #7040, #61080, #25704, #19582, #62640, #36724 ) ) ;
#31814 = CARTESIAN_POINT ( 'NONE',  ( 20.36894250292379738, 49.92874883491396787, -10.36894250292379027 ) ) ;
#31815 = CARTESIAN_POINT ( 'NONE',  ( 0.1532563361054100626, 25.80059781766744820, -2.638427012816831230 ) ) ;
#31817 = CARTESIAN_POINT ( 'NONE',  ( 12.74414838903271452, 15.00000000000000888, 7.178093659842060603 ) ) ;
#31816 = CARTESIAN_POINT ( 'NONE',  ( 20.00000000000000000, 0.000000000000000000, -4.500000000000001776 ) ) ;
#31818 = CARTESIAN_POINT ( 'NONE',  ( 10.00000000000000000, 51.81368534415484106, -10.88017736071110342 ) ) ;
#31819 = CARTESIAN_POINT ( 'NONE',  ( 16.40814093676324603, 47.45696800326375353, -11.09922568453594671 ) ) ;
#31820 = CARTESIAN_POINT ( 'NONE',  ( 2.035157376598822676, 12.43868534415483751, -7.964842623401177768 ) ) ;
#31822 = VERTEX_POINT ( 'NONE', #15852 ) ;
#31821 = CARTESIAN_POINT ( 'NONE',  ( -1.099225684535947600, 53.70696800326376064, -6.408140936763238038 ) ) ;
#31823 = CARTESIAN_POINT ( 'NONE',  ( 7.361572987183169658, 64.96726448433412315, -9.846743663894592657 ) ) ;
#31824 = CARTESIAN_POINT ( 'NONE',  ( 7.361572987183170547, 2.050597817667451750, 9.846743663894590881 ) ) ;
#31825 = ORIENTED_EDGE ( 'NONE', *, *, #13544, .F. ) ;
#31826 = CARTESIAN_POINT ( 'NONE',  ( 3.715841784917714108, 15.00000000000000000, 15.55859621770270529 ) ) ;
#31827 = B_SPLINE_CURVE_WITH_KNOTS ( 'NONE', 3,
 ( #69472, #61954, #1485, #77446, #53970, #8959 ),
 .UNSPECIFIED., .F., .F.,
 ( 4, 2, 4 ),
 ( 7.755077673624249124E-18, 0.0002626113303185991302, 0.0005252226606371905625 ),
 .UNSPECIFIED. ) ;
#31828 = DIRECTION ( 'NONE',  ( 1.927470528863119542E-16, -1.000000000000000000, 0.000000000000000000 ) ) ;
#31829 = CARTESIAN_POINT ( 'NONE',  ( 24.16423886937410614, 49.30374883491396787, 8.672049930838204340E-16 ) ) ;
#31830 = CARTESIAN_POINT ( 'NONE',  ( 22.26659068614895176, 9.720415501580633943, -7.082119434687042414 ) ) ;
#31831 = CARTESIAN_POINT ( 'NONE',  ( 15.44008868035555793, 21.39701867748817321, -9.422509992056140149 ) ) ;
#31832 = CARTESIAN_POINT ( 'NONE',  ( -0.8801773607110991993, 37.85535201082151247, -2.915334737309923874 ) ) ;
#31833 = DIRECTION ( 'NONE',  ( -0.000000000000000000, 1.000000000000000000, -0.000000000000000000 ) ) ;
#31834 = FACE_OUTER_BOUND ( 'NONE', #35443, .T. ) ;
#31835 = CARTESIAN_POINT ( 'NONE',  ( 0.1532563361054100626, 0.8005978176674514168, -2.638427012816831230 ) ) ;
#31836 = CARTESIAN_POINT ( 'NONE',  ( 18.52753015748618282, 18.92559781766745175, -4.923371831947291888 ) ) ;
#31837 = CARTESIAN_POINT ( 'NONE',  ( 3.640395162852214650, 89.00000000000000000, 5.000000000000000000 ) ) ;
#31838 = DIRECTION ( 'NONE',  ( 0.000000000000000000, 1.000000000000000000, 0.000000000000000000 ) ) ;
#31839 = CARTESIAN_POINT ( 'NONE',  ( 2.791683348922240793, 6.633931151000785675, 7.208316651077764092 ) ) ;
#31840 = CARTESIAN_POINT ( 'NONE',  ( 0.1532563361054082862, 36.21726448433410894, 2.638427012816831674 ) ) ;
#31841 = VECTOR ( 'NONE', #26065, 1000.000000000000000 ) ;
#31842 = CARTESIAN_POINT ( 'NONE',  ( 17.96484262340118221, 14.93868534415483751, 7.964842623401181321 ) ) ;
#31843 = EDGE_CURVE ( 'NONE', #41037, #81080, #17190, .T. ) ;
#31844 = CARTESIAN_POINT ( 'NONE',  ( 22.81628187352648496, 26.83196800326374998, -3.434112377981050290 ) ) ;
#31845 = CARTESIAN_POINT ( 'NONE',  ( 12.63842701281683034, 2.467264484334118269, 9.846743663894596210 ) ) ;
#31846 = CARTESIAN_POINT ( 'NONE',  ( 5.200846386093635587, 0.000000000000000000, -1.639820566680944225 ) ) ;
#31847 = CARTESIAN_POINT ( 'NONE',  ( 17.20831665107776587, 49.13393115100078745, -7.208316651077762316 ) ) ;
#31848 = CARTESIAN_POINT ( 'NONE',  ( 2.791683348922237240, 30.38393115100078390, -7.208316651077763204 ) ) ;
#31849 = ADVANCED_FACE ( 'NONE', ( #53335 ), #84829, .T. ) ;
#31850 = CARTESIAN_POINT ( 'NONE',  ( 24.16423886937410614, 19.51208216824729647, -3.795296366450302550 ) ) ;
#31851 = CARTESIAN_POINT ( 'NONE',  ( 0.5774900079438590739, 52.64701867748817676, -5.440088680355550821 ) ) ;
#31852 = CARTESIAN_POINT ( 'NONE',  ( -0.8801773607111009756, 13.06368534415483929, 1.068504757029289695E-15 ) ) ;
#31853 = CARTESIAN_POINT ( 'NONE',  ( 7.084665262690076126, 47.02201867748818387, -10.88017736071110164 ) ) ;
#31854 = CARTESIAN_POINT ( 'NONE',  ( 15.44008868035555793, 31.39701867748817676, -9.422509992056140149 ) ) ;
#31855 = ORIENTED_EDGE ( 'NONE', *, *, #49008, .T. ) ;
#31856 = CARTESIAN_POINT ( 'NONE',  ( 4.559911319644449179, 33.89701867748817676, 9.422509992056141925 ) ) ;
#31857 = EDGE_LOOP ( 'NONE', ( #84626, #38571, #46009, #82078 ) ) ;
#31858 = CARTESIAN_POINT ( 'NONE',  ( 0.6178305044545818747, 58.49863466993042493, -9.382169495545419124 ) ) ;
#31859 = CARTESIAN_POINT ( 'NONE',  ( 20.88017736071110164, 55.35535201082149825, 2.915334737309930979 ) ) ;
#31860 = EDGE_LOOP ( 'NONE', ( #43758, #17158, #32781, #33393 ) ) ;
#31861 = CARTESIAN_POINT ( 'NONE',  ( 15.44008868035555793, 46.39701867748817676, -9.422509992056140149 ) ) ;
#31862 = CARTESIAN_POINT ( 'NONE',  ( -32.19000000000001194, 93.50000000000000000, -9.500000000000000000 ) ) ;
#31863 = DIRECTION ( 'NONE',  ( -0.000000000000000000, 1.000000000000000000, -0.000000000000000000 ) ) ;
#31864 =( NAMED_UNIT ( * ) SI_UNIT ( $, .STERADIAN. ) SOLID_ANGLE_UNIT ( ) );
#31865 = CARTESIAN_POINT ( 'NONE',  ( 17.08211943468705840, 60.13708216824729647, -12.26659068614894466 ) ) ;
#31866 = CARTESIAN_POINT ( 'NONE',  ( 17.96484262340118221, 66.18868534415483396, -7.964842623401177768 ) ) ;
#31867 = CARTESIAN_POINT ( 'NONE',  ( -0.3689425029237898834, 11.17874883491396787, -10.36894250292378850 ) ) ;
#31868 = PRESENTATION_STYLE_ASSIGNMENT (( #1415 ) ) ;
#31869 = CARTESIAN_POINT ( 'NONE',  ( 10.00000000000000178, 14.31368534415483751, 10.88017736071110342 ) ) ;
#31870 = CARTESIAN_POINT ( 'NONE',  ( 12.63842701281683034, 47.46726448433412315, 9.846743663894596210 ) ) ;
#31871 = ORIENTED_EDGE ( 'NONE', *, *, #80905, .F. ) ;
#31872 = CARTESIAN_POINT ( 'NONE',  ( 0.1532563361054100626, 40.80059781766745886, -2.638427012816831230 ) ) ;
#31873 = CARTESIAN_POINT ( 'NONE',  ( 10.00000000000000178, 44.31368534415484106, 10.88017736071110342 ) ) ;
#31874 = CARTESIAN_POINT ( 'NONE',  ( 12.63842701281683922, 39.55059781766744464, -9.846743663894590881 ) ) ;
#31875 = CARTESIAN_POINT ( 'NONE',  ( 16.40814093676323893, 30.79030133659708923, 11.09922568453595026 ) ) ;
#31877 = DIRECTION ( 'NONE',  ( 0.000000000000000000, 0.000000000000000000, -1.000000000000000000 ) ) ;
#31876 = CARTESIAN_POINT ( 'NONE',  ( 15.00000000000000178, 73.00000000000000000, -6.250000000000000000 ) ) ;
#31878 = CARTESIAN_POINT ( 'NONE',  ( 20.88017736071110164, 45.35535201082149115, 2.915334737309930979 ) ) ;
#31879 = VECTOR ( 'NONE', #12339, 1000.000000000000000 ) ;
#31880 = CARTESIAN_POINT ( 'NONE',  ( 17.08211943468705840, 60.13708216824729647, -12.26659068614894466 ) ) ;
#31881 = EDGE_CURVE ( 'NONE', #37315, #1778, #25189, .T. ) ;
#31882 = TOROIDAL_SURFACE ( 'NONE', #46253, 14.49999999999999822, 0.5000000000000000000 ) ;
#31883 = CARTESIAN_POINT ( 'NONE',  ( 10.00000000000000178, 20.37363466993042138, 12.81628187352647608 ) ) ;
#31884 = DIRECTION ( 'NONE',  ( 0.000000000000000000, 0.000000000000000000, -1.000000000000000000 ) ) ;
#31885 = ORIENTED_EDGE ( 'NONE', *, *, #36631, .T. ) ;
#31886 = CARTESIAN_POINT ( 'NONE',  ( 19.38216949554541557, 22.24863466993041428, -9.382169495545420901 ) ) ;
#31887 = CARTESIAN_POINT ( 'NONE',  ( 19.42250999205614548, 25.98035201082150891, -5.440088680355545492 ) ) ;
#31888 = ORIENTED_EDGE ( 'NONE', *, *, #97816, .T. ) ;
#31889 = MECHANICAL_DESIGN_GEOMETRIC_PRESENTATION_REPRESENTATION (  '', ( #15929 ), #20713 ) ;
#31890 = CARTESIAN_POINT ( 'NONE',  ( 7.084665262690076126, 67.02201867748817676, -10.88017736071110164 ) ) ;
#31891 = CARTESIAN_POINT ( 'NONE',  ( 17.20831665107776587, 49.13393115100078745, -7.208316651077762316 ) ) ;
#31892 = CARTESIAN_POINT ( 'NONE',  ( 18.52753015748618282, 33.92559781766745886, -4.923371831947291888 ) ) ;
#31893 = DIRECTION ( 'NONE',  ( 0.000000000000000000, 0.000000000000000000, 1.000000000000000000 ) ) ;
#31894 = CARTESIAN_POINT ( 'NONE',  ( 10.00000000000000178, 65.37363466993042493, 12.81628187352647608 ) ) ;
#31895 = CARTESIAN_POINT ( 'NONE',  ( 12.63842701281683922, 24.55059781766745175, -9.846743663894590881 ) ) ;
#31896 = CARTESIAN_POINT ( 'NONE',  ( 20.32896413005680003, 56.77164270246083788, 5.963430220938287007 ) ) ;
#31897 = DIRECTION ( 'NONE',  ( 0.000000000000000000, 0.000000000000000000, 1.000000000000000000 ) ) ;
#31899 = CARTESIAN_POINT ( 'NONE',  ( 14.92337183194729633, 2.675597817667451750, 8.527530157486181039 ) ) ;
#31898 = CARTESIAN_POINT ( 'NONE',  ( 19.84674366389459266, 8.717264484334116048, -2.638427012816827677 ) ) ;
#31900 = CARTESIAN_POINT ( 'NONE',  ( 0.000000000000000000, 0.5000000000000004441, 0.000000000000000000 ) ) ;
#31902 = EDGE_LOOP ( 'NONE', ( #59791, #49718, #13350, #72317 ) ) ;
#31901 = CARTESIAN_POINT ( 'NONE',  ( 12.63842701281683922, 44.55059781766745175, -9.846743663894590881 ) ) ;
#31903 = CARTESIAN_POINT ( 'NONE',  ( 20.15039907845753575, 16.74884699246888431, 6.262539305110077059 ) ) ;
#31904 = CARTESIAN_POINT ( 'NONE',  ( 10.00000000000000000, 27.87363466993042138, -12.81628187352647608 ) ) ;
#31905 = FACE_OUTER_BOUND ( 'NONE', #6571, .T. ) ;
#31906 = CARTESIAN_POINT ( 'NONE',  ( 20.36894250292379738, 39.92874883491396787, -10.36894250292379027 ) ) ;
#31907 = CARTESIAN_POINT ( 'NONE',  ( 5.076628168052704559, 0.1755978176674514724, -8.527530157486179263 ) ) ;
#31908 = CARTESIAN_POINT ( 'NONE',  ( 14.62617646268087768, 0.5000000000000004441, -3.327906561566883692 ) ) ;
#31909 = CARTESIAN_POINT ( 'NONE',  ( 17.08211943468705130, 48.47041550158063927, 12.26659068614894998 ) ) ;
#31910 = CARTESIAN_POINT ( 'NONE',  ( -4.164238869374099927, 62.01208216824728936, 3.795296366450308767 ) ) ;
#31911 = CARTESIAN_POINT ( 'NONE',  ( -2.266590686148945544, 17.22041550158063572, 7.082119434687048631 ) ) ;
#31913 = DIRECTION ( 'NONE',  ( -0.1132032137679106348, 0.000000000000000000, 0.9935718556765871234 ) ) ;
#31912 = CARTESIAN_POINT ( 'NONE',  ( 2.917880565312950480, 30.97041550158063572, -12.26659068614894821 ) ) ;
#31914 = CARTESIAN_POINT ( 'NONE',  ( 4.526800700887880780, -5.190657137169758073, -3.750000000000000888 ) ) ;
#31915 = B_SPLINE_CURVE_WITH_KNOTS ( 'NONE', 3,
 ( #19362, #25885, #86388, #18875, #56384, #40892 ),
 .UNSPECIFIED., .F., .F.,
 ( 4, 2, 4 ),
 ( 0.000000000000000000, 0.0002701661927229362576, 0.0005403323854458725152 ),
 .UNSPECIFIED. ) ;
#31917 = CARTESIAN_POINT ( 'NONE',  ( 19.84674366389459621, 38.50893115100078745, 7.409399052514197653E-17 ) ) ;
#31916 = CARTESIAN_POINT ( 'NONE',  ( 6.324684870385063995, -50.88968658577716297, 2.500000000000000888 ) ) ;
#31918 = B_SPLINE_CURVE_WITH_KNOTS ( 'NONE', 3,
 ( #36344, #87861, #72361, #79875 ),
 .UNSPECIFIED., .F., .F.,
 ( 4, 4 ),
 ( 1.644748632280675619E-16, 0.001060528352561984416 ),
 .UNSPECIFIED. ) ;
#31919 = ORIENTED_EDGE ( 'NONE', *, *, #41296, .F. ) ;
#31920 = CARTESIAN_POINT ( 'NONE',  ( 0.5774900079438607392, 43.48035201082151247, 5.440088680355550821 ) ) ;
#31921 = CARTESIAN_POINT ( 'NONE',  ( 20.00000000000000711, 89.78870847431471702, -4.994901225416799484 ) ) ;
#31922 = ADVANCED_FACE ( 'NONE', ( #31319 ), #61819, .F. ) ;
#31923 = CARTESIAN_POINT ( 'NONE',  ( 1.472469842513823179, 36.42559781766745175, 4.923371831947296329 ) ) ;
#31924 = CARTESIAN_POINT ( 'NONE',  ( 16.40814093676324603, 57.45696800326375353, -11.09922568453594671 ) ) ;
#31925 = CARTESIAN_POINT ( 'NONE',  ( 3.795296366450306547, -9.654584498419360727, -14.16423886937410259 ) ) ;
#31926 = CARTESIAN_POINT ( 'NONE',  ( 2.791683348922240793, 41.63393115100078745, 7.208316651077764092 ) ) ;
#31927 = CARTESIAN_POINT ( 'NONE',  ( 2.791683348922237240, 60.38393115100078745, -7.208316651077763204 ) ) ;
#31928 = CARTESIAN_POINT ( 'NONE',  ( 13.79529636645031943, 40.34541550158063217, -14.16423886937409904 ) ) ;
#31929 = ORIENTED_EDGE ( 'NONE', *, *, #95318, .T. ) ;
#31930 = CARTESIAN_POINT ( 'NONE',  ( 22.26659068614894466, 18.88708216824730002, 7.082119434687054849 ) ) ;
#31931 = CARTESIAN_POINT ( 'NONE',  ( 9.779999999999994031, 1.885066177228129719E-15, 3.000000000000000000 ) ) ;
#31932 = CARTESIAN_POINT ( 'NONE',  ( 0.000000000000000000, 14.49999999999999822, 0.000000000000000000 ) ) ;
#31933 = CARTESIAN_POINT ( 'NONE',  ( 4.559911319644449179, 12.23035201082150714, -9.422509992056141925 ) ) ;
#31934 = CARTESIAN_POINT ( 'NONE',  ( 19.38216949554541202, 5.998634669930420493, 9.382169495545424454 ) ) ;
#31935 = CARTESIAN_POINT ( 'NONE',  ( -14.26139399674459263, 4.837279266207889341E-16, 2.619664342929711509 ) ) ;
#31936 = CARTESIAN_POINT ( 'NONE',  ( -0.8801773607110991993, 62.85535201082150536, -2.915334737309923874 ) ) ;
#31937 = CARTESIAN_POINT ( 'NONE',  ( 4.721518086276724979, -3.620742741961517019, -4.000000000000000000 ) ) ;
#31938 = CARTESIAN_POINT ( 'NONE',  ( -46.50435961404672014, 102.7681846068616238, -6.785878169524574233 ) ) ;
#31939 = DIRECTION ( 'NONE',  ( -0.000000000000000000, -0.000000000000000000, -1.000000000000000000 ) ) ;
#31940 = CARTESIAN_POINT ( 'NONE',  ( 10.00000000000000178, 63.05374883491396076, 14.16423886937410082 ) ) ;
#31941 = CARTESIAN_POINT ( 'NONE',  ( 2.896551724137929273, 22.29452073070357088, 3.547252797530261487E-16 ) ) ;
#31942 = CARTESIAN_POINT ( 'NONE',  ( 19.42250999205614548, 20.98035201082150891, -5.440088680355545492 ) ) ;
#31943 = CARTESIAN_POINT ( 'NONE',  ( 12.91533473730993009, 26.60535201082150536, -10.88017736071109987 ) ) ;
#31944 = CARTESIAN_POINT ( 'NONE',  ( -1.099225684535947600, -0.4596986634029132657, 6.408140936763237150 ) ) ;
#31945 = CARTESIAN_POINT ( 'NONE',  ( 5.076628168052704559, 55.17559781766745175, -8.527530157486179263 ) ) ;
#31946 = CARTESIAN_POINT ( 'NONE',  ( 10.00000000000000178, 60.37363466993041783, 12.81628187352647608 ) ) ;
#31948 = ORIENTED_EDGE ( 'NONE', *, *, #92212, .F. ) ;
#31947 = AXIS2_PLACEMENT_3D ( 'NONE', #87850, #81822, #65340 ) ;
#31949 = CARTESIAN_POINT ( 'NONE',  ( 10.00000000000000178, 34.31368534415484106, 10.88017736071110342 ) ) ;
#31950 = CARTESIAN_POINT ( 'NONE',  ( 22.81628187352647785, 26.41530133659708923, 3.434112377981063169 ) ) ;
#31951 = SPHERICAL_SURFACE ( 'NONE', #52919, 0.2500000000000000000 ) ;
#31952 = ADVANCED_FACE ( 'NONE', ( #22368 ), #52353, .T. ) ;
#31953 = CARTESIAN_POINT ( 'NONE',  ( 1.472469842513823179, 65.59226448433412315, -4.923371831947296329 ) ) ;
#31954 = CARTESIAN_POINT ( 'NONE',  ( 2.035157376598822676, 47.43868534415484817, -7.964842623401177768 ) ) ;
#31955 = CARTESIAN_POINT ( 'NONE',  ( 0.1532563361054083140, 11.00893115100078568, 1.131784320476157264E-15 ) ) ;
#31956 = CARTESIAN_POINT ( 'NONE',  ( 10.00000000000000000, 37.87363466993041783, -12.81628187352647608 ) ) ;
#31958 = LINE ( 'NONE', #16989, #59133 ) ;
#31957 = CARTESIAN_POINT ( 'NONE',  ( 20.88017736071110519, 65.56368534415483396, 2.639326808657452039E-16 ) ) ;
#31959 = CARTESIAN_POINT ( 'NONE',  ( 10.91061041304821977, 0.2306972965111880602, 10.20767530377056431 ) ) ;
#31960 = VERTEX_POINT ( 'NONE', #57267 ) ;
#31961 = CARTESIAN_POINT ( 'NONE',  ( 11.96291822454875842, 15.00000000000000000, 8.193813980849165901 ) ) ;
#31962 = CARTESIAN_POINT ( 'NONE',  ( 18.72515096720609051, 25.05509018479941119, 6.499999999999470646 ) ) ;
#31963 = EDGE_CURVE ( 'NONE', #41634, #25948, #17811, .T. ) ;
#31964 = CARTESIAN_POINT ( 'NONE',  ( 15.44008868035555793, 51.39701867748816966, -9.422509992056140149 ) ) ;
#31965 = CARTESIAN_POINT ( 'NONE',  ( 3.591859063236763294, 43.29030133659708923, -11.09922568453595026 ) ) ;
#31966 = CARTESIAN_POINT ( 'NONE',  ( 12.63842701281683034, 17.46726448433411250, 9.846743663894596210 ) ) ;
#31967 = AXIS2_PLACEMENT_3D ( 'NONE', #58740, #4280, #50245 ) ;
#31968 = CARTESIAN_POINT ( 'NONE',  ( 0.1532563361054100626, 15.80059781766745353, -2.638427012816831230 ) ) ;
#31969 = CARTESIAN_POINT ( 'NONE',  ( 2.575439399273669938, 0.4791814250636889927, -6.500000000000363265 ) ) ;
#31970 = CARTESIAN_POINT ( 'NONE',  ( -2.266590686148945544, 61.38708216824730357, -7.082119434687050408 ) ) ;
#31971 = VERTEX_POINT ( 'NONE', #85816 ) ;
#31972 = CARTESIAN_POINT ( 'NONE',  ( -6.898461952320262824, 4.061641280801676772E-16, -12.75387089053318590 ) ) ;
#31973 = CARTESIAN_POINT ( 'NONE',  ( 10.00000000000000000, 11.81368534415483751, -10.88017736071110342 ) ) ;
#31974 = CARTESIAN_POINT ( 'NONE',  ( 19.72487221294570858, 46.86607318730077054, 6.500000000000000888 ) ) ;
#31975 = VERTEX_POINT ( 'NONE', #40811 ) ;
#31976 = CARTESIAN_POINT ( 'NONE',  ( -0.8801773607111009756, 8.063685344154837509, 1.068504757029289695E-15 ) ) ;
#31977 = CARTESIAN_POINT ( 'NONE',  ( 4.559911319644449179, 3.897018677488171434, 9.422509992056141925 ) ) ;
#31978 = CARTESIAN_POINT ( 'NONE',  ( 0.1532563361054082862, 46.21726448433411605, 2.638427012816831674 ) ) ;
#31979 = CARTESIAN_POINT ( 'NONE',  ( 22.81628187352647785, 46.41530133659708213, 3.434112377981063169 ) ) ;
#31980 = FACE_OUTER_BOUND ( 'NONE', #23868, .T. ) ;
#31982 = CARTESIAN_POINT ( 'NONE',  ( -2.266590686148945544, 17.22041550158063572, 7.082119434687048631 ) ) ;
#31981 = DIRECTION ( 'NONE',  ( 0.000000000000000000, 0.000000000000000000, -1.000000000000000000 ) ) ;
#31983 = CARTESIAN_POINT ( 'NONE',  ( 12.91533473730993009, 26.60535201082150536, -10.88017736071109987 ) ) ;
#31984 = CARTESIAN_POINT ( 'NONE',  ( 20.88017736071110164, 5.355352010821503583, 2.915334737309930979 ) ) ;
#31985 = CARTESIAN_POINT ( 'NONE',  ( 19.84674366389459621, 38.50893115100078745, 7.409399052514197653E-17 ) ) ;
#31986 = LINE ( 'NONE', #93496, #68436 ) ;
#31987 = CARTESIAN_POINT ( 'NONE',  ( 10.00000000000000000, 34.75893115100078745, -9.846743663894594434 ) ) ;
#31988 = LINE ( 'NONE', #38171, #43094 ) ;
#31989 = CARTESIAN_POINT ( 'NONE',  ( 3.640395162852214650, 89.00000000000000000, -12.00000000000000000 ) ) ;
#31990 = CARTESIAN_POINT ( 'NONE',  ( 9.846743663894590881, 23.30059781766746596, 2.638427012816828565 ) ) ;
#31991 = ORIENTED_EDGE ( 'NONE', *, *, #41900, .T. ) ;
#31992 = CARTESIAN_POINT ( 'NONE',  ( -6.761335002692915985, 14.76984993307862837, -13.32315948060046829 ) ) ;
#31993 = CARTESIAN_POINT ( 'NONE',  ( 1.472469842513823179, 1.425597817667451528, 4.923371831947296329 ) ) ;
#31994 = CARTESIAN_POINT ( 'NONE',  ( 14.92337183194729988, 59.34226448433412315, -8.527530157486177487 ) ) ;
#31996 = CARTESIAN_POINT ( 'NONE',  ( 7.084665262690076126, 49.10535201082149825, 10.88017736071109987 ) ) ;
#31995 = CARTESIAN_POINT ( 'NONE',  ( 17.96484262340118221, 44.93868534415483396, 7.964842623401181321 ) ) ;
#31998 = CARTESIAN_POINT ( 'NONE',  ( -1.099225684535947600, 49.54030133659708923, 6.408140936763237150 ) ) ;
#31997 = CARTESIAN_POINT ( 'NONE',  ( 17.96484262340118221, 6.188685344154836621, -7.964842623401177768 ) ) ;
#31999 = CARTESIAN_POINT ( 'NONE',  ( -2.266590686148945544, 12.22041550158063394, 7.082119434687048631 ) ) ;
#32000 = EDGE_CURVE ( 'NONE', #92229, #44802, #40320, .T. ) ;
#32001 = COLOUR_RGB ( '', 0.72549020, 0.75294118, 0.79215686) ;
#32002 = CARTESIAN_POINT ( 'NONE',  ( 3.591859063236761518, 49.95696800326375353, 11.09922568453594849 ) ) ;
#32003 = ORIENTED_EDGE ( 'NONE', *, *, #49247, .T. ) ;
#32004 = CARTESIAN_POINT ( 'NONE',  ( 18.52753015748618282, 58.92559781766745886, -4.923371831947291888 ) ) ;
#32005 = CARTESIAN_POINT ( 'NONE',  ( 2.035157376598824452, 18.68868534415484106, 7.964842623401179544 ) ) ;
#32006 = ORIENTED_EDGE ( 'NONE', *, *, #42012, .T. ) ;
#32007 = TOROIDAL_SURFACE ( 'NONE', #91114, 14.49999999999999822, 0.5000000000000000000 ) ;
#32008 = CARTESIAN_POINT ( 'NONE',  ( 0.5774900079438590739, 32.64701867748816966, -5.440088680355550821 ) ) ;
#32009 = ADVANCED_FACE ( 'NONE', ( #78301 ), #71311, .T. ) ;
#32010 = ORIENTED_EDGE ( 'NONE', *, *, #1305, .T. ) ;
#32011 = CARTESIAN_POINT ( 'NONE',  ( 10.00000000000000000, 61.81368534415484106, -10.88017736071110342 ) ) ;
#32012 =( BOUNDED_CURVE ( )  B_SPLINE_CURVE ( 2, ( #61592, #77582, #93080, #76606, #92105, #70101, #85596, #17109, #47592 ),
 .UNSPECIFIED., .F., .T. ) 
 B_SPLINE_CURVE_WITH_KNOTS ( ( 3, 2, 2, 2, 3 ),
 ( 0.3310855930462679453, 0.3333333333333333148, 0.3392857142857143016, 0.3452380952380952328, 0.3474858355251606024 ),
 .UNSPECIFIED. ) 
 CURVE ( )  GEOMETRIC_REPRESENTATION_ITEM ( )  RATIONAL_B_SPLINE_CURVE ( ( 0.9839835555609424134, 0.9871328979762477029, 1.000000000000000000, 0.9659258262890683122, 1.000000000000000000, 0.9659258262890683122, 1.000000000000000000, 0.9871328979762477029, 0.9839835555609424134 ) ) 
 REPRESENTATION_ITEM ( '' )  );
#32013 = CARTESIAN_POINT ( 'NONE',  ( 7.361572987183169658, 4.967264484334119601, -9.846743663894592657 ) ) ;
#32014 = CARTESIAN_POINT ( 'NONE',  ( 0.1532563361054100626, 0.8005978176674514168, -2.638427012816831230 ) ) ;
#32015 = AXIS2_PLACEMENT_3D ( 'NONE', #79229, #62742, #71733 ) ;
#32016 = CARTESIAN_POINT ( 'NONE',  ( -5.302565485995502037, 0.000000000000000000, 1.273033341818796460 ) ) ;
#32017 = CARTESIAN_POINT ( 'NONE',  ( -46.94000000000001194, 101.0890360526157252, 7.984865333617746863 ) ) ;
#32019 = ORIENTED_EDGE ( 'NONE', *, *, #64952, .T. ) ;
#32018 = CARTESIAN_POINT ( 'NONE',  ( 17.20831665107776587, 2.883931151000785231, 7.208316651077764980 ) ) ;
#32020 = CARTESIAN_POINT ( 'NONE',  ( 10.00000000000000178, 37.25893115100078745, 9.846743663894594434 ) ) ;
#32021 = ORIENTED_EDGE ( 'NONE', *, *, #92033, .F. ) ;
#32022 = ORIENTED_EDGE ( 'NONE', *, *, #84873, .F. ) ;
#32023 = CARTESIAN_POINT ( 'NONE',  ( 12.60589901313216110, 0.5000000000000004441, 8.129656208642140669 ) ) ;
#32024 = CARTESIAN_POINT ( 'NONE',  ( 2.917880565312948704, 12.63708216824730179, 12.26659068614894643 ) ) ;
#32025 = CARTESIAN_POINT ( 'NONE',  ( 22.81628187352647785, 61.41530133659709634, 3.434112377981063169 ) ) ;
#32026 = CARTESIAN_POINT ( 'NONE',  ( 10.00000000000000000, 0.5537488349139675359, -14.16423886937410082 ) ) ;
#32027 = CARTESIAN_POINT ( 'NONE',  ( 10.00000000000000000, 20.55374883491396787, -14.16423886937410082 ) ) ;
#32028 = FACE_OUTER_BOUND ( 'NONE', #62522, .T. ) ;
#32030 = CARTESIAN_POINT ( 'NONE',  ( 0.5774900079438607392, 63.48035201082149825, 5.440088680355550821 ) ) ;
#32029 = CARTESIAN_POINT ( 'NONE',  ( 19.05866839779138644, 10.95508385108958826, -6.499999999999970690 ) ) ;
#32031 = CARTESIAN_POINT ( 'NONE',  ( 19.42250999205614193, 15.14701867748817143, 5.440088680355555262 ) ) ;
#32032 = CARTESIAN_POINT ( 'NONE',  ( 0.1955144967548754498, 59.32703681773342907, -6.500000000002697398 ) ) ;
#32033 = ORIENTED_EDGE ( 'NONE', *, *, #97652, .T. ) ;
#32034 = CARTESIAN_POINT ( 'NONE',  ( 10.00000000000000000, -0.2410688489992152128, -9.846743663894594434 ) ) ;
#32035 = CARTESIAN_POINT ( 'NONE',  ( 19.84674366389459266, 8.300597817667451750, 2.638427012816836559 ) ) ;
#32036 = VECTOR ( 'NONE', #30583, 1000.000000000000000 ) ;
#32037 = CARTESIAN_POINT ( 'NONE',  ( 22.81628187352647785, 26.41530133659708923, 3.434112377981063169 ) ) ;
#32038 = CARTESIAN_POINT ( 'NONE',  ( 0.1532563361054100626, 30.80059781766744820, -2.638427012816831230 ) ) ;
#32039 = EDGE_CURVE ( 'NONE', #54527, #30230, #95582, .T. ) ;
#32040 = CARTESIAN_POINT ( 'NONE',  ( 3.591859063236761518, 19.95696800326375353, 11.09922568453594849 ) ) ;
#32041 = CARTESIAN_POINT ( 'NONE',  ( 20.10421743870886857, 40.60736173766202484, -6.337391062633416894 ) ) ;
#32042 = AXIS2_PLACEMENT_3D ( 'NONE', #22228, #36730, #7720 ) ;
#32043 = CARTESIAN_POINT ( 'NONE',  ( 18.52753015748617571, 3.092264484334118269, 4.923371831947298993 ) ) ;
#32044 = ORIENTED_EDGE ( 'NONE', *, *, #46756, .F. ) ;
#32045 = EDGE_CURVE ( 'NONE', #8279, #23534, #34569, .T. ) ;
#32046 = VERTEX_POINT ( 'NONE', #79780 ) ;
#32047 = CARTESIAN_POINT ( 'NONE',  ( -0.8801773607111008646, 43.27201867748817676, 2.915334737309923430 ) ) ;
#32048 = CARTESIAN_POINT ( 'NONE',  ( 20.36894250292379382, 33.67874883491396076, 10.36894250292379205 ) ) ;
#32049 = CARTESIAN_POINT ( 'NONE',  ( 19.84674366389459266, 43.71726448433410894, -2.638427012816827677 ) ) ;
#32050 = CARTESIAN_POINT ( 'NONE',  ( -0.8801773607110991993, 62.85535201082150536, -2.915334737309923874 ) ) ;
#32052 = CARTESIAN_POINT ( 'NONE',  ( -7.127794346849581686, -80.93619716733994096, -3.750000000000000000 ) ) ;
#32051 = CARTESIAN_POINT ( 'NONE',  ( -2.816281873526471635, 58.91530133659707502, -3.434112377981056508 ) ) ;
#32053 = CARTESIAN_POINT ( 'NONE',  ( 17.96484262340118221, 31.18868534415483751, -7.964842623401177768 ) ) ;
#32054 = DIRECTION ( 'NONE',  ( 0.000000000000000000, 0.000000000000000000, -1.000000000000000000 ) ) ;
#32055 = CARTESIAN_POINT ( 'NONE',  ( 6.565887622018943937, 20.16530133659708213, 12.81628187352647430 ) ) ;
#32056 = CARTESIAN_POINT ( 'NONE',  ( 16.40814093676324603, 27.45696800326375708, -11.09922568453594671 ) ) ;
#32057 = CARTESIAN_POINT ( 'NONE',  ( 10.00000000000000178, 37.25893115100078745, 9.846743663894594434 ) ) ;
#32058 = CARTESIAN_POINT ( 'NONE',  ( -7.964842623401179544, 2.438685344154844170, -7.964842623401174215 ) ) ;
#32059 = CARTESIAN_POINT ( 'NONE',  ( -2.816281873526473856, 49.33196800326374643, 3.434112377981055619 ) ) ;
#32060 = CARTESIAN_POINT ( 'NONE',  ( 14.56089864659469946, -2.824431362619463692E-15, 1.374314915485391753 ) ) ;
#32062 = DIRECTION ( 'NONE',  ( 1.000000000000000000, 0.000000000000000000, 0.000000000000000000 ) ) ;
#32061 = CARTESIAN_POINT ( 'NONE',  ( 10.00000000000000178, 49.31368534415484106, 10.88017736071110342 ) ) ;
#32063 = CARTESIAN_POINT ( 'NONE',  ( -10.53011945866294852, -98.59345040283277228, 4.000000000000000000 ) ) ;
#32064 = CARTESIAN_POINT ( 'NONE',  ( 0.000000000000000000, 15.00000000000000000, 0.000000000000000000 ) ) ;
#32065 = CARTESIAN_POINT ( 'NONE',  ( 2.035157376598822676, 52.43868534415483396, -7.964842623401177768 ) ) ;
#32066 = VECTOR ( 'NONE', #10082, 1000.000000000000000 ) ;
#32067 = CARTESIAN_POINT ( 'NONE',  ( 20.88017736071110164, 55.35535201082149825, 2.915334737309930979 ) ) ;
#32068 = CARTESIAN_POINT ( 'NONE',  ( 0.000000000000000000, 15.00000000000000000, 0.000000000000000000 ) ) ;
#32070 = ADVANCED_FACE ( 'NONE', ( #70824 ), #56986, .T. ) ;
#32069 = CARTESIAN_POINT ( 'NONE',  ( 3.469446951953614189E-15, 10.93830936912750573, 11.92686044187656513 ) ) ;
#32071 = CARTESIAN_POINT ( 'NONE',  ( 20.88017736071110164, 10.35535201082150714, 2.915334737309930979 ) ) ;
#32072 = CARTESIAN_POINT ( 'NONE',  ( 10.00000000000000178, 57.25893115100078745, 9.846743663894594434 ) ) ;
#32074 = CARTESIAN_POINT ( 'NONE',  ( 26.00000000000000355, 35.99999999999997158, -7.000000000000000000 ) ) ;
#32073 = CARTESIAN_POINT ( 'NONE',  ( 12.91533473730992121, 19.52201867748816611, 10.88017736071110164 ) ) ;
#32075 = ADVANCED_FACE ( 'NONE', ( #26771 ), #29395, .T. ) ;
#32076 = CARTESIAN_POINT ( 'NONE',  ( 0.6178305044545818747, 28.49863466993041783, -9.382169495545419124 ) ) ;
#32077 = ORIENTED_EDGE ( 'NONE', *, *, #54836, .F. ) ;
#32078 = CARTESIAN_POINT ( 'NONE',  ( 4.559911319644449179, 43.89701867748816966, 9.422509992056141925 ) ) ;
#32079 = EDGE_CURVE ( 'NONE', #31750, #60629, #42795, .T. ) ;
#32081 = CYLINDRICAL_SURFACE ( 'NONE', #71744, 0.2500000000000002220 ) ;
#32080 = CARTESIAN_POINT ( 'NONE',  ( 19.38216949554541557, 2.248634669930420049, -9.382169495545420901 ) ) ;
#32082 = CARTESIAN_POINT ( 'NONE',  ( -0.8801773607111009756, 8.063685344154837509, 1.068504757029289695E-15 ) ) ;
#32083 = COLOUR_RGB ( '', 0.66274510, 0.83137255, 0.94901961) ;
#32084 = CARTESIAN_POINT ( 'NONE',  ( 12.91533473730992121, 44.52201867748816966, 10.88017736071110164 ) ) ;
#32085 = CARTESIAN_POINT ( 'NONE',  ( 6.204703633549690345, 57.84541550158063927, 14.16423886937410082 ) ) ;
#32086 = CARTESIAN_POINT ( 'NONE',  ( 10.00000000000000178, 47.25893115100078745, 9.846743663894594434 ) ) ;
#32087 = CARTESIAN_POINT ( 'NONE',  ( 15.44008868035555793, 66.39701867748817676, -9.422509992056140149 ) ) ;
#32088 = FACE_OUTER_BOUND ( 'NONE', #94878, .T. ) ;
#32089 = CARTESIAN_POINT ( 'NONE',  ( -4.164238869374098151, 21.59541550158063217, -3.795296366450310543 ) ) ;
#32090 = UNCERTAINTY_MEASURE_WITH_UNIT (LENGTH_MEASURE( 1.000000000000000082E-05 ), #71913, 'distance_accuracy_value', 'NONE');
#32091 = CARTESIAN_POINT ( 'NONE',  ( 19.67858290521088804, 89.00000000000000000, -5.461713021790605360 ) ) ;
#32092 = VERTEX_POINT ( 'NONE', #15762 ) ;
#32093 = VERTEX_POINT ( 'NONE', #98290 ) ;
#32094 = CARTESIAN_POINT ( 'NONE',  ( 6.204703633549690345, 30.76208216824730357, -14.16423886937410259 ) ) ;
#32095 = CARTESIAN_POINT ( 'NONE',  ( -2.266590686148945544, 32.22041550158063927, 7.082119434687048631 ) ) ;
#32096 = CARTESIAN_POINT ( 'NONE',  ( 0.1532563361054082862, 6.217264484334118713, 2.638427012816831674 ) ) ;
#32097 = CARTESIAN_POINT ( 'NONE',  ( 17.20831665107776587, 57.88393115100078745, 7.208316651077764980 ) ) ;
#32098 = CARTESIAN_POINT ( 'NONE',  ( 20.03447792253738768, 52.65514106990692511, -6.401564815979734924 ) ) ;
#32100 = CARTESIAN_POINT ( 'NONE',  ( 6.565887622018943937, 38.08196800326376064, -12.81628187352647608 ) ) ;
#32099 = CARTESIAN_POINT ( 'NONE',  ( 12.91533473730993009, 61.60535201082150536, -10.88017736071109987 ) ) ;
#32101 = CARTESIAN_POINT ( 'NONE',  ( 22.26659068614894466, 28.88708216824730357, 7.082119434687054849 ) ) ;
#32102 = CARTESIAN_POINT ( 'NONE',  ( 15.44008868035555793, 31.39701867748817676, -9.422509992056140149 ) ) ;
#32103 = CARTESIAN_POINT ( 'NONE',  ( 20.15039907845753930, 4.722660991849187972, 6.262539305110067289 ) ) ;
#32104 = CARTESIAN_POINT ( 'NONE',  ( 0.1532563361054100626, 0.8005978176674514168, -2.638427012816831230 ) ) ;
#32105 = CARTESIAN_POINT ( 'NONE',  ( 2.638427012816829897, -15.44940218233254470, -9.846743663894592657 ) ) ;
#32106 = VERTEX_POINT ( 'NONE', #68269 ) ;
#32107 = LINE ( 'NONE', #16644, #97065 ) ;
#32108 = ORIENTED_EDGE ( 'NONE', *, *, #97600, .F. ) ;
#32109 = SURFACE_STYLE_USAGE ( .BOTH. , #47626 ) ;
#32110 = ORIENTED_EDGE ( 'NONE', *, *, #74171, .F. ) ;
#32111 = AXIS2_PLACEMENT_3D ( 'NONE', #59361, #91341, #22869 ) ;
#32112 = CARTESIAN_POINT ( 'NONE',  ( 22.26659068614895176, 4.720415501580633943, -7.082119434687042414 ) ) ;
#32114 = CARTESIAN_POINT ( 'NONE',  ( 4.559911319644449179, 17.23035201082150536, -9.422509992056141925 ) ) ;
#32113 = CARTESIAN_POINT ( 'NONE',  ( 24.16423886937410614, 64.51208216824728936, -3.795296366450302550 ) ) ;
#32116 = CARTESIAN_POINT ( 'NONE',  ( 7.361572987183169658, 54.96726448433413026, -9.846743663894592657 ) ) ;
#32115 = CARTESIAN_POINT ( 'NONE',  ( 10.00000000000000000, 34.75893115100078745, -9.846743663894594434 ) ) ;
#32117 = DIRECTION ( 'NONE',  ( 0.000000000000000000, 1.000000000000000000, 0.000000000000000000 ) ) ;
#32118 = AXIS2_PLACEMENT_3D ( 'NONE', #2828, #70822, #10310 ) ;
#32119 = CARTESIAN_POINT ( 'NONE',  ( -13.96552416078061043, 14.95037115134968708, -4.756200848675268489 ) ) ;
#32120 = EDGE_CURVE ( 'NONE', #64665, #33002, #45755, .T. ) ;
#32121 = TOROIDAL_SURFACE ( 'NONE', #14599, 14.49999999999999822, 0.5000000000000000000 ) ;
#32122 = CARTESIAN_POINT ( 'NONE',  ( 13.43411237798106583, 2.665301336597086568, -12.81628187352647252 ) ) ;
#32123 = ORIENTED_EDGE ( 'NONE', *, *, #55919, .T. ) ;
#32124 = CARTESIAN_POINT ( 'NONE',  ( -0.3689425029237898834, 41.17874883491397497, -10.36894250292378850 ) ) ;
#32125 = ORIENTED_EDGE ( 'NONE', *, *, #64785, .T. ) ;
#32126 = CARTESIAN_POINT ( 'NONE',  ( 17.08211943468705130, 43.47041550158063927, 12.26659068614894998 ) ) ;
#32127 = VERTEX_POINT ( 'NONE', #15275 ) ;
#32128 = CARTESIAN_POINT ( 'NONE',  ( -0.8801773607111008646, 23.27201867748817676, 2.915334737309923430 ) ) ;
#32129 =( LENGTH_UNIT ( ) NAMED_UNIT ( * ) SI_UNIT ( .MILLI., .METRE. ) );
#32130 = CARTESIAN_POINT ( 'NONE',  ( 15.44008868035555260, 44.73035201082151247, 9.422509992056143702 ) ) ;
#32131 = CARTESIAN_POINT ( 'NONE',  ( 0.1532563361054083140, 46.00893115100079456, 1.131784320476157264E-15 ) ) ;
#32132 = CARTESIAN_POINT ( 'NONE',  ( 15.44008868035555260, 39.73035201082150536, 9.422509992056143702 ) ) ;
#32133 = CARTESIAN_POINT ( 'NONE',  ( 20.88017736071110519, 60.56368534415484106, 2.639326808657452039E-16 ) ) ;
#32134 = CARTESIAN_POINT ( 'NONE',  ( 4.559911319644449179, 28.89701867748817321, 9.422509992056141925 ) ) ;
#32137 = ORIENTED_EDGE ( 'NONE', *, *, #23470, .T. ) ;
#32136 = AXIS2_PLACEMENT_3D ( 'NONE', #74117, #28137, #12150 ) ;
#32135 = CARTESIAN_POINT ( 'NONE',  ( 0.000000000000000000, 14.49999999999999822, 0.000000000000000000 ) ) ;
#32138 = CARTESIAN_POINT ( 'NONE',  ( 10.00000000000000178, 7.258931151000785675, 9.846743663894594434 ) ) ;
#32139 = CARTESIAN_POINT ( 'NONE',  ( -4.259797195126484581, -13.81744876717395876, 2.750000000000000888 ) ) ;
#32140 = VERTEX_POINT ( 'NONE', #60740 ) ;
#32141 = DIRECTION ( 'NONE',  ( -0.06975647374410356982, -0.9975640502598257520, -0.000000000000000000 ) ) ;
#32142 = CARTESIAN_POINT ( 'NONE',  ( 10.00000000000000000, 39.75893115100078745, -9.846743663894594434 ) ) ;
#32143 = FACE_OUTER_BOUND ( 'NONE', #53859, .T. ) ;
#32144 = CARTESIAN_POINT ( 'NONE',  ( 22.81628187352648496, 46.83196800326376064, -3.434112377981050290 ) ) ;
#32145 = COLOUR_RGB ( '', 0.66274510, 0.83137255, 0.94901961) ;
#32146 = CARTESIAN_POINT ( 'NONE',  ( 14.17193700899789022, 0.000000000000000000, 1.489530601564113654 ) ) ;
#32147 = ORIENTED_EDGE ( 'NONE', *, *, #11098, .T. ) ;
#32148 = CARTESIAN_POINT ( 'NONE',  ( 1.472469842513823179, 65.59226448433412315, -4.923371831947296329 ) ) ;
#32149 = CARTESIAN_POINT ( 'NONE',  ( 19.72487221294569792, 32.80223176428832232, -6.500000000000008882 ) ) ;
#32150 = CARTESIAN_POINT ( 'NONE',  ( 19.84674366389459621, 53.50893115100078745, 7.409399052514197653E-17 ) ) ;
#32151 = CARTESIAN_POINT ( 'NONE',  ( 24.16423886937409904, 44.09541550158063927, 3.795296366450317205 ) ) ;
#32152 = CARTESIAN_POINT ( 'NONE',  ( 19.84674366389459266, 63.30059781766745886, 2.638427012816836559 ) ) ;
#32153 = ORIENTED_EDGE ( 'NONE', *, *, #87703, .F. ) ;
#32155 = VECTOR ( 'NONE', #21164, 1000.000000000000000 ) ;
#32154 = FACE_OUTER_BOUND ( 'NONE', #66799, .T. ) ;
#32156 = CARTESIAN_POINT ( 'NONE',  ( 17.20831665107776587, 19.13393115100078035, -7.208316651077762316 ) ) ;
#32157 = CARTESIAN_POINT ( 'NONE',  ( 13.43411237798106583, 52.66530133659708213, -12.81628187352647252 ) ) ;
#32158 = CARTESIAN_POINT ( 'NONE',  ( 10.00000000000000178, 62.25893115100078745, 9.846743663894594434 ) ) ;
#32159 = CARTESIAN_POINT ( 'NONE',  ( 0.5774900079438590739, 57.64701867748817676, -5.440088680355550821 ) ) ;
#32160 = CARTESIAN_POINT ( 'NONE',  ( 19.72487221294571569, 30.71833443783938122, -6.499999999999989342 ) ) ;
#32161 = ADVANCED_FACE ( 'NONE', ( #85232 ), #92718, .F. ) ;
#32162 = EDGE_CURVE ( 'NONE', #97093, #45049, #24043, .T. ) ;
#32163 = EDGE_CURVE ( 'NONE', #85662, #48243, #54223, .T. ) ;
#32164 = EDGE_LOOP ( 'NONE', ( #43217, #83434, #50604, #77500 ) ) ;
#32165 = CARTESIAN_POINT ( 'NONE',  ( 20.36894250292379738, 59.92874883491397497, -10.36894250292379027 ) ) ;
#32166 = CARTESIAN_POINT ( 'NONE',  ( 6.000000000000000000, 11.50000000000000000, -6.000000000000000000 ) ) ;
#32167 = CARTESIAN_POINT ( 'NONE',  ( -0.8801773607111008646, 33.27201867748817676, 2.915334737309923430 ) ) ;
#32169 = CARTESIAN_POINT ( 'NONE',  ( 2.035157376598824452, 53.68868534415484817, 7.964842623401179544 ) ) ;
#32168 = CARTESIAN_POINT ( 'NONE',  ( 0.6178305044545838731, 14.74863466993041783, 9.382169495545420901 ) ) ;
#32170 = CARTESIAN_POINT ( 'NONE',  ( 3.969999999999999751, 37.25000000000000000, 3.750000000000000000 ) ) ;
#32171 = LINE ( 'NONE', #93672, #18254 ) ;
#32173 = CARTESIAN_POINT ( 'NONE',  ( 17.85158348494331904, 34.73726573380434957, -6.499999999999977796 ) ) ;
#32172 = CARTESIAN_POINT ( 'NONE',  ( 4.559911319644449179, 47.23035201082150536, -9.422509992056141925 ) ) ;
#32174 = CARTESIAN_POINT ( 'NONE',  ( 5.076628168052704559, 35.17559781766745175, -8.527530157486179263 ) ) ;
#32175 = CARTESIAN_POINT ( 'NONE',  ( 2.791683348922237240, 5.383931151000785675, -7.208316651077763204 ) ) ;
#32176 = CARTESIAN_POINT ( 'NONE',  ( 5.440088680355556150, -35.26964798917848753, 9.422509992056138373 ) ) ;
#32177 = CARTESIAN_POINT ( 'NONE',  ( 3.591859063236761518, 14.95696800326375531, 11.09922568453594849 ) ) ;
#32179 = CARTESIAN_POINT ( 'NONE',  ( 1.492507162822266142, 67.19955587570481725, -6.500000000000075495 ) ) ;
#32178 = CARTESIAN_POINT ( 'NONE',  ( 0.5774900079438607392, 13.48035201082150358, 5.440088680355550821 ) ) ;
#32180 = VECTOR ( 'NONE', #85316, 1000.000000000000114 ) ;
#32181 = CARTESIAN_POINT ( 'NONE',  ( 13.79529636645030344, 38.26208216824729647, 14.16423886937410614 ) ) ;
#32182 = CARTESIAN_POINT ( 'NONE',  ( 22.26659068614895176, 29.72041550158063572, -7.082119434687042414 ) ) ;
#32183 = CARTESIAN_POINT ( 'NONE',  ( 17.08211943468705840, 60.13708216824729647, -12.26659068614894466 ) ) ;
#32184 = CARTESIAN_POINT ( 'NONE',  ( 10.00000000000000000, 24.75893115100078745, -9.846743663894594434 ) ) ;
#32185 = CARTESIAN_POINT ( 'NONE',  ( 2.035157376598824452, 8.688685344154839285, 7.964842623401179544 ) ) ;
#32186 = AXIS2_PLACEMENT_3D ( 'NONE', #16855, #56330, #2363 ) ;
#32187 = ORIENTED_EDGE ( 'NONE', *, *, #11523, .T. ) ;
#32188 = CARTESIAN_POINT ( 'NONE',  ( 14.92337183194729633, 37.67559781766745175, 8.527530157486181039 ) ) ;
#32189 = CARTESIAN_POINT ( 'NONE',  ( 4.559911319644449179, 23.89701867748817321, 9.422509992056141925 ) ) ;
#32190 = CARTESIAN_POINT ( 'NONE',  ( 3.591859063236763294, -1.709698663402913210, -11.09922568453595026 ) ) ;
#32192 = DIRECTION ( 'NONE',  ( 0.6360782202777701677, 0.000000000000000000, -0.7716245833877148907 ) ) ;
#32191 = CARTESIAN_POINT ( 'NONE',  ( -0.3689425029237898834, 21.17874883491396432, -10.36894250292378850 ) ) ;
#32193 = CARTESIAN_POINT ( 'NONE',  ( -2.393480905992977803, 14.49999999999999112, -14.80781041047760382 ) ) ;
#32194 = UNCERTAINTY_MEASURE_WITH_UNIT (LENGTH_MEASURE( 1.000000000000000082E-05 ), #66925, 'distance_accuracy_value', 'NONE');
#32195 = CARTESIAN_POINT ( 'NONE',  ( 5.076628168052703671, 6.842264484334118713, 8.527530157486179263 ) ) ;
#32196 = CARTESIAN_POINT ( 'NONE',  ( 22.81628187352647785, 46.62363466993041783, 6.195893100308588602E-16 ) ) ;
#32197 = CARTESIAN_POINT ( 'NONE',  ( 2.791683348922237240, 55.38393115100078745, -7.208316651077763204 ) ) ;
#32198 = EDGE_LOOP ( 'NONE', ( #41111, #18850, #7307, #15867, #32539, #27315 ) ) ;
#32199 = ADVANCED_FACE ( 'NONE', ( #62213 ), #53051, .T. ) ;
#32200 = CYLINDRICAL_SURFACE ( 'NONE', #55686, 11.92686044187656513 ) ;
#32201 = LINE ( 'NONE', #85229, #31488 ) ;
#32202 = CARTESIAN_POINT ( 'NONE',  ( 15.44008868035555793, 6.397018677488171434, -9.422509992056140149 ) ) ;
#32203 = CARTESIAN_POINT ( 'NONE',  ( 20.88017736071110519, 50.56368534415484106, 2.639326808657452039E-16 ) ) ;
#32204 = CARTESIAN_POINT ( 'NONE',  ( -4.164238869374099927, 12.01208216824730357, 3.795296366450308767 ) ) ;
#32205 = CARTESIAN_POINT ( 'NONE',  ( 12.91533473730992121, 54.52201867748816255, 10.88017736071110164 ) ) ;
#32206 = CARTESIAN_POINT ( 'NONE',  ( 12.63842701281683034, 42.46726448433412315, 9.846743663894596210 ) ) ;
#32207 = CARTESIAN_POINT ( 'NONE',  ( -0.8801773607111008646, 23.27201867748817676, 2.915334737309923430 ) ) ;
#32208 = CARTESIAN_POINT ( 'NONE',  ( -3.750000000000000000, 36.75000000000000000, -2.750000000000000000 ) ) ;
#32209 = CARTESIAN_POINT ( 'NONE',  ( 0.1532563361054100626, 65.80059781766745175, -2.638427012816831230 ) ) ;
#32210 = CARTESIAN_POINT ( 'NONE',  ( 2.791683348922240793, 1.633931151000784565, 7.208316651077764092 ) ) ;
#32211 = UNCERTAINTY_MEASURE_WITH_UNIT (LENGTH_MEASURE( 1.000000000000000082E-05 ), #85381, 'distance_accuracy_value', 'NONE');
#32212 = EDGE_LOOP ( 'NONE', ( #68303, #71729, #32245, #33229 ) ) ;
#32213 = EDGE_LOOP ( 'NONE', ( #86633, #58288, #93434, #78428, #69643, #17490 ) ) ;
#32214 = CARTESIAN_POINT ( 'NONE',  ( 14.09394518620612224, 15.00000000000000000, -3.407449058785360752 ) ) ;
#32215 = DIRECTION ( 'NONE',  ( -0.9914448613738113814, 0.000000000000000000, 0.1305261922200445512 ) ) ;
#32216 =( LENGTH_UNIT ( ) NAMED_UNIT ( * ) SI_UNIT ( .MILLI., .METRE. ) );
#32217 = CARTESIAN_POINT ( 'NONE',  ( 2.917880565312950480, 45.97041550158063927, -12.26659068614894821 ) ) ;
#32218 = CARTESIAN_POINT ( 'NONE',  ( 19.84674366389459621, 43.50893115100078745, 7.409399052514197653E-17 ) ) ;
#32219 = CARTESIAN_POINT ( 'NONE',  ( 19.84674366389459266, 18.71726448433411960, -2.638427012816827677 ) ) ;
#32220 = CARTESIAN_POINT ( 'NONE',  ( 0.6178305044545838731, 64.74863466993043914, 9.382169495545420901 ) ) ;
#32222 = CARTESIAN_POINT ( 'NONE',  ( 1.472469842513823179, 45.59226448433412315, -4.923371831947296329 ) ) ;
#32221 = CARTESIAN_POINT ( 'NONE',  ( 0.5774900079438607392, 13.48035201082150358, 5.440088680355550821 ) ) ;
#32223 = CARTESIAN_POINT ( 'NONE',  ( 0.000000000000000000, 14.49999999999999822, 0.000000000000000000 ) ) ;
#32224 = CARTESIAN_POINT ( 'NONE',  ( -4.164238869374099927, 42.01208216824728936, 3.795296366450308767 ) ) ;
#32225 = CARTESIAN_POINT ( 'NONE',  ( -0.3689425029237881626, 57.42874883491397497, 10.36894250292379027 ) ) ;
#32226 = CARTESIAN_POINT ( 'NONE',  ( 5.076628168052704559, 65.17559781766745175, -8.527530157486179263 ) ) ;
#32227 = VECTOR ( 'NONE', #6812, 1000.000000000000000 ) ;
#32228 = CARTESIAN_POINT ( 'NONE',  ( 18.00000000000000000, 77.35022402048976176, 4.131279366366106487 ) ) ;
#32229 = CARTESIAN_POINT ( 'NONE',  ( 0.5774900079438607392, 48.48035201082150536, 5.440088680355550821 ) ) ;
#32230 = CARTESIAN_POINT ( 'NONE',  ( 2.791683348922240793, 21.63393115100078745, 7.208316651077764092 ) ) ;
#32231 = CARTESIAN_POINT ( 'NONE',  ( -4.139459722423826982, -8.271751626981549421, 4.000000000000000000 ) ) ;
#32232 = ORIENTED_EDGE ( 'NONE', *, *, #63452, .F. ) ;
#32233 = CARTESIAN_POINT ( 'NONE',  ( 10.83696084481538691, -98.17058944465519232, 4.000000000000000000 ) ) ;
#32234 = ADVANCED_BREP_SHAPE_REPRESENTATION ( '', ( #74465, #27931 ), #93381 ) ;
#32235 = AXIS2_PLACEMENT_3D ( 'NONE', #46075, #76563, #55033 ) ;
#32236 = ORIENTED_EDGE ( 'NONE', *, *, #39579, .T. ) ;
#32237 = CARTESIAN_POINT ( 'NONE',  ( 1.472469842513823179, 11.42559781766745175, 4.923371831947296329 ) ) ;
#32238 = ORIENTED_EDGE ( 'NONE', *, *, #39625, .F. ) ;
#32239 = CARTESIAN_POINT ( 'NONE',  ( -0.3689425029237881626, 17.42874883491397142, 10.36894250292379027 ) ) ;
#32240 = CARTESIAN_POINT ( 'NONE',  ( 10.00000000000000000, 14.75893115100078568, -9.846743663894594434 ) ) ;
#32241 = CARTESIAN_POINT ( 'NONE',  ( 17.96484262340118221, 46.18868534415484106, -7.964842623401177768 ) ) ;
#32242 = VERTEX_POINT ( 'NONE', #51904 ) ;
#32243 = CARTESIAN_POINT ( 'NONE',  ( 0.5774900079438607392, 38.48035201082150536, 5.440088680355550821 ) ) ;
#32244 = CARTESIAN_POINT ( 'NONE',  ( -12.81628187352647608, -5.876365330069576842, 3.903127820947815962E-15 ) ) ;
#32245 = ORIENTED_EDGE ( 'NONE', *, *, #57243, .F. ) ;
#32246 = CARTESIAN_POINT ( 'NONE',  ( 12.91533473730993009, 46.60535201082150536, -10.88017736071109987 ) ) ;
#32247 = CARTESIAN_POINT ( 'NONE',  ( 13.79529636645030344, 13.26208216824729824, 14.16423886937410614 ) ) ;
#32248 = VERTEX_POINT ( 'NONE', #96434 ) ;
#32249 = ORIENTED_EDGE ( 'NONE', *, *, #98486, .F. ) ;
#32250 = CARTESIAN_POINT ( 'NONE',  ( 6.565887622018943937, 25.16530133659708213, 12.81628187352647430 ) ) ;
#32251 = CARTESIAN_POINT ( 'NONE',  ( 10.00000000000000000, 0.5537488349139675359, -14.16423886937410082 ) ) ;
#32252 = CARTESIAN_POINT ( 'NONE',  ( 14.92337183194729988, 4.342264484334117824, -8.527530157486177487 ) ) ;
#32253 = CARTESIAN_POINT ( 'NONE',  ( 17.96484262340118221, 6.188685344154836621, -7.964842623401177768 ) ) ;
#32254 = CARTESIAN_POINT ( 'NONE',  ( 19.10478245763048477, 11.02576239577082262, -5.990408912944377384 ) ) ;
#32255 = CARTESIAN_POINT ( 'NONE',  ( 17.20831665107776587, 14.13393115100078568, -7.208316651077762316 ) ) ;
#32256 = CARTESIAN_POINT ( 'NONE',  ( -0.8801773607110991993, 42.85535201082150536, -2.915334737309923874 ) ) ;
#32257 = EDGE_CURVE ( 'NONE', #1146, #13064, #60377, .T. ) ;
#32258 = ORIENTED_EDGE ( 'NONE', *, *, #27217, .T. ) ;
#32259 = ORIENTED_EDGE ( 'NONE', *, *, #32079, .T. ) ;
#32260 = DIRECTION ( 'NONE',  ( 0.000000000000000000, -1.000000000000000000, 0.000000000000000000 ) ) ;
#32261 = CARTESIAN_POINT ( 'NONE',  ( 17.96484262340118221, 56.18868534415484817, -7.964842623401177768 ) ) ;
#32262 = CARTESIAN_POINT ( 'NONE',  ( 2.189666204609191702, 15.00000000000000888, 14.46180170876167992 ) ) ;
#32263 = CARTESIAN_POINT ( 'NONE',  ( 16.40814093676324603, 62.45696800326376064, -11.09922568453594671 ) ) ;
#32264 = CARTESIAN_POINT ( 'NONE',  ( 12.91533473730992121, 59.52201867748816966, 10.88017736071110164 ) ) ;
#32265 = CARTESIAN_POINT ( 'NONE',  ( 12.00809552683952752, 0.5000000000000004441, 8.989195838243626113 ) ) ;
#32266 = CARTESIAN_POINT ( 'NONE',  ( 7.361572987183170547, 32.05059781766745175, 9.846743663894590881 ) ) ;
#32267 = FACE_OUTER_BOUND ( 'NONE', #80814, .T. ) ;
#32268 = CARTESIAN_POINT ( 'NONE',  ( 10.00000000000000178, 3.053748834913967425, 14.16423886937410082 ) ) ;
#32269 = CARTESIAN_POINT ( 'NONE',  ( 10.00000000000000178, 17.25893115100078745, 9.846743663894594434 ) ) ;
#32270 = CARTESIAN_POINT ( 'NONE',  ( 19.38216949554541202, 25.99863466993042138, 9.382169495545424454 ) ) ;
#32272 = DIRECTION ( 'NONE',  ( -0.000000000000000000, -1.000000000000000000, -0.000000000000000000 ) ) ;
#32271 = DIRECTION ( 'NONE',  ( -0.000000000000000000, 0.000000000000000000, 1.000000000000000000 ) ) ;
#32273 = CARTESIAN_POINT ( 'NONE',  ( 20.88017736071110875, 55.77201867748816966, -2.915334737309920765 ) ) ;
#32274 = EDGE_CURVE ( 'NONE', #59804, #717, #47355, .T. ) ;
#32275 = CARTESIAN_POINT ( 'NONE',  ( 0.1532563361054100626, 65.80059781766745175, -2.638427012816831230 ) ) ;
#32276 = CARTESIAN_POINT ( 'NONE',  ( 1.354709868695515684, 0.5000000000000004441, 14.93870011653152652 ) ) ;
#32277 = CARTESIAN_POINT ( 'NONE',  ( 14.92337183194729988, 19.34226448433411960, -8.527530157486177487 ) ) ;
#32278 = CARTESIAN_POINT ( 'NONE',  ( 7.084665262690076126, 14.10535201082150358, 10.88017736071109987 ) ) ;
#32279 = CARTESIAN_POINT ( 'NONE',  ( 3.591859063236763294, 13.29030133659708746, -11.09922568453595026 ) ) ;
#32280 = VECTOR ( 'NONE', #94741, 1000.000000000000114 ) ;
#32281 = CARTESIAN_POINT ( 'NONE',  ( 12.63842701281683922, 24.55059781766745175, -9.846743663894590881 ) ) ;
#32282 = CARTESIAN_POINT ( 'NONE',  ( -7.750355510519348456, 84.07179676972448590, 4.000000000000000000 ) ) ;
#32283 = ADVANCED_FACE ( 'NONE', ( #73902 ), #13830, .T. ) ;
#32284 = CARTESIAN_POINT ( 'NONE',  ( -0.8801773607111008646, 18.27201867748817321, 2.915334737309923430 ) ) ;
#32285 = EDGE_CURVE ( 'NONE', #50081, #74944, #39646, .T. ) ;
#32286 = ORIENTED_EDGE ( 'NONE', *, *, #62760, .F. ) ;
#32287 = VECTOR ( 'NONE', #47759, 1000.000000000000000 ) ;
#32288 = FACE_OUTER_BOUND ( 'NONE', #46282, .T. ) ;
#32290 = CARTESIAN_POINT ( 'NONE',  ( 12.91533473730992121, 14.52201867748817143, 10.88017736071110164 ) ) ;
#32289 = CARTESIAN_POINT ( 'NONE',  ( 17.20831665107776587, 47.88393115100078745, 7.208316651077764980 ) ) ;
#32291 = AXIS2_PLACEMENT_3D ( 'NONE', #17624, #41610, #64561 ) ;
#32292 = CARTESIAN_POINT ( 'NONE',  ( 7.084665262690076126, 49.10535201082149825, 10.88017736071109987 ) ) ;
#32294 = DIRECTION ( 'NONE',  ( 0.000000000000000000, 0.000000000000000000, 1.000000000000000000 ) ) ;
#32293 = CARTESIAN_POINT ( 'NONE',  ( 2.035157376598824452, 18.68868534415484106, 7.964842623401179544 ) ) ;
#32295 = CARTESIAN_POINT ( 'NONE',  ( 18.52753015748618282, 8.925597817667451750, -4.923371831947291888 ) ) ;
#32296 = PRESENTATION_LAYER_ASSIGNMENT (  '', '', ( #72206 ) ) ;
#32297 = CARTESIAN_POINT ( 'NONE',  ( 7.361572987183170547, 42.05059781766745886, 9.846743663894590881 ) ) ;
#32298 = DIRECTION ( 'NONE',  ( 5.782411586589362323E-17, 1.000000000000000000, -0.000000000000000000 ) ) ;
#32299 = DIRECTION ( 'NONE',  ( 0.000000000000000000, 0.000000000000000000, 1.000000000000000000 ) ) ;
#32300 = CARTESIAN_POINT ( 'NONE',  ( 10.00000000000000178, 67.25893115100079456, 9.846743663894594434 ) ) ;
#32301 = CARTESIAN_POINT ( 'NONE',  ( 2.917880565312950480, 0.9704155015806342766, -12.26659068614894821 ) ) ;
#32303 = CIRCLE ( 'NONE', #48295, 14.49999999999999822 ) ;
#32302 = CARTESIAN_POINT ( 'NONE',  ( 20.36894250292379382, 28.67874883491396787, 10.36894250292379205 ) ) ;
#32304 = CARTESIAN_POINT ( 'NONE',  ( 0.1532563361054083140, 36.00893115100078745, 1.131784320476157264E-15 ) ) ;
#32305 = DIRECTION ( 'NONE',  ( -0.9969173337331274087, 0.000000000000000000, -0.07845909572785238206 ) ) ;
#32306 = ORIENTED_EDGE ( 'NONE', *, *, #64407, .T. ) ;
#32307 = CARTESIAN_POINT ( 'NONE',  ( 24.16423886937410614, 49.30374883491396787, 8.672049930838204340E-16 ) ) ;
#32308 = CARTESIAN_POINT ( 'NONE',  ( 7.361572987183169658, 19.96726448433411960, -9.846743663894592657 ) ) ;
#32310 = CARTESIAN_POINT ( 'NONE',  ( -9.343156623282764528, 88.41679554545851261, -5.273290232418045953 ) ) ;
#32309 = CARTESIAN_POINT ( 'NONE',  ( 0.2751277870542889192, 28.21833443783938122, 6.499999999999990230 ) ) ;
#32311 = CARTESIAN_POINT ( 'NONE',  ( -0.8801773607111009756, 48.06368534415484817, 1.068504757029289695E-15 ) ) ;
#32312 = CARTESIAN_POINT ( 'NONE',  ( 0.6178305044545818747, 63.49863466993043204, -9.382169495545419124 ) ) ;
#32313 = CARTESIAN_POINT ( 'NONE',  ( 10.00000000000000000, 11.81368534415483751, -10.88017736071110342 ) ) ;
#32314 = CARTESIAN_POINT ( 'NONE',  ( -1.099225684535947600, 54.54030133659708923, 6.408140936763237150 ) ) ;
#32315 = CARTESIAN_POINT ( 'NONE',  ( 16.40814093676324603, 17.45696800326375353, -11.09922568453594671 ) ) ;
#32316 = CARTESIAN_POINT ( 'NONE',  ( 17.39651004071842166, 12.93575266056827822, 6.499999999999998224 ) ) ;
#32317 = CARTESIAN_POINT ( 'NONE',  ( 0.1532563361054100626, 10.80059781766745175, -2.638427012816831230 ) ) ;
#32318 = ORIENTED_EDGE ( 'NONE', *, *, #47770, .T. ) ;
#32319 = CARTESIAN_POINT ( 'NONE',  ( 1.780824192092501423, 15.00000000000000000, -14.89391369643513485 ) ) ;
#32320 = EDGE_CURVE ( 'NONE', #80097, #78251, #35905, .T. ) ;
#32321 = DIRECTION ( 'NONE',  ( -0.000000000000000000, 1.000000000000000000, -0.000000000000000000 ) ) ;
#32322 = CARTESIAN_POINT ( 'NONE',  ( 2.917880565312950480, 50.97041550158064638, -12.26659068614894821 ) ) ;
#32323 = CARTESIAN_POINT ( 'NONE',  ( 24.16423886937410614, 29.30374883491396787, 8.672049930838204340E-16 ) ) ;
#32324 = CARTESIAN_POINT ( 'NONE',  ( 0.5774900079438590739, 17.64701867748817321, -5.440088680355550821 ) ) ;
#32325 = CARTESIAN_POINT ( 'NONE',  ( 12.91533473730993009, 36.60535201082151247, -10.88017736071109987 ) ) ;
#32326 = CARTESIAN_POINT ( 'NONE',  ( -46.58162315985163815, 100.7785275715626057, -9.484706478859457945 ) ) ;
#32327 = CARTESIAN_POINT ( 'NONE',  ( 5.076628168052703671, 1.842264484334118047, 8.527530157486179263 ) ) ;
#32328 = CARTESIAN_POINT ( 'NONE',  ( 0.1532563361054082862, 21.21726448433412315, 2.638427012816831674 ) ) ;
#32329 = CARTESIAN_POINT ( 'NONE',  ( 5.500000000000000000, 10.49999999999999822, 6.000000000000000000 ) ) ;
#32330 = SURFACE_STYLE_FILL_AREA ( #78328 ) ;
#32331 = CARTESIAN_POINT ( 'NONE',  ( 1.472469842513823179, 20.59226448433411960, -4.923371831947296329 ) ) ;
#32332 = CARTESIAN_POINT ( 'NONE',  ( 0.1532563361054083140, 41.00893115100078745, 1.131784320476157264E-15 ) ) ;
#32333 = CARTESIAN_POINT ( 'NONE',  ( 7.084665262690076126, 12.02201867748817143, -10.88017736071110164 ) ) ;
#32334 = EDGE_CURVE ( 'NONE', #1572, #29895, #18609, .T. ) ;
#32335 = UNCERTAINTY_MEASURE_WITH_UNIT (LENGTH_MEASURE( 1.000000000000000082E-05 ), #55165, 'distance_accuracy_value', 'NONE');
#32336 =( BOUNDED_CURVE ( )  B_SPLINE_CURVE ( 3, ( #22852, #76330, #53830, #98374 ),
 .UNSPECIFIED., .F., .F. ) 
 B_SPLINE_CURVE_WITH_KNOTS ( ( 4, 4 ),
 ( 1.570796326794896558, 2.588785175020066109 ),
 .UNSPECIFIED. ) 
 CURVE ( )  GEOMETRIC_REPRESENTATION_ITEM ( )  RATIONAL_B_SPLINE_CURVE ( ( 1.000000000000000000, 0.9154899770527740177, 0.9154899770527740177, 1.000000000000000000 ) ) 
 REPRESENTATION_ITEM ( '' )  );
#32337 = AXIS2_PLACEMENT_3D ( 'NONE', #94858, #70405, #55394 ) ;
#32338 = CARTESIAN_POINT ( 'NONE',  ( 19.38216949554541202, 30.99863466993042138, 9.382169495545424454 ) ) ;
#32339 = CARTESIAN_POINT ( 'NONE',  ( 20.88017736071110519, 50.56368534415484106, 2.639326808657452039E-16 ) ) ;
#32341 = CARTESIAN_POINT ( 'NONE',  ( 19.84674366389459266, 8.300597817667451750, 2.638427012816836559 ) ) ;
#32340 = CARTESIAN_POINT ( 'NONE',  ( 13.79529636645031943, 45.34541550158062506, -14.16423886937409904 ) ) ;
#32342 = CARTESIAN_POINT ( 'NONE',  ( 0.000000000000000000, 15.00000000000000000, 0.000000000000000000 ) ) ;
#32343 = CARTESIAN_POINT ( 'NONE',  ( 0.1532563361054100626, 50.80059781766745175, -2.638427012816831230 ) ) ;
#32345 = CARTESIAN_POINT ( 'NONE',  ( 22.26659068614894466, 13.88708216824730179, 7.082119434687054849 ) ) ;
#32344 = CARTESIAN_POINT ( 'NONE',  ( 0.1532563361054082862, 26.21726448433411605, 2.638427012816831674 ) ) ;
#32346 = CARTESIAN_POINT ( 'NONE',  ( -0.3689425029237881626, 12.42874883491396609, 10.36894250292379027 ) ) ;
#32347 = CARTESIAN_POINT ( 'NONE',  ( 1.472469842513823179, 35.59226448433412315, -4.923371831947296329 ) ) ;
#32348 = CARTESIAN_POINT ( 'NONE',  ( 19.42250999205614193, 45.14701867748817676, 5.440088680355555262 ) ) ;
#32349 = CARTESIAN_POINT ( 'NONE',  ( 15.44008868035555793, 16.39701867748817321, -9.422509992056140149 ) ) ;
#32350 = CARTESIAN_POINT ( 'NONE',  ( 7.084665262690076126, 52.02201867748816255, -10.88017736071110164 ) ) ;
#32351 = CARTESIAN_POINT ( 'NONE',  ( 2.035157376598822676, 27.43868534415483396, -7.964842623401177768 ) ) ;
#32352 = ORIENTED_EDGE ( 'NONE', *, *, #55136, .T. ) ;
#32353 = CARTESIAN_POINT ( 'NONE',  ( 20.88017736071110519, 35.56368534415484106, 2.639326808657452039E-16 ) ) ;
#32354 = ORIENTED_EDGE ( 'NONE', *, *, #86519, .F. ) ;
#32355 = CARTESIAN_POINT ( 'NONE',  ( 6.565887622018943937, 65.16530133659709634, 12.81628187352647430 ) ) ;
#32356 = CARTESIAN_POINT ( 'NONE',  ( 0.5774900079438607392, 68.48035201082150536, 5.440088680355550821 ) ) ;
#32357 = ORIENTED_EDGE ( 'NONE', *, *, #68238, .T. ) ;
#32358 = CARTESIAN_POINT ( 'NONE',  ( 4.559911319644449179, 48.89701867748817676, 9.422509992056141925 ) ) ;
#32359 = CARTESIAN_POINT ( 'NONE',  ( 2.035157376598822676, 7.438685344154837509, -7.964842623401177768 ) ) ;
#32360 = CARTESIAN_POINT ( 'NONE',  ( 1.350000000000004086, 98.49999999999998579, -8.525133428036873795 ) ) ;
#32361 = CARTESIAN_POINT ( 'NONE',  ( 2.917880565312948704, 62.63708216824730357, 12.26659068614894643 ) ) ;
#32363 = VERTEX_POINT ( 'NONE', #66900 ) ;
#32362 = CARTESIAN_POINT ( 'NONE',  ( 0.5774900079438590739, 62.64701867748817676, -5.440088680355550821 ) ) ;
#32364 = AXIS2_PLACEMENT_3D ( 'NONE', #98226, #75697, #7208 ) ;
#32365 = CARTESIAN_POINT ( 'NONE',  ( 7.361572987183169658, 9.967264484334119601, -9.846743663894592657 ) ) ;
#32366 = COLOUR_RGB ( '', 0.66274510, 0.83137255, 0.94901961) ;
#32367 = CARTESIAN_POINT ( 'NONE',  ( 0.5774900079438590739, 12.64701867748817143, -5.440088680355550821 ) ) ;
#32368 = CARTESIAN_POINT ( 'NONE',  ( 12.63842701281683922, 49.55059781766744464, -9.846743663894590881 ) ) ;
#32369 = ORIENTED_EDGE ( 'NONE', *, *, #30268, .F. ) ;
#32370 = CARTESIAN_POINT ( 'NONE',  ( 2.791683348922237240, 50.38393115100078035, -7.208316651077763204 ) ) ;
#32371 =( GEOMETRIC_REPRESENTATION_CONTEXT ( 3 ) GLOBAL_UNCERTAINTY_ASSIGNED_CONTEXT ( ( #17126 ) ) GLOBAL_UNIT_ASSIGNED_CONTEXT ( ( #1365, #71317, #3806 ) ) REPRESENTATION_CONTEXT ( 'NONE', 'WORKASPACE' ) );
#32372 = CARTESIAN_POINT ( 'NONE',  ( 17.96484262340118221, 36.18868534415484106, -7.964842623401177768 ) ) ;
#32373 = CARTESIAN_POINT ( 'NONE',  ( 19.84674366389459266, 53.71726448433411605, -2.638427012816827677 ) ) ;
#32374 = CARTESIAN_POINT ( 'NONE',  ( 10.00000000000000178, 30.37363466993042138, 12.81628187352647608 ) ) ;
#32376 = DIRECTION ( 'NONE',  ( -1.224646799147353207E-16, 1.540077580099091490E-33, 1.000000000000000000 ) ) ;
#32375 = DIRECTION ( 'NONE',  ( 0.5547001962252290364, 0.8320502943378437211, 0.000000000000000000 ) ) ;
#32377 = CARTESIAN_POINT ( 'NONE',  ( 20.88017736071110164, 40.35535201082150536, 2.915334737309930979 ) ) ;
#32378 = CARTESIAN_POINT ( 'NONE',  ( -4.164238869374099039, 56.80374883491397497, 8.674139862899312516E-16 ) ) ;
#32379 = ADVANCED_FACE ( 'NONE', ( #83388 ), #49833, .T. ) ;
#32380 = CARTESIAN_POINT ( 'NONE',  ( 13.43411237798106583, 22.66530133659708923, -12.81628187352647252 ) ) ;
#32381 = CARTESIAN_POINT ( 'NONE',  ( 0.000000000000000000, 0.000000000000000000, 0.000000000000000000 ) ) ;
#32382 = VERTEX_POINT ( 'NONE', #17382 ) ;
#32383 = CARTESIAN_POINT ( 'NONE',  ( 3.591859063236763294, 33.29030133659708213, -11.09922568453595026 ) ) ;
#32384 = CARTESIAN_POINT ( 'NONE',  ( 0.5774900079438590739, 27.64701867748817676, -5.440088680355550821 ) ) ;
#32385 = EDGE_LOOP ( 'NONE', ( #79342, #58498, #36456, #48535 ) ) ;
#32386 = TOROIDAL_SURFACE ( 'NONE', #88283, 14.49999999999999822, 0.5000000000000000000 ) ;
#32387 = CARTESIAN_POINT ( 'NONE',  ( 17.96484262340118221, 64.93868534415483396, 7.964842623401181321 ) ) ;
#32388 = CARTESIAN_POINT ( 'NONE',  ( 14.92337183194729988, 44.34226448433412315, -8.527530157486177487 ) ) ;
#32390 = CARTESIAN_POINT ( 'NONE',  ( 17.20831665107776587, 42.88393115100077324, 7.208316651077764980 ) ) ;
#32389 = CARTESIAN_POINT ( 'NONE',  ( 17.20831665107776587, 14.13393115100078568, -7.208316651077762316 ) ) ;
#32391 = LINE ( 'NONE', #10887, #8993 ) ;
#32392 =( LENGTH_UNIT ( ) NAMED_UNIT ( * ) SI_UNIT ( .MILLI., .METRE. ) );
#32393 = CARTESIAN_POINT ( 'NONE',  ( 1.472469842513823179, 26.42559781766745175, 4.923371831947296329 ) ) ;
#32394 = CARTESIAN_POINT ( 'NONE',  ( -14.71525861348291819, 14.49999999999999112, -2.908807992686814003 ) ) ;
#32395 = DIRECTION ( 'NONE',  ( 0.000000000000000000, -1.000000000000000000, 0.000000000000000000 ) ) ;
#32396 = CIRCLE ( 'NONE', #11714, 11.99999999999999645 ) ;
#32397 = CARTESIAN_POINT ( 'NONE',  ( 19.84674366389459266, 23.30059781766745530, 2.638427012816836559 ) ) ;
#32398 = FACE_BOUND ( 'NONE', #16560, .T. ) ;
#32400 = ORIENTED_EDGE ( 'NONE', *, *, #32680, .T. ) ;
#32399 = CARTESIAN_POINT ( 'NONE',  ( 2.791683348922237240, 50.38393115100078035, -7.208316651077763204 ) ) ;
#32401 =( BOUNDED_SURFACE ( )  B_SPLINE_SURFACE ( 1, 2, ( 
 ( #78523, #40039, #94017, #54526, #54047, #63513, #40538, #24561, #70540, #48508, #31535, #61542, #70045, #84558, #92051, #32018, #92531, #2558, #16058, #39062, #47031, #47531, #16557, #78033, #1072, #32524, #85042, #55537, #9535, #55022, #86033, #62031, #63023, #77525, #17546, #2062, #85539, #48014, #17051, #69555, #93523, #79011, #10035, #93025, #25051, #71036, #33014, #25539, #23578, #56030, #46546, #86527, #18027, #10516, #62521, #41030, #9042, #71532, #77046, #24061, #8559, #39556, #1569, #11497, #72979, #79994, #35474, #12971, #56993, #49487, #71997, #57973, #34479, #33980, #4508, #80982, #95498, #26989, #43464, #88978, #95997, #3522, #88479, #27480, #18514, #57488, #34974, #94501, #20485, #41529, #26020, #33493, #96497, #63991, #11012, #65471, #42494, #50479, #64483, #94991, #26496, #87982, #65970, #50973, #19011, #4017, #19493, #49988, #81466, #56515, #73466, #73966, #87005, #42018, #80495, #4993, #87496, #27970, #12482, #58463, #49003, #79510, #72483, #64972, #19981, #11993, #42985, #36472, #75943, #66466, #83449, #44454, #52453, #97984, #74955, #22463, #82956, #37966, #97485, #96996, #7469, #14971, #67463, #14469, #91439, #74452, #45949, #13979, #28473, #5495, #6458, #66966, #45441, #58970, #81958, #89955, #90435, #59454, #21976, #37470, #98483, #60442, #15468, #59945, #43953, #68456, #44944, #28952, #98978, #30431, #13472, #89467, #82456, #90935, #60933, #29938, #75449, #6962, #22965, #20983, #21471, #51469, #36967, #5980, #51970, #52939, #53431, #29441, #67960, #83940, #35967, #17427, #2437, #8920, #9919, #76924, #476, #47896, #70422, #16434, #17909, #62398, #16927, #93403, #38941, #84924, #39435, #31412, #78399, #32895, #46430, #91932, #69929, #68945, #7954, #31901, #46912, #9417, #92906, #8434, #1941, #55908, #24436, #1449, #69430, #54902, #86407, #38449, #951, #61915, #92419, #53935, #40423, #77906, #84443, #85416, #25426, #24929, #76438, #54412, #77405, #70917, #47404, #32399, #30923, #23944, #39919, #62903, #61422, #23459, #55410, #15940, #85916, #63393, #93898, #4390, #35356, #4877, #96378, #48393, #49374, #63871, #34857, #79876, #11380, #56876, #80865, #71881, #87378, #94383, #19379, #27849, #42869, #10404, #49862, #41420, #18397, #88855, #64368, #58337, #72856, #25900, #50354, #18894, #12363, #95372, #48879, #94877, #78895, #65352, #56401, #73353, #41901, #65848, #26871, #79389, #80375, #42379, #95880, #40911, #3894, #86887, #57854, #34362, #10895, #27361, #71410, #3397, #33375, #26377, #88365, #19861, #2927, #11874, #33859, #72362, #64853, #57367, #87862, #97362, #66338, #43346, #44819, #14349, #20859 ),
 ( #98858, #75824, #82828, #89349, #75326, #6839, #5374, #13851, #21854, #81352, #7346, #28352, #12848, #20364, #83329, #50858, #96876, #90316, #29325, #37353, #58842, #81833, #13349, #74834, #22349, #37846, #5854, #89834, #44329, #36847, #68337, #73845, #60329, #30313, #60813, #28831, #6337, #90820, #43833, #14855, #67844, #45327, #35850, #51350, #52822, #74329, #98362, #36346, #66841, #59331, #21350, #51842, #29820, #82329, #67337, #97862, #59822, #52335, #69815, #24811, #84332, #83824, #93286, #70310, #54297, #1338, #78283, #61308, #32775, #839, #15350, #91313, #61799, #23340, #32279, #45834, #68831, #76805, #77294, #46319, #8807, #7838, #40297, #53820, #62787, #53316, #1826, #31299, #39319, #84812, #92307, #9299, #31789, #55287, #15832, #76320, #85797, #17309, #16318, #62288, #9798, #91819, #22841, #23834, #38337, #361, #46802, #8323, #47786, #30811, #38826, #69318, #92792, #24321, #54787, #85304, #16810, #47286, #77787, #39809, #70805, #2322, #26263, #40790, #11261, #80746, #57247, #94763, #56761, #18780, #34237, #80249, #4760, #42264, #93779, #49262, #87744, #64733, #64245, #87255, #48763, #41780, #11755, #33266, #79763, #33744, #79270, #41297, #3783, #10780, #65230, #42751, #86781, #71770, #2814, #19257, #72249, #63759, #95245, #72733, #26752, #49741, #73232, #19748, #4266, #94264, #34739, #95756, #48271, #27240, #57736, #25307, #50232, #71289, #55793, #63271, #88239, #86288, #25790, #12241, #17796, #78785, #56285, #18284, #3281, #10292, #91578, #15594, #28228, #81717, #7096, #98620, #46077, #35231, #61067, #76566, #65729, #14612, #30069, #23095, #96754, #84079, #68585, #8083, #38579, #96256, #53565, #5256, #7602, #53073, #38098, #88732, #35735, #58727, #66223, #27734, #58217, #69076, #20244, #22596, #60578, #91070, #50747, #81235, #12734, #43231, #73725, #116, #75584, #89231, #30562, #20740, #51233, #45079, #37598, #68092, #83585, #15102, #45578, #76072, #61297, #91302, #91806, #60802, #23328, #45315, #76794, #98846, #828, #53809, #350, #31288, #68817, #83318, #84319, #24310, #61786, #38323, #30797, #15820, #8310, #23820, #47274, #84798, #37343, #46308, #92296, #38813, #7827, #69306, #22829, #54283, #16307, #75812, #46789, #76309, #53305, #83813, #77282, #15339, #8793, #85291, #30300, #45822, #7334, #39310, #69803, #37835, #1326, #31778, #62273, #92779, #16798, #54775, #6829, #68326, #67833, #98351, #90809, #29809, #60318, #22337, #52811, #14843, #70297, #77775, #41767, #9288, #55275, #48751, #86769, #94751, #17298, #40284, #70792, #33256, #79751, #34225, #63259, #48260, #2801, #94252, #64722, #39797, #18769 ) ),
 .UNSPECIFIED., .F., .F., .T. ) 
 B_SPLINE_SURFACE_WITH_KNOTS ( ( 2, 2 ),
 ( 3, 2, 2, 2, 2, 2, 2, 2, 2, 2, 2, 2, 2, 2, 2, 2, 2, 2, 2, 2, 2, 2, 2, 2, 2, 2, 2, 2, 2, 2, 2, 2, 2, 2, 2, 2, 2, 2, 2, 2, 2, 2, 2, 2, 2, 2, 2, 2, 2, 2, 2, 2, 2, 2, 2, 2, 2, 2, 2, 2, 2, 2, 2, 2, 2, 2, 2, 2, 2, 2, 2, 2, 2, 2, 2, 2, 2, 2, 2, 2, 2, 2, 2, 2, 2, 2, 2, 2, 2, 2, 2, 2, 2, 2, 2, 2, 2, 2, 2, 2, 2, 2, 2, 2, 2, 2, 2, 2, 2, 2, 2, 2, 2, 2, 2, 2, 2, 2, 2, 2, 2, 2, 2, 2, 2, 2, 2, 2, 2, 2, 2, 2, 2, 2, 2, 2, 2, 2, 2, 2, 2, 2, 2, 2, 2, 2, 2, 2, 2, 2, 2, 2, 2, 2, 2, 2, 2, 2, 2, 2, 2, 2, 3 ),
 ( 0.000000000000000000, 1.000000000000000000 ),
 ( 0.000000000000000000, 0.005952380952380952051, 0.01190476190476190410, 0.01785714285714285615, 0.02380952380952380820, 0.02976190476190476025, 0.03571428571428571230, 0.04166666666666666435, 0.04761904761904761640, 0.05357142857142856845, 0.05952380952380952051, 0.06547619047619047949, 0.07142857142857142461, 0.07738095238095238360, 0.08333333333333332871, 0.08928571428571428770, 0.09523809523809523281, 0.1011904761904761918, 0.1071428571428571369, 0.1130952380952380959, 0.1190476190476190410, 0.1250000000000000000, 0.1309523809523809590, 0.1369047619047619180, 0.1428571428571428492, 0.1488095238095238082, 0.1547619047619047672, 0.1607142857142857262, 0.1666666666666666574, 0.1726190476190476164, 0.1785714285714285754, 0.1845238095238095344, 0.1904761904761904656, 0.1964285714285714246, 0.2023809523809523836, 0.2083333333333333426, 0.2142857142857142738, 0.2202380952380952328, 0.2261904761904761918, 0.2321428571428571508, 0.2380952380952380820, 0.2440476190476190410, 0.2500000000000000000, 0.2559523809523809312, 0.2619047619047619180, 0.2678571428571428492, 0.2738095238095238360, 0.2797619047619047672, 0.2857142857142856984, 0.2916666666666666852, 0.2976190476190476164, 0.3035714285714285476, 0.3095238095238095344, 0.3154761904761904656, 0.3214285714285714524, 0.3273809523809523836, 0.3333333333333333148, 0.3392857142857143016, 0.3452380952380952328, 0.3511904761904761640, 0.3571428571428571508, 0.3630952380952380820, 0.3690476190476190688, 0.3750000000000000000, 0.3809523809523809312, 0.3869047619047619180, 0.3928571428571428492, 0.3988095238095238360, 0.4047619047619047672, 0.4107142857142856984, 0.4166666666666666852, 0.4226190476190476164, 0.4285714285714285476, 0.4345238095238095344, 0.4404761904761904656, 0.4464285714285714524, 0.4523809523809523836, 0.4583333333333333148, 0.4642857142857143016, 0.4702380952380952328, 0.4761904761904761640, 0.4821428571428571508, 0.4880952380952380820, 0.4940476190476190688, 0.5000000000000000000, 0.5059523809523809312, 0.5119047619047618625, 0.5178571428571429047, 0.5238095238095238360, 0.5297619047619047672, 0.5357142857142856984, 0.5416666666666666297, 0.5476190476190476719, 0.5535714285714286031, 0.5595238095238095344, 0.5654761904761904656, 0.5714285714285713969, 0.5773809523809523281, 0.5833333333333333703, 0.5892857142857143016, 0.5952380952380952328, 0.6011904761904761640, 0.6071428571428570953, 0.6130952380952381375, 0.6190476190476190688, 0.6250000000000000000, 0.6309523809523809312, 0.6369047619047618625, 0.6428571428571429047, 0.6488095238095238360, 0.6547619047619047672, 0.6607142857142856984, 0.6666666666666666297, 0.6726190476190476719, 0.6785714285714286031, 0.6845238095238095344, 0.6904761904761904656, 0.6964285714285713969, 0.7023809523809523281, 0.7083333333333333703, 0.7142857142857143016, 0.7202380952380952328, 0.7261904761904761640, 0.7321428571428570953, 0.7380952380952381375, 0.7440476190476190688, 0.7500000000000000000, 0.7559523809523809312, 0.7619047619047618625, 0.7678571428571429047, 0.7738095238095238360, 0.7797619047619047672, 0.7857142857142856984, 0.7916666666666666297, 0.7976190476190476719, 0.8035714285714286031, 0.8095238095238095344, 0.8154761904761904656, 0.8214285714285713969, 0.8273809523809523281, 0.8333333333333333703, 0.8392857142857143016, 0.8452380952380952328, 0.8511904761904761640, 0.8571428571428570953, 0.8630952380952381375, 0.8690476190476190688, 0.8750000000000000000, 0.8809523809523809312, 0.8869047619047618625, 0.8928571428571429047, 0.8988095238095238360, 0.9047619047619047672, 0.9107142857142856984, 0.9166666666666666297, 0.9226190476190476719, 0.9285714285714286031, 0.9345238095238095344, 0.9404761904761904656, 0.9464285714285713969, 0.9523809523809523281, 0.9583333333333333703, 0.9642857142857143016 ),
 .UNSPECIFIED. ) 
 GEOMETRIC_REPRESENTATION_ITEM ( )  RATIONAL_B_SPLINE_SURFACE ( (
 ( 1.000000000000000000, 0.9659258262890683122, 1.000000000000000000, 0.9659258262890683122, 1.000000000000000000, 0.9659258262890683122, 1.000000000000000000, 0.9659258262890683122, 1.000000000000000000, 0.9659258262890683122, 1.000000000000000000, 0.9659258262890683122, 1.000000000000000000, 0.9659258262890683122, 1.000000000000000000, 0.9659258262890683122, 1.000000000000000000, 0.9659258262890683122, 1.000000000000000000, 0.9659258262890683122, 1.000000000000000000, 0.9659258262890683122, 1.000000000000000000, 0.9659258262890683122, 1.000000000000000000, 0.9659258262890683122, 1.000000000000000000, 0.9659258262890683122, 1.000000000000000000, 0.9659258262890683122, 1.000000000000000000, 0.9659258262890683122, 1.000000000000000000, 0.9659258262890683122, 1.000000000000000000, 0.9659258262890683122, 1.000000000000000000, 0.9659258262890683122, 1.000000000000000000, 0.9659258262890683122, 1.000000000000000000, 0.9659258262890683122, 1.000000000000000000, 0.9659258262890683122, 1.000000000000000000, 0.9659258262890683122, 1.000000000000000000, 0.9659258262890683122, 1.000000000000000000, 0.9659258262890683122, 1.000000000000000000, 0.9659258262890683122, 1.000000000000000000, 0.9659258262890683122, 1.000000000000000000, 0.9659258262890683122, 1.000000000000000000, 0.9659258262890683122, 1.000000000000000000, 0.9659258262890683122, 1.000000000000000000, 0.9659258262890683122, 1.000000000000000000, 0.9659258262890683122, 1.000000000000000000, 0.9659258262890683122, 1.000000000000000000, 0.9659258262890683122, 1.000000000000000000, 0.9659258262890683122, 1.000000000000000000, 0.9659258262890683122, 1.000000000000000000, 0.9659258262890683122, 1.000000000000000000, 0.9659258262890683122, 1.000000000000000000, 0.9659258262890683122, 1.000000000000000000, 0.9659258262890683122, 1.000000000000000000, 0.9659258262890683122, 1.000000000000000000, 0.9659258262890683122, 1.000000000000000000, 0.9659258262890683122, 1.000000000000000000, 0.9659258262890683122, 1.000000000000000000, 0.9659258262890683122, 1.000000000000000000, 0.9659258262890683122, 1.000000000000000000, 0.9659258262890683122, 1.000000000000000000, 0.9659258262890683122, 1.000000000000000000, 0.9659258262890683122, 1.000000000000000000, 0.9659258262890683122, 1.000000000000000000, 0.9659258262890683122, 1.000000000000000000, 0.9659258262890683122, 1.000000000000000000, 0.9659258262890683122, 1.000000000000000000, 0.9659258262890683122, 1.000000000000000000, 0.9659258262890683122, 1.000000000000000000, 0.9659258262890683122, 1.000000000000000000, 0.9659258262890683122, 1.000000000000000000, 0.9659258262890683122, 1.000000000000000000, 0.9659258262890683122, 1.000000000000000000, 0.9659258262890683122, 1.000000000000000000, 0.9659258262890683122, 1.000000000000000000, 0.9659258262890683122, 1.000000000000000000, 0.9659258262890683122, 1.000000000000000000, 0.9659258262890683122, 1.000000000000000000, 0.9659258262890683122, 1.000000000000000000, 0.9659258262890683122, 1.000000000000000000, 0.9659258262890683122, 1.000000000000000000, 0.9659258262890683122, 1.000000000000000000, 0.9659258262890683122, 1.000000000000000000, 0.9659258262890683122, 1.000000000000000000, 0.9659258262890683122, 1.000000000000000000, 0.9659258262890683122, 1.000000000000000000, 0.9659258262890683122, 1.000000000000000000, 0.9659258262890683122, 1.000000000000000000, 0.9659258262890683122, 1.000000000000000000, 0.9659258262890683122, 1.000000000000000000, 0.9659258262890683122, 1.000000000000000000, 0.9659258262890683122, 1.000000000000000000, 0.9659258262890683122, 1.000000000000000000, 0.9659258262890683122, 1.000000000000000000, 0.9659258262890683122, 1.000000000000000000, 0.9659258262890683122, 1.000000000000000000, 0.9659258262890683122, 1.000000000000000000, 0.9659258262890683122, 1.000000000000000000, 0.9659258262890683122, 1.000000000000000000, 0.9659258262890683122, 1.000000000000000000, 0.9659258262890683122, 1.000000000000000000, 0.9659258262890683122, 1.000000000000000000, 0.9659258262890683122, 1.000000000000000000, 0.9659258262890683122, 1.000000000000000000, 0.9659258262890683122, 1.000000000000000000, 0.9659258262890683122, 1.000000000000000000, 0.9659258262890683122, 1.000000000000000000, 0.9659258262890683122, 1.000000000000000000, 0.9659258262890683122, 1.000000000000000000, 0.9659258262890683122, 1.000000000000000000, 0.9659258262890683122, 1.000000000000000000, 0.9659258262890683122, 1.000000000000000000, 0.9659258262890683122, 1.000000000000000000, 0.9659258262890683122, 1.000000000000000000, 0.9659258262890683122, 1.000000000000000000, 0.9659258262890683122, 1.000000000000000000, 0.9659258262890683122, 1.000000000000000000, 0.9659258262890683122, 1.000000000000000000, 0.9659258262890683122, 1.000000000000000000, 0.9659258262890683122, 1.000000000000000000, 0.9659258262890683122, 1.000000000000000000, 0.9659258262890683122, 1.000000000000000000, 0.9659258262890683122, 1.000000000000000000, 0.9659258262890683122, 1.000000000000000000, 0.9659258262890683122, 1.000000000000000000, 0.9659258262890683122, 1.000000000000000000, 0.9659258262890683122, 1.000000000000000000, 0.9659258262890683122, 1.000000000000000000, 0.9659258262890683122, 1.000000000000000000, 0.9659258262890683122, 1.000000000000000000, 0.9659258262890683122, 1.000000000000000000, 0.9659258262890683122, 1.000000000000000000, 0.9659258262890683122, 1.000000000000000000, 0.9659258262890683122, 1.000000000000000000, 0.9659258262890683122, 1.000000000000000000, 0.9659258262890683122, 1.000000000000000000, 0.9659258262890683122, 1.000000000000000000, 0.9659258262890683122, 1.000000000000000000, 0.9659258262890683122, 1.000000000000000000, 0.9659258262890683122, 1.000000000000000000, 0.9659258262890683122, 1.000000000000000000, 0.9659258262890683122, 1.000000000000000000, 0.9659258262890683122, 1.000000000000000000, 0.9659258262890683122, 1.000000000000000000, 0.9659258262890683122, 1.000000000000000000, 0.9659258262890683122, 1.000000000000000000, 0.9659258262890683122, 1.000000000000000000, 0.9659258262890683122, 1.000000000000000000, 0.9659258262890683122, 1.000000000000000000, 0.9659258262890683122, 1.000000000000000000, 0.9659258262890683122, 1.000000000000000000, 0.9659258262890683122, 1.000000000000000000, 0.9659258262890683122, 1.000000000000000000, 0.9659258262890683122, 1.000000000000000000, 0.9659258262890683122, 1.000000000000000000, 0.9659258262890683122, 1.000000000000000000, 0.9659258262890683122, 1.000000000000000000, 0.9659258262890683122, 1.000000000000000000, 0.9659258262890683122, 1.000000000000000000, 0.9659258262890683122, 1.000000000000000000, 0.9659258262890683122, 1.000000000000000000, 0.9659258262890683122, 1.000000000000000000, 0.9659258262890683122, 1.000000000000000000, 0.9659258262890683122, 1.000000000000000000, 0.9659258262890683122, 1.000000000000000000, 0.9659258262890683122, 1.000000000000000000, 0.9659258262890683122, 1.000000000000000000, 0.9659258262890683122, 1.000000000000000000, 0.9659258262890683122, 1.000000000000000000, 0.9659258262890683122, 1.000000000000000000, 0.9659258262890683122, 1.000000000000000000, 0.9659258262890683122, 1.000000000000000000, 0.9659258262890683122, 1.000000000000000000, 0.9659258262890683122, 1.000000000000000000, 0.9659258262890683122, 1.000000000000000000, 0.9659258262890683122, 1.000000000000000000),
 ( 1.000000000000000000, 0.9659258262890683122, 1.000000000000000000, 0.9659258262890683122, 1.000000000000000000, 0.9659258262890683122, 1.000000000000000000, 0.9659258262890683122, 1.000000000000000000, 0.9659258262890683122, 1.000000000000000000, 0.9659258262890683122, 1.000000000000000000, 0.9659258262890683122, 1.000000000000000000, 0.9659258262890683122, 1.000000000000000000, 0.9659258262890683122, 1.000000000000000000, 0.9659258262890683122, 1.000000000000000000, 0.9659258262890683122, 1.000000000000000000, 0.9659258262890683122, 1.000000000000000000, 0.9659258262890683122, 1.000000000000000000, 0.9659258262890683122, 1.000000000000000000, 0.9659258262890683122, 1.000000000000000000, 0.9659258262890683122, 1.000000000000000000, 0.9659258262890683122, 1.000000000000000000, 0.9659258262890683122, 1.000000000000000000, 0.9659258262890683122, 1.000000000000000000, 0.9659258262890683122, 1.000000000000000000, 0.9659258262890683122, 1.000000000000000000, 0.9659258262890683122, 1.000000000000000000, 0.9659258262890683122, 1.000000000000000000, 0.9659258262890683122, 1.000000000000000000, 0.9659258262890683122, 1.000000000000000000, 0.9659258262890683122, 1.000000000000000000, 0.9659258262890683122, 1.000000000000000000, 0.9659258262890683122, 1.000000000000000000, 0.9659258262890683122, 1.000000000000000000, 0.9659258262890683122, 1.000000000000000000, 0.9659258262890683122, 1.000000000000000000, 0.9659258262890683122, 1.000000000000000000, 0.9659258262890683122, 1.000000000000000000, 0.9659258262890683122, 1.000000000000000000, 0.9659258262890683122, 1.000000000000000000, 0.9659258262890683122, 1.000000000000000000, 0.9659258262890683122, 1.000000000000000000, 0.9659258262890683122, 1.000000000000000000, 0.9659258262890683122, 1.000000000000000000, 0.9659258262890683122, 1.000000000000000000, 0.9659258262890683122, 1.000000000000000000, 0.9659258262890683122, 1.000000000000000000, 0.9659258262890683122, 1.000000000000000000, 0.9659258262890683122, 1.000000000000000000, 0.9659258262890683122, 1.000000000000000000, 0.9659258262890683122, 1.000000000000000000, 0.9659258262890683122, 1.000000000000000000, 0.9659258262890683122, 1.000000000000000000, 0.9659258262890683122, 1.000000000000000000, 0.9659258262890683122, 1.000000000000000000, 0.9659258262890683122, 1.000000000000000000, 0.9659258262890683122, 1.000000000000000000, 0.9659258262890683122, 1.000000000000000000, 0.9659258262890683122, 1.000000000000000000, 0.9659258262890683122, 1.000000000000000000, 0.9659258262890683122, 1.000000000000000000, 0.9659258262890683122, 1.000000000000000000, 0.9659258262890683122, 1.000000000000000000, 0.9659258262890683122, 1.000000000000000000, 0.9659258262890683122, 1.000000000000000000, 0.9659258262890683122, 1.000000000000000000, 0.9659258262890683122, 1.000000000000000000, 0.9659258262890683122, 1.000000000000000000, 0.9659258262890683122, 1.000000000000000000, 0.9659258262890683122, 1.000000000000000000, 0.9659258262890683122, 1.000000000000000000, 0.9659258262890683122, 1.000000000000000000, 0.9659258262890683122, 1.000000000000000000, 0.9659258262890683122, 1.000000000000000000, 0.9659258262890683122, 1.000000000000000000, 0.9659258262890683122, 1.000000000000000000, 0.9659258262890683122, 1.000000000000000000, 0.9659258262890683122, 1.000000000000000000, 0.9659258262890683122, 1.000000000000000000, 0.9659258262890683122, 1.000000000000000000, 0.9659258262890683122, 1.000000000000000000, 0.9659258262890683122, 1.000000000000000000, 0.9659258262890683122, 1.000000000000000000, 0.9659258262890683122, 1.000000000000000000, 0.9659258262890683122, 1.000000000000000000, 0.9659258262890683122, 1.000000000000000000, 0.9659258262890683122, 1.000000000000000000, 0.9659258262890683122, 1.000000000000000000, 0.9659258262890683122, 1.000000000000000000, 0.9659258262890683122, 1.000000000000000000, 0.9659258262890683122, 1.000000000000000000, 0.9659258262890683122, 1.000000000000000000, 0.9659258262890683122, 1.000000000000000000, 0.9659258262890683122, 1.000000000000000000, 0.9659258262890683122, 1.000000000000000000, 0.9659258262890683122, 1.000000000000000000, 0.9659258262890683122, 1.000000000000000000, 0.9659258262890683122, 1.000000000000000000, 0.9659258262890683122, 1.000000000000000000, 0.9659258262890683122, 1.000000000000000000, 0.9659258262890683122, 1.000000000000000000, 0.9659258262890683122, 1.000000000000000000, 0.9659258262890683122, 1.000000000000000000, 0.9659258262890683122, 1.000000000000000000, 0.9659258262890683122, 1.000000000000000000, 0.9659258262890683122, 1.000000000000000000, 0.9659258262890683122, 1.000000000000000000, 0.9659258262890683122, 1.000000000000000000, 0.9659258262890683122, 1.000000000000000000, 0.9659258262890683122, 1.000000000000000000, 0.9659258262890683122, 1.000000000000000000, 0.9659258262890683122, 1.000000000000000000, 0.9659258262890683122, 1.000000000000000000, 0.9659258262890683122, 1.000000000000000000, 0.9659258262890683122, 1.000000000000000000, 0.9659258262890683122, 1.000000000000000000, 0.9659258262890683122, 1.000000000000000000, 0.9659258262890683122, 1.000000000000000000, 0.9659258262890683122, 1.000000000000000000, 0.9659258262890683122, 1.000000000000000000, 0.9659258262890683122, 1.000000000000000000, 0.9659258262890683122, 1.000000000000000000, 0.9659258262890683122, 1.000000000000000000, 0.9659258262890683122, 1.000000000000000000, 0.9659258262890683122, 1.000000000000000000, 0.9659258262890683122, 1.000000000000000000, 0.9659258262890683122, 1.000000000000000000, 0.9659258262890683122, 1.000000000000000000, 0.9659258262890683122, 1.000000000000000000, 0.9659258262890683122, 1.000000000000000000, 0.9659258262890683122, 1.000000000000000000, 0.9659258262890683122, 1.000000000000000000, 0.9659258262890683122, 1.000000000000000000, 0.9659258262890683122, 1.000000000000000000, 0.9659258262890683122, 1.000000000000000000, 0.9659258262890683122, 1.000000000000000000, 0.9659258262890683122, 1.000000000000000000, 0.9659258262890683122, 1.000000000000000000, 0.9659258262890683122, 1.000000000000000000, 0.9659258262890683122, 1.000000000000000000, 0.9659258262890683122, 1.000000000000000000, 0.9659258262890683122, 1.000000000000000000, 0.9659258262890683122, 1.000000000000000000, 0.9659258262890683122, 1.000000000000000000, 0.9659258262890683122, 1.000000000000000000, 0.9659258262890683122, 1.000000000000000000, 0.9659258262890683122, 1.000000000000000000, 0.9659258262890683122, 1.000000000000000000, 0.9659258262890683122, 1.000000000000000000, 0.9659258262890683122, 1.000000000000000000, 0.9659258262890683122, 1.000000000000000000, 0.9659258262890683122, 1.000000000000000000, 0.9659258262890683122, 1.000000000000000000, 0.9659258262890683122, 1.000000000000000000, 0.9659258262890683122, 1.000000000000000000, 0.9659258262890683122, 1.000000000000000000, 0.9659258262890683122, 1.000000000000000000, 0.9659258262890683122, 1.000000000000000000, 0.9659258262890683122, 1.000000000000000000, 0.9659258262890683122, 1.000000000000000000, 0.9659258262890683122, 1.000000000000000000, 0.9659258262890683122, 1.000000000000000000, 0.9659258262890683122, 1.000000000000000000, 0.9659258262890683122, 1.000000000000000000, 0.9659258262890683122, 1.000000000000000000, 0.9659258262890683122, 1.000000000000000000, 0.9659258262890683122, 1.000000000000000000) ) ) 
 REPRESENTATION_ITEM ( '' )  SURFACE ( )  );
#32402 = AXIS2_PLACEMENT_3D ( 'NONE', #68811, #54275, #62266 ) ;
#32403 = DIRECTION ( 'NONE',  ( -1.000000000000000000, 0.000000000000000000, 0.000000000000000000 ) ) ;
#32404 = ADVANCED_FACE ( 'NONE', ( #31370 ), #92375, .F. ) ;
#32405 = B_SPLINE_CURVE_WITH_KNOTS ( 'NONE', 3,
 ( #77305, #8819, #39333, #97881 ),
 .UNSPECIFIED., .F., .F.,
 ( 4, 4 ),
 ( 2.168404344971008868E-19, 0.002657014572711346306 ),
 .UNSPECIFIED. ) ;
#32406 = CARTESIAN_POINT ( 'NONE',  ( 21.09922568453594849, 31.20696800326375353, 6.408140936763242479 ) ) ;
#32407 = CARTESIAN_POINT ( 'NONE',  ( -13.07751017357388257, 4.569076162262063760E-16, 6.263284095430414311 ) ) ;
#32408 = CARTESIAN_POINT ( 'NONE',  ( -2.266590686148945544, 52.22041550158064638, 7.082119434687048631 ) ) ;
#32409 = CARTESIAN_POINT ( 'NONE',  ( 5.076628168052704559, 25.17559781766745175, -8.527530157486179263 ) ) ;
#32410 = EDGE_CURVE ( 'NONE', #40991, #56450, #40862, .T. ) ;
#32411 = CARTESIAN_POINT ( 'NONE',  ( 18.52753015748618282, 3.925597817667451306, -4.923371831947291888 ) ) ;
#32412 = CARTESIAN_POINT ( 'NONE',  ( 20.00000000000000711, 97.09902325089555575, 4.954892789985619217 ) ) ;
#32413 = CARTESIAN_POINT ( 'NONE',  ( 2.917880565312950480, 45.97041550158063927, -12.26659068614894821 ) ) ;
#32414 = CARTESIAN_POINT ( 'NONE',  ( 17.20831665107776587, 57.88393115100078745, 7.208316651077764980 ) ) ;
#32415 = CARTESIAN_POINT ( 'NONE',  ( -4.164238869374098151, 56.59541550158063927, -3.795296366450310543 ) ) ;
#32416 = CARTESIAN_POINT ( 'NONE',  ( 6.204703633549690345, 27.84541550158063217, 14.16423886937410082 ) ) ;
#32417 = CARTESIAN_POINT ( 'NONE',  ( -4.164238869374098151, 36.59541550158063217, -3.795296366450310543 ) ) ;
#32418 = PLANE ( 'NONE',  #21181 ) ;
#32419 = PRODUCT_DEFINITION ( 'UNKNOWN', '', #21597, #5500 ) ;
#32421 = CARTESIAN_POINT ( 'NONE',  ( 18.52753015748618282, 53.92559781766745175, -4.923371831947291888 ) ) ;
#32420 = CARTESIAN_POINT ( 'NONE',  ( 4.919406150738182326, -13.80316667506059858, 2.500000000000000000 ) ) ;
#32422 = ORIENTED_EDGE ( 'NONE', *, *, #49008, .F. ) ;
#32423 = CARTESIAN_POINT ( 'NONE',  ( 15.44008868035555793, 31.39701867748817676, -9.422509992056140149 ) ) ;
#32424 = DIRECTION ( 'NONE',  ( -1.000000000000000000, 0.000000000000000000, 0.000000000000000000 ) ) ;
#32425 = CARTESIAN_POINT ( 'NONE',  ( 19.99999999998935607, 97.09160088439429614, -4.954669604078111966 ) ) ;
#32426 = CARTESIAN_POINT ( 'NONE',  ( 0.1532563361054083140, 36.00893115100078745, 1.131784320476157264E-15 ) ) ;
#32427 = CARTESIAN_POINT ( 'NONE',  ( 19.50000000000000355, 98.59912998021083297, 5.000000000000000000 ) ) ;
#32428 = CARTESIAN_POINT ( 'NONE',  ( -3.795296366450300773, -2.154584498419360283, 14.16423886937410437 ) ) ;
#32429 = CARTESIAN_POINT ( 'NONE',  ( 12.63842701281683034, 37.46726448433411605, 9.846743663894596210 ) ) ;
#32430 = CARTESIAN_POINT ( 'NONE',  ( 5.076628168052704559, 65.17559781766745175, -8.527530157486179263 ) ) ;
#32431 = ORIENTED_EDGE ( 'NONE', *, *, #89671, .F. ) ;
#32432 = CARTESIAN_POINT ( 'NONE',  ( 10.00000000000000000, 10.55374883491396787, -14.16423886937410082 ) ) ;
#32433 = EDGE_CURVE ( 'NONE', #75573, #95619, #86851, .T. ) ;
#32434 = DIRECTION ( 'NONE',  ( 0.000000000000000000, 0.000000000000000000, -1.000000000000000000 ) ) ;
#32436 = DIRECTION ( 'NONE',  ( -0.000000000000000000, -1.000000000000000000, -0.000000000000000000 ) ) ;
#32435 = FILL_AREA_STYLE_COLOUR ( '', #54640 ) ;
#32438 = VECTOR ( 'NONE', #69548, 999.9999999999998863 ) ;
#32437 = CARTESIAN_POINT ( 'NONE',  ( 6.204703633549690345, 67.84541550158060375, 14.16423886937410082 ) ) ;
#32439 = CARTESIAN_POINT ( 'NONE',  ( 3.591859063236763294, 28.29030133659708568, -11.09922568453595026 ) ) ;
#32440 = CARTESIAN_POINT ( 'NONE',  ( 18.00000000000000355, 77.07179676972445748, 4.250000000000000000 ) ) ;
#32441 = CARTESIAN_POINT ( 'NONE',  ( 7.361572987183169658, -0.03273551566588185635, -9.846743663894592657 ) ) ;
#32442 = COLOUR_RGB ( '', 0.09019608, 0.27058824, 0.51372549) ;
#32443 = DIRECTION ( 'NONE',  ( 0.000000000000000000, 0.000000000000000000, 1.000000000000000000 ) ) ;
#32444 = CARTESIAN_POINT ( 'NONE',  ( 1.959929470562270071, 31.50257860105348939, 5.767676674365832312 ) ) ;
#32445 = CYLINDRICAL_SURFACE ( 'NONE', #5604, 0.09999999999999939493 ) ;
#32446 = CARTESIAN_POINT ( 'NONE',  ( 17.08211943468705130, 63.47041550158063927, 12.26659068614894998 ) ) ;
#32447 = CARTESIAN_POINT ( 'NONE',  ( 18.04007052943772038, 44.00257860105348584, -5.767676674365850076 ) ) ;
#32448 = CARTESIAN_POINT ( 'NONE',  ( -0.04068437667222732368, 42.21974360917722180, -6.396802510829763477 ) ) ;
#32449 = CARTESIAN_POINT ( 'NONE',  ( 12.91533473730993009, 26.60535201082150536, -10.88017736071109987 ) ) ;
#32450 = CARTESIAN_POINT ( 'NONE',  ( 20.88017736071110164, 35.35535201082150536, 2.915334737309930979 ) ) ;
#32451 = CARTESIAN_POINT ( 'NONE',  ( 16.40814093676323893, 5.790301336597087456, 11.09922568453595026 ) ) ;
#32452 = CARTESIAN_POINT ( 'NONE',  ( 18.52753015748618282, 53.92559781766745175, -4.923371831947291888 ) ) ;
#32453 = CARTESIAN_POINT ( 'NONE',  ( -43.49625190214930370, 106.3671137969544986, -5.071642103756534681 ) ) ;
#32454 = CARTESIAN_POINT ( 'NONE',  ( 1.816707512666855928, 55.10290668512021739, -6.500000000000003553 ) ) ;
#32455 = ORIENTED_EDGE ( 'NONE', *, *, #68114, .F. ) ;
#32456 = CARTESIAN_POINT ( 'NONE',  ( 19.42250999205614548, 25.98035201082150891, -5.440088680355545492 ) ) ;
#32457 = CARTESIAN_POINT ( 'NONE',  ( -2.816281873526471635, 33.91530133659708213, -3.434112377981056508 ) ) ;
#32458 = CARTESIAN_POINT ( 'NONE',  ( -0.000000000000000000, 73.92154906606739928, 5.594368090432983109 ) ) ;
#32459 = CARTESIAN_POINT ( 'NONE',  ( 19.84674366389459266, 58.71726448433411605, -2.638427012816827677 ) ) ;
#32460 = B_SPLINE_CURVE_WITH_KNOTS ( 'NONE', 3,
 ( #39839, #24360, #54823, #70345 ),
 .UNSPECIFIED., .F., .F.,
 ( 4, 4 ),
 ( 0.000000000000000000, 0.001036303429213370061 ),
 .UNSPECIFIED. ) ;
#32461 = CARTESIAN_POINT ( 'NONE',  ( 7.084665262690076126, 54.10535201082151247, 10.88017736071109987 ) ) ;
#32462 = CARTESIAN_POINT ( 'NONE',  ( 0.1532563361054083140, 16.00893115100078390, 1.131784320476157264E-15 ) ) ;
#32463 = CARTESIAN_POINT ( 'NONE',  ( -2.816281873526473856, 34.12363466993042493, 9.499525473075851096E-16 ) ) ;
#32465 = DIRECTION ( 'NONE',  ( -0.000000000000000000, -0.000000000000000000, -1.000000000000000000 ) ) ;
#32464 = CARTESIAN_POINT ( 'NONE',  ( 4.559911319644449179, 58.89701867748817676, 9.422509992056141925 ) ) ;
#32466 = CARTESIAN_POINT ( 'NONE',  ( 10.93781366033340063, 0.5000000000000004441, 10.26470809774072634 ) ) ;
#32467 = CARTESIAN_POINT ( 'NONE',  ( 22.81628187352648496, 61.83196800326376774, -3.434112377981050290 ) ) ;
#32468 = ORIENTED_EDGE ( 'NONE', *, *, #97807, .T. ) ;
#32469 = SURFACE_STYLE_USAGE ( .BOTH. , #77972 ) ;
#32470 = CARTESIAN_POINT ( 'NONE',  ( 2.153642693323435164, 16.13791097397318808, -6.500000000000007105 ) ) ;
#32471 = CARTESIAN_POINT ( 'NONE',  ( -0.8801773607111008646, 3.272018677488171434, 2.915334737309923430 ) ) ;
#32473 = CARTESIAN_POINT ( 'NONE',  ( 24.16423886937410614, 14.51208216824730179, -3.795296366450302550 ) ) ;
#32472 = CARTESIAN_POINT ( 'NONE',  ( 10.00000000000000178, 50.37363466993042493, 12.81628187352647608 ) ) ;
#32474 = CARTESIAN_POINT ( 'NONE',  ( 14.92337183194729633, 17.67559781766745175, 8.527530157486181039 ) ) ;
#32475 = CARTESIAN_POINT ( 'NONE',  ( 20.88017736071110164, 5.355352010821502695, 2.915334737309930979 ) ) ;
#32476 = CARTESIAN_POINT ( 'NONE',  ( 18.52753015748617571, 23.09226448433411960, 4.923371831947298993 ) ) ;
#32477 = CARTESIAN_POINT ( 'NONE',  ( -4.164238869374098151, 56.59541550158063927, -3.795296366450310543 ) ) ;
#32478 = ORIENTED_EDGE ( 'NONE', *, *, #9656, .F. ) ;
#32479 = CARTESIAN_POINT ( 'NONE',  ( -0.8801773607111008646, 3.272018677488171434, 2.915334737309923430 ) ) ;
#32480 = CARTESIAN_POINT ( 'NONE',  ( 17.96484262340118221, 26.18868534415483396, -7.964842623401177768 ) ) ;
#32481 = CARTESIAN_POINT ( 'NONE',  ( 19.80448550324509327, 46.82703681773345039, 6.500000000002693845 ) ) ;
#32482 = ORIENTED_EDGE ( 'NONE', *, *, #40571, .F. ) ;
#32483 = ORIENTED_EDGE ( 'NONE', *, *, #79645, .F. ) ;
#32484 = VECTOR ( 'NONE', #40417, 1000.000000000000000 ) ;
#32485 = CARTESIAN_POINT ( 'NONE',  ( 17.96484262340118221, 16.18868534415483396, -7.964842623401177768 ) ) ;
#32486 = CARTESIAN_POINT ( 'NONE',  ( 12.91533473730993009, 16.60535201082150891, -10.88017736071109987 ) ) ;
#32487 = CARTESIAN_POINT ( 'NONE',  ( 0.1532563361054083140, 56.00893115100078745, 1.131784320476157264E-15 ) ) ;
#32488 = PLANE ( 'NONE',  #69980 ) ;
#32490 = CARTESIAN_POINT ( 'NONE',  ( 2.917880565312948704, 17.63708216824730357, 12.26659068614894643 ) ) ;
#32489 = CARTESIAN_POINT ( 'NONE',  ( -0.1503990784575328643, 20.12777174578613071, 6.262539305110068177 ) ) ;
#32491 = CARTESIAN_POINT ( 'NONE',  ( 19.42250999205614548, 25.98035201082150891, -5.440088680355545492 ) ) ;
#32492 = CARTESIAN_POINT ( 'NONE',  ( 4.559911319644449179, 7.230352010821505360, -9.422509992056141925 ) ) ;
#32493 = CARTESIAN_POINT ( 'NONE',  ( 1.472469842513823179, 51.42559781766745886, 4.923371831947296329 ) ) ;
#32494 = CARTESIAN_POINT ( 'NONE',  ( 17.62281668512000010, 43.28593319516822646, 6.500000000000063061 ) ) ;
#32495 = CARTESIAN_POINT ( 'NONE',  ( 0.1532563361054083140, 36.00893115100078745, 1.131784320476157264E-15 ) ) ;
#32496 = CARTESIAN_POINT ( 'NONE',  ( 14.92337183194729988, 9.342264484334119601, -8.527530157486177487 ) ) ;
#32497 = CARTESIAN_POINT ( 'NONE',  ( 8.527530157486179263, 28.09226448433413381, 4.923371831947292776 ) ) ;
#32498 = ORIENTED_EDGE ( 'NONE', *, *, #46856, .F. ) ;
#32499 = LINE ( 'NONE', #93994, #62125 ) ;
#32500 = CARTESIAN_POINT ( 'NONE',  ( 7.084665262690076126, 69.10535201082151957, 10.88017736071109987 ) ) ;
#32501 = CARTESIAN_POINT ( 'NONE',  ( -2.816281873526471635, 3.915301336597087456, -3.434112377981056508 ) ) ;
#32503 = CARTESIAN_POINT ( 'NONE',  ( 10.00000000000000000, 46.81368534415484106, -10.88017736071110342 ) ) ;
#32502 = CARTESIAN_POINT ( 'NONE',  ( 15.44008868035555260, 44.73035201082151247, 9.422509992056143702 ) ) ;
#32505 = CARTESIAN_POINT ( 'NONE',  ( -2.816281873526473856, 44.33196800326375353, 3.434112377981055619 ) ) ;
#32504 = CARTESIAN_POINT ( 'NONE',  ( 7.084665262690076126, 4.105352010821503583, 10.88017736071109987 ) ) ;
#32506 = CARTESIAN_POINT ( 'NONE',  ( 13.79529636645030344, 23.26208216824730002, 14.16423886937410614 ) ) ;
#32507 = EDGE_CURVE ( 'NONE', #59552, #52000, #27811, .T. ) ;
#32508 = ADVANCED_FACE ( 'NONE', ( #11826 ), #64806, .T. ) ;
#32509 = CARTESIAN_POINT ( 'NONE',  ( -1.099225684535947600, 48.70696800326375353, -6.408140936763238038 ) ) ;
#32510 = ORIENTED_EDGE ( 'NONE', *, *, #64347, .T. ) ;
#32511 = CARTESIAN_POINT ( 'NONE',  ( 1.472469842513823179, 56.42559781766745886, 4.923371831947296329 ) ) ;
#32512 = CARTESIAN_POINT ( 'NONE',  ( 19.42250999205614548, 15.98035201082150714, -5.440088680355545492 ) ) ;
#32513 = PRESENTATION_LAYER_ASSIGNMENT (  '', '', ( #70869 ) ) ;
#32514 = CARTESIAN_POINT ( 'NONE',  ( 4.559911319644449179, 33.89701867748817676, 9.422509992056141925 ) ) ;
#32515 = VERTEX_POINT ( 'NONE', #49328 ) ;
#32516 = CARTESIAN_POINT ( 'NONE',  ( 0.1532563361054083140, 11.00893115100078568, 1.131784320476157264E-15 ) ) ;
#32517 = CARTESIAN_POINT ( 'NONE',  ( -45.94000000000001194, 103.9981609152045507, 5.961202730336935041 ) ) ;
#32518 = CARTESIAN_POINT ( 'NONE',  ( 0.1532563361054083140, 11.00893115100078568, 1.131784320476157264E-15 ) ) ;
#32519 = CARTESIAN_POINT ( 'NONE',  ( 1.472469842513823179, 0.5922644843341181575, -4.923371831947296329 ) ) ;
#32520 = LINE ( 'NONE', #63018, #61841 ) ;
#32522 = CARTESIAN_POINT ( 'NONE',  ( -5.056330833731569108, 4.047076681631624764E-16, -13.58983143750706724 ) ) ;
#32521 = CARTESIAN_POINT ( 'NONE',  ( 19.42250999205614548, 55.98035201082150536, -5.440088680355545492 ) ) ;
#32523 = CARTESIAN_POINT ( 'NONE',  ( 10.00000000000000178, 69.31368534415484817, 10.88017736071110342 ) ) ;
#32525 = VERTEX_POINT ( 'NONE', #65802 ) ;
#32524 = CARTESIAN_POINT ( 'NONE',  ( 7.361572987183169658, 4.967264484334119601, -9.846743663894592657 ) ) ;
#32526 = DIRECTION ( 'NONE',  ( 1.000000000000000000, 0.000000000000000000, -1.224646799147353207E-16 ) ) ;
#32527 = EDGE_CURVE ( 'NONE', #94433, #88013, #79344, .T. ) ;
#32528 = CARTESIAN_POINT ( 'NONE',  ( 5.076628168052703671, 61.84226448433412315, 8.527530157486179263 ) ) ;
#32529 = ORIENTED_EDGE ( 'NONE', *, *, #40896, .T. ) ;
#32530 = ORIENTED_EDGE ( 'NONE', *, *, #45564, .F. ) ;
#32531 = CARTESIAN_POINT ( 'NONE',  ( 67.06412365047464164, 26.99999999999998224, 10.00000000000000000 ) ) ;
#32532 = CARTESIAN_POINT ( 'NONE',  ( 2.917880565312948704, 2.637082168247300906, 12.26659068614894643 ) ) ;
#32533 = CARTESIAN_POINT ( 'NONE',  ( -1.099225684535947600, 53.70696800326376064, -6.408140936763238038 ) ) ;
#32534 = CARTESIAN_POINT ( 'NONE',  ( 6.204703633549690345, 2.845415501580634388, 14.16423886937410082 ) ) ;
#32535 = CARTESIAN_POINT ( 'NONE',  ( 6.204703633549690345, 20.76208216824730357, -14.16423886937410259 ) ) ;
#32536 = DIRECTION ( 'NONE',  ( 0.4146932426562279228, 0.000000000000000000, 0.9099612708765483227 ) ) ;
#32537 = CARTESIAN_POINT ( 'NONE',  ( -14.47650479471824880, 0.5000000000000004441, 3.928206833721914482 ) ) ;
#32538 = CARTESIAN_POINT ( 'NONE',  ( 10.00000000000000178, 24.31368534415484106, 10.88017736071110342 ) ) ;
#32539 = ORIENTED_EDGE ( 'NONE', *, *, #80905, .T. ) ;
#32540 = CARTESIAN_POINT ( 'NONE',  ( 12.63842701281683922, 9.550597817667449974, -9.846743663894590881 ) ) ;
#32541 = CARTESIAN_POINT ( 'NONE',  ( 19.84674366389459621, 18.50893115100078745, 7.409399052514197653E-17 ) ) ;
#32542 = CARTESIAN_POINT ( 'NONE',  ( 6.565887622018943937, 30.16530133659708568, 12.81628187352647430 ) ) ;
#32543 = CARTESIAN_POINT ( 'NONE',  ( 1.472469842513823179, 35.59226448433412315, -4.923371831947296329 ) ) ;
#32544 = CARTESIAN_POINT ( 'NONE',  ( -0.000000000000000000, 91.25000000000000000, -7.750000000000000000 ) ) ;
#32545 = CARTESIAN_POINT ( 'NONE',  ( -2.816281873526473856, 14.12363466993041961, 9.499525473075851096E-16 ) ) ;
#32546 = FACE_OUTER_BOUND ( 'NONE', #49125, .T. ) ;
#32547 = CARTESIAN_POINT ( 'NONE',  ( 5.076628168052704559, 30.17559781766745175, -8.527530157486179263 ) ) ;
#32548 = CARTESIAN_POINT ( 'NONE',  ( 2.791683348922237240, 0.3839311510007847872, -7.208316651077763204 ) ) ;
#32549 = VERTEX_POINT ( 'NONE', #18357 ) ;
#32550 = ORIENTED_EDGE ( 'NONE', *, *, #2179, .F. ) ;
#32551 = CARTESIAN_POINT ( 'NONE',  ( 2.035157376598824452, 38.68868534415483396, 7.964842623401179544 ) ) ;
#32552 = CARTESIAN_POINT ( 'NONE',  ( -2.266590686148945544, 26.38708216824730357, -7.082119434687050408 ) ) ;
#32553 = CARTESIAN_POINT ( 'NONE',  ( 14.92337183194729988, 44.34226448433412315, -8.527530157486177487 ) ) ;
#32554 = CARTESIAN_POINT ( 'NONE',  ( 18.52753015748617571, 18.09226448433411960, 4.923371831947298993 ) ) ;
#32556 = DIRECTION ( 'NONE',  ( 0.000000000000000000, 0.000000000000000000, 1.000000000000000000 ) ) ;
#32555 = CARTESIAN_POINT ( 'NONE',  ( 22.81628187352648496, 56.83196800326374643, -3.434112377981050290 ) ) ;
#32557 = CARTESIAN_POINT ( 'NONE',  ( 4.559911319644449179, 33.89701867748817676, 9.422509992056141925 ) ) ;
#32558 = DIRECTION ( 'NONE',  ( 0.000000000000000000, 0.000000000000000000, 1.000000000000000000 ) ) ;
#32559 = EDGE_CURVE ( 'NONE', #11334, #77048, #56146, .T. ) ;
#32560 = CARTESIAN_POINT ( 'NONE',  ( 10.00000000000000178, 20.37363466993042138, 12.81628187352647608 ) ) ;
#32561 = CARTESIAN_POINT ( 'NONE',  ( 21.09922568453595559, 22.04030133659708923, -6.408140936763230044 ) ) ;
#32562 = CARTESIAN_POINT ( 'NONE',  ( 14.92337183194729633, 37.67559781766745175, 8.527530157486181039 ) ) ;
#32563 = CARTESIAN_POINT ( 'NONE',  ( -9.422509992056145478, 2.647018677488177651, -5.440088680355541939 ) ) ;
#32564 = CARTESIAN_POINT ( 'NONE',  ( 16.40814093676324603, 47.45696800326375353, -11.09922568453594671 ) ) ;
#32566 = DIRECTION ( 'NONE',  ( 0.000000000000000000, 0.000000000000000000, -1.000000000000000000 ) ) ;
#32565 = CARTESIAN_POINT ( 'NONE',  ( -0.8801773607110991993, 57.85535201082149825, -2.915334737309923874 ) ) ;
#32567 = EDGE_CURVE ( 'NONE', #27610, #96556, #17888, .T. ) ;
#32568 = CARTESIAN_POINT ( 'NONE',  ( 0.000000000000000000, 0.5000000000000004441, 0.000000000000000000 ) ) ;
#32569 = CARTESIAN_POINT ( 'NONE',  ( 0.000000000000000000, 69.99999999999998579, 4.000000000000000000 ) ) ;
#32570 = CARTESIAN_POINT ( 'NONE',  ( 10.00000000000000000, 51.81368534415484106, -10.88017736071110342 ) ) ;
#32571 = CARTESIAN_POINT ( 'NONE',  ( 0.5774900079438590739, 62.64701867748817676, -5.440088680355550821 ) ) ;
#32572 = DIRECTION ( 'NONE',  ( 0.8433914458128849434, 0.000000000000000000, 0.5372996083468249973 ) ) ;
#32573 = SURFACE_STYLE_FILL_AREA ( #48557 ) ;
#32574 = STYLED_ITEM ( 'NONE', ( #81170 ), #97716 ) ;
#32575 = CARTESIAN_POINT ( 'NONE',  ( 10.00000000000000178, 4.313685344154837509, 10.88017736071110342 ) ) ;
#32576 = CARTESIAN_POINT ( 'NONE',  ( 5.076628168052703671, 61.84226448433412315, 8.527530157486179263 ) ) ;
#32578 = CARTESIAN_POINT ( 'NONE',  ( 0.000000000000000000, -97.00000000000000000, -2.500000000000000000 ) ) ;
#32577 = CARTESIAN_POINT ( 'NONE',  ( 20.88017736071110164, 20.35535201082150891, 2.915334737309930979 ) ) ;
#32579 = B_SPLINE_CURVE_WITH_KNOTS ( 'NONE', 3,
 ( #14715, #43208, #22211, #45190, #22704, #73702 ),
 .UNSPECIFIED., .F., .F.,
 ( 4, 2, 4 ),
 ( 0.0002800484630363999391, 0.0006862541666483241206, 0.001092459870260248465 ),
 .UNSPECIFIED. ) ;
#32580 = CARTESIAN_POINT ( 'NONE',  ( -1.099225684535947600, 23.70696800326375708, -6.408140936763238038 ) ) ;
#32581 = ORIENTED_EDGE ( 'NONE', *, *, #89065, .F. ) ;
#32582 = CARTESIAN_POINT ( 'NONE',  ( 10.00000000000000000, 56.81368534415484106, -10.88017736071110342 ) ) ;
#32583 = CARTESIAN_POINT ( 'NONE',  ( 18.52753015748618282, 33.92559781766745886, -4.923371831947291888 ) ) ;
#32584 = STYLED_ITEM ( 'NONE', ( #22241 ), #94194 ) ;
#32586 = CARTESIAN_POINT ( 'NONE',  ( 19.88565890683629078, 47.71691075486302935, -6.480892540919839462 ) ) ;
#32585 = CARTESIAN_POINT ( 'NONE',  ( 10.00000000000000178, 10.37363466993041961, 12.81628187352647608 ) ) ;
#32587 = CARTESIAN_POINT ( 'NONE',  ( 0.5774900079438590739, 7.647018677488171434, -5.440088680355550821 ) ) ;
#32588 = CARTESIAN_POINT ( 'NONE',  ( 17.96484262340118221, 41.18868534415484106, -7.964842623401177768 ) ) ;
#32589 = CARTESIAN_POINT ( 'NONE',  ( 24.16423886937409904, 54.09541550158063217, 3.795296366450317205 ) ) ;
#32590 = CARTESIAN_POINT ( 'NONE',  ( 17.20831665107776587, 39.13393115100079456, -7.208316651077762316 ) ) ;
#32591 = CARTESIAN_POINT ( 'NONE',  ( 4.559911319644449179, 63.89701867748817676, 9.422509992056141925 ) ) ;
#32592 = SURFACE_STYLE_USAGE ( .BOTH. , #23145 ) ;
#32593 = CARTESIAN_POINT ( 'NONE',  ( 22.26659068614895176, 14.72041550158063572, -7.082119434687042414 ) ) ;
#32594 = DIRECTION ( 'NONE',  ( -0.000000000000000000, -0.000000000000000000, -1.000000000000000000 ) ) ;
#32595 = CARTESIAN_POINT ( 'NONE',  ( 1.274849032794306947, 7.555090184799359676, -6.499999999999997335 ) ) ;
#32596 = ORIENTED_EDGE ( 'NONE', *, *, #51630, .T. ) ;
#32597 = CARTESIAN_POINT ( 'NONE',  ( -4.164238869374099927, 37.01208216824731068, 3.795296366450308767 ) ) ;
#32598 = CARTESIAN_POINT ( 'NONE',  ( -2.266590686148945544, 37.22041550158063217, 7.082119434687048631 ) ) ;
#32599 = CARTESIAN_POINT ( 'NONE',  ( 7.361572987183170547, 7.050597817667451750, 9.846743663894590881 ) ) ;
#32600 = B_SPLINE_CURVE_WITH_KNOTS ( 'NONE', 3,
 ( #35866, #28370, #51365, #58857, #81852, #5872 ),
 .UNSPECIFIED., .F., .F.,
 ( 4, 2, 4 ),
 ( 0.0002800245631444383903, 0.0006862300328522850414, 0.001092435502560131855 ),
 .UNSPECIFIED. ) ;
#32601 = CARTESIAN_POINT ( 'NONE',  ( 22.81628187352647785, 11.62363466993042138, 6.195893100308588602E-16 ) ) ;
#32602 = CARTESIAN_POINT ( 'NONE',  ( 7.361572987183170547, 67.05059781766746596, 9.846743663894590881 ) ) ;
#32603 = LINE ( 'NONE', #63099, #22761 ) ;
#32605 = CARTESIAN_POINT ( 'NONE',  ( 22.81628187352648496, 31.83196800326375353, -3.434112377981050290 ) ) ;
#32604 = CARTESIAN_POINT ( 'NONE',  ( 19.42250999205614193, 65.14701867748817676, 5.440088680355555262 ) ) ;
#32606 = CARTESIAN_POINT ( 'NONE',  ( -0.3689425029237881626, 32.42874883491395366, 10.36894250292379027 ) ) ;
#32607 = CARTESIAN_POINT ( 'NONE',  ( 4.559911319644449179, 27.23035201082150536, -9.422509992056141925 ) ) ;
#32608 = CARTESIAN_POINT ( 'NONE',  ( 20.15039907845753930, 70.00000000000000000, -6.262539305110068177 ) ) ;
#32609 = CARTESIAN_POINT ( 'NONE',  ( 12.63842701281683034, 2.467264484334118269, 9.846743663894596210 ) ) ;
#32610 = CARTESIAN_POINT ( 'NONE',  ( 3.469446951953614189E-15, -7.741068848999208107, 9.846743663894594434 ) ) ;
#32611 = EDGE_LOOP ( 'NONE', ( #93359, #61012, #56981, #6879, #96001, #22156 ) ) ;
#32612 = DIRECTION ( 'NONE',  ( 0.3987490689252528031, 0.000000000000000000, -0.9170600743851211600 ) ) ;
#32613 =( BOUNDED_SURFACE ( )  B_SPLINE_SURFACE ( 1, 2, ( 
 ( #85990, #84511, #47482, #69020, #17502, #93972, #70495, #32479, #551, #47967, #1025, #78477, #24015, #9993, #31484, #61988, #40493, #92488, #77482, #2513, #63470, #30997, #61494, #92000, #96449, #79947, #49942, #58412, #41969, #10475, #19449, #64437, #73419, #65921, #95450, #86956, #27431, #41485, #18469, #48955, #27921, #56470, #79463, #57926, #26941, #94945, #17983, #19934, #80447, #2997, #11451, #11946, #42449, #57442, #48466, #88435, #78963, #72434, #10961, #72932, #87933, #4461, #34927, #71954, #50429, #3961, #34430, #65425, #40985, #71481, #87448, #95949, #64923, #3475, #4945, #80936, #12430, #33447, #63942, #18962, #42937, #26446, #56946, #33933, #35425, #94454, #49442, #25971, #58918, #89418, #45391, #20932, #51420, #81910, #75394, #96950, #66418, #51918, #13928, #6914, #28422, #44405, #82403, #21926, #74404, #13419, #90889, #82905, #22418, #7421, #37918, #21423, #37424, #68406, #29890, #43905, #67410, #5930, #43419, #35920, #36421, #67912, #73920, #74906, #97939, #29396, #60393, #66914, #28900, #97435, #14923, #59404, #89909, #6407, #36918, #98928, #59897, #90388, #52404, #52891, #5448, #14423, #44892, #98434, #83402, #20437, #75896, #30384, #88928, #50925, #81421, #12923, #62859, #23408, #31856, #84877, #68902, #69383, #78354, #40373, #8388, #906, #32353, #93355, #53892, #70378, #53382, #83893, #431, #39871, #31368, #9874, #85867, #38898, #61868, #54368, #39388, #9368, #85368, #92373, #16880, #47848, #77858, #70874, #69882, #23899, #77360, #1896, #84398, #16386, #46870, #8870, #24880, #1402, #46386, #55364, #17380, #15423, #62355, #92859, #24388, #54856, #47356, #2390, #60886, #30881, #15897, #91385, #22915, #45904, #76391, #7906, #38402, #61377, #91886, #76872, #95323, #11333, #12317, #4345, #32844, #87329, #94339, #64804, #3848, #41850, #49815, #71365, #34813, #94829, #56831, #26824, #93850, #42823, #3348, #72316, #26332, #18354, #19815, #18845, #11823, #27311, #25377, #80816, #57809, #65302, #33811, #78850, #49326, #50304, #79341, #86849, #95828, #88317, #33331, #79828, #64317, #73308, #63344, #2881, #42330, #17859, #25856, #63825, #56353, #55862, #34306, #57317, #87811, #71839, #86359, #19331, #48831, #80322, #48345, #10360, #40859, #72803, #10851, #41372, #66800, #14812, #6796, #65799, #74793, #81309, #51800, #89790, #36304, #97320, #73796, #59783, #21808, #43304, #59293, #96333, #52292, #52778, #36803, #90274, #27808, #67297, #12804, #28792, #81787, #21308, #5327, #58798, #37310, #35808, #66294, #44780, #82788, #13303, #82285, #96829, #83287, #13804, #97824, #45283, #44289, #58291, #6301, #51305, #60283 ),
 ( #28306, #89306, #29286, #14310, #75286, #20814, #67799, #98318, #29772, #43790, #74283, #90780, #22306, #4831, #35306, #88808, #20320, #50816, #5812, #16767, #7794, #54255, #38290, #30269, #22795, #68785, #92750, #60771, #8281, #84766, #16275, #47241, #30759, #15788, #91773, #1779, #317, #46276, #76279, #38778, #55239, #45788, #799, #76761, #77743, #91273, #23294, #69766, #15303, #46757, #7300, #1296, #24275, #70263, #61265, #53772, #32237, #9256, #84289, #77252, #31251, #83780, #69277, #93236, #85754, #61747, #92266, #39763, #62736, #23790, #85260, #68297, #98816, #8761, #54739, #39277, #24762, #17265, #31749, #62244, #75778, #37800, #53273, #72208, #86737, #3736, #34694, #64689, #27192, #56719, #25750, #64204, #95199, #10248, #56244, #79223, #71728, #26705, #26226, #33222, #49694, #72687, #40253, #18734, #3238, #18239, #79718, #33704, #41737, #94719, #57694, #70760, #48720, #87697, #94220, #10734, #40741, #4223, #49214, #41253, #2274, #17754, #48231, #65187, #78740, #71244, #11218, #25267, #87210, #34196, #57200, #19213, #2768, #80203, #11709, #86241, #42221, #9751, #95709, #88194, #47740, #78237, #32730, #63229, #55750, #93733, #63717, #82167, #6184, #36687, #82668, #29165, #90158, #14184, #44667, #75161, #67683, #29649, #60158, #42705, #63079, #71589, #53744, #22280, #32583, #76254, #86583, #79068, #9594, #98793, #40595, #53250, #30240, #60744, #10582, #68273, #91245, #71092, #40098, #7771, #41092, #33073, #93580, #14786, #23268, #25115, #55597, #70599, #29749, #2618, #60258, #85600, #22769, #86092, #2124, #17603, #48073, #83755, #63569, #91748, #17114, #78586, #90752, #52754, #289, #10098, #47597, #15279, #18092, #78091, #94077, #25598, #83262, #45256, #56091, #48568, #30735, #75753, #7275, #37776, #38265, #45760, #68758, #61242, #33555, #64053, #94565, #56577, #3101, #26083, #77955, #83987, #91976, #30972, #38495, #62948, #92460, #39483, #69480, #38987, #24976, #69973, #68990, #54459, #47940, #60976, #78446, #998, #9462, #84967, #61961, #9962, #1986, #91489, #8482, #31459, #23988, #16976, #77453, #84485, #32452, #55461, #23009, #1492, #16484, #46959, #31945, #8967, #92949, #62446, #40468, #53477, #24484, #39963, #46473, #54947, #23505, #85964, #85464, #47456, #15512, #61469, #53976, #28, #15986, #76969, #70464, #93451, #7997, #76483, #30475, #45994, #87910, #10451, #26421, #33908, #3938, #56447, #40959, #72908, #64896, #4441, #88414, #19914, #3451, #57417, #50405, #11923, #2970, #49418, #33420, #25474, #17954, #63919, #19424, #55956, #64416, #79919, #11428, #42427, #25945, #10938, #86933, #95929, #94430 ) ),
 .UNSPECIFIED., .F., .F., .T. ) 
 B_SPLINE_SURFACE_WITH_KNOTS ( ( 2, 2 ),
 ( 3, 2, 2, 2, 2, 2, 2, 2, 2, 2, 2, 2, 2, 2, 2, 2, 2, 2, 2, 2, 2, 2, 2, 2, 2, 2, 2, 2, 2, 2, 2, 2, 2, 2, 2, 2, 2, 2, 2, 2, 2, 2, 2, 2, 2, 2, 2, 2, 2, 2, 2, 2, 2, 2, 2, 2, 2, 2, 2, 2, 2, 2, 2, 2, 2, 2, 2, 2, 2, 2, 2, 2, 2, 2, 2, 2, 2, 2, 2, 2, 2, 2, 2, 2, 2, 2, 2, 2, 2, 2, 2, 2, 2, 2, 2, 2, 2, 2, 2, 2, 2, 2, 2, 2, 2, 2, 2, 2, 2, 2, 2, 2, 2, 2, 2, 2, 2, 2, 2, 2, 2, 2, 2, 2, 2, 2, 2, 2, 2, 2, 2, 2, 2, 2, 2, 2, 2, 2, 2, 2, 2, 2, 2, 2, 2, 2, 2, 2, 2, 2, 2, 2, 2, 2, 2, 2, 2, 2, 2, 2, 2, 2, 3 ),
 ( 0.000000000000000000, 1.000000000000000000 ),
 ( 0.000000000000000000, 0.005952380952380952051, 0.01190476190476190410, 0.01785714285714285615, 0.02380952380952380820, 0.02976190476190476025, 0.03571428571428571230, 0.04166666666666666435, 0.04761904761904761640, 0.05357142857142856845, 0.05952380952380952051, 0.06547619047619047949, 0.07142857142857142461, 0.07738095238095238360, 0.08333333333333332871, 0.08928571428571428770, 0.09523809523809523281, 0.1011904761904761918, 0.1071428571428571369, 0.1130952380952380959, 0.1190476190476190410, 0.1250000000000000000, 0.1309523809523809590, 0.1369047619047619180, 0.1428571428571428492, 0.1488095238095238082, 0.1547619047619047672, 0.1607142857142857262, 0.1666666666666666574, 0.1726190476190476164, 0.1785714285714285754, 0.1845238095238095344, 0.1904761904761904656, 0.1964285714285714246, 0.2023809523809523836, 0.2083333333333333426, 0.2142857142857142738, 0.2202380952380952328, 0.2261904761904761918, 0.2321428571428571508, 0.2380952380952380820, 0.2440476190476190410, 0.2500000000000000000, 0.2559523809523809312, 0.2619047619047619180, 0.2678571428571428492, 0.2738095238095238360, 0.2797619047619047672, 0.2857142857142856984, 0.2916666666666666852, 0.2976190476190476164, 0.3035714285714285476, 0.3095238095238095344, 0.3154761904761904656, 0.3214285714285714524, 0.3273809523809523836, 0.3333333333333333148, 0.3392857142857143016, 0.3452380952380952328, 0.3511904761904761640, 0.3571428571428571508, 0.3630952380952380820, 0.3690476190476190688, 0.3750000000000000000, 0.3809523809523809312, 0.3869047619047619180, 0.3928571428571428492, 0.3988095238095238360, 0.4047619047619047672, 0.4107142857142856984, 0.4166666666666666852, 0.4226190476190476164, 0.4285714285714285476, 0.4345238095238095344, 0.4404761904761904656, 0.4464285714285714524, 0.4523809523809523836, 0.4583333333333333148, 0.4642857142857143016, 0.4702380952380952328, 0.4761904761904761640, 0.4821428571428571508, 0.4880952380952380820, 0.4940476190476190688, 0.5000000000000000000, 0.5059523809523809312, 0.5119047619047618625, 0.5178571428571429047, 0.5238095238095238360, 0.5297619047619047672, 0.5357142857142856984, 0.5416666666666666297, 0.5476190476190476719, 0.5535714285714286031, 0.5595238095238095344, 0.5654761904761904656, 0.5714285714285713969, 0.5773809523809523281, 0.5833333333333333703, 0.5892857142857143016, 0.5952380952380952328, 0.6011904761904761640, 0.6071428571428570953, 0.6130952380952381375, 0.6190476190476190688, 0.6250000000000000000, 0.6309523809523809312, 0.6369047619047618625, 0.6428571428571429047, 0.6488095238095238360, 0.6547619047619047672, 0.6607142857142856984, 0.6666666666666666297, 0.6726190476190476719, 0.6785714285714286031, 0.6845238095238095344, 0.6904761904761904656, 0.6964285714285713969, 0.7023809523809523281, 0.7083333333333333703, 0.7142857142857143016, 0.7202380952380952328, 0.7261904761904761640, 0.7321428571428570953, 0.7380952380952381375, 0.7440476190476190688, 0.7500000000000000000, 0.7559523809523809312, 0.7619047619047618625, 0.7678571428571429047, 0.7738095238095238360, 0.7797619047619047672, 0.7857142857142856984, 0.7916666666666666297, 0.7976190476190476719, 0.8035714285714286031, 0.8095238095238095344, 0.8154761904761904656, 0.8214285714285713969, 0.8273809523809523281, 0.8333333333333333703, 0.8392857142857143016, 0.8452380952380952328, 0.8511904761904761640, 0.8571428571428570953, 0.8630952380952381375, 0.8690476190476190688, 0.8750000000000000000, 0.8809523809523809312, 0.8869047619047618625, 0.8928571428571429047, 0.8988095238095238360, 0.9047619047619047672, 0.9107142857142856984, 0.9166666666666666297, 0.9226190476190476719, 0.9285714285714286031, 0.9345238095238095344, 0.9404761904761904656, 0.9464285714285713969, 0.9523809523809523281, 0.9583333333333333703, 0.9642857142857143016 ),
 .UNSPECIFIED. ) 
 GEOMETRIC_REPRESENTATION_ITEM ( )  RATIONAL_B_SPLINE_SURFACE ( (
 ( 1.000000000000000000, 0.9659258262890683122, 1.000000000000000000, 0.9659258262890683122, 1.000000000000000000, 0.9659258262890683122, 1.000000000000000000, 0.9659258262890683122, 1.000000000000000000, 0.9659258262890683122, 1.000000000000000000, 0.9659258262890683122, 1.000000000000000000, 0.9659258262890683122, 1.000000000000000000, 0.9659258262890683122, 1.000000000000000000, 0.9659258262890683122, 1.000000000000000000, 0.9659258262890683122, 1.000000000000000000, 0.9659258262890683122, 1.000000000000000000, 0.9659258262890683122, 1.000000000000000000, 0.9659258262890683122, 1.000000000000000000, 0.9659258262890683122, 1.000000000000000000, 0.9659258262890683122, 1.000000000000000000, 0.9659258262890683122, 1.000000000000000000, 0.9659258262890683122, 1.000000000000000000, 0.9659258262890683122, 1.000000000000000000, 0.9659258262890683122, 1.000000000000000000, 0.9659258262890683122, 1.000000000000000000, 0.9659258262890683122, 1.000000000000000000, 0.9659258262890683122, 1.000000000000000000, 0.9659258262890683122, 1.000000000000000000, 0.9659258262890683122, 1.000000000000000000, 0.9659258262890683122, 1.000000000000000000, 0.9659258262890683122, 1.000000000000000000, 0.9659258262890683122, 1.000000000000000000, 0.9659258262890683122, 1.000000000000000000, 0.9659258262890683122, 1.000000000000000000, 0.9659258262890683122, 1.000000000000000000, 0.9659258262890683122, 1.000000000000000000, 0.9659258262890683122, 1.000000000000000000, 0.9659258262890683122, 1.000000000000000000, 0.9659258262890683122, 1.000000000000000000, 0.9659258262890683122, 1.000000000000000000, 0.9659258262890683122, 1.000000000000000000, 0.9659258262890683122, 1.000000000000000000, 0.9659258262890683122, 1.000000000000000000, 0.9659258262890683122, 1.000000000000000000, 0.9659258262890683122, 1.000000000000000000, 0.9659258262890683122, 1.000000000000000000, 0.9659258262890683122, 1.000000000000000000, 0.9659258262890683122, 1.000000000000000000, 0.9659258262890683122, 1.000000000000000000, 0.9659258262890683122, 1.000000000000000000, 0.9659258262890683122, 1.000000000000000000, 0.9659258262890683122, 1.000000000000000000, 0.9659258262890683122, 1.000000000000000000, 0.9659258262890683122, 1.000000000000000000, 0.9659258262890683122, 1.000000000000000000, 0.9659258262890683122, 1.000000000000000000, 0.9659258262890683122, 1.000000000000000000, 0.9659258262890683122, 1.000000000000000000, 0.9659258262890683122, 1.000000000000000000, 0.9659258262890683122, 1.000000000000000000, 0.9659258262890683122, 1.000000000000000000, 0.9659258262890683122, 1.000000000000000000, 0.9659258262890683122, 1.000000000000000000, 0.9659258262890683122, 1.000000000000000000, 0.9659258262890683122, 1.000000000000000000, 0.9659258262890683122, 1.000000000000000000, 0.9659258262890683122, 1.000000000000000000, 0.9659258262890683122, 1.000000000000000000, 0.9659258262890683122, 1.000000000000000000, 0.9659258262890683122, 1.000000000000000000, 0.9659258262890683122, 1.000000000000000000, 0.9659258262890683122, 1.000000000000000000, 0.9659258262890683122, 1.000000000000000000, 0.9659258262890683122, 1.000000000000000000, 0.9659258262890683122, 1.000000000000000000, 0.9659258262890683122, 1.000000000000000000, 0.9659258262890683122, 1.000000000000000000, 0.9659258262890683122, 1.000000000000000000, 0.9659258262890683122, 1.000000000000000000, 0.9659258262890683122, 1.000000000000000000, 0.9659258262890683122, 1.000000000000000000, 0.9659258262890683122, 1.000000000000000000, 0.9659258262890683122, 1.000000000000000000, 0.9659258262890683122, 1.000000000000000000, 0.9659258262890683122, 1.000000000000000000, 0.9659258262890683122, 1.000000000000000000, 0.9659258262890683122, 1.000000000000000000, 0.9659258262890683122, 1.000000000000000000, 0.9659258262890683122, 1.000000000000000000, 0.9659258262890683122, 1.000000000000000000, 0.9659258262890683122, 1.000000000000000000, 0.9659258262890683122, 1.000000000000000000, 0.9659258262890683122, 1.000000000000000000, 0.9659258262890683122, 1.000000000000000000, 0.9659258262890683122, 1.000000000000000000, 0.9659258262890683122, 1.000000000000000000, 0.9659258262890683122, 1.000000000000000000, 0.9659258262890683122, 1.000000000000000000, 0.9659258262890683122, 1.000000000000000000, 0.9659258262890683122, 1.000000000000000000, 0.9659258262890683122, 1.000000000000000000, 0.9659258262890683122, 1.000000000000000000, 0.9659258262890683122, 1.000000000000000000, 0.9659258262890683122, 1.000000000000000000, 0.9659258262890683122, 1.000000000000000000, 0.9659258262890683122, 1.000000000000000000, 0.9659258262890683122, 1.000000000000000000, 0.9659258262890683122, 1.000000000000000000, 0.9659258262890683122, 1.000000000000000000, 0.9659258262890683122, 1.000000000000000000, 0.9659258262890683122, 1.000000000000000000, 0.9659258262890683122, 1.000000000000000000, 0.9659258262890683122, 1.000000000000000000, 0.9659258262890683122, 1.000000000000000000, 0.9659258262890683122, 1.000000000000000000, 0.9659258262890683122, 1.000000000000000000, 0.9659258262890683122, 1.000000000000000000, 0.9659258262890683122, 1.000000000000000000, 0.9659258262890683122, 1.000000000000000000, 0.9659258262890683122, 1.000000000000000000, 0.9659258262890683122, 1.000000000000000000, 0.9659258262890683122, 1.000000000000000000, 0.9659258262890683122, 1.000000000000000000, 0.9659258262890683122, 1.000000000000000000, 0.9659258262890683122, 1.000000000000000000, 0.9659258262890683122, 1.000000000000000000, 0.9659258262890683122, 1.000000000000000000, 0.9659258262890683122, 1.000000000000000000, 0.9659258262890683122, 1.000000000000000000, 0.9659258262890683122, 1.000000000000000000, 0.9659258262890683122, 1.000000000000000000, 0.9659258262890683122, 1.000000000000000000, 0.9659258262890683122, 1.000000000000000000, 0.9659258262890683122, 1.000000000000000000, 0.9659258262890683122, 1.000000000000000000, 0.9659258262890683122, 1.000000000000000000, 0.9659258262890683122, 1.000000000000000000, 0.9659258262890683122, 1.000000000000000000, 0.9659258262890683122, 1.000000000000000000, 0.9659258262890683122, 1.000000000000000000, 0.9659258262890683122, 1.000000000000000000, 0.9659258262890683122, 1.000000000000000000, 0.9659258262890683122, 1.000000000000000000, 0.9659258262890683122, 1.000000000000000000, 0.9659258262890683122, 1.000000000000000000, 0.9659258262890683122, 1.000000000000000000, 0.9659258262890683122, 1.000000000000000000, 0.9659258262890683122, 1.000000000000000000, 0.9659258262890683122, 1.000000000000000000, 0.9659258262890683122, 1.000000000000000000, 0.9659258262890683122, 1.000000000000000000, 0.9659258262890683122, 1.000000000000000000, 0.9659258262890683122, 1.000000000000000000, 0.9659258262890683122, 1.000000000000000000, 0.9659258262890683122, 1.000000000000000000, 0.9659258262890683122, 1.000000000000000000, 0.9659258262890683122, 1.000000000000000000, 0.9659258262890683122, 1.000000000000000000, 0.9659258262890683122, 1.000000000000000000, 0.9659258262890683122, 1.000000000000000000, 0.9659258262890683122, 1.000000000000000000, 0.9659258262890683122, 1.000000000000000000, 0.9659258262890683122, 1.000000000000000000, 0.9659258262890683122, 1.000000000000000000, 0.9659258262890683122, 1.000000000000000000, 0.9659258262890683122, 1.000000000000000000, 0.9659258262890683122, 1.000000000000000000),
 ( 1.000000000000000000, 0.9659258262890683122, 1.000000000000000000, 0.9659258262890683122, 1.000000000000000000, 0.9659258262890683122, 1.000000000000000000, 0.9659258262890683122, 1.000000000000000000, 0.9659258262890683122, 1.000000000000000000, 0.9659258262890683122, 1.000000000000000000, 0.9659258262890683122, 1.000000000000000000, 0.9659258262890683122, 1.000000000000000000, 0.9659258262890683122, 1.000000000000000000, 0.9659258262890683122, 1.000000000000000000, 0.9659258262890683122, 1.000000000000000000, 0.9659258262890683122, 1.000000000000000000, 0.9659258262890683122, 1.000000000000000000, 0.9659258262890683122, 1.000000000000000000, 0.9659258262890683122, 1.000000000000000000, 0.9659258262890683122, 1.000000000000000000, 0.9659258262890683122, 1.000000000000000000, 0.9659258262890683122, 1.000000000000000000, 0.9659258262890683122, 1.000000000000000000, 0.9659258262890683122, 1.000000000000000000, 0.9659258262890683122, 1.000000000000000000, 0.9659258262890683122, 1.000000000000000000, 0.9659258262890683122, 1.000000000000000000, 0.9659258262890683122, 1.000000000000000000, 0.9659258262890683122, 1.000000000000000000, 0.9659258262890683122, 1.000000000000000000, 0.9659258262890683122, 1.000000000000000000, 0.9659258262890683122, 1.000000000000000000, 0.9659258262890683122, 1.000000000000000000, 0.9659258262890683122, 1.000000000000000000, 0.9659258262890683122, 1.000000000000000000, 0.9659258262890683122, 1.000000000000000000, 0.9659258262890683122, 1.000000000000000000, 0.9659258262890683122, 1.000000000000000000, 0.9659258262890683122, 1.000000000000000000, 0.9659258262890683122, 1.000000000000000000, 0.9659258262890683122, 1.000000000000000000, 0.9659258262890683122, 1.000000000000000000, 0.9659258262890683122, 1.000000000000000000, 0.9659258262890683122, 1.000000000000000000, 0.9659258262890683122, 1.000000000000000000, 0.9659258262890683122, 1.000000000000000000, 0.9659258262890683122, 1.000000000000000000, 0.9659258262890683122, 1.000000000000000000, 0.9659258262890683122, 1.000000000000000000, 0.9659258262890683122, 1.000000000000000000, 0.9659258262890683122, 1.000000000000000000, 0.9659258262890683122, 1.000000000000000000, 0.9659258262890683122, 1.000000000000000000, 0.9659258262890683122, 1.000000000000000000, 0.9659258262890683122, 1.000000000000000000, 0.9659258262890683122, 1.000000000000000000, 0.9659258262890683122, 1.000000000000000000, 0.9659258262890683122, 1.000000000000000000, 0.9659258262890683122, 1.000000000000000000, 0.9659258262890683122, 1.000000000000000000, 0.9659258262890683122, 1.000000000000000000, 0.9659258262890683122, 1.000000000000000000, 0.9659258262890683122, 1.000000000000000000, 0.9659258262890683122, 1.000000000000000000, 0.9659258262890683122, 1.000000000000000000, 0.9659258262890683122, 1.000000000000000000, 0.9659258262890683122, 1.000000000000000000, 0.9659258262890683122, 1.000000000000000000, 0.9659258262890683122, 1.000000000000000000, 0.9659258262890683122, 1.000000000000000000, 0.9659258262890683122, 1.000000000000000000, 0.9659258262890683122, 1.000000000000000000, 0.9659258262890683122, 1.000000000000000000, 0.9659258262890683122, 1.000000000000000000, 0.9659258262890683122, 1.000000000000000000, 0.9659258262890683122, 1.000000000000000000, 0.9659258262890683122, 1.000000000000000000, 0.9659258262890683122, 1.000000000000000000, 0.9659258262890683122, 1.000000000000000000, 0.9659258262890683122, 1.000000000000000000, 0.9659258262890683122, 1.000000000000000000, 0.9659258262890683122, 1.000000000000000000, 0.9659258262890683122, 1.000000000000000000, 0.9659258262890683122, 1.000000000000000000, 0.9659258262890683122, 1.000000000000000000, 0.9659258262890683122, 1.000000000000000000, 0.9659258262890683122, 1.000000000000000000, 0.9659258262890683122, 1.000000000000000000, 0.9659258262890683122, 1.000000000000000000, 0.9659258262890683122, 1.000000000000000000, 0.9659258262890683122, 1.000000000000000000, 0.9659258262890683122, 1.000000000000000000, 0.9659258262890683122, 1.000000000000000000, 0.9659258262890683122, 1.000000000000000000, 0.9659258262890683122, 1.000000000000000000, 0.9659258262890683122, 1.000000000000000000, 0.9659258262890683122, 1.000000000000000000, 0.9659258262890683122, 1.000000000000000000, 0.9659258262890683122, 1.000000000000000000, 0.9659258262890683122, 1.000000000000000000, 0.9659258262890683122, 1.000000000000000000, 0.9659258262890683122, 1.000000000000000000, 0.9659258262890683122, 1.000000000000000000, 0.9659258262890683122, 1.000000000000000000, 0.9659258262890683122, 1.000000000000000000, 0.9659258262890683122, 1.000000000000000000, 0.9659258262890683122, 1.000000000000000000, 0.9659258262890683122, 1.000000000000000000, 0.9659258262890683122, 1.000000000000000000, 0.9659258262890683122, 1.000000000000000000, 0.9659258262890683122, 1.000000000000000000, 0.9659258262890683122, 1.000000000000000000, 0.9659258262890683122, 1.000000000000000000, 0.9659258262890683122, 1.000000000000000000, 0.9659258262890683122, 1.000000000000000000, 0.9659258262890683122, 1.000000000000000000, 0.9659258262890683122, 1.000000000000000000, 0.9659258262890683122, 1.000000000000000000, 0.9659258262890683122, 1.000000000000000000, 0.9659258262890683122, 1.000000000000000000, 0.9659258262890683122, 1.000000000000000000, 0.9659258262890683122, 1.000000000000000000, 0.9659258262890683122, 1.000000000000000000, 0.9659258262890683122, 1.000000000000000000, 0.9659258262890683122, 1.000000000000000000, 0.9659258262890683122, 1.000000000000000000, 0.9659258262890683122, 1.000000000000000000, 0.9659258262890683122, 1.000000000000000000, 0.9659258262890683122, 1.000000000000000000, 0.9659258262890683122, 1.000000000000000000, 0.9659258262890683122, 1.000000000000000000, 0.9659258262890683122, 1.000000000000000000, 0.9659258262890683122, 1.000000000000000000, 0.9659258262890683122, 1.000000000000000000, 0.9659258262890683122, 1.000000000000000000, 0.9659258262890683122, 1.000000000000000000, 0.9659258262890683122, 1.000000000000000000, 0.9659258262890683122, 1.000000000000000000, 0.9659258262890683122, 1.000000000000000000, 0.9659258262890683122, 1.000000000000000000, 0.9659258262890683122, 1.000000000000000000, 0.9659258262890683122, 1.000000000000000000, 0.9659258262890683122, 1.000000000000000000, 0.9659258262890683122, 1.000000000000000000, 0.9659258262890683122, 1.000000000000000000, 0.9659258262890683122, 1.000000000000000000, 0.9659258262890683122, 1.000000000000000000, 0.9659258262890683122, 1.000000000000000000, 0.9659258262890683122, 1.000000000000000000, 0.9659258262890683122, 1.000000000000000000, 0.9659258262890683122, 1.000000000000000000, 0.9659258262890683122, 1.000000000000000000, 0.9659258262890683122, 1.000000000000000000, 0.9659258262890683122, 1.000000000000000000, 0.9659258262890683122, 1.000000000000000000, 0.9659258262890683122, 1.000000000000000000, 0.9659258262890683122, 1.000000000000000000, 0.9659258262890683122, 1.000000000000000000, 0.9659258262890683122, 1.000000000000000000, 0.9659258262890683122, 1.000000000000000000, 0.9659258262890683122, 1.000000000000000000, 0.9659258262890683122, 1.000000000000000000, 0.9659258262890683122, 1.000000000000000000, 0.9659258262890683122, 1.000000000000000000, 0.9659258262890683122, 1.000000000000000000, 0.9659258262890683122, 1.000000000000000000) ) ) 
 REPRESENTATION_ITEM ( '' )  SURFACE ( )  );
#32614 = CARTESIAN_POINT ( 'NONE',  ( 4.555630843329476320, 77.03495325336415078, -9.500000000000000000 ) ) ;
#32615 = VERTEX_POINT ( 'NONE', #86361 ) ;
#32617 = CARTESIAN_POINT ( 'NONE',  ( 4.559911319644449179, 8.897018677488173211, 9.422509992056141925 ) ) ;
#32616 = CARTESIAN_POINT ( 'NONE',  ( 17.96484262340118221, 4.938685344154837509, 7.964842623401181321 ) ) ;
#32619 = CARTESIAN_POINT ( 'NONE',  ( 0.6178305044545838731, 9.748634669930416052, 9.382169495545420901 ) ) ;
#32618 = CARTESIAN_POINT ( 'NONE',  ( 7.361572987183170547, 32.05059781766745175, 9.846743663894590881 ) ) ;
#32620 = DIRECTION ( 'NONE',  ( 1.000000000000000000, -0.000000000000000000, -0.000000000000000000 ) ) ;
#32621 = CYLINDRICAL_SURFACE ( 'NONE', #73414, 15.00000000000000000 ) ;
#32622 = EDGE_CURVE ( 'NONE', #17080, #60216, #819, .T. ) ;
#32623 = EDGE_CURVE ( 'NONE', #35666, #29544, #65305, .T. ) ;
#32624 = CARTESIAN_POINT ( 'NONE',  ( 21.09922568453594849, 6.206968003263753531, 6.408140936763242479 ) ) ;
#32625 = ORIENTED_EDGE ( 'NONE', *, *, #91027, .T. ) ;
#32626 = CARTESIAN_POINT ( 'NONE',  ( -2.266590686148945544, 42.22041550158063217, 7.082119434687048631 ) ) ;
#32627 = ORIENTED_EDGE ( 'NONE', *, *, #31485, .T. ) ;
#32628 = CARTESIAN_POINT ( 'NONE',  ( 13.79529636645031943, 60.34541550158063927, -14.16423886937409904 ) ) ;
#32629 = VERTEX_POINT ( 'NONE', #26335 ) ;
#32630 = CARTESIAN_POINT ( 'NONE',  ( 10.00000000000000178, 29.31368534415483751, 10.88017736071110342 ) ) ;
#32631 = CARTESIAN_POINT ( 'NONE',  ( 7.084665262690076126, 44.10535201082151247, 10.88017736071109987 ) ) ;
#32632 = B_SPLINE_CURVE_WITH_KNOTS ( 'NONE', 3,
 ( #71432, #2946, #9436, #85938, #78421, #17930 ),
 .UNSPECIFIED., .F., .F.,
 ( 4, 2, 4 ),
 ( 0.0002800015744458416345, 0.0006862068192651665267, 0.001092412064084491473 ),
 .UNSPECIFIED. ) ;
#32633 = CARTESIAN_POINT ( 'NONE',  ( 1.472469842513823179, 66.42559781766745175, 4.923371831947296329 ) ) ;
#32634 = CARTESIAN_POINT ( 'NONE',  ( 7.084665262690076126, 42.02201867748816966, -10.88017736071110164 ) ) ;
#32635 = CARTESIAN_POINT ( 'NONE',  ( 0.5774900079438607392, 63.48035201082149825, 5.440088680355550821 ) ) ;
#32636 = CARTESIAN_POINT ( 'NONE',  ( 20.88017736071110875, 25.77201867748816966, -2.915334737309920765 ) ) ;
#32637 = DIRECTION ( 'NONE',  ( -0.000000000000000000, 1.000000000000000000, 0.000000000000000000 ) ) ;
#32638 = ADVANCED_FACE ( 'NONE', ( #3850 ), #5177, .T. ) ;
#32639 = VECTOR ( 'NONE', #72858, 1000.000000000000000 ) ;
#32640 = CARTESIAN_POINT ( 'NONE',  ( 18.52753015748618282, 18.92559781766745175, -4.923371831947291888 ) ) ;
#32641 = DIRECTION ( 'NONE',  ( 0.000000000000000000, 1.000000000000000000, 0.000000000000000000 ) ) ;
#32642 = ORIENTED_EDGE ( 'NONE', *, *, #60181, .T. ) ;
#32643 = FACE_OUTER_BOUND ( 'NONE', #34584, .T. ) ;
#32644 = CARTESIAN_POINT ( 'NONE',  ( 7.361572987183169658, 44.96726448433412315, -9.846743663894592657 ) ) ;
#32645 = AXIS2_PLACEMENT_3D ( 'NONE', #87888, #43377, #20891 ) ;
#32646 = DIRECTION ( 'NONE',  ( 0.000000000000000000, 0.000000000000000000, -1.000000000000000000 ) ) ;
#32647 = CARTESIAN_POINT ( 'NONE',  ( -2.816281873526473856, 44.33196800326375353, 3.434112377981055619 ) ) ;
#32648 = ADVANCED_FACE ( 'NONE', ( #21955 ), #6649, .T. ) ;
#32649 = AXIS2_PLACEMENT_3D ( 'NONE', #79549, #58507, #11049 ) ;
#32650 = LINE ( 'NONE', #63144, #23562 ) ;
#32651 = CARTESIAN_POINT ( 'NONE',  ( 18.72515096720569616, 10.05509018479935968, 6.500000000000001776 ) ) ;
#32652 = DIRECTION ( 'NONE',  ( 1.000000000000000000, 0.000000000000000000, 0.000000000000000000 ) ) ;
#32653 = CARTESIAN_POINT ( 'NONE',  ( 5.076628168052703671, 51.84226448433412315, 8.527530157486179263 ) ) ;
#32654 = CARTESIAN_POINT ( 'NONE',  ( -4.164238869374099039, 46.80374883491397497, 8.674139862899312516E-16 ) ) ;
#32655 = CARTESIAN_POINT ( 'NONE',  ( 7.361572987183169658, 64.96726448433412315, -9.846743663894592657 ) ) ;
#32656 = EDGE_LOOP ( 'NONE', ( #23084, #62526, #57974, #9335, #79236, #41869 ) ) ;
#32657 = LINE ( 'NONE', #56163, #55990 ) ;
#32658 = CARTESIAN_POINT ( 'NONE',  ( 19.84674366389459266, 18.71726448433411960, -2.638427012816827677 ) ) ;
#32659 = CARTESIAN_POINT ( 'NONE',  ( 22.81628187352647785, 56.41530133659708213, 3.434112377981063169 ) ) ;
#32660 = CARTESIAN_POINT ( 'NONE',  ( 10.00000000000000178, 67.25893115100079456, 9.846743663894594434 ) ) ;
#32661 = CARTESIAN_POINT ( 'NONE',  ( 0.1532563361054082862, 1.217264484334117824, 2.638427012816831674 ) ) ;
#32662 = CARTESIAN_POINT ( 'NONE',  ( 19.05866839779139355, 30.95508385108959004, -6.499999999999974243 ) ) ;
#32663 = VECTOR ( 'NONE', #54814, 1000.000000000000000 ) ;
#32664 = VERTEX_POINT ( 'NONE', #52328 ) ;
#32665 = CARTESIAN_POINT ( 'NONE',  ( 10.00000000000000000, 60.55374883491397497, -14.16423886937410082 ) ) ;
#32666 = CARTESIAN_POINT ( 'NONE',  ( 19.42250999205614548, 40.98035201082150536, -5.440088680355545492 ) ) ;
#32668 = CARTESIAN_POINT ( 'NONE',  ( 20.88017736071110519, 60.56368534415484106, 2.639326808657452039E-16 ) ) ;
#32667 = CARTESIAN_POINT ( 'NONE',  ( -2.816281873526471635, 8.915301336597083903, -3.434112377981056508 ) ) ;
#32669 = CARTESIAN_POINT ( 'NONE',  ( -1.926860441876562247, 62.45379003517448524, -3.195792623639530650 ) ) ;
#32670 = DIRECTION ( 'NONE',  ( -0.1736481776669272503, 0.9848077530122086864, 0.000000000000000000 ) ) ;
#32671 = CARTESIAN_POINT ( 'NONE',  ( 0.2751277870542980231, 10.30223176428831522, 6.500000000000002665 ) ) ;
#32672 = CARTESIAN_POINT ( 'NONE',  ( 12.63842701281683922, 49.55059781766744464, -9.846743663894590881 ) ) ;
#32673 = CARTESIAN_POINT ( 'NONE',  ( 12.63842701281683922, 4.550597817667451750, -9.846743663894590881 ) ) ;
#32674 = CARTESIAN_POINT ( 'NONE',  ( -12.26659068614894110, 32.22041550158063927, 7.082119434687058401 ) ) ;
#32675 = CARTESIAN_POINT ( 'NONE',  ( -2.816281873526473856, 9.331968003263753531, 3.434112377981055619 ) ) ;
#32677 = CARTESIAN_POINT ( 'NONE',  ( 2.603489959281613420, 65.43575266056828355, -6.500000000000031086 ) ) ;
#32676 = CARTESIAN_POINT ( 'NONE',  ( 15.44008868035555793, 11.39701867748817143, -9.422509992056140149 ) ) ;
#32678 = SURFACE_SIDE_STYLE ('',( #62682 ) ) ;
#32679 = CARTESIAN_POINT ( 'NONE',  ( 24.16423886937410614, 29.51208216824729647, -3.795296366450302550 ) ) ;
#32680 = EDGE_CURVE ( 'NONE', #49491, #6552, #80106, .T. ) ;
#32681 = CARTESIAN_POINT ( 'NONE',  ( 2.917880565312948704, 27.63708216824730357, 12.26659068614894643 ) ) ;
#32682 = CARTESIAN_POINT ( 'NONE',  ( 17.08211943468705840, 65.13708216824730357, -12.26659068614894466 ) ) ;
#32683 = CARTESIAN_POINT ( 'NONE',  ( 10.00000000000000178, 22.25893115100078745, 9.846743663894594434 ) ) ;
#32684 = CARTESIAN_POINT ( 'NONE',  ( 0.5774900079438590739, 12.64701867748817143, -5.440088680355550821 ) ) ;
#32685 = EDGE_LOOP ( 'NONE', ( #8904, #95196, #20071, #17507 ) ) ;
#32686 = CARTESIAN_POINT ( 'NONE',  ( 2.791683348922237240, 35.38393115100079456, -7.208316651077763204 ) ) ;
#32687 = CARTESIAN_POINT ( 'NONE',  ( 15.44008868035555260, 39.73035201082150536, 9.422509992056143702 ) ) ;
#32688 = CARTESIAN_POINT ( 'NONE',  ( 14.92337183194729633, 62.67559781766745886, 8.527530157486181039 ) ) ;
#32690 = DIRECTION ( 'NONE',  ( 0.000000000000000000, 0.000000000000000000, 1.000000000000000000 ) ) ;
#32689 = CARTESIAN_POINT ( 'NONE',  ( -4.164238869374099039, 21.80374883491396787, 8.674139862899312516E-16 ) ) ;
#32691 = DIRECTION ( 'NONE',  ( 0.000000000000000000, 1.000000000000000000, 0.000000000000000000 ) ) ;
#32692 = CARTESIAN_POINT ( 'NONE',  ( 1.472469842513823179, 26.42559781766745175, 4.923371831947296329 ) ) ;
#32693 = CARTESIAN_POINT ( 'NONE',  ( 19.38216949554541557, 52.24863466993041072, -9.382169495545420901 ) ) ;
#32694 = CARTESIAN_POINT ( 'NONE',  ( 18.52753015748618282, 53.92559781766745175, -4.923371831947291888 ) ) ;
#32695 = ORIENTED_EDGE ( 'NONE', *, *, #54565, .F. ) ;
#32696 = CARTESIAN_POINT ( 'NONE',  ( 0.000000000000000000, -0.03417435944610275333, 14.25000000000000000 ) ) ;
#32697 = CARTESIAN_POINT ( 'NONE',  ( 0.2751277870542967463, 70.00000000000000000, -6.000000000000000000 ) ) ;
#32698 = CARTESIAN_POINT ( 'NONE',  ( 0.5774900079438590739, 7.647018677488171434, -5.440088680355550821 ) ) ;
#32699 = CARTESIAN_POINT ( 'NONE',  ( 0.5774900079438590739, 57.64701867748817676, -5.440088680355550821 ) ) ;
#32700 = CARTESIAN_POINT ( 'NONE',  ( -2.266590686148945544, 6.387082168247300906, -7.082119434687050408 ) ) ;
#32701 = CARTESIAN_POINT ( 'NONE',  ( 10.00000000000000000, -0.2410688489992152128, -9.846743663894594434 ) ) ;
#32702 = CARTESIAN_POINT ( 'NONE',  ( 0.1532563361054083140, 56.00893115100078745, 1.131784320476157264E-15 ) ) ;
#32703 = CARTESIAN_POINT ( 'NONE',  ( 12.91533473730993009, 21.60535201082150536, -10.88017736071109987 ) ) ;
#32704 = SURFACE_SIDE_STYLE ('',( #77717 ) ) ;
#32705 = CARTESIAN_POINT ( 'NONE',  ( 18.52753015748618282, 63.92559781766745886, -4.923371831947291888 ) ) ;
#32706 =( GEOMETRIC_REPRESENTATION_CONTEXT ( 3 ) GLOBAL_UNCERTAINTY_ASSIGNED_CONTEXT ( ( #5162 ) ) GLOBAL_UNIT_ASSIGNED_CONTEXT ( ( #13393, #91360, #45874 ) ) REPRESENTATION_CONTEXT ( 'NONE', 'WORKASPACE' ) );
#32707 = CARTESIAN_POINT ( 'NONE',  ( 7.361572987183169658, -0.03273551566588185635, -9.846743663894592657 ) ) ;
#32708 = CARTESIAN_POINT ( 'NONE',  ( 0.6178305044545818747, 58.49863466993042493, -9.382169495545419124 ) ) ;
#32709 = EDGE_LOOP ( 'NONE', ( #19939, #97091 ) ) ;
#32710 = ORIENTED_EDGE ( 'NONE', *, *, #35578, .F. ) ;
#32711 = CARTESIAN_POINT ( 'NONE',  ( -0.1503990784575328643, 70.00000000000000000, 6.262539305110068177 ) ) ;
#32712 = CARTESIAN_POINT ( 'NONE',  ( 13.79529636645031943, 40.34541550158063217, -14.16423886937409904 ) ) ;
#32713 = CARTESIAN_POINT ( 'NONE',  ( 0.1532563361054100626, 60.80059781766744464, -2.638427012816831230 ) ) ;
#32714 = CARTESIAN_POINT ( 'NONE',  ( 10.00000000000000000, 24.75893115100078745, -9.846743663894594434 ) ) ;
#32715 = CARTESIAN_POINT ( 'NONE',  ( 2.603489959281614308, 36.58210964143329136, 6.500000000000031086 ) ) ;
#32717 = CARTESIAN_POINT ( 'NONE',  ( 17.20831665107776587, 57.88393115100078745, 7.208316651077764980 ) ) ;
#32716 = CARTESIAN_POINT ( 'NONE',  ( 20.88017736071110519, 25.56368534415483751, 2.639326808657452039E-16 ) ) ;
#32718 = CARTESIAN_POINT ( 'NONE',  ( 0.000000000000000000, 0.5000000000000004441, 0.000000000000000000 ) ) ;
#32719 = STYLED_ITEM ( 'NONE', ( #12358 ), #85111 ) ;
#32720 = CARTESIAN_POINT ( 'NONE',  ( -2.266590686148945544, 52.22041550158064638, 7.082119434687048631 ) ) ;
#32721 = DIRECTION ( 'NONE',  ( 0.000000000000000000, 0.000000000000000000, -1.000000000000000000 ) ) ;
#32722 = ADVANCED_FACE ( 'NONE', ( #37347 ), #51342, .T. ) ;
#32723 = CARTESIAN_POINT ( 'NONE',  ( -11.35178980618984568, 14.63606909211651264, 9.804941009311860967 ) ) ;
#32724 = CARTESIAN_POINT ( 'NONE',  ( 20.88017736071110875, 60.77201867748817676, -2.915334737309920765 ) ) ;
#32725 = CARTESIAN_POINT ( 'NONE',  ( 0.1532563361054083140, 11.00893115100078568, 1.131784320476157264E-15 ) ) ;
#32726 = CARTESIAN_POINT ( 'NONE',  ( -6.060988839905887993, -36.09899559455953977, 4.000000000000000000 ) ) ;
#32727 = ORIENTED_EDGE ( 'NONE', *, *, #67690, .F. ) ;
#32728 = DIRECTION ( 'NONE',  ( 0.9914448613738084948, 0.000000000000000000, 0.1305261922200653124 ) ) ;
#32729 = VERTEX_POINT ( 'NONE', #91307 ) ;
#32730 = CARTESIAN_POINT ( 'NONE',  ( 14.92337183194729988, 29.34226448433411960, -8.527530157486177487 ) ) ;
#32731 = VERTEX_POINT ( 'NONE', #66834 ) ;
#32732 = CARTESIAN_POINT ( 'NONE',  ( -4.164238869374098151, 36.59541550158063217, -3.795296366450310543 ) ) ;
#32733 = CARTESIAN_POINT ( 'NONE',  ( 14.92337183194729633, 27.67559781766745530, 8.527530157486181039 ) ) ;
#32734 = CARTESIAN_POINT ( 'NONE',  ( 10.00000000000000178, 49.31368534415484106, 10.88017736071110342 ) ) ;
#32735 = CARTESIAN_POINT ( 'NONE',  ( 14.71525861348288799, 0.3640475087720990710, 2.908807992686685218 ) ) ;
#32736 = EDGE_CURVE ( 'NONE', #63206, #75691, #18687, .T. ) ;
#32737 = VERTEX_POINT ( 'NONE', #58834 ) ;
#32738 = CARTESIAN_POINT ( 'NONE',  ( 12.91533473730993009, 41.60535201082149825, -10.88017736071109987 ) ) ;
#32739 = FACE_OUTER_BOUND ( 'NONE', #21977, .T. ) ;
#32740 = MECHANICAL_DESIGN_GEOMETRIC_PRESENTATION_REPRESENTATION (  '', ( #71083 ), #40750 ) ;
#32741 = ADVANCED_FACE ( 'NONE', ( #54780 ), #61301, .T. ) ;
#32742 = EDGE_CURVE ( 'NONE', #61441, #50256, #93279, .T. ) ;
#32743 = CARTESIAN_POINT ( 'NONE',  ( 9.382169495545419124, -9.001365330069580395, 9.382169495545417348 ) ) ;
#32744 = ORIENTED_EDGE ( 'NONE', *, *, #82988, .T. ) ;
#32745 = CARTESIAN_POINT ( 'NONE',  ( 24.16423886937410614, 4.512082168247300906, -3.795296366450302550 ) ) ;
#32746 = ORIENTED_EDGE ( 'NONE', *, *, #9727, .F. ) ;
#32747 = CARTESIAN_POINT ( 'NONE',  ( 6.565887622018943937, 33.08196800326374643, -12.81628187352647608 ) ) ;
#32748 = CARTESIAN_POINT ( 'NONE',  ( 5.076628168052704559, 20.17559781766745175, -8.527530157486179263 ) ) ;
#32749 = DIRECTION ( 'NONE',  ( 1.000000000000000000, 0.000000000000000000, 0.000000000000000000 ) ) ;
#32750 = CARTESIAN_POINT ( 'NONE',  ( 5.076628168052704559, 25.17559781766745175, -8.527530157486179263 ) ) ;
#32751 = AXIS2_PLACEMENT_3D ( 'NONE', #4890, #5868, #87872 ) ;
#32752 = ORIENTED_EDGE ( 'NONE', *, *, #65812, .T. ) ;
#32753 = EDGE_CURVE ( 'NONE', #80833, #68278, #13021, .T. ) ;
#32754 = CARTESIAN_POINT ( 'NONE',  ( -6.189940676892205396, 14.95037117674007376, 13.39186120658999357 ) ) ;
#32755 = VECTOR ( 'NONE', #94677, 1000.000000000000000 ) ;
#32756 = CARTESIAN_POINT ( 'NONE',  ( 20.88017736071110164, 50.35535201082151247, 2.915334737309930979 ) ) ;
#32757 = DIRECTION ( 'NONE',  ( 0.000000000000000000, 1.000000000000000000, 0.000000000000000000 ) ) ;
#32758 = FILL_AREA_STYLE_COLOUR ( '', #90822 ) ;
#32759 = CARTESIAN_POINT ( 'NONE',  ( 1.472469842513823179, 10.59226448433411782, -4.923371831947296329 ) ) ;
#32760 = ADVANCED_FACE ( 'NONE', ( #16311 ), #84802, .T. ) ;
#32761 = FACE_OUTER_BOUND ( 'NONE', #74939, .T. ) ;
#32762 = TOROIDAL_SURFACE ( 'NONE', #69549, 14.49999999999999822, 0.5000000000000000000 ) ;
#32763 = CARTESIAN_POINT ( 'NONE',  ( 18.52753015748617571, 33.09226448433411605, 4.923371831947298993 ) ) ;
#32764 = LINE ( 'NONE', #41285, #18601 ) ;
#32765 = CARTESIAN_POINT ( 'NONE',  ( 10.00000000000000000, 10.55374883491396787, -14.16423886937410082 ) ) ;
#32766 = CARTESIAN_POINT ( 'NONE',  ( 17.20831665107776587, 22.88393115100078745, 7.208316651077764980 ) ) ;
#32767 = CARTESIAN_POINT ( 'NONE',  ( 19.38216949554541557, 32.24863466993041783, -9.382169495545420901 ) ) ;
#32768 = DIRECTION ( 'NONE',  ( 0.000000000000000000, 0.000000000000000000, -1.000000000000000000 ) ) ;
#32769 = CARTESIAN_POINT ( 'NONE',  ( -0.8801773607111008646, 53.27201867748816966, 2.915334737309923430 ) ) ;
#32770 = CARTESIAN_POINT ( 'NONE',  ( 13.43411237798106583, 7.665301336597086568, -12.81628187352647252 ) ) ;
#32771 = FACE_OUTER_BOUND ( 'NONE', #19499, .T. ) ;
#32772 = CARTESIAN_POINT ( 'NONE',  ( 19.84674366389459621, 28.50893115100078745, 7.409399052514197653E-17 ) ) ;
#32773 = CARTESIAN_POINT ( 'NONE',  ( 17.20831665107776587, 17.88393115100078745, 7.208316651077764980 ) ) ;
#32774 = CARTESIAN_POINT ( 'NONE',  ( 17.96484262340118221, 31.18868534415483751, -7.964842623401177768 ) ) ;
#32775 = CARTESIAN_POINT ( 'NONE',  ( 21.09922568453595559, 12.04030133659708746, -6.408140936763230044 ) ) ;
#32776 = CARTESIAN_POINT ( 'NONE',  ( 7.361572987183169658, 24.96726448433412315, -9.846743663894592657 ) ) ;
#32777 =( NAMED_UNIT ( * ) SI_UNIT ( $, .STERADIAN. ) SOLID_ANGLE_UNIT ( ) );
#32778 = CARTESIAN_POINT ( 'NONE',  ( -0.9082943533635161604, 4.683954948888111413E-16, -14.47152380945586359 ) ) ;
#32779 = CARTESIAN_POINT ( 'NONE',  ( 2.035157376598822676, 17.43868534415483751, -7.964842623401177768 ) ) ;
#32780 = STYLED_ITEM ( 'NONE', ( #22719 ), #85915 ) ;
#32781 = ORIENTED_EDGE ( 'NONE', *, *, #80448, .F. ) ;
#32782 = CARTESIAN_POINT ( 'NONE',  ( 20.88017736071110164, 65.35535201082150536, 2.915334737309930979 ) ) ;
#32783 = CYLINDRICAL_SURFACE ( 'NONE', #36131, 0.2500000000000002220 ) ;
#32785 = CARTESIAN_POINT ( 'NONE',  ( 0.5774900079438590739, 22.64701867748817321, -5.440088680355550821 ) ) ;
#32784 = CARTESIAN_POINT ( 'NONE',  ( 17.20831665107776587, 39.13393115100079456, -7.208316651077762316 ) ) ;
#32786 = FACE_OUTER_BOUND ( 'NONE', #11138, .T. ) ;
#32787 = CARTESIAN_POINT ( 'NONE',  ( 7.084665262690076126, 47.02201867748818387, -10.88017736071110164 ) ) ;
#32788 = CARTESIAN_POINT ( 'NONE',  ( 10.00000000000000000, 16.81368534415483751, -10.88017736071110342 ) ) ;
#32789 = CARTESIAN_POINT ( 'NONE',  ( 0.1532563361054083140, 16.00893115100078390, 1.131784320476157264E-15 ) ) ;
#32790 = CARTESIAN_POINT ( 'NONE',  ( 17.20831665107776587, 37.88393115100078745, 7.208316651077764980 ) ) ;
#32791 = CARTESIAN_POINT ( 'NONE',  ( -6.000000000000009770, 40.99999999999999289, 4.250000000000000000 ) ) ;
#32792 = CARTESIAN_POINT ( 'NONE',  ( -3.750000000000000000, 10.25000000000000000, -3.750000000000000000 ) ) ;
#32793 = SURFACE_STYLE_FILL_AREA ( #48293 ) ;
#32794 = CARTESIAN_POINT ( 'NONE',  ( 20.36894250292379738, 24.92874883491396787, -10.36894250292379027 ) ) ;
#32795 = CARTESIAN_POINT ( 'NONE',  ( 19.84674366389459266, 38.71726448433412315, -2.638427012816827677 ) ) ;
#32796 = CARTESIAN_POINT ( 'NONE',  ( 19.72487221294570858, 0.000000000000000000, -6.500000000000000888 ) ) ;
#32797 = ORIENTED_EDGE ( 'NONE', *, *, #50672, .T. ) ;
#32798 = VECTOR ( 'NONE', #9448, 1000.000000000000000 ) ;
#32799 = CARTESIAN_POINT ( 'NONE',  ( 22.26659068614895176, 64.72041550158064638, -7.082119434687042414 ) ) ;
#32800 = CARTESIAN_POINT ( 'NONE',  ( 7.361572987183169658, 24.96726448433412315, -9.846743663894592657 ) ) ;
#32802 = CARTESIAN_POINT ( 'NONE',  ( -8.000343251535921851, 84.06932101904432386, -3.750000000000000000 ) ) ;
#32801 = CARTESIAN_POINT ( 'NONE',  ( 0.000000000000000000, 0.000000000000000000, 0.000000000000000000 ) ) ;
#32803 = CARTESIAN_POINT ( 'NONE',  ( 2.035157376598824452, 48.68868534415483396, 7.964842623401179544 ) ) ;
#32804 = CARTESIAN_POINT ( 'NONE',  ( 5.419894505350532299, 14.49999999999999112, 13.98659156302467466 ) ) ;
#32805 = CARTESIAN_POINT ( 'NONE',  ( 12.91533473730993009, 11.60535201082150536, -10.88017736071109987 ) ) ;
#32806 = CARTESIAN_POINT ( 'NONE',  ( 6.565887622018943937, 50.16530133659708213, 12.81628187352647430 ) ) ;
#32807 = CARTESIAN_POINT ( 'NONE',  ( -1.099225684535947600, 9.540301336597087456, 6.408140936763237150 ) ) ;
#32808 = CARTESIAN_POINT ( 'NONE',  ( 10.00000000000000000, 14.75893115100078568, -9.846743663894594434 ) ) ;
#32809 = EDGE_LOOP ( 'NONE', ( #14441, #74905, #8513, #8533 ) ) ;
#32810 = PLANE ( 'NONE',  #7740 ) ;
#32811 = CARTESIAN_POINT ( 'NONE',  ( -4.164238869374099039, 56.80374883491397497, 8.674139862899312516E-16 ) ) ;
#32812 = CARTESIAN_POINT ( 'NONE',  ( -4.164238869374099927, 27.01208216824730357, 3.795296366450308767 ) ) ;
#32813 = CARTESIAN_POINT ( 'NONE',  ( 4.559911319644449179, 13.89701867748817143, 9.422509992056141925 ) ) ;
#32814 = CARTESIAN_POINT ( 'NONE',  ( 7.084665262690076126, 54.10535201082151247, 10.88017736071109987 ) ) ;
#32815 = DIRECTION ( 'NONE',  ( 0.000000000000000000, 0.000000000000000000, -1.000000000000000000 ) ) ;
#32816 = PLANE ( 'NONE',  #36884 ) ;
#32817 = CARTESIAN_POINT ( 'NONE',  ( 20.88017736071110519, 60.56368534415484106, 2.639326808657452039E-16 ) ) ;
#32818 = CARTESIAN_POINT ( 'NONE',  ( 1.472469842513823179, 21.42559781766745175, 4.923371831947296329 ) ) ;
#32819 = CARTESIAN_POINT ( 'NONE',  ( 2.603489959281614308, 51.58210964143330557, 6.500000000000031086 ) ) ;
#32820 = PRESENTATION_STYLE_ASSIGNMENT (( #92843 ) ) ;
#32821 = CARTESIAN_POINT ( 'NONE',  ( 2.791683348922240793, 21.63393115100078745, 7.208316651077764092 ) ) ;
#32822 = CARTESIAN_POINT ( 'NONE',  ( 7.361572987183169658, 44.96726448433412315, -9.846743663894592657 ) ) ;
#32823 = AXIS2_PLACEMENT_3D ( 'NONE', #80261, #28733, #89728 ) ;
#32824 = CARTESIAN_POINT ( 'NONE',  ( -0.8801773607110991993, 12.85535201082150358, -2.915334737309923874 ) ) ;
#32825 = CARTESIAN_POINT ( 'NONE',  ( 6.565887622018943937, 35.16530133659708923, 12.81628187352647430 ) ) ;
#32826 = VECTOR ( 'NONE', #54700, 1000.000000000000000 ) ;
#32827 = CARTESIAN_POINT ( 'NONE',  ( 19.42250999205614193, 55.14701867748817676, 5.440088680355555262 ) ) ;
#32828 = CARTESIAN_POINT ( 'NONE',  ( 2.791683348922240793, 26.63393115100078745, 7.208316651077764092 ) ) ;
#32830 = CARTESIAN_POINT ( 'NONE',  ( 19.84674366389459266, 23.30059781766745530, 2.638427012816836559 ) ) ;
#32829 = CARTESIAN_POINT ( 'NONE',  ( 22.26659068614895176, 49.72041550158063927, -7.082119434687042414 ) ) ;
#32831 = CARTESIAN_POINT ( 'NONE',  ( -8.000000000000000000, 80.07179676972448590, -6.250000000000000000 ) ) ;
#32832 = CARTESIAN_POINT ( 'NONE',  ( 0.1532563361054082862, 56.21726448433411605, 2.638427012816831674 ) ) ;
#32834 = CARTESIAN_POINT ( 'NONE',  ( 13.79529636645031943, 15.34541550158063750, -14.16423886937409904 ) ) ;
#32833 = CARTESIAN_POINT ( 'NONE',  ( 10.00000000000000000, 34.75893115100078745, -9.846743663894594434 ) ) ;
#32835 = CARTESIAN_POINT ( 'NONE',  ( -4.164238869374099927, 22.01208216824730357, 3.795296366450308767 ) ) ;
#32836 = CARTESIAN_POINT ( 'NONE',  ( 18.52753015748617571, 28.09226448433411960, 4.923371831947298993 ) ) ;
#32837 = CARTESIAN_POINT ( 'NONE',  ( 4.559911319644449179, 42.23035201082151247, -9.422509992056141925 ) ) ;
#32838 = CARTESIAN_POINT ( 'NONE',  ( 19.42250999205614193, 25.14701867748817321, 5.440088680355555262 ) ) ;
#32839 = CARTESIAN_POINT ( 'NONE',  ( 10.00000000000000000, 46.81368534415484106, -10.88017736071110342 ) ) ;
#32840 = CARTESIAN_POINT ( 'NONE',  ( 15.44008868035555793, 26.39701867748817321, -9.422509992056140149 ) ) ;
#32841 = VERTEX_POINT ( 'NONE', #91812 ) ;
#32842 = CARTESIAN_POINT ( 'NONE',  ( 21.09922568453595559, 37.04030133659708923, -6.408140936763230044 ) ) ;
#32843 = EDGE_CURVE ( 'NONE', #74689, #18880, #64106, .T. ) ;
#32844 = CARTESIAN_POINT ( 'NONE',  ( 0.5774900079438590739, 47.64701867748817676, -5.440088680355550821 ) ) ;
#32845 = ORIENTED_EDGE ( 'NONE', *, *, #7294, .F. ) ;
#32846 = CARTESIAN_POINT ( 'NONE',  ( 3.591859063236761518, 54.95696800326376064, 11.09922568453594849 ) ) ;
#32847 = CARTESIAN_POINT ( 'NONE',  ( -0.8801773607111009756, 63.06368534415484106, 1.068504757029289695E-15 ) ) ;
#32848 = ORIENTED_EDGE ( 'NONE', *, *, #58296, .F. ) ;
#32849 = VECTOR ( 'NONE', #4835, 1000.000000000000000 ) ;
#32851 = EDGE_CURVE ( 'NONE', #2953, #45712, #69808, .T. ) ;
#32850 = CARTESIAN_POINT ( 'NONE',  ( 2.035157376598824452, 68.68868534415484817, 7.964842623401179544 ) ) ;
#32852 = DIRECTION ( 'NONE',  ( -0.000000000000000000, 1.000000000000000000, -0.000000000000000000 ) ) ;
#32853 = VECTOR ( 'NONE', #45334, 1000.000000000000114 ) ;
#32854 = CARTESIAN_POINT ( 'NONE',  ( 14.56332774647473904, 0.04922511925146993983, -2.357028871694184513 ) ) ;
#32855 = DIRECTION ( 'NONE',  ( -0.000000000000000000, -1.000000000000000000, -0.000000000000000000 ) ) ;
#32856 = CARTESIAN_POINT ( 'NONE',  ( 22.26659068614894466, 58.88708216824729647, 7.082119434687054849 ) ) ;
#32857 = CARTESIAN_POINT ( 'NONE',  ( 1.472469842513823179, 5.592264484334118713, -4.923371831947296329 ) ) ;
#32858 = CARTESIAN_POINT ( 'NONE',  ( -0.3689425029237881626, 2.428748834913967869, 10.36894250292379027 ) ) ;
#32859 =( GEOMETRIC_REPRESENTATION_CONTEXT ( 3 ) GLOBAL_UNCERTAINTY_ASSIGNED_CONTEXT ( ( #90445 ) ) GLOBAL_UNIT_ASSIGNED_CONTEXT ( ( #16978, #68992, #53978 ) ) REPRESENTATION_CONTEXT ( 'NONE', 'WORKASPACE' ) );
#32860 = EDGE_CURVE ( 'NONE', #21688, #54112, #85445, .T. ) ;
#32861 = CARTESIAN_POINT ( 'NONE',  ( 17.20831665107776587, 7.883931151000784787, 7.208316651077764980 ) ) ;
#32862 = CARTESIAN_POINT ( 'NONE',  ( 15.44008868035555260, 9.730352010821505360, 9.422509992056143702 ) ) ;
#32863 = CARTESIAN_POINT ( 'NONE',  ( 7.361572987183170547, 42.05059781766745886, 9.846743663894590881 ) ) ;
#32864 = VERTEX_POINT ( 'NONE', #24315 ) ;
#32865 = CARTESIAN_POINT ( 'NONE',  ( 2.791683348922237240, 45.38393115100079456, -7.208316651077763204 ) ) ;
#32866 = CARTESIAN_POINT ( 'NONE',  ( 5.500000000000000000, 11.50000000000000000, 5.000000000000000000 ) ) ;
#32867 = CARTESIAN_POINT ( 'NONE',  ( 10.00000000000000178, 34.31368534415484106, 10.88017736071110342 ) ) ;
#32868 = CARTESIAN_POINT ( 'NONE',  ( 19.84674366389459266, 48.71726448433413026, -2.638427012816827677 ) ) ;
#32870 = FACE_OUTER_BOUND ( 'NONE', #60055, .T. ) ;
#32869 = CARTESIAN_POINT ( 'NONE',  ( -13.75503023589414830, 0.04922511925147124434, 5.333408231410639466 ) ) ;
#32871 = CARTESIAN_POINT ( 'NONE',  ( 17.96484262340118221, 54.93868534415484106, 7.964842623401181321 ) ) ;
#32872 = CARTESIAN_POINT ( 'NONE',  ( 20.88017736071110164, 10.35535201082150714, 2.915334737309930979 ) ) ;
#32873 = TOROIDAL_SURFACE ( 'NONE', #12107, 2.899999999999999467, 0.1000000000000000056 ) ;
#32874 = CARTESIAN_POINT ( 'NONE',  ( 3.591859063236761518, 44.95696800326376064, 11.09922568453594849 ) ) ;
#32875 = CARTESIAN_POINT ( 'NONE',  ( 9.879999999999990123, 20.99999999999999645, -2.899999999999999911 ) ) ;
#32876 = ORIENTED_EDGE ( 'NONE', *, *, #76553, .T. ) ;
#32877 = CARTESIAN_POINT ( 'NONE',  ( -2.816281873526473856, 34.33196800326376064, 3.434112377981055619 ) ) ;
#32878 = CARTESIAN_POINT ( 'NONE',  ( 19.42250999205614548, 35.98035201082151247, -5.440088680355545492 ) ) ;
#32880 = ORIENTED_EDGE ( 'NONE', *, *, #2629, .F. ) ;
#32879 = EDGE_CURVE ( 'NONE', #16289, #40665, #9790, .T. ) ;
#32881 = ORIENTED_EDGE ( 'NONE', *, *, #47002, .T. ) ;
#32882 = CARTESIAN_POINT ( 'NONE',  ( 19.84674366389459266, 3.717264484334118713, -2.638427012816827677 ) ) ;
#32883 = CARTESIAN_POINT ( 'NONE',  ( 7.361572987183169658, 44.96726448433412315, -9.846743663894592657 ) ) ;
#32885 = CARTESIAN_POINT ( 'NONE',  ( 18.52753015748617571, 43.09226448433412315, 4.923371831947298993 ) ) ;
#32884 = CARTESIAN_POINT ( 'NONE',  ( 2.791683348922237240, 15.38393115100078212, -7.208316651077763204 ) ) ;
#32886 = DIRECTION ( 'NONE',  ( 0.000000000000000000, 0.000000000000000000, 1.000000000000000000 ) ) ;
#32887 = CARTESIAN_POINT ( 'NONE',  ( -2.816281873526473856, 64.12363466993042493, 9.499525473075851096E-16 ) ) ;
#32888 = CARTESIAN_POINT ( 'NONE',  ( 10.00000000000000000, 24.75893115100078745, -9.846743663894594434 ) ) ;
#32889 = DIRECTION ( 'NONE',  ( 0.000000000000000000, 0.000000000000000000, 1.000000000000000000 ) ) ;
#32890 = AXIS2_PLACEMENT_3D ( 'NONE', #59621, #61588, #22136 ) ;
#32891 = PLANE ( 'NONE',  #43611 ) ;
#32893 = CARTESIAN_POINT ( 'NONE',  ( 0.7375392941517191492, 0.3640475087720981828, 14.98185688723472353 ) ) ;
#32892 = CARTESIAN_POINT ( 'NONE',  ( 18.52753015748617571, 33.09226448433411605, 4.923371831947298993 ) ) ;
#32894 = DIRECTION ( 'NONE',  ( 0.000000000000000000, 0.000000000000000000, 1.000000000000000000 ) ) ;
#32896 = VERTEX_POINT ( 'NONE', #24803 ) ;
#32895 = CARTESIAN_POINT ( 'NONE',  ( 19.84674366389459266, 43.30059781766744464, 2.638427012816836559 ) ) ;
#32897 = ADVANCED_FACE ( 'NONE', ( #77780 ), #9293, .T. ) ;
#32898 = CARTESIAN_POINT ( 'NONE',  ( 13.78891971893208357, 14.49999999999999822, -5.904717858191528279 ) ) ;
#32899 = CARTESIAN_POINT ( 'NONE',  ( 16.40814093676324603, 27.45696800326375708, -11.09922568453594671 ) ) ;
#32900 = CARTESIAN_POINT ( 'NONE',  ( 24.16423886937409904, 44.09541550158063927, 3.795296366450317205 ) ) ;
#32901 = CARTESIAN_POINT ( 'NONE',  ( 2.791683348922237240, 20.38393115100078745, -7.208316651077763204 ) ) ;
#32902 = VERTEX_POINT ( 'NONE', #22835 ) ;
#32903 = CARTESIAN_POINT ( 'NONE',  ( 5.076628168052703671, 1.842264484334118047, 8.527530157486179263 ) ) ;
#32904 = CARTESIAN_POINT ( 'NONE',  ( 19.99999999999861089, 92.23760269512273169, 5.246947360776563762 ) ) ;
#32905 = CARTESIAN_POINT ( 'NONE',  ( 10.00000000000000178, 48.05374883491396787, 14.16423886937410082 ) ) ;
#32906 = CARTESIAN_POINT ( 'NONE',  ( 18.52753015748618282, 58.92559781766745886, -4.923371831947291888 ) ) ;
#32907 = CARTESIAN_POINT ( 'NONE',  ( 7.084665262690076126, 12.02201867748817321, -10.88017736071110164 ) ) ;
#32908 = CARTESIAN_POINT ( 'NONE',  ( 10.00000000000000178, 23.05374883491397142, 14.16423886937410082 ) ) ;
#32909 = CARTESIAN_POINT ( 'NONE',  ( -0.3689425029237898834, 41.17874883491397497, -10.36894250292378850 ) ) ;
#32910 = DIRECTION ( 'NONE',  ( -0.5547001962252291474, -0.8320502943378437211, -0.000000000000000000 ) ) ;
#32912 = CARTESIAN_POINT ( 'NONE',  ( 1.472469842513823179, 51.42559781766745886, 4.923371831947296329 ) ) ;
#32911 = CARTESIAN_POINT ( 'NONE',  ( 6.905507196100984402, -69.44000359832136837, 2.499999999998390621 ) ) ;
#32913 = AXIS2_PLACEMENT_3D ( 'NONE', #16824, #70325, #24826 ) ;
#32914 = ORIENTED_EDGE ( 'NONE', *, *, #95950, .T. ) ;
#32915 = CARTESIAN_POINT ( 'NONE',  ( -0.8801773607111008646, 33.27201867748817676, 2.915334737309923430 ) ) ;
#32916 = CARTESIAN_POINT ( 'NONE',  ( 0.000000000000000000, 0.000000000000000000, 0.000000000000000000 ) ) ;
#32917 = CARTESIAN_POINT ( 'NONE',  ( 2.603489959281613420, 65.43575266056828355, -6.500000000000031086 ) ) ;
#32918 = CARTESIAN_POINT ( 'NONE',  ( 7.361572987183170547, 42.05059781766745886, 9.846743663894590881 ) ) ;
#32919 = CARTESIAN_POINT ( 'NONE',  ( 17.35999999999999943, 33.99999999999997158, -9.500000000000000000 ) ) ;
#32920 = CARTESIAN_POINT ( 'NONE',  ( 3.795296366450306547, 5.345415501580633943, -14.16423886937410259 ) ) ;
#32921 = CARTESIAN_POINT ( 'NONE',  ( 0.1532563361054083140, 61.00893115100078745, 1.131784320476157264E-15 ) ) ;
#32922 = LINE ( 'NONE', #48908, #92866 ) ;
#32923 = CIRCLE ( 'NONE', #10595, 0.2500000000000002220 ) ;
#32924 = COLOUR_RGB ( '', 0.08235294, 0.09019608, 0.10196078) ;
#32925 = ORIENTED_EDGE ( 'NONE', *, *, #95741, .F. ) ;
#32926 = CARTESIAN_POINT ( 'NONE',  ( 17.08211943468705130, 23.47041550158063572, 12.26659068614894998 ) ) ;
#32927 = AXIS2_PLACEMENT_3D ( 'NONE', #29677, #22209, #52686 ) ;
#32928 = CARTESIAN_POINT ( 'NONE',  ( -6.189940676891933613, 0.04962882325992939991, -13.39186120659011614 ) ) ;
#32929 = CARTESIAN_POINT ( 'NONE',  ( 0.5774900079438607392, 8.480352010821505360, 5.440088680355550821 ) ) ;
#32930 = CARTESIAN_POINT ( 'NONE',  ( 22.81628187352647785, 26.41530133659708923, 3.434112377981063169 ) ) ;
#32931 = DIRECTION ( 'NONE',  ( -0.000000000000000000, -1.000000000000000000, -0.000000000000000000 ) ) ;
#32932 = CARTESIAN_POINT ( 'NONE',  ( -0.8801773607111009756, 63.06368534415484106, 1.068504757029289695E-15 ) ) ;
#32933 = EDGE_CURVE ( 'NONE', #28166, #9012, #63264, .T. ) ;
#32934 = CARTESIAN_POINT ( 'NONE',  ( 10.00000000000000178, 14.31368534415483929, 10.88017736071110342 ) ) ;
#32935 = CARTESIAN_POINT ( 'NONE',  ( -14.99847009497944583, 15.00000000000000000, 0.2142307401079343032 ) ) ;
#32936 = CARTESIAN_POINT ( 'NONE',  ( 2.035157376598822676, 22.43868534415483396, -7.964842623401177768 ) ) ;
#32937 = CARTESIAN_POINT ( 'NONE',  ( -0.8801773607110991993, 37.85535201082151247, -2.915334737309923874 ) ) ;
#32938 = CARTESIAN_POINT ( 'NONE',  ( 0.1532563361054100626, 65.80059781766745175, -2.638427012816831230 ) ) ;
#32939 = CARTESIAN_POINT ( 'NONE',  ( -8.000000000000000000, 79.82179676972448590, -6.250000000000000000 ) ) ;
#32940 = CARTESIAN_POINT ( 'NONE',  ( 3.591859063236761518, 64.95696800326376774, 11.09922568453594849 ) ) ;
#32941 = CARTESIAN_POINT ( 'NONE',  ( 17.20831665107776587, 14.13393115100078568, -7.208316651077762316 ) ) ;
#32942 = ORIENTED_EDGE ( 'NONE', *, *, #21654, .T. ) ;
#32943 = EDGE_CURVE ( 'NONE', #73495, #18004, #37020, .T. ) ;
#32944 = CARTESIAN_POINT ( 'NONE',  ( 2.035157376598822676, 27.43868534415483396, -7.964842623401177768 ) ) ;
#32945 = CARTESIAN_POINT ( 'NONE',  ( 6.565887622018943937, 30.16530133659708568, 12.81628187352647430 ) ) ;
#32946 = PRESENTATION_LAYER_ASSIGNMENT (  '', '', ( #28587 ) ) ;
#32947 = DIRECTION ( 'NONE',  ( -0.000000000000000000, -0.000000000000000000, 1.000000000000000000 ) ) ;
#32948 = AXIS2_PLACEMENT_3D ( 'NONE', #59097, #89606, #6114 ) ;
#32949 = CARTESIAN_POINT ( 'NONE',  ( 2.791683348922240793, 56.63393115100078035, 7.208316651077764092 ) ) ;
#32950 = CARTESIAN_POINT ( 'NONE',  ( 10.00000000000000000, 46.81368534415484106, -10.88017736071110342 ) ) ;
#32951 = CARTESIAN_POINT ( 'NONE',  ( -2.816281873526471635, 33.91530133659708213, -3.434112377981056508 ) ) ;
#32953 = DIRECTION ( 'NONE',  ( -0.000000000000000000, -1.000000000000000000, -0.000000000000000000 ) ) ;
#32952 = CARTESIAN_POINT ( 'NONE',  ( 2.035157376598822676, 67.43868534415484817, -7.964842623401177768 ) ) ;
#32954 = CARTESIAN_POINT ( 'NONE',  ( 17.84635730667659104, 53.63791097397319874, 6.499999999999959144 ) ) ;
#32955 = ORIENTED_EDGE ( 'NONE', *, *, #49106, .F. ) ;
#32956 = DIRECTION ( 'NONE',  ( -0.1736481776669272503, 0.9848077530122086864, 0.000000000000000000 ) ) ;
#32957 = LINE ( 'NONE', #56937, #14287 ) ;
#32958 = CARTESIAN_POINT ( 'NONE',  ( 19.42250999205614193, 5.147018677488171434, 5.440088680355555262 ) ) ;
#32959 = CARTESIAN_POINT ( 'NONE',  ( 10.00000000000000000, 52.87363466993041783, -12.81628187352647608 ) ) ;
#32960 = CARTESIAN_POINT ( 'NONE',  ( 7.361572987183169658, 14.96726448433411960, -9.846743663894592657 ) ) ;
#32961 = CARTESIAN_POINT ( 'NONE',  ( 0.5774900079438590739, 7.647018677488171434, -5.440088680355550821 ) ) ;
#32962 = CARTESIAN_POINT ( 'NONE',  ( 0.1532563361054082862, 21.21726448433412315, 2.638427012816831674 ) ) ;
#32963 = CARTESIAN_POINT ( 'NONE',  ( 10.00000000000000000, 60.55374883491397497, -14.16423886937410082 ) ) ;
#32964 = ORIENTED_EDGE ( 'NONE', *, *, #12999, .T. ) ;
#32965 = AXIS2_PLACEMENT_3D ( 'NONE', #28651, #74646, #29137 ) ;
#32966 = FILL_AREA_STYLE ('',( #8510 ) ) ;
#32967 = CARTESIAN_POINT ( 'NONE',  ( 10.00000000000000178, 24.31368534415484106, 10.88017736071110342 ) ) ;
#32968 = DIRECTION ( 'NONE',  ( 1.000000000000000000, 0.000000000000000000, -0.000000000000000000 ) ) ;
#32969 = ORIENTED_EDGE ( 'NONE', *, *, #91547, .F. ) ;
#32970 = ORIENTED_EDGE ( 'NONE', *, *, #58486, .T. ) ;
#32972 = ADVANCED_FACE ( 'NONE', ( #68822 ), #354, .F. ) ;
#32971 = CARTESIAN_POINT ( 'NONE',  ( 15.44008868035555793, 6.397018677488171434, -9.422509992056140149 ) ) ;
#32973 = CARTESIAN_POINT ( 'NONE',  ( 18.52753015748617571, 53.09226448433412315, 4.923371831947298993 ) ) ;
#32974 = CARTESIAN_POINT ( 'NONE',  ( 19.38216949554541202, 50.99863466993042493, 9.382169495545424454 ) ) ;
#32975 = CARTESIAN_POINT ( 'NONE',  ( 10.58981376305288613, 15.00000000000000000, -9.535111140613709679 ) ) ;
#32977 = CARTESIAN_POINT ( 'NONE',  ( 10.00000000000000178, 23.05374883491397142, 14.16423886937410082 ) ) ;
#32976 = FACE_OUTER_BOUND ( 'NONE', #64772, .T. ) ;
#32978 = CARTESIAN_POINT ( 'NONE',  ( 19.42250999205614193, 40.14701867748817676, 5.440088680355555262 ) ) ;
#32979 = CARTESIAN_POINT ( 'NONE',  ( 0.5774900079438607392, 18.48035201082150536, 5.440088680355550821 ) ) ;
#32980 = CARTESIAN_POINT ( 'NONE',  ( 19.84674366389459266, 58.30059781766745886, 2.638427012816836559 ) ) ;
#32981 = ADVANCED_FACE ( 'NONE', ( #95237 ), #41290, .T. ) ;
#32982 = AXIS2_PLACEMENT_3D ( 'NONE', #49951, #80455, #95958 ) ;
#32983 = CARTESIAN_POINT ( 'NONE',  ( -9.795294835246881604, -28.02932231004771069, -3.750000000000001332 ) ) ;
#32984 = CARTESIAN_POINT ( 'NONE',  ( 0.1532563361054100626, 40.80059781766745886, -2.638427012816831230 ) ) ;
#32985 = CARTESIAN_POINT ( 'NONE',  ( 0.1532563361054082862, 6.217264484334118713, 2.638427012816831674 ) ) ;
#32986 = CARTESIAN_POINT ( 'NONE',  ( 9.846743663894594434, 23.50893115100079100, -2.168404344971008868E-15 ) ) ;
#32987 = ORIENTED_EDGE ( 'NONE', *, *, #34089, .T. ) ;
#32988 = CARTESIAN_POINT ( 'NONE',  ( 5.795997163830165277, 15.00000000000000000, -13.01802277140705932 ) ) ;
#32989 = CARTESIAN_POINT ( 'NONE',  ( 19.84674366389459266, 8.717264484334116048, -2.638427012816827677 ) ) ;
#32990 = CARTESIAN_POINT ( 'NONE',  ( 16.40814093676323893, 5.790301336597087456, 11.09922568453595026 ) ) ;
#32992 = CARTESIAN_POINT ( 'NONE',  ( 19.42250999205614548, 45.98035201082150536, -5.440088680355545492 ) ) ;
#32991 = CARTESIAN_POINT ( 'NONE',  ( 19.42250999205614193, 50.14701867748817676, 5.440088680355555262 ) ) ;
#32994 = CARTESIAN_POINT ( 'NONE',  ( 10.00000000000000178, 45.37363466993041783, 12.81628187352647608 ) ) ;
#32993 = CARTESIAN_POINT ( 'NONE',  ( 7.084665262690076126, 7.022018677488169658, -10.88017736071110164 ) ) ;
#32995 = VECTOR ( 'NONE', #40808, 1000.000000000000000 ) ;
#32996 = CARTESIAN_POINT ( 'NONE',  ( -2.266590686148945544, 27.22041550158063572, 7.082119434687048631 ) ) ;
#32997 = PRESENTATION_STYLE_ASSIGNMENT (( #27461 ) ) ;
#32998 = CIRCLE ( 'NONE', #63323, 14.49999999999999822 ) ;
#32999 =( BOUNDED_SURFACE ( )  B_SPLINE_SURFACE ( 3, 2, ( 
 ( #56158, #17671, #33135 ),
 ( #41164, #71648, #40165 ),
 ( #3156, #79635, #11134 ),
 ( #72120, #3648, #34113 ),
 ( #92661, #85174, #16684 ),
 ( #47154, #39689, #13100 ) ),
 .UNSPECIFIED., .F., .F., .F. ) 
 B_SPLINE_SURFACE_WITH_KNOTS ( ( 4, 2, 4 ),
 ( 3, 3 ),
 ( -1.734723475976807094E-17, 0.002729166040780114846, 0.005458332081560247039 ),
 ( 0.000000000000000000, 1.000000000000000000 ),
 .UNSPECIFIED. ) 
 GEOMETRIC_REPRESENTATION_ITEM ( )  RATIONAL_B_SPLINE_SURFACE ( (
 ( 1.000000000000000000, 0.8188293140827536121, 1.000000000000000000),
 ( 1.000000000000000000, 0.8032367185880369131, 1.000000000000000000),
 ( 1.000000000000000000, 0.7862107325766692911, 1.000000000000000000),
 ( 1.000000000000000000, 0.7489714018702576803, 1.000000000000000000),
 ( 1.000000000000000000, 0.7286611199003509842, 1.000000000000000000),
 ( 1.000000000000000000, 0.7071067811865507924, 1.000000000000000000) ) ) 
 REPRESENTATION_ITEM ( '' )  SURFACE ( )  );
#33001 = CARTESIAN_POINT ( 'NONE',  ( 6.565887622018943937, 53.08196800326374643, -12.81628187352647608 ) ) ;
#33000 = STYLED_ITEM ( 'NONE', ( #35595 ), #87902 ) ;
#33002 = VERTEX_POINT ( 'NONE', #87738 ) ;
#33003 = CARTESIAN_POINT ( 'NONE',  ( 0.1532563361054083140, 61.00893115100078745, 1.131784320476157264E-15 ) ) ;
#33004 = CARTESIAN_POINT ( 'NONE',  ( 15.44008868035555260, 14.73035201082150536, 9.422509992056143702 ) ) ;
#33006 = EDGE_LOOP ( 'NONE', ( #53552, #9714, #68153, #34092 ) ) ;
#33005 = EDGE_CURVE ( 'NONE', #69773, #55108, #33261, .T. ) ;
#33007 = CARTESIAN_POINT ( 'NONE',  ( 7.361572987183169658, 4.967264484334119601, -9.846743663894592657 ) ) ;
#33008 = FACE_OUTER_BOUND ( 'NONE', #13806, .T. ) ;
#33009 = CARTESIAN_POINT ( 'NONE',  ( 19.84674366389459266, 13.30059781766745353, 2.638427012816836559 ) ) ;
#33010 = CARTESIAN_POINT ( 'NONE',  ( -0.8801773607110991993, 67.85535201082151957, -2.915334737309923874 ) ) ;
#33011 = PLANE ( 'NONE',  #2785 ) ;
#33012 = CARTESIAN_POINT ( 'NONE',  ( 20.88017736071110875, 50.77201867748817676, -2.915334737309920765 ) ) ;
#33013 = CARTESIAN_POINT ( 'NONE',  ( 12.91533473730993009, 61.60535201082150536, -10.88017736071109987 ) ) ;
#33015 = ORIENTED_EDGE ( 'NONE', *, *, #44953, .T. ) ;
#33014 = CARTESIAN_POINT ( 'NONE',  ( 14.92337183194729988, 9.342264484334119601, -8.527530157486177487 ) ) ;
#33016 = AXIS2_PLACEMENT_3D ( 'NONE', #51541, #81047, #51041 ) ;
#33017 = CARTESIAN_POINT ( 'NONE',  ( 14.36383853300405988, 0.04962896932678220047, 3.367113227849034551 ) ) ;
#33018 = AXIS2_PLACEMENT_3D ( 'NONE', #36497, #5515, #35992 ) ;
#33019 = CARTESIAN_POINT ( 'NONE',  ( 12.63842701281683034, 52.46726448433413026, 9.846743663894596210 ) ) ;
#33020 = ORIENTED_EDGE ( 'NONE', *, *, #14994, .F. ) ;
#33021 = ORIENTED_EDGE ( 'NONE', *, *, #26972, .F. ) ;
#33022 = DIRECTION ( 'NONE',  ( -0.000000000000000000, 1.000000000000000000, -0.000000000000000000 ) ) ;
#33023 = CARTESIAN_POINT ( 'NONE',  ( 6.204703633549690345, 5.762082168247301794, -14.16423886937410259 ) ) ;
#33024 = CARTESIAN_POINT ( 'NONE',  ( 16.40814093676323893, 55.79030133659708923, 11.09922568453595026 ) ) ;
#33025 = CARTESIAN_POINT ( 'NONE',  ( -4.164238869374098151, 6.595415501580634832, -3.795296366450310543 ) ) ;
#33026 = CARTESIAN_POINT ( 'NONE',  ( -0.3689425029237881626, 32.42874883491395366, 10.36894250292379027 ) ) ;
#33027 = CARTESIAN_POINT ( 'NONE',  ( 1.087200977610002450, 0.000000000000000000, -5.343763529286909453 ) ) ;
#33028 = CARTESIAN_POINT ( 'NONE',  ( -4.164238869374098151, 1.595415501580634388, -3.795296366450310543 ) ) ;
#33029 = CARTESIAN_POINT ( 'NONE',  ( 15.44008868035555793, 16.39701867748817321, -9.422509992056140149 ) ) ;
#33030 = ORIENTED_EDGE ( 'NONE', *, *, #73216, .T. ) ;
#33031 = CARTESIAN_POINT ( 'NONE',  ( 7.361572987183170547, 7.050597817667451750, 9.846743663894590881 ) ) ;
#33032 = CARTESIAN_POINT ( 'NONE',  ( 17.20831665107776587, 14.13393115100078568, -7.208316651077762316 ) ) ;
#33033 = CARTESIAN_POINT ( 'NONE',  ( 16.40814093676323893, 30.79030133659708923, 11.09922568453595026 ) ) ;
#33034 = CARTESIAN_POINT ( 'NONE',  ( 0.1532563361054082862, 31.21726448433412315, 2.638427012816831674 ) ) ;
#33035 = DIRECTION ( 'NONE',  ( 0.000000000000000000, 4.683753385137383573E-14, -1.000000000000000000 ) ) ;
#33036 = CARTESIAN_POINT ( 'NONE',  ( -2.816281873526471635, 33.91530133659708213, -3.434112377981056508 ) ) ;
#33037 = DIRECTION ( 'NONE',  ( -5.818595309480553908E-17, -1.000000000000000000, -0.000000000000000000 ) ) ;
#33038 = CARTESIAN_POINT ( 'NONE',  ( 14.92337183194729633, 32.67559781766745175, 8.527530157486181039 ) ) ;
#33039 = CARTESIAN_POINT ( 'NONE',  ( 22.26659068614895176, 19.72041550158063572, -7.082119434687042414 ) ) ;
#33040 = ORIENTED_EDGE ( 'NONE', *, *, #98157, .F. ) ;
#33041 = VECTOR ( 'NONE', #53011, 1000.000000000000000 ) ;
#33042 = CARTESIAN_POINT ( 'NONE',  ( -0.8801773607110991993, 32.85535201082151247, -2.915334737309923874 ) ) ;
#33043 = CARTESIAN_POINT ( 'NONE',  ( 17.08211943468705130, 33.47041550158063927, 12.26659068614894998 ) ) ;
#33044 = CARTESIAN_POINT ( 'NONE',  ( 2.791683348922237240, 55.38393115100078745, -7.208316651077763204 ) ) ;
#33045 = CARTESIAN_POINT ( 'NONE',  ( 17.20831665107776587, 19.13393115100078035, -7.208316651077762316 ) ) ;
#33047 = DIRECTION ( 'NONE',  ( -0.000000000000000000, 1.000000000000000000, 0.000000000000000000 ) ) ;
#33046 = CARTESIAN_POINT ( 'NONE',  ( 13.43411237798106583, 57.66530133659708923, -12.81628187352647252 ) ) ;
#33048 = CARTESIAN_POINT ( 'NONE',  ( 12.91533473730992121, 34.52201867748817676, 10.88017736071110164 ) ) ;
#33049 = CARTESIAN_POINT ( 'NONE',  ( 0.000000000000000000, 15.00000000000000000, 0.000000000000000000 ) ) ;
#33050 = CARTESIAN_POINT ( 'NONE',  ( 19.38216949554541557, 17.24863466993041783, -9.382169495545420901 ) ) ;
#33051 = CARTESIAN_POINT ( 'NONE',  ( 10.00000000000000000, 34.75893115100078745, -9.846743663894594434 ) ) ;
#33052 = CARTESIAN_POINT ( 'NONE',  ( 9.422509992056141925, 5.147018677488180316, 5.440088680355547268 ) ) ;
#33053 = DIRECTION ( 'NONE',  ( 0.8070303256584298035, -0.5905099943842175847, 0.000000000000000000 ) ) ;
#33055 = DIRECTION ( 'NONE',  ( 0.000000000000000000, 0.000000000000000000, 1.000000000000000000 ) ) ;
#33054 = CARTESIAN_POINT ( 'NONE',  ( 17.96484262340118221, 64.93868534415483396, 7.964842623401181321 ) ) ;
#33056 = EDGE_CURVE ( 'NONE', #40528, #95502, #59217, .T. ) ;
#33057 = CARTESIAN_POINT ( 'NONE',  ( -10.32520421619553197, -40.46224970676419019, 4.000000000000000888 ) ) ;
#33058 = CARTESIAN_POINT ( 'NONE',  ( -13.61464873478178284, 14.49999999999999112, 6.296136897217746942 ) ) ;
#33059 = CARTESIAN_POINT ( 'NONE',  ( 10.00000000000000178, 49.31368534415484106, 10.88017736071110342 ) ) ;
#33060 = STYLED_ITEM ( 'NONE', ( #34201 ), #18110 ) ;
#33061 = CARTESIAN_POINT ( 'NONE',  ( 2.035157376598824452, 58.68868534415482685, 7.964842623401179544 ) ) ;
#33062 = CARTESIAN_POINT ( 'NONE',  ( -8.124115902427741176, 75.04369783535875627, -3.000000000000000000 ) ) ;
#33063 = FACE_OUTER_BOUND ( 'NONE', #64213, .T. ) ;
#33064 = CIRCLE ( 'NONE', #52203, 2.500000000000002220 ) ;
#33065 = CARTESIAN_POINT ( 'NONE',  ( 15.44008868035555260, 4.730352010821505360, 9.422509992056143702 ) ) ;
#33066 = CARTESIAN_POINT ( 'NONE',  ( -2.816281873526473856, -0.8763653300695799508, 9.499525473075851096E-16 ) ) ;
#33068 = CARTESIAN_POINT ( 'NONE',  ( 19.05866839779139355, 55.95508385108959715, -6.499999999999974243 ) ) ;
#33067 = CARTESIAN_POINT ( 'NONE',  ( 2.035157376598822676, 27.43868534415483396, -7.964842623401177768 ) ) ;
#33069 = CARTESIAN_POINT ( 'NONE',  ( 0.000000000000000000, 0.5000000000000004441, 0.000000000000000000 ) ) ;
#33070 = CARTESIAN_POINT ( 'NONE',  ( 3.591859063236761518, 24.95696800326375353, 11.09922568453594849 ) ) ;
#33071 = VERTEX_POINT ( 'NONE', #71764 ) ;
#33072 = CARTESIAN_POINT ( 'NONE',  ( 12.91533473730993009, 51.60535201082149825, -10.88017736071109987 ) ) ;
#33073 = CARTESIAN_POINT ( 'NONE',  ( 12.63842701281683034, 37.46726448433411605, 9.846743663894596210 ) ) ;
#33075 = LINE ( 'NONE', #63571, #79735 ) ;
#33074 = CARTESIAN_POINT ( 'NONE',  ( -2.816281873526473856, 9.331968003263753531, 3.434112377981055619 ) ) ;
#33076 = CARTESIAN_POINT ( 'NONE',  ( 2.035157376598822676, 27.43868534415483396, -7.964842623401177768 ) ) ;
#33077 = CARTESIAN_POINT ( 'NONE',  ( 7.084665262690076126, 39.10535201082150536, 10.88017736071109987 ) ) ;
#33078 = CARTESIAN_POINT ( 'NONE',  ( -2.266590686148945544, 46.38708216824730357, -7.082119434687050408 ) ) ;
#33079 = CARTESIAN_POINT ( 'NONE',  ( 1.472469842513823179, 41.42559781766745886, 4.923371831947296329 ) ) ;
#33080 = CARTESIAN_POINT ( 'NONE',  ( 0.5774900079438607392, 63.48035201082149825, 5.440088680355550821 ) ) ;
#33081 = CARTESIAN_POINT ( 'NONE',  ( 17.08211943468705130, 18.47041550158063572, 12.26659068614894998 ) ) ;
#33082 = AXIS2_PLACEMENT_3D ( 'NONE', #95480, #26971, #57469 ) ;
#33083 = AXIS2_PLACEMENT_3D ( 'NONE', #68212, #72849, #45199 ) ;
#33084 = DIRECTION ( 'NONE',  ( -1.000000000000000000, 0.000000000000000000, 0.000000000000000000 ) ) ;
#33085 = CARTESIAN_POINT ( 'NONE',  ( 0.1532563361054082862, 66.21726448433413736, 2.638427012816831674 ) ) ;
#33086 = VECTOR ( 'NONE', #96326, 1000.000000000000000 ) ;
#33087 = ORIENTED_EDGE ( 'NONE', *, *, #55445, .F. ) ;
#33088 = CARTESIAN_POINT ( 'NONE',  ( 24.16423886937410614, 44.51208216824730357, -3.795296366450302550 ) ) ;
#33090 = EDGE_CURVE ( 'NONE', #72566, #59600, #17790, .T. ) ;
#33089 = CARTESIAN_POINT ( 'NONE',  ( 6.204703633549690345, 42.84541550158063217, 14.16423886937410082 ) ) ;
#33091 = CARTESIAN_POINT ( 'NONE',  ( 5.076628168052703671, 11.84226448433411960, 8.527530157486179263 ) ) ;
#33092 = CARTESIAN_POINT ( 'NONE',  ( 22.81628187352647785, 21.41530133659708923, 3.434112377981063169 ) ) ;
#33093 = CARTESIAN_POINT ( 'NONE',  ( 1.472469842513823179, 66.42559781766745175, 4.923371831947296329 ) ) ;
#33094 = CARTESIAN_POINT ( 'NONE',  ( 20.10239578412224404, 52.63377557478296609, -6.340343622311915617 ) ) ;
#33096 = CARTESIAN_POINT ( 'NONE',  ( 21.09922568453595559, 32.04030133659708923, -6.408140936763230044 ) ) ;
#33095 = CARTESIAN_POINT ( 'NONE',  ( 20.88017736071110875, 55.77201867748816966, -2.915334737309920765 ) ) ;
#33097 = CARTESIAN_POINT ( 'NONE',  ( 24.16423886937410614, 44.51208216824730357, -3.795296366450302550 ) ) ;
#33098 = EDGE_CURVE ( 'NONE', #18747, #69558, #3389, .T. ) ;
#33099 = CARTESIAN_POINT ( 'NONE',  ( 10.17177286909470624, 0.2301502795151879610, -10.94336654633681327 ) ) ;
#33100 = CARTESIAN_POINT ( 'NONE',  ( 17.96484262340118221, 64.93868534415483396, 7.964842623401181321 ) ) ;
#33101 = CARTESIAN_POINT ( 'NONE',  ( 9.846743663894590881, -6.282735515665877735, -2.638427012816833894 ) ) ;
#33102 = ORIENTED_EDGE ( 'NONE', *, *, #92517, .T. ) ;
#33103 = DIRECTION ( 'NONE',  ( 0.000000000000000000, -1.000000000000000000, 0.000000000000000000 ) ) ;
#33104 = VERTEX_POINT ( 'NONE', #26745 ) ;
#33105 = CARTESIAN_POINT ( 'NONE',  ( 17.08211943468705840, 5.137082168247300906, -12.26659068614894466 ) ) ;
#33107 = CARTESIAN_POINT ( 'NONE',  ( -0.8801773607111009756, 8.063685344154837509, 1.068504757029289695E-15 ) ) ;
#33106 = CARTESIAN_POINT ( 'NONE',  ( 15.44008868035555793, 11.39701867748817143, -9.422509992056140149 ) ) ;
#33109 = CARTESIAN_POINT ( 'NONE',  ( 16.40814093676323893, 10.79030133659708923, 11.09922568453595026 ) ) ;
#33108 = CARTESIAN_POINT ( 'NONE',  ( 12.63842701281683034, 37.46726448433411605, 9.846743663894596210 ) ) ;
#33110 = DIRECTION ( 'NONE',  ( 2.569960705150826877E-16, -1.000000000000000000, 0.000000000000000000 ) ) ;
#33111 = CARTESIAN_POINT ( 'NONE',  ( -13.86102707272217494, 15.00000000000000711, -4.666951904077385471 ) ) ;
#33112 = CARTESIAN_POINT ( 'NONE',  ( 6.565887622018943937, 20.16530133659708213, 12.81628187352647430 ) ) ;
#33113 = CARTESIAN_POINT ( 'NONE',  ( -11.09922568453595382, 28.70696800326377840, -6.408140936763226492 ) ) ;
#33114 = VERTEX_POINT ( 'NONE', #57729 ) ;
#33115 = CARTESIAN_POINT ( 'NONE',  ( 13.79529636645031943, 45.34541550158062506, -14.16423886937409904 ) ) ;
#33116 = ORIENTED_EDGE ( 'NONE', *, *, #15058, .F. ) ;
#33117 = CARTESIAN_POINT ( 'NONE',  ( -4.164238869374099927, 57.01208216824731068, 3.795296366450308767 ) ) ;
#33118 = ORIENTED_EDGE ( 'NONE', *, *, #17170, .F. ) ;
#33119 = CARTESIAN_POINT ( 'NONE',  ( -0.8801773607111008646, 28.27201867748817321, 2.915334737309923430 ) ) ;
#33120 = CARTESIAN_POINT ( 'NONE',  ( -0.8801773607110991993, 32.85535201082151247, -2.915334737309923874 ) ) ;
#33121 = CARTESIAN_POINT ( 'NONE',  ( 7.084665262690076126, 37.02201867748817676, -10.88017736071110164 ) ) ;
#33122 = CARTESIAN_POINT ( 'NONE',  ( 7.084665262690076126, 62.02201867748816966, -10.88017736071110164 ) ) ;
#33123 = CARTESIAN_POINT ( 'NONE',  ( 20.88017736071110519, 25.56368534415483751, 2.639326808657452039E-16 ) ) ;
#33124 = EDGE_CURVE ( 'NONE', #12575, #30635, #11254, .T. ) ;
#33125 = TOROIDAL_SURFACE ( 'NONE', #41149, 14.49999999999999822, 0.5000000000000000000 ) ;
#33127 = VECTOR ( 'NONE', #37769, 999.9999999999998863 ) ;
#33126 = CARTESIAN_POINT ( 'NONE',  ( 19.72487221294571214, 22.80223176428831877, -6.499999999999988454 ) ) ;
#33128 = CARTESIAN_POINT ( 'NONE',  ( 7.361572987183169658, 9.967264484334119601, -9.846743663894592657 ) ) ;
#33129 = VERTEX_POINT ( 'NONE', #33737 ) ;
#33130 = CARTESIAN_POINT ( 'NONE',  ( 12.63842701281683034, 47.46726448433412315, 9.846743663894596210 ) ) ;
#33131 = CARTESIAN_POINT ( 'NONE',  ( -14.66196617519555545, 0.2306972965111886154, -2.874856965128016473 ) ) ;
#33132 = CARTESIAN_POINT ( 'NONE',  ( 0.6178305044545818747, 43.49863466993042493, -9.382169495545419124 ) ) ;
#33133 = CARTESIAN_POINT ( 'NONE',  ( -8.000000000000000000, 79.82179676972448590, 4.000000000000000000 ) ) ;
#33134 = AXIS2_PLACEMENT_3D ( 'NONE', #59169, #45154, #37673 ) ;
#33135 = CARTESIAN_POINT ( 'NONE',  ( -46.30928139467842186, 104.0823827281712397, 5.529860068218138025 ) ) ;
#33136 = CARTESIAN_POINT ( 'NONE',  ( 10.00000000000000000, 64.75893115100078035, -9.846743663894594434 ) ) ;
#33137 = CARTESIAN_POINT ( 'NONE',  ( -0.3689425029237881626, 42.42874883491396787, 10.36894250292379027 ) ) ;
#33138 = CARTESIAN_POINT ( 'NONE',  ( 11.96291822454875842, 15.00000000000000000, 8.193813980849165901 ) ) ;
#33139 = ORIENTED_EDGE ( 'NONE', *, *, #29117, .F. ) ;
#33140 = CARTESIAN_POINT ( 'NONE',  ( 14.15281240980445077, 15.00000000000000178, 3.688687068602797492 ) ) ;
#33141 = CARTESIAN_POINT ( 'NONE',  ( 17.20831665107776587, 24.13393115100078035, -7.208316651077762316 ) ) ;
#33142 = VECTOR ( 'NONE', #27876, 1000.000000000000000 ) ;
#33143 = CARTESIAN_POINT ( 'NONE',  ( 4.219999999999999751, 10.00000000000000000, -2.500000000000000000 ) ) ;
#33144 = CARTESIAN_POINT ( 'NONE',  ( 7.361572987183169658, 59.96726448433410894, -9.846743663894592657 ) ) ;
#33145 = CARTESIAN_POINT ( 'NONE',  ( 10.00000000000000178, 2.258931151000784787, 9.846743663894594434 ) ) ;
#33146 = VECTOR ( 'NONE', #47588, 1000.000000000000000 ) ;
#33147 = DIRECTION ( 'NONE',  ( 0.000000000000000000, 0.000000000000000000, -1.000000000000000000 ) ) ;
#33148 = CARTESIAN_POINT ( 'NONE',  ( 0.1532563361054100626, 60.80059781766744464, -2.638427012816831230 ) ) ;
#33149 = VECTOR ( 'NONE', #82661, 999.9999999999998863 ) ;
#33150 = CARTESIAN_POINT ( 'NONE',  ( 4.395797040798766098, -0.8371465525189527579, -2.750000000000000444 ) ) ;
#33151 = EDGE_LOOP ( 'NONE', ( #17522, #21569, #26333, #36061 ) ) ;
#33152 = CARTESIAN_POINT ( 'NONE',  ( -4.164238869374099927, 62.01208216824728936, 3.795296366450308767 ) ) ;
#33153 = DIRECTION ( 'NONE',  ( -0.000000000000000000, -1.000000000000000000, -0.000000000000000000 ) ) ;
#33154 = CARTESIAN_POINT ( 'NONE',  ( 7.084665262690076126, 42.02201867748816966, -10.88017736071110164 ) ) ;
#33156 = DIRECTION ( 'NONE',  ( 1.000000000000000000, -0.000000000000000000, -0.000000000000000000 ) ) ;
#33155 = CARTESIAN_POINT ( 'NONE',  ( 3.591859063236763294, 8.290301336597087456, -11.09922568453595026 ) ) ;
#33157 = CARTESIAN_POINT ( 'NONE',  ( -13.61464873478158211, 0.5000000000000004441, -6.296136897218027606 ) ) ;
#33158 = CARTESIAN_POINT ( 'NONE',  ( 0.000000000000000000, 14.49999999999999822, 0.000000000000000000 ) ) ;
#33159 = CARTESIAN_POINT ( 'NONE',  ( 1.046131998950040831, 30.73810908735726244, 6.499999999999992006 ) ) ;
#33160 = CARTESIAN_POINT ( 'NONE',  ( 10.00000000000000178, 57.25893115100078745, 9.846743663894594434 ) ) ;
#33161 = CARTESIAN_POINT ( 'NONE',  ( 7.361572987183170547, 7.050597817667451750, 9.846743663894590881 ) ) ;
#33162 = B_SPLINE_CURVE_WITH_KNOTS ( 'NONE', 3,
 ( #8785, #1322, #82812, #53299, #98344, #38803 ),
 .UNSPECIFIED., .F., .F.,
 ( 4, 2, 4 ),
 ( 3.409110551482055714E-05, 0.0004400426677366462216, 0.0008459942299584719471 ),
 .UNSPECIFIED. ) ;
#33163 = CARTESIAN_POINT ( 'NONE',  ( -7.964842623401179544, -37.56131465584516604, -7.964842623401174215 ) ) ;
#33164 = CARTESIAN_POINT ( 'NONE',  ( 22.81628187352648496, 11.83196800326375531, -3.434112377981050290 ) ) ;
#33166 = FACE_OUTER_BOUND ( 'NONE', #92756, .T. ) ;
#33165 = CARTESIAN_POINT ( 'NONE',  ( 2.035157376598824452, 13.68868534415483751, 7.964842623401179544 ) ) ;
#33167 = PLANE ( 'NONE',  #58015 ) ;
#33168 = CARTESIAN_POINT ( 'NONE',  ( 24.16423886937410614, 34.51208216824731068, -3.795296366450302550 ) ) ;
#33169 = EDGE_CURVE ( 'NONE', #6101, #34568, #57738, .T. ) ;
#33170 = CARTESIAN_POINT ( 'NONE',  ( -0.3689425029237881626, 32.42874883491395366, 10.36894250292379027 ) ) ;
#33171 = CARTESIAN_POINT ( 'NONE',  ( -0.8801773607111008646, 3.272018677488171434, 2.915334737309923430 ) ) ;
#33172 = CARTESIAN_POINT ( 'NONE',  ( 19.84674366389459621, 33.50893115100078745, 7.409399052514197653E-17 ) ) ;
#33173 = CARTESIAN_POINT ( 'NONE',  ( 3.591859063236763294, 43.29030133659708923, -11.09922568453595026 ) ) ;
#33174 = CARTESIAN_POINT ( 'NONE',  ( 4.559911319644449179, 13.89701867748817143, 9.422509992056141925 ) ) ;
#33175 = B_SPLINE_CURVE_WITH_KNOTS ( 'NONE', 3,
 ( #40619, #8636, #85129, #16640, #78613, #63104 ),
 .UNSPECIFIED., .F., .F.,
 ( 4, 2, 4 ),
 ( 3.409110551496089355E-05, 0.0004400426677367838069, 0.0008459942299586067135 ),
 .UNSPECIFIED. ) ;
#33176 = ORIENTED_EDGE ( 'NONE', *, *, #43035, .F. ) ;
#33177 = CARTESIAN_POINT ( 'NONE',  ( 18.52753015748618282, 33.92559781766745886, -4.923371831947291888 ) ) ;
#33178 = CARTESIAN_POINT ( 'NONE',  ( 19.42250999205614548, 40.98035201082150536, -5.440088680355545492 ) ) ;
#33179 = CARTESIAN_POINT ( 'NONE',  ( 13.43411237798105340, 5.581968003263753531, 12.81628187352647963 ) ) ;
#33181 = DIRECTION ( 'NONE',  ( 1.000000000000000000, 0.000000000000000000, 0.000000000000000000 ) ) ;
#33180 = CARTESIAN_POINT ( 'NONE',  ( 6.204703633549690345, 15.76208216824730179, -14.16423886937410259 ) ) ;
#33182 = CARTESIAN_POINT ( 'NONE',  ( -2.120353041430432128, 15.00000000000000000, -14.34413130794946234 ) ) ;
#33183 = UNCERTAINTY_MEASURE_WITH_UNIT (LENGTH_MEASURE( 1.000000000000000082E-05 ), #3816, 'distance_accuracy_value', 'NONE');
#33184 = CARTESIAN_POINT ( 'NONE',  ( 12.63842701281683034, 27.46726448433411250, 9.846743663894596210 ) ) ;
#33185 = CARTESIAN_POINT ( 'NONE',  ( -2.816281873526471635, 53.91530133659709634, -3.434112377981056508 ) ) ;
#33186 = CARTESIAN_POINT ( 'NONE',  ( 18.52753015748617571, 58.09226448433411605, 4.923371831947298993 ) ) ;
#33187 = ORIENTED_EDGE ( 'NONE', *, *, #73132, .T. ) ;
#33188 = PLANE ( 'NONE',  #98830 ) ;
#33189 = FILL_AREA_STYLE ('',( #11182 ) ) ;
#33190 = CARTESIAN_POINT ( 'NONE',  ( 2.917880565312948704, 62.63708216824730357, 12.26659068614894643 ) ) ;
#33191 = CARTESIAN_POINT ( 'NONE',  ( 2.917880565312948704, 17.63708216824730357, 12.26659068614894643 ) ) ;
#33192 = CARTESIAN_POINT ( 'NONE',  ( 15.44008868035555260, 64.73035201082151957, 9.422509992056143702 ) ) ;
#33193 = CARTESIAN_POINT ( 'NONE',  ( 2.791683348922240793, 46.63393115100077324, 7.208316651077764092 ) ) ;
#33194 = CARTESIAN_POINT ( 'NONE',  ( 15.44008868035555260, 24.73035201082150891, 9.422509992056143702 ) ) ;
#33195 = FACE_OUTER_BOUND ( 'NONE', #83792, .T. ) ;
#33196 = DIRECTION ( 'NONE',  ( 0.000000000000000000, -1.000000000000000000, 0.000000000000000000 ) ) ;
#33197 = AXIS2_PLACEMENT_3D ( 'NONE', #7046, #8520, #77993 ) ;
#33198 = CARTESIAN_POINT ( 'NONE',  ( 7.882504294823842628, 15.00000000000000711, 12.32089577884796050 ) ) ;
#33199 = VERTEX_POINT ( 'NONE', #64239 ) ;
#33200 = ORIENTED_EDGE ( 'NONE', *, *, #47745, .T. ) ;
#33201 = LINE ( 'NONE', #35165, #80476 ) ;
#33202 = CARTESIAN_POINT ( 'NONE',  ( 20.36894250292379738, 14.92874883491396432, -10.36894250292379027 ) ) ;
#33204 = EDGE_CURVE ( 'NONE', #4701, #68203, #71105, .T. ) ;
#33203 = SURFACE_SIDE_STYLE ('',( #40232 ) ) ;
#33205 = CARTESIAN_POINT ( 'NONE',  ( -2.266590686148945544, 41.38708216824729647, -7.082119434687050408 ) ) ;
#33206 = CARTESIAN_POINT ( 'NONE',  ( 10.00000000000000178, 57.25893115100078745, 9.846743663894594434 ) ) ;
#33207 = CARTESIAN_POINT ( 'NONE',  ( 12.63842701281683034, 27.46726448433411250, 9.846743663894596210 ) ) ;
#33208 = FACE_OUTER_BOUND ( 'NONE', #83051, .T. ) ;
#33210 = CARTESIAN_POINT ( 'NONE',  ( 19.84674366389459266, 58.30059781766745886, 2.638427012816836559 ) ) ;
#33209 = CARTESIAN_POINT ( 'NONE',  ( 19.42250999205614193, 20.14701867748817321, 5.440088680355555262 ) ) ;
#33211 = CARTESIAN_POINT ( 'NONE',  ( 11.10136736363534560, 0.04922511925147036310, -9.716261771424912652 ) ) ;
#33212 = CARTESIAN_POINT ( 'NONE',  ( 12.91533473730993009, 11.60535201082150714, -10.88017736071109987 ) ) ;
#33213 = DIRECTION ( 'NONE',  ( -0.9025852843498618494, 0.000000000000000000, 0.4305110968082926926 ) ) ;
#33214 = CARTESIAN_POINT ( 'NONE',  ( 17.75000000000000000, 78.80384757729336798, 4.000000000000000000 ) ) ;
#33215 = CARTESIAN_POINT ( 'NONE',  ( 17.96484262340118221, 59.93868534415484106, 7.964842623401181321 ) ) ;
#33216 = ADVANCED_FACE ( 'NONE', ( #3777 ), #34230, .T. ) ;
#33217 = CARTESIAN_POINT ( 'NONE',  ( 7.361572987183170547, 12.05059781766744997, 9.846743663894590881 ) ) ;
#33218 =( GEOMETRIC_REPRESENTATION_CONTEXT ( 3 ) GLOBAL_UNCERTAINTY_ASSIGNED_CONTEXT ( ( #81144 ) ) GLOBAL_UNIT_ASSIGNED_CONTEXT ( ( #82421, #79101, #13945 ) ) REPRESENTATION_CONTEXT ( 'NONE', 'WORKASPACE' ) );
#33219 = CARTESIAN_POINT ( 'NONE',  ( -7.117921737454939723, -58.38558715620312256, 4.000000000000000888 ) ) ;
#33220 = ORIENTED_EDGE ( 'NONE', *, *, #17437, .F. ) ;
#33221 = VERTEX_POINT ( 'NONE', #19741 ) ;
#33222 = CARTESIAN_POINT ( 'NONE',  ( 2.791683348922237240, 20.38393115100078745, -7.208316651077763204 ) ) ;
#33223 = ORIENTED_EDGE ( 'NONE', *, *, #16283, .T. ) ;
#33224 = CARTESIAN_POINT ( 'NONE',  ( -4.164238869374099039, 36.80374883491396787, 8.674139862899312516E-16 ) ) ;
#33225 = CARTESIAN_POINT ( 'NONE',  ( 12.63842701281683034, 27.46726448433411250, 9.846743663894596210 ) ) ;
#33226 = CARTESIAN_POINT ( 'NONE',  ( 4.559911319644449179, 48.89701867748817676, 9.422509992056141925 ) ) ;
#33227 = CIRCLE ( 'NONE', #89111, 2.250000000000001332 ) ;
#33228 = SURFACE_STYLE_USAGE ( .BOTH. , #78746 ) ;
#33229 = ORIENTED_EDGE ( 'NONE', *, *, #52279, .F. ) ;
#33230 = AXIS2_PLACEMENT_3D ( 'NONE', #52653, #81665, #5693 ) ;
#33231 = CARTESIAN_POINT ( 'NONE',  ( 4.559911319644449179, 43.89701867748816966, 9.422509992056141925 ) ) ;
#33232 = DIRECTION ( 'NONE',  ( 0.8788171126619646056, -0.000000000000000000, 0.4771587602596096267 ) ) ;
#33233 = CARTESIAN_POINT ( 'NONE',  ( -12.81628187352647963, -1.084698663402915653, -3.434112377981046293 ) ) ;
#33234 = ORIENTED_EDGE ( 'NONE', *, *, #11281, .F. ) ;
#33235 = CARTESIAN_POINT ( 'NONE',  ( 4.559911319644449179, 43.89701867748816966, 9.422509992056141925 ) ) ;
#33236 = CARTESIAN_POINT ( 'NONE',  ( 17.08211943468705840, 5.137082168247300906, -12.26659068614894466 ) ) ;
#33237 = ORIENTED_EDGE ( 'NONE', *, *, #43586, .F. ) ;
#33238 = ORIENTED_EDGE ( 'NONE', *, *, #82890, .T. ) ;
#33239 = CARTESIAN_POINT ( 'NONE',  ( 16.40814093676324603, 37.45696800326376064, -11.09922568453594671 ) ) ;
#33240 = CARTESIAN_POINT ( 'NONE',  ( 2.791683348922240793, 26.63393115100078745, 7.208316651077764092 ) ) ;
#33241 = CARTESIAN_POINT ( 'NONE',  ( 7.084665262690076126, 4.105352010821503583, 10.88017736071109987 ) ) ;
#33242 = CARTESIAN_POINT ( 'NONE',  ( 0.4400000000000020006, 1.019547802438468986, 3.750000000000000000 ) ) ;
#33243 = CARTESIAN_POINT ( 'NONE',  ( 10.00000000000000000, 34.75893115100078745, -9.846743663894594434 ) ) ;
#33244 = ADVANCED_FACE ( 'NONE', ( #49734 ), #40784, .F. ) ;
#33245 = CARTESIAN_POINT ( 'NONE',  ( -0.8801773607111008646, 58.27201867748816966, 2.915334737309923430 ) ) ;
#33246 = PRESENTATION_STYLE_ASSIGNMENT (( #26246 ) ) ;
#33247 = CARTESIAN_POINT ( 'NONE',  ( 0.2751277870542967463, 0.000000000000000000, 6.500000000000000888 ) ) ;
#33248 = DIRECTION ( 'NONE',  ( 0.5664062369248205053, 0.000000000000000000, 0.8241261886220241362 ) ) ;
#33249 = CARTESIAN_POINT ( 'NONE',  ( -2.816281873526471635, 63.91530133659708923, -3.434112377981056508 ) ) ;
#33250 = CARTESIAN_POINT ( 'NONE',  ( 5.076628168052704559, 5.175597817667451750, -8.527530157486179263 ) ) ;
#33251 = CARTESIAN_POINT ( 'NONE',  ( -2.816281873526471635, 13.91530133659708746, -3.434112377981056508 ) ) ;
#33252 = LINE ( 'NONE', #63745, #16400 ) ;
#33254 = EDGE_CURVE ( 'NONE', #11366, #95706, #46554, .T. ) ;
#33253 = B_SPLINE_CURVE_WITH_KNOTS ( 'NONE', 3,
 ( #22524, #83511, #47954, #70480, #1513, #70979, #24993, #32954, #55476, #63457 ),
 .UNSPECIFIED., .F., .F.,
 ( 4, 3, 3, 4 ),
 ( 0.000000000000000000, 0.0006253016069560473613, 0.001250604074564875320, 0.002501455912506565619 ),
 .UNSPECIFIED. ) ;
#33255 = CARTESIAN_POINT ( 'NONE',  ( 17.20831665107776587, 47.88393115100078745, 7.208316651077764980 ) ) ;
#33256 = CARTESIAN_POINT ( 'NONE',  ( 0.6178305044545818747, 63.49863466993043204, -9.382169495545419124 ) ) ;
#33257 = CARTESIAN_POINT ( 'NONE',  ( 2.917880565312950480, 5.970415501580634832, -12.26659068614894821 ) ) ;
#33258 = CARTESIAN_POINT ( 'NONE',  ( 18.52753015748618282, 28.92559781766745175, -4.923371831947291888 ) ) ;
#33259 = CARTESIAN_POINT ( 'NONE',  ( -1.099225684535947600, 34.54030133659708923, 6.408140936763237150 ) ) ;
#33261 = LINE ( 'NONE', #49257, #33625 ) ;
#33260 = PRESENTATION_STYLE_ASSIGNMENT (( #48264 ) ) ;
#33262 = CARTESIAN_POINT ( 'NONE',  ( 19.42250999205614193, 50.14701867748817676, 5.440088680355555262 ) ) ;
#33263 = CARTESIAN_POINT ( 'NONE',  ( 3.591859063236763294, 3.290301336597087012, -11.09922568453595026 ) ) ;
#33264 = CARTESIAN_POINT ( 'NONE',  ( 19.84674366389459266, 23.71726448433412315, -2.638427012816827677 ) ) ;
#33265 = CARTESIAN_POINT ( 'NONE',  ( 19.42250999205614548, 20.98035201082150891, -5.440088680355545492 ) ) ;
#33266 = CARTESIAN_POINT ( 'NONE',  ( 13.43411237798106583, 27.66530133659708568, -12.81628187352647252 ) ) ;
#33267 = DIRECTION ( 'NONE',  ( -1.483861936729427615E-16, 1.000000000000000000, 0.000000000000000000 ) ) ;
#33268 = CARTESIAN_POINT ( 'NONE',  ( 0.5774900079438607392, 13.48035201082150358, 5.440088680355550821 ) ) ;
#33269 = CARTESIAN_POINT ( 'NONE',  ( 4.559911319644449179, 57.23035201082150536, -9.422509992056141925 ) ) ;
#33270 = CARTESIAN_POINT ( 'NONE',  ( 0.5774900079438607392, 8.480352010821505360, 5.440088680355550821 ) ) ;
#33272 = CARTESIAN_POINT ( 'NONE',  ( 0.5774900079438590739, 27.64701867748817676, -5.440088680355550821 ) ) ;
#33271 = CARTESIAN_POINT ( 'NONE',  ( 5.076628168052703671, 36.84226448433412315, 8.527530157486179263 ) ) ;
#33273 = CARTESIAN_POINT ( 'NONE',  ( -7.551349515323269479, -0.03417435944610275333, 12.08468537022900868 ) ) ;
#33274 = CARTESIAN_POINT ( 'NONE',  ( 20.88017736071110164, 45.35535201082149115, 2.915334737309930979 ) ) ;
#33275 =( GEOMETRIC_REPRESENTATION_CONTEXT ( 3 ) GLOBAL_UNCERTAINTY_ASSIGNED_CONTEXT ( ( #97169 ) ) GLOBAL_UNIT_ASSIGNED_CONTEXT ( ( #12114, #96620, #89099 ) ) REPRESENTATION_CONTEXT ( 'NONE', 'WORKASPACE' ) );
#33277 = CARTESIAN_POINT ( 'NONE',  ( 4.879999999999994564, 43.00000000000000711, -6.250000000000000000 ) ) ;
#33276 = CARTESIAN_POINT ( 'NONE',  ( 7.084665262690076126, 17.02201867748817676, -10.88017736071110164 ) ) ;
#33278 = CARTESIAN_POINT ( 'NONE',  ( 20.24186590665277663, 54.73410085661204505, 6.114288769123050749 ) ) ;
#33279 = CARTESIAN_POINT ( 'NONE',  ( 12.63842701281683034, 32.46726448433412315, 9.846743663894596210 ) ) ;
#33280 = CARTESIAN_POINT ( 'NONE',  ( -46.68456736488006698, 103.6675473310227176, 5.775421524742653467 ) ) ;
#33281 = CARTESIAN_POINT ( 'NONE',  ( 10.00000000000000178, 5.373634669930420493, 12.81628187352647608 ) ) ;
#33283 = CARTESIAN_POINT ( 'NONE',  ( -12.34557190004669458, 14.95077488074853456, -8.076692058882660064 ) ) ;
#33282 = VECTOR ( 'NONE', #94103, 1000.000000000000000 ) ;
#33284 = EDGE_CURVE ( 'NONE', #24535, #23105, #80659, .T. ) ;
#33285 = PRESENTATION_LAYER_ASSIGNMENT (  '', '', ( #34794 ) ) ;
#33286 = CARTESIAN_POINT ( 'NONE',  ( 13.79529636645030344, 28.26208216824729647, 14.16423886937410614 ) ) ;
#33287 = CARTESIAN_POINT ( 'NONE',  ( 10.00000000000000178, 0.000000000000000000, 0.000000000000000000 ) ) ;
#33288 = ORIENTED_EDGE ( 'NONE', *, *, #7658, .T. ) ;
#33289 = CARTESIAN_POINT ( 'NONE',  ( -2.266590686148945544, 62.22041550158063927, 7.082119434687048631 ) ) ;
#33290 = ADVANCED_FACE ( 'NONE', ( #82710 ), #54052, .F. ) ;
#33291 = CARTESIAN_POINT ( 'NONE',  ( 10.00000000000000178, 27.25893115100078390, 9.846743663894594434 ) ) ;
#33292 = DIRECTION ( 'NONE',  ( 0.000000000000000000, 0.000000000000000000, 1.000000000000000000 ) ) ;
#33293 = CARTESIAN_POINT ( 'NONE',  ( 19.42250999205614548, 55.98035201082150536, -5.440088680355545492 ) ) ;
#33294 = CARTESIAN_POINT ( 'NONE',  ( 22.81628187352648496, 61.83196800326376774, -3.434112377981050290 ) ) ;
#33295 = CARTESIAN_POINT ( 'NONE',  ( 20.88017736071110519, 30.56368534415484106, 2.639326808657452039E-16 ) ) ;
#33296 = DIRECTION ( 'NONE',  ( 0.000000000000000000, 1.000000000000000000, 0.000000000000000000 ) ) ;
#33297 = CARTESIAN_POINT ( 'NONE',  ( -2.816281873526473856, 9.123634669930421381, 9.499525473075851096E-16 ) ) ;
#33298 = CARTESIAN_POINT ( 'NONE',  ( 2.791683348922240793, 11.63393115100078568, 7.208316651077764092 ) ) ;
#33299 = ORIENTED_EDGE ( 'NONE', *, *, #18233, .F. ) ;
#33300 =( LENGTH_UNIT ( ) NAMED_UNIT ( * ) SI_UNIT ( .MILLI., .METRE. ) );
#33301 = CARTESIAN_POINT ( 'NONE',  ( 2.863845842055925406, 14.95077488074853456, -14.47219703936412927 ) ) ;
#33302 = CARTESIAN_POINT ( 'NONE',  ( 24.16423886937410614, 54.30374883491396787, 8.672049930838204340E-16 ) ) ;
#33303 = CARTESIAN_POINT ( 'NONE',  ( -4.164238869374099927, 22.01208216824730357, 3.795296366450308767 ) ) ;
#33304 = CARTESIAN_POINT ( 'NONE',  ( 17.96484262340118221, 31.18868534415483751, -7.964842623401177768 ) ) ;
#33305 = CARTESIAN_POINT ( 'NONE',  ( 4.559911319644449179, 43.89701867748816966, 9.422509992056141925 ) ) ;
#33306 =( NAMED_UNIT ( * ) PLANE_ANGLE_UNIT ( ) SI_UNIT ( $, .RADIAN. ) );
#33307 = CARTESIAN_POINT ( 'NONE',  ( -7.684764310694706779, 0.3640475087720986269, -12.88194075009946182 ) ) ;
#33308 = CARTESIAN_POINT ( 'NONE',  ( 19.84674366389459266, 8.300597817667451750, 2.638427012816836559 ) ) ;
#33309 = DIRECTION ( 'NONE',  ( 0.000000000000000000, 0.000000000000000000, -1.000000000000000000 ) ) ;
#33310 = CARTESIAN_POINT ( 'NONE',  ( 18.52753015748618282, 13.92559781766745175, -4.923371831947291888 ) ) ;
#33311 = CARTESIAN_POINT ( 'NONE',  ( 19.84674366389459266, 23.30059781766745530, 2.638427012816836559 ) ) ;
#33312 = CARTESIAN_POINT ( 'NONE',  ( 0.1532563361054082862, 51.21726448433412315, 2.638427012816831674 ) ) ;
#33313 = UNCERTAINTY_MEASURE_WITH_UNIT (LENGTH_MEASURE( 1.000000000000000082E-05 ), #81747, 'distance_accuracy_value', 'NONE');
#33314 = CARTESIAN_POINT ( 'NONE',  ( 13.43411237798106583, 37.66530133659708923, -12.81628187352647252 ) ) ;
#33315 = CARTESIAN_POINT ( 'NONE',  ( 0.5774900079438590739, 57.64701867748817676, -5.440088680355550821 ) ) ;
#33316 = CARTESIAN_POINT ( 'NONE',  ( 17.20831665107776587, 29.13393115100078390, -7.208316651077762316 ) ) ;
#33318 = CARTESIAN_POINT ( 'NONE',  ( 10.00000000000000000, 19.75893115100078390, -9.846743663894594434 ) ) ;
#33317 = CARTESIAN_POINT ( 'NONE',  ( -2.266590686148945544, 47.22041550158063927, 7.082119434687048631 ) ) ;
#33319 = DIRECTION ( 'NONE',  ( -0.8433914458128813907, 0.000000000000000000, -0.5372996083468306594 ) ) ;
#33320 = CARTESIAN_POINT ( 'NONE',  ( 17.20831665107776587, 54.13393115100079456, -7.208316651077762316 ) ) ;
#33322 = CARTESIAN_POINT ( 'NONE',  ( 17.08211943468705130, 8.470415501580635720, 12.26659068614894998 ) ) ;
#33321 = CARTESIAN_POINT ( 'NONE',  ( 2.791683348922237240, 50.38393115100078035, -7.208316651077763204 ) ) ;
#33323 = CARTESIAN_POINT ( 'NONE',  ( 10.00000000000000178, 33.05374883491396787, 14.16423886937410082 ) ) ;
#33324 = CARTESIAN_POINT ( 'NONE',  ( 14.92337183194729633, 27.67559781766745530, 8.527530157486181039 ) ) ;
#33325 = CARTESIAN_POINT ( 'NONE',  ( 4.559911319644449179, 22.23035201082150536, -9.422509992056141925 ) ) ;
#33326 = EDGE_CURVE ( 'NONE', #69120, #80329, #50741, .T. ) ;
#33327 = CARTESIAN_POINT ( 'NONE',  ( 15.44008868035555260, 49.73035201082150536, 9.422509992056143702 ) ) ;
#33328 = CARTESIAN_POINT ( 'NONE',  ( 4.559911319644449179, 42.23035201082151247, -9.422509992056141925 ) ) ;
#33329 = ORIENTED_EDGE ( 'NONE', *, *, #64090, .T. ) ;
#33330 = CARTESIAN_POINT ( 'NONE',  ( 19.38216949554541557, 32.24863466993041783, -9.382169495545420901 ) ) ;
#33331 = CARTESIAN_POINT ( 'NONE',  ( 15.44008868035555260, 54.73035201082150536, 9.422509992056143702 ) ) ;
#33332 = ORIENTED_EDGE ( 'NONE', *, *, #66504, .T. ) ;
#33333 = CARTESIAN_POINT ( 'NONE',  ( 10.00000000000000000, -0.2410688489992152128, -9.846743663894594434 ) ) ;
#33334 = CARTESIAN_POINT ( 'NONE',  ( 7.084665262690076126, 64.10535201082150536, 10.88017736071109987 ) ) ;
#33335 = EDGE_LOOP ( 'NONE', ( #94593, #47255, #8000, #90030 ) ) ;
#33336 = CARTESIAN_POINT ( 'NONE',  ( 2.035157376598822676, 57.43868534415484106, -7.964842623401177768 ) ) ;
#33337 =( NAMED_UNIT ( * ) PLANE_ANGLE_UNIT ( ) SI_UNIT ( $, .RADIAN. ) );
#33338 = CARTESIAN_POINT ( 'NONE',  ( 0.000000000000000000, -97.00000000000000000, 3.750000000000000000 ) ) ;
#33339 = CARTESIAN_POINT ( 'NONE',  ( 20.20024927138663884, 0.02462294155896342304, 6.181741512439034913 ) ) ;
#33340 = CARTESIAN_POINT ( 'NONE',  ( 12.91533473730992121, 4.522018677488170546, 10.88017736071110164 ) ) ;
#33341 = CARTESIAN_POINT ( 'NONE',  ( 0.1532563361054083140, 16.00893115100078390, 1.131784320476157264E-15 ) ) ;
#33342 = CARTESIAN_POINT ( 'NONE',  ( -0.3689425029237898834, 1.178748834913967869, -10.36894250292378850 ) ) ;
#33343 = CARTESIAN_POINT ( 'NONE',  ( 10.00000000000000178, 7.258931151000785675, 9.846743663894594434 ) ) ;
#33344 = CARTESIAN_POINT ( 'NONE',  ( 10.00000000000000178, 4.313685344154837509, 10.88017736071110342 ) ) ;
#33345 = CARTESIAN_POINT ( 'NONE',  ( 19.84674366389459266, 48.30059781766745175, 2.638427012816836559 ) ) ;
#33346 = ORIENTED_EDGE ( 'NONE', *, *, #36104, .F. ) ;
#33347 = CARTESIAN_POINT ( 'NONE',  ( 19.84674366389459266, 43.30059781766744464, 2.638427012816836559 ) ) ;
#33348 = ORIENTED_EDGE ( 'NONE', *, *, #5334, .T. ) ;
#33349 = DIRECTION ( 'NONE',  ( 1.000000000000000000, 0.000000000000000000, 0.000000000000000000 ) ) ;
#33350 = CARTESIAN_POINT ( 'NONE',  ( 15.44008868035555260, 59.73035201082151247, 9.422509992056143702 ) ) ;
#33351 = CARTESIAN_POINT ( 'NONE',  ( 7.361572987183169658, 44.96726448433412315, -9.846743663894592657 ) ) ;
#33352 = CARTESIAN_POINT ( 'NONE',  ( 20.88017736071110875, 65.77201867748817676, -2.915334737309920765 ) ) ;
#33353 = CARTESIAN_POINT ( 'NONE',  ( 4.559911319644449179, 58.89701867748817676, 9.422509992056141925 ) ) ;
#33354 = CARTESIAN_POINT ( 'NONE',  ( 20.88017736071110519, 10.56368534415483929, 2.639326808657452039E-16 ) ) ;
#33355 = EDGE_CURVE ( 'NONE', #68797, #27569, #94993, .T. ) ;
#33356 = PRESENTATION_LAYER_ASSIGNMENT (  '', '', ( #7839 ) ) ;
#33357 = CARTESIAN_POINT ( 'NONE',  ( 21.09922568453595559, 42.04030133659708213, -6.408140936763230044 ) ) ;
#33358 = DIRECTION ( 'NONE',  ( -0.000000000000000000, -1.000000000000000000, -0.000000000000000000 ) ) ;
#33359 = ORIENTED_EDGE ( 'NONE', *, *, #96875, .T. ) ;
#33360 = CARTESIAN_POINT ( 'NONE',  ( 21.09922568453595559, 32.04030133659708923, -6.408140936763230044 ) ) ;
#33361 = CARTESIAN_POINT ( 'NONE',  ( 2.035157376598822676, 37.43868534415484106, -7.964842623401177768 ) ) ;
#33362 = ORIENTED_EDGE ( 'NONE', *, *, #57470, .F. ) ;
#33363 = DIRECTION ( 'NONE',  ( -1.000000000000000000, 0.000000000000000000, 0.000000000000000000 ) ) ;
#33364 = CARTESIAN_POINT ( 'NONE',  ( 0.1532563361054083140, 11.00893115100078568, 1.131784320476157264E-15 ) ) ;
#33365 = CARTESIAN_POINT ( 'NONE',  ( 0.6178305044545838731, -0.2513653300695798953, 9.382169495545420901 ) ) ;
#33367 = CARTESIAN_POINT ( 'NONE',  ( 12.63842701281683922, 54.55059781766745175, -9.846743663894590881 ) ) ;
#33366 = CARTESIAN_POINT ( 'NONE',  ( 5.076628168052704559, 10.17559781766745175, -8.527530157486179263 ) ) ;
#33368 = CARTESIAN_POINT ( 'NONE',  ( 10.39692778084940272, 14.95037106203290911, -10.46714871971199301 ) ) ;
#33369 = LINE ( 'NONE', #62392, #39493 ) ;
#33370 = CARTESIAN_POINT ( 'NONE',  ( -7.750000000000000000, 80.32179676972448590, 4.250000000000000000 ) ) ;
#33371 = FACE_OUTER_BOUND ( 'NONE', #55861, .T. ) ;
#33372 = CIRCLE ( 'NONE', #22208, 10.90000000000026326 ) ;
#33373 = CARTESIAN_POINT ( 'NONE',  ( 19.84674366389459621, 33.50893115100078745, 7.409399052514197653E-17 ) ) ;
#33374 = FILL_AREA_STYLE_COLOUR ( '', #23414 ) ;
#33376 = ORIENTED_EDGE ( 'NONE', *, *, #48758, .F. ) ;
#33375 = CARTESIAN_POINT ( 'NONE',  ( 18.52753015748618282, 63.92559781766745886, -4.923371831947291888 ) ) ;
#33377 = CARTESIAN_POINT ( 'NONE',  ( 0.5774900079438590739, 7.647018677488171434, -5.440088680355550821 ) ) ;
#33378 = CARTESIAN_POINT ( 'NONE',  ( 3.591859063236761518, 19.95696800326375353, 11.09922568453594849 ) ) ;
#33379 = CARTESIAN_POINT ( 'NONE',  ( 19.84674366389459266, 43.30059781766744464, 2.638427012816836559 ) ) ;
#33380 = CARTESIAN_POINT ( 'NONE',  ( -4.267749253172059554, 0.000000000000000000, -3.394721039305347077 ) ) ;
#33381 = CARTESIAN_POINT ( 'NONE',  ( 17.08211943468705840, 45.13708216824730357, -12.26659068614894466 ) ) ;
#33382 = CARTESIAN_POINT ( 'NONE',  ( 14.92337183194729633, 12.67559781766745353, 8.527530157486181039 ) ) ;
#33383 = ORIENTED_EDGE ( 'NONE', *, *, #94387, .F. ) ;
#33384 = CARTESIAN_POINT ( 'NONE',  ( -1.514341385896341929, -0.03417435944610275333, -15.92432625271835533 ) ) ;
#33385 = CARTESIAN_POINT ( 'NONE',  ( 22.26659068614894466, 38.88708216824731068, 7.082119434687054849 ) ) ;
#33386 = CARTESIAN_POINT ( 'NONE',  ( 1.472469842513823179, 55.59226448433412315, -4.923371831947296329 ) ) ;
#33387 = CARTESIAN_POINT ( 'NONE',  ( -0.8801773607111009756, 8.063685344154837509, 1.068504757029289695E-15 ) ) ;
#33388 = CARTESIAN_POINT ( 'NONE',  ( 20.36894250292379382, 28.67874883491396787, 10.36894250292379205 ) ) ;
#33389 = CARTESIAN_POINT ( 'NONE',  ( 2.917880565312950480, 40.97041550158063217, -12.26659068614894821 ) ) ;
#33390 = SURFACE_STYLE_FILL_AREA ( #2942 ) ;
#33392 = CARTESIAN_POINT ( 'NONE',  ( 5.076628168052703671, 51.84226448433412315, 8.527530157486179263 ) ) ;
#33391 = DIRECTION ( 'NONE',  ( 0.000000000000000000, 0.000000000000000000, 1.000000000000000000 ) ) ;
#33393 = ORIENTED_EDGE ( 'NONE', *, *, #88589, .F. ) ;
#33394 = CARTESIAN_POINT ( 'NONE',  ( 20.88017736071110875, 30.77201867748816966, -2.915334737309920765 ) ) ;
#33395 = DIRECTION ( 'NONE',  ( 1.000000000000000000, 0.000000000000000000, 0.000000000000000000 ) ) ;
#33396 = CARTESIAN_POINT ( 'NONE',  ( 20.00000000000000711, 93.02849646088141355, -5.197973391108903662 ) ) ;
#33397 = DIRECTION ( 'NONE',  ( 0.7808688094430307203, -0.6246950475544238435, 0.000000000000000000 ) ) ;
#33398 = CARTESIAN_POINT ( 'NONE',  ( -5.204170427930421283E-15, 0.5537488349139709776, -14.16423886937410082 ) ) ;
#33399 = CARTESIAN_POINT ( 'NONE',  ( 0.1532563361054082862, 51.21726448433412315, 2.638427012816831674 ) ) ;
#33400 = LINE ( 'NONE', #25927, #30552 ) ;
#33401 = ADVANCED_FACE ( 'NONE', ( #43224 ), #91173, .T. ) ;
#33402 = ORIENTED_EDGE ( 'NONE', *, *, #42395, .T. ) ;
#33403 = CARTESIAN_POINT ( 'NONE',  ( -4.164238869374098151, 26.59541550158063217, -3.795296366450310543 ) ) ;
#33404 = EDGE_CURVE ( 'NONE', #23929, #62689, #20237, .T. ) ;
#33405 = ADVANCED_FACE ( 'NONE', ( #21734 ), #81989, .T. ) ;
#33406 = DIRECTION ( 'NONE',  ( 1.000000000000000000, -0.000000000000000000, -0.000000000000000000 ) ) ;
#33407 = CARTESIAN_POINT ( 'NONE',  ( -3.521809514228322335, -0.8352226969046322447, -2.499999999999393818 ) ) ;
#33408 = CARTESIAN_POINT ( 'NONE',  ( 10.00000000000000178, 68.05374883491397497, 14.16423886937410082 ) ) ;
#33409 = CARTESIAN_POINT ( 'NONE',  ( 16.40814093676324603, 27.45696800326375708, -11.09922568453594671 ) ) ;
#33410 = CYLINDRICAL_SURFACE ( 'NONE', #25728, 8.000000000000000000 ) ;
#33411 = CARTESIAN_POINT ( 'NONE',  ( 14.92337183194729633, 17.67559781766745175, 8.527530157486181039 ) ) ;
#33412 = CARTESIAN_POINT ( 'NONE',  ( 10.39655283154085197, 0.04922511925147234763, -10.46698568711264699 ) ) ;
#33413 = DIRECTION ( 'NONE',  ( 1.000000000000000000, 0.000000000000000000, 0.000000000000000000 ) ) ;
#33414 = FACE_OUTER_BOUND ( 'NONE', #70119, .T. ) ;
#33415 = CARTESIAN_POINT ( 'NONE',  ( 17.96484262340118221, 11.18868534415484106, -7.964842623401177768 ) ) ;
#33416 = CARTESIAN_POINT ( 'NONE',  ( -19.64999999999999858, 92.00000000000000000, 7.750000000000000000 ) ) ;
#33417 = CARTESIAN_POINT ( 'NONE',  ( 20.88017736071110164, 40.35535201082150536, 2.915334737309930979 ) ) ;
#33418 = CARTESIAN_POINT ( 'NONE',  ( 2.035157376598824452, 43.68868534415484106, 7.964842623401179544 ) ) ;
#33419 = CARTESIAN_POINT ( 'NONE',  ( 18.52753015748617571, 63.09226448433412315, 4.923371831947298993 ) ) ;
#33420 = CARTESIAN_POINT ( 'NONE',  ( 14.92337183194729988, 64.34226448433412315, -8.527530157486177487 ) ) ;
#33421 = CARTESIAN_POINT ( 'NONE',  ( -45.65418601736590176, 104.2903935945944056, -5.789884099738774381 ) ) ;
#33422 = CARTESIAN_POINT ( 'NONE',  ( 17.20831665107776587, 4.133931151000785675, -7.208316651077762316 ) ) ;
#33423 = ORIENTED_EDGE ( 'NONE', *, *, #43684, .T. ) ;
#33424 = ADVANCED_FACE ( 'NONE', ( #41184 ), #48129, .F. ) ;
#33425 = CARTESIAN_POINT ( 'NONE',  ( 10.00000000000000178, 24.31368534415484106, 10.88017736071110342 ) ) ;
#33426 = CARTESIAN_POINT ( 'NONE',  ( 22.81628187352647785, 31.41530133659709279, 3.434112377981063169 ) ) ;
#33427 = CARTESIAN_POINT ( 'NONE',  ( 0.000000000000000000, 70.80332830338373640, 5.000000000000000000 ) ) ;
#33428 = CARTESIAN_POINT ( 'NONE',  ( 10.00000000000000000, 64.75893115100078035, -9.846743663894594434 ) ) ;
#33429 = CARTESIAN_POINT ( 'NONE',  ( -0.8801773607111008646, 68.27201867748817676, 2.915334737309923430 ) ) ;
#33430 = CARTESIAN_POINT ( 'NONE',  ( 10.00000000000000000, 9.758931151000785675, -9.846743663894594434 ) ) ;
#33431 = CARTESIAN_POINT ( 'NONE',  ( 16.40814093676324603, 32.45696800326375353, -11.09922568453594671 ) ) ;
#33433 = CARTESIAN_POINT ( 'NONE',  ( -5.803070148808146200, 15.00000000000000000, -13.28812917035395813 ) ) ;
#33432 = CARTESIAN_POINT ( 'NONE',  ( 17.96484262340118221, 61.18868534415482685, -7.964842623401177768 ) ) ;
#33434 = ORIENTED_EDGE ( 'NONE', *, *, #18435, .T. ) ;
#33435 = B_SPLINE_CURVE_WITH_KNOTS ( 'NONE', 3,
 ( #81766, #37777, #36783, #68274, #30241, #36279, #60745, #13278, #91246, #13777, #53251, #43769, #74259, #5788, #59264, #89766, #82261, #44263 ),
 .UNSPECIFIED., .F., .F.,
 ( 4, 2, 2, 2, 2, 2, 2, 2, 4 ),
 ( 0.000000000000000000, 0.001396361802156549344, 0.002792723604313098688, 0.004189085406469648248, 0.005585447208626197375, 0.006981809010782746502, 0.008378170812939296497, 0.009774532615095844756, 0.01117089441725239475 ),
 .UNSPECIFIED. ) ;
#33436 = SURFACE_STYLE_USAGE ( .BOTH. , #39983 ) ;
#33437 = CARTESIAN_POINT ( 'NONE',  ( 20.88017736071110164, 5.355352010821502695, 2.915334737309930979 ) ) ;
#33439 = CARTESIAN_POINT ( 'NONE',  ( 6.204703633549690345, 25.76208216824730712, -14.16423886937410259 ) ) ;
#33438 = CARTESIAN_POINT ( 'NONE',  ( 0.6178305044545838731, 54.74863466993042493, 9.382169495545420901 ) ) ;
#33440 = EDGE_CURVE ( 'NONE', #3959, #36305, #49647, .T. ) ;
#33441 = CARTESIAN_POINT ( 'NONE',  ( 14.92337183194729988, 19.34226448433411960, -8.527530157486177487 ) ) ;
#33442 = AXIS2_PLACEMENT_3D ( 'NONE', #19419, #49911, #95924 ) ;
#33443 = CARTESIAN_POINT ( 'NONE',  ( 7.084665262690076126, 9.105352010821503583, 10.88017736071109987 ) ) ;
#33444 = CARTESIAN_POINT ( 'NONE',  ( 0.1532563361054082862, 16.21726448433411960, 2.638427012816831674 ) ) ;
#33445 = CARTESIAN_POINT ( 'NONE',  ( -0.3689425029237881626, 52.42874883491396076, 10.36894250292379027 ) ) ;
#33446 = ORIENTED_EDGE ( 'NONE', *, *, #75055, .T. ) ;
#33447 = CARTESIAN_POINT ( 'NONE',  ( -0.8801773607110991993, 17.85535201082150536, -2.915334737309923874 ) ) ;
#33448 = AXIS2_PLACEMENT_3D ( 'NONE', #64430, #92969, #48457 ) ;
#33449 = CARTESIAN_POINT ( 'NONE',  ( 12.91533473730992121, 19.52201867748816611, 10.88017736071110164 ) ) ;
#33450 = CARTESIAN_POINT ( 'NONE',  ( 9.399392868737743711, 4.718572659598065102E-16, 11.04089732309480532 ) ) ;
#33451 = ORIENTED_EDGE ( 'NONE', *, *, #80392, .F. ) ;
#33452 = CARTESIAN_POINT ( 'NONE',  ( 21.92686044187657401, 10.37045670184113888, -3.195792623639525765 ) ) ;
#33453 = CARTESIAN_POINT ( 'NONE',  ( 10.00000000000000178, 29.31368534415483751, 10.88017736071110342 ) ) ;
#33454 = CARTESIAN_POINT ( 'NONE',  ( 7.361572987183169658, 54.96726448433413026, -9.846743663894592657 ) ) ;
#33455 = CARTESIAN_POINT ( 'NONE',  ( 0.000000000000000000, 0.000000000000000000, 0.000000000000000000 ) ) ;
#33456 = DIRECTION ( 'NONE',  ( 1.927470528863119295E-16, -1.000000000000000000, 0.000000000000000000 ) ) ;
#33457 = CARTESIAN_POINT ( 'NONE',  ( -0.3689425029237881626, 17.42874883491397142, 10.36894250292379027 ) ) ;
#33458 = CARTESIAN_POINT ( 'NONE',  ( -0.8801773607111008646, 38.27201867748816255, 2.915334737309923430 ) ) ;
#33459 = CARTESIAN_POINT ( 'NONE',  ( 19.42250999205614548, 10.98035201082150536, -5.440088680355545492 ) ) ;
#33460 = CARTESIAN_POINT ( 'NONE',  ( 17.20831665107776587, 54.13393115100079456, -7.208316651077762316 ) ) ;
#33461 = CARTESIAN_POINT ( 'NONE',  ( -11.62814856721715095, -77.87341909757282110, -3.750000000000000000 ) ) ;
#33462 = CARTESIAN_POINT ( 'NONE',  ( 10.00000000000000178, 37.25893115100078745, 9.846743663894594434 ) ) ;
#33463 = CARTESIAN_POINT ( 'NONE',  ( 8.008672916919360803E-16, 22.29452073070357088, 0.000000000000000000 ) ) ;
#33464 = CARTESIAN_POINT ( 'NONE',  ( 1.472469842513823179, 11.42559781766745175, 4.923371831947296329 ) ) ;
#33465 = CARTESIAN_POINT ( 'NONE',  ( -9.382169495545413795, -30.25136533006957507, 9.382169495545428006 ) ) ;
#33466 = ORIENTED_EDGE ( 'NONE', *, *, #78683, .T. ) ;
#33467 = CIRCLE ( 'NONE', #43054, 15.00000000000000000 ) ;
#33468 = CARTESIAN_POINT ( 'NONE',  ( -0.8801773607111008646, 18.27201867748817321, 2.915334737309923430 ) ) ;
#33469 = CARTESIAN_POINT ( 'NONE',  ( 17.20831665107776587, 9.133931151000787452, -7.208316651077762316 ) ) ;
#33470 = CARTESIAN_POINT ( 'NONE',  ( 12.63842701281683922, 64.55059781766745175, -9.846743663894590881 ) ) ;
#33471 = CARTESIAN_POINT ( 'NONE',  ( 15.44008868035555260, 49.73035201082150536, 9.422509992056143702 ) ) ;
#33473 = CARTESIAN_POINT ( 'NONE',  ( -1.099225684535947600, 48.70696800326375353, -6.408140936763238038 ) ) ;
#33472 = CARTESIAN_POINT ( 'NONE',  ( 0.5774900079438590739, 17.64701867748817321, -5.440088680355550821 ) ) ;
#33474 = CARTESIAN_POINT ( 'NONE',  ( 22.26659068614894466, 28.88708216824730357, 7.082119434687054849 ) ) ;
#33475 = DIRECTION ( 'NONE',  ( 0.000000000000000000, 0.000000000000000000, -1.000000000000000000 ) ) ;
#33476 = CIRCLE ( 'NONE', #28702, 0.2500000000000002220 ) ;
#33477 = CARTESIAN_POINT ( 'NONE',  ( 10.00000000000000178, 60.37363466993041783, 12.81628187352647608 ) ) ;
#33478 = ORIENTED_EDGE ( 'NONE', *, *, #59394, .F. ) ;
#33479 = CARTESIAN_POINT ( 'NONE',  ( 5.076628168052704559, 60.17559781766745175, -8.527530157486179263 ) ) ;
#33480 = CARTESIAN_POINT ( 'NONE',  ( 17.96484262340118221, 39.93868534415484106, 7.964842623401181321 ) ) ;
#33481 = VERTEX_POINT ( 'NONE', #41674 ) ;
#33483 = CARTESIAN_POINT ( 'NONE',  ( 14.61146088927471176, 15.00000000000000888, -0.6660010753334455469 ) ) ;
#33482 = CARTESIAN_POINT ( 'NONE',  ( 19.84674366389459266, 3.300597817667451750, 2.638427012816836559 ) ) ;
#33484 = LINE ( 'NONE', #62515, #32438 ) ;
#33485 = CARTESIAN_POINT ( 'NONE',  ( 19.84674366389459266, 8.300597817667451750, 2.638427012816836559 ) ) ;
#33486 = CARTESIAN_POINT ( 'NONE',  ( 7.361572987183170547, 27.05059781766745175, 9.846743663894590881 ) ) ;
#33487 = CARTESIAN_POINT ( 'NONE',  ( 10.00000000000000178, 2.258931151000784787, 9.846743663894594434 ) ) ;
#33488 = CARTESIAN_POINT ( 'NONE',  ( 2.791683348922237240, 5.383931151000785675, -7.208316651077763204 ) ) ;
#33489 = ADVANCED_FACE ( 'NONE', ( #72142 ), #80641, .F. ) ;
#33491 = CARTESIAN_POINT ( 'NONE',  ( -5.204170427930421283E-15, 11.67180217785154817, -11.25000000000000178 ) ) ;
#33490 = CARTESIAN_POINT ( 'NONE',  ( 15.44008868035555793, 56.39701867748817676, -9.422509992056140149 ) ) ;
#33492 = CARTESIAN_POINT ( 'NONE',  ( 4.559911319644449179, 57.23035201082150536, -9.422509992056141925 ) ) ;
#33494 = EDGE_LOOP ( 'NONE', ( #29688, #29561, #84037, #8737 ) ) ;
#33493 = CARTESIAN_POINT ( 'NONE',  ( 19.84674366389459266, 18.71726448433411960, -2.638427012816827677 ) ) ;
#33495 = CARTESIAN_POINT ( 'NONE',  ( 0.5774900079438607392, 63.48035201082149825, 5.440088680355550821 ) ) ;
#33496 = CARTESIAN_POINT ( 'NONE',  ( 5.076628168052703671, 56.84226448433412315, 8.527530157486179263 ) ) ;
#33497 = EDGE_LOOP ( 'NONE', ( #44578, #83017, #64063, #61964, #94948, #56162 ) ) ;
#33498 = EDGE_LOOP ( 'NONE', ( #64956, #21456, #3099, #54519 ) ) ;
#33499 = DIRECTION ( 'NONE',  ( -8.673617379884026597E-16, -1.000000000000000000, 7.806255641895624036E-15 ) ) ;
#33500 = CARTESIAN_POINT ( 'NONE',  ( 6.204703633549690345, 7.845415501580634832, 14.16423886937410082 ) ) ;
#33501 = UNCERTAINTY_MEASURE_WITH_UNIT (LENGTH_MEASURE( 1.000000000000000082E-05 ), #22022, 'distance_accuracy_value', 'NONE');
#33502 = CARTESIAN_POINT ( 'NONE',  ( 13.43411237798105340, 55.58196800326374643, 12.81628187352647963 ) ) ;
#33503 = CARTESIAN_POINT ( 'NONE',  ( 10.00000000000000178, 8.053748834913967869, 14.16423886937410082 ) ) ;
#33504 = CARTESIAN_POINT ( 'NONE',  ( 2.917880565312948704, 27.63708216824730357, 12.26659068614894643 ) ) ;
#33505 = DIRECTION ( 'NONE',  ( 0.000000000000000000, 0.000000000000000000, 1.000000000000000000 ) ) ;
#33506 = CARTESIAN_POINT ( 'NONE',  ( 2.917880565312950480, 5.970415501580634832, -12.26659068614894821 ) ) ;
#33507 = CARTESIAN_POINT ( 'NONE',  ( 10.00000000000000000, 16.81368534415483751, -10.88017736071110342 ) ) ;
#33508 =( NAMED_UNIT ( * ) SI_UNIT ( $, .STERADIAN. ) SOLID_ANGLE_UNIT ( ) );
#33509 = ORIENTED_EDGE ( 'NONE', *, *, #599, .F. ) ;
#33510 = CARTESIAN_POINT ( 'NONE',  ( 12.63842701281683034, 12.46726448433411782, 9.846743663894596210 ) ) ;
#33513 = VECTOR ( 'NONE', #58817, 1000.000000000000000 ) ;
#33512 = CARTESIAN_POINT ( 'NONE',  ( 1.472469842513823179, 15.59226448433411960, -4.923371831947296329 ) ) ;
#33511 = CARTESIAN_POINT ( 'NONE',  ( 12.91533473730993009, 51.60535201082149825, -10.88017736071109987 ) ) ;
#33514 = CARTESIAN_POINT ( 'NONE',  ( 13.43411237798105340, 50.58196800326375353, 12.81628187352647963 ) ) ;
#33515 = CARTESIAN_POINT ( 'NONE',  ( 19.84674366389459266, 33.71726448433410894, -2.638427012816827677 ) ) ;
#33516 = VECTOR ( 'NONE', #5466, 1000.000000000000000 ) ;
#33517 = DIRECTION ( 'NONE',  ( -0.000000000000000000, -0.000000000000000000, -1.000000000000000000 ) ) ;
#33518 = CARTESIAN_POINT ( 'NONE',  ( 10.00000000000000178, 54.31368534415484106, 10.88017736071110342 ) ) ;
#33519 = CARTESIAN_POINT ( 'NONE',  ( 13.43411237798105340, 35.58196800326375353, 12.81628187352647963 ) ) ;
#33520 = CARTESIAN_POINT ( 'NONE',  ( -7.082119434687058401, -39.02958449841936073, -12.26659068614894110 ) ) ;
#33521 = CARTESIAN_POINT ( 'NONE',  ( 7.361572987183169658, 24.96726448433412315, -9.846743663894592657 ) ) ;
#33522 = EDGE_CURVE ( 'NONE', #31275, #95619, #35349, .T. ) ;
#33523 = CARTESIAN_POINT ( 'NONE',  ( 2.917880565312950480, 15.97041550158063217, -12.26659068614894821 ) ) ;
#33524 = ORIENTED_EDGE ( 'NONE', *, *, #13416, .F. ) ;
#33525 = EDGE_CURVE ( 'NONE', #42002, #7455, #64136, .T. ) ;
#33526 = CARTESIAN_POINT ( 'NONE',  ( 20.88017736071110875, 35.77201867748816966, -2.915334737309920765 ) ) ;
#33527 = CARTESIAN_POINT ( 'NONE',  ( -4.164238869374099927, 37.01208216824731068, 3.795296366450308767 ) ) ;
#33528 = CARTESIAN_POINT ( 'NONE',  ( 12.63842701281683034, 52.46726448433413026, 9.846743663894596210 ) ) ;
#33529 = CARTESIAN_POINT ( 'NONE',  ( 12.63842701281683922, 9.550597817667449974, -9.846743663894590881 ) ) ;
#33531 = LINE ( 'NONE', #79042, #25723 ) ;
#33530 = CARTESIAN_POINT ( 'NONE',  ( 16.40814093676323893, 50.79030133659708923, 11.09922568453595026 ) ) ;
#33532 = CARTESIAN_POINT ( 'NONE',  ( 12.91533473730992121, 39.52201867748817676, 10.88017736071110164 ) ) ;
#33533 = CARTESIAN_POINT ( 'NONE',  ( -6.732636091893172470, -88.11213685669366669, -3.750000000000000000 ) ) ;
#33534 = CIRCLE ( 'NONE', #89442, 4.000000000000001776 ) ;
#33535 = CARTESIAN_POINT ( 'NONE',  ( 22.81628187352647785, 26.41530133659708923, 3.434112377981063169 ) ) ;
#33536 = CARTESIAN_POINT ( 'NONE',  ( 1.472469842513823179, 60.59226448433412315, -4.923371831947296329 ) ) ;
#33537 = CARTESIAN_POINT ( 'NONE',  ( -5.204170427930421283E-15, 11.81368534415484817, -10.88017736071110342 ) ) ;
#33538 = SURFACE_STYLE_USAGE ( .BOTH. , #3571 ) ;
#33540 = DIRECTION ( 'NONE',  ( 0.000000000000000000, 1.000000000000000000, 0.000000000000000000 ) ) ;
#33539 = CARTESIAN_POINT ( 'NONE',  ( 4.559911319644449179, 67.23035201082150536, -9.422509992056141925 ) ) ;
#33541 = LINE ( 'NONE', #64035, #84903 ) ;
#33542 = DIRECTION ( 'NONE',  ( 0.2840153447039108769, 0.000000000000000000, 0.9588197348681966048 ) ) ;
#33543 = CARTESIAN_POINT ( 'NONE',  ( 12.91533473730992121, 59.52201867748816966, 10.88017736071110164 ) ) ;
#33544 = CARTESIAN_POINT ( 'NONE',  ( -0.8801773607111009756, 63.06368534415484106, 1.068504757029289695E-15 ) ) ;
#33545 = CARTESIAN_POINT ( 'NONE',  ( -12.60589901313216998, 14.49999999999999112, -8.129656208642240145 ) ) ;
#33546 = DIRECTION ( 'NONE',  ( -0.000000000000000000, 1.000000000000000000, 0.000000000000000000 ) ) ;
#33547 = CARTESIAN_POINT ( 'NONE',  ( 18.52753015748617571, 23.09226448433411960, 4.923371831947298993 ) ) ;
#33548 = CARTESIAN_POINT ( 'NONE',  ( -0.8801773607111008646, 28.27201867748817321, 2.915334737309923430 ) ) ;
#33549 = CARTESIAN_POINT ( 'NONE',  ( 6.565887622018943937, -1.918031996736246692, -12.81628187352647608 ) ) ;
#33551 = CARTESIAN_POINT ( 'NONE',  ( -0.1503990784575277573, 33.10158574516643171, 6.262539305110076171 ) ) ;
#33550 = CARTESIAN_POINT ( 'NONE',  ( -0.8801773607111008646, 28.27201867748817321, 2.915334737309923430 ) ) ;
#33552 = CARTESIAN_POINT ( 'NONE',  ( 19.38216949554541557, 22.24863466993041428, -9.382169495545420901 ) ) ;
#33553 = ORIENTED_EDGE ( 'NONE', *, *, #41019, .T. ) ;
#33554 = CARTESIAN_POINT ( 'NONE',  ( 20.88017736071110164, 50.35535201082151247, 2.915334737309930979 ) ) ;
#33555 = CARTESIAN_POINT ( 'NONE',  ( 1.472469842513823179, 46.42559781766745175, 4.923371831947296329 ) ) ;
#33557 =( LENGTH_UNIT ( ) NAMED_UNIT ( * ) SI_UNIT ( .MILLI., .METRE. ) );
#33556 = CARTESIAN_POINT ( 'NONE',  ( 16.40814093676323893, 25.79030133659708923, 11.09922568453595026 ) ) ;
#33558 = ADVANCED_FACE ( 'NONE', ( #89617, #37124, #51628, #66115 ), #96644, .F. ) ;
#33559 = CARTESIAN_POINT ( 'NONE',  ( 2.035157376598822676, 22.43868534415483396, -7.964842623401177768 ) ) ;
#33560 = CARTESIAN_POINT ( 'NONE',  ( 22.26659068614895176, 44.72041550158063927, -7.082119434687042414 ) ) ;
#33561 = CARTESIAN_POINT ( 'NONE',  ( 5.076628168052704559, 40.17559781766745175, -8.527530157486179263 ) ) ;
#33562 = CARTESIAN_POINT ( 'NONE',  ( 7.361572987183169658, 9.967264484334119601, -9.846743663894592657 ) ) ;
#33563 = CARTESIAN_POINT ( 'NONE',  ( 20.88017736071110519, 50.56368534415484106, 2.639326808657452039E-16 ) ) ;
#33564 = DIRECTION ( 'NONE',  ( 0.000000000000000000, 0.000000000000000000, 1.000000000000000000 ) ) ;
#33565 = CARTESIAN_POINT ( 'NONE',  ( 6.204703633549690345, 17.84541550158063217, 14.16423886937410082 ) ) ;
#33566 = DIRECTION ( 'NONE',  ( -1.257402221000611116E-16, 1.000000000000000000, 0.000000000000000000 ) ) ;
#33567 = CARTESIAN_POINT ( 'NONE',  ( 2.377183314879970588, 20.78593319516822646, -6.499999999999988454 ) ) ;
#33568 = STYLED_ITEM ( 'NONE', ( #774 ), #66500 ) ;
#33569 = ORIENTED_EDGE ( 'NONE', *, *, #7958, .F. ) ;
#33570 = VERTEX_POINT ( 'NONE', #75602 ) ;
#33571 = CARTESIAN_POINT ( 'NONE',  ( 2.917880565312950480, 45.97041550158063927, -12.26659068614894821 ) ) ;
#33572 = CARTESIAN_POINT ( 'NONE',  ( 22.26659068614895176, 54.72041550158063217, -7.082119434687042414 ) ) ;
#33573 = CARTESIAN_POINT ( 'NONE',  ( 18.52753015748617571, 13.09226448433411960, 4.923371831947298993 ) ) ;
#33574 = CARTESIAN_POINT ( 'NONE',  ( 0.6178305044545838731, 14.74863466993041783, 9.382169495545420901 ) ) ;
#33575 = DIRECTION ( 'NONE',  ( -0.000000000000000000, -1.000000000000000000, -0.000000000000000000 ) ) ;
#33576 = CARTESIAN_POINT ( 'NONE',  ( 19.80427997160309417, 52.75733960839545489, -6.499999999999988454 ) ) ;
#33578 = CARTESIAN_POINT ( 'NONE',  ( 6.565887622018943937, 35.16530133659708923, 12.81628187352647430 ) ) ;
#33577 = CARTESIAN_POINT ( 'NONE',  ( 15.44008868035555260, 4.730352010821504471, 9.422509992056143702 ) ) ;
#33579 = CARTESIAN_POINT ( 'NONE',  ( 13.79529636645031943, 45.34541550158062506, -14.16423886937409904 ) ) ;
#33580 = SURFACE_STYLE_FILL_AREA ( #26582 ) ;
#33581 = SURFACE_STYLE_USAGE ( .BOTH. , #3123 ) ;
#33582 = CARTESIAN_POINT ( 'NONE',  ( 4.923371831947295441, 9.342264484334124930, -8.527530157486179263 ) ) ;
#33583 = ORIENTED_EDGE ( 'NONE', *, *, #40774, .F. ) ;
#33584 = DIRECTION ( 'NONE',  ( 1.000000000000000000, 0.000000000000000000, 0.000000000000000000 ) ) ;
#33585 = CARTESIAN_POINT ( 'NONE',  ( 12.63842701281683034, 22.46726448433411605, 9.846743663894596210 ) ) ;
#33586 = DIRECTION ( 'NONE',  ( 0.000000000000000000, 0.000000000000000000, -1.000000000000000000 ) ) ;
#33587 = VECTOR ( 'NONE', #19721, 1000.000000000000000 ) ;
#33588 = ORIENTED_EDGE ( 'NONE', *, *, #57686, .F. ) ;
#33590 = CARTESIAN_POINT ( 'NONE',  ( 20.88017736071110875, 15.77201867748817143, -2.915334737309920765 ) ) ;
#33589 = CARTESIAN_POINT ( 'NONE',  ( 0.5774900079438590739, 12.64701867748817321, -5.440088680355550821 ) ) ;
#33592 = CARTESIAN_POINT ( 'NONE',  ( 19.38216949554541557, 7.248634669930421381, -9.382169495545420901 ) ) ;
#33591 = CARTESIAN_POINT ( 'NONE',  ( 0.1532563361054082862, 56.21726448433411605, 2.638427012816831674 ) ) ;
#33593 = SURFACE_STYLE_FILL_AREA ( #3618 ) ;
#33594 = DIRECTION ( 'NONE',  ( -1.000000000000000000, 0.000000000000000000, 0.000000000000000000 ) ) ;
#33595 = CARTESIAN_POINT ( 'NONE',  ( 22.81628187352648496, 21.83196800326374643, -3.434112377981050290 ) ) ;
#33596 = ORIENTED_EDGE ( 'NONE', *, *, #33404, .F. ) ;
#33597 = CARTESIAN_POINT ( 'NONE',  ( 17.08211943468705840, 60.13708216824729647, -12.26659068614894466 ) ) ;
#33598 = B_SPLINE_CURVE_WITH_KNOTS ( 'NONE', 3,
 ( #38710, #15729, #75216, #30201, #61682, #22729 ),
 .UNSPECIFIED., .F., .F.,
 ( 4, 2, 4 ),
 ( 3.409110551496108329E-05, 0.0004400426677367840237, 0.0008459942299586070387 ),
 .UNSPECIFIED. ) ;
#33599 = ORIENTED_EDGE ( 'NONE', *, *, #30772, .F. ) ;
#33600 = CARTESIAN_POINT ( 'NONE',  ( 10.00000000000000178, 53.05374883491396787, 14.16423886937410082 ) ) ;
#33601 = EDGE_LOOP ( 'NONE', ( #3125, #23701, #8992, #75660 ) ) ;
#33602 = CARTESIAN_POINT ( 'NONE',  ( 10.00000000000000000, 31.81368534415483751, -10.88017736071110342 ) ) ;
#33603 = AXIS2_PLACEMENT_3D ( 'NONE', #5150, #88632, #48664 ) ;
#33604 = CARTESIAN_POINT ( 'NONE',  ( 0.5774900079438590739, 32.64701867748816966, -5.440088680355550821 ) ) ;
#33605 = CARTESIAN_POINT ( 'NONE',  ( 2.035157376598822676, 67.43868534415484817, -7.964842623401177768 ) ) ;
#33606 = CARTESIAN_POINT ( 'NONE',  ( 17.96484262340118221, 21.18868534415483396, -7.964842623401177768 ) ) ;
#33607 = AXIS2_PLACEMENT_3D ( 'NONE', #93059, #61087, #77076 ) ;
#33608 = EDGE_CURVE ( 'NONE', #65098, #82021, #37618, .T. ) ;
#33609 = B_SPLINE_CURVE_WITH_KNOTS ( 'NONE', 3,
 ( #438, #61385, #76399, #9377, #23906, #84406 ),
 .UNSPECIFIED., .F., .F.,
 ( 4, 2, 4 ),
 ( 0.0002800630492131323673, 0.0006862688956284098384, 0.001092474742043687309 ),
 .UNSPECIFIED. ) ;
#33610 = FACE_OUTER_BOUND ( 'NONE', #16561, .T. ) ;
#33611 = CARTESIAN_POINT ( 'NONE',  ( 17.20831665107776587, 9.133931151000787452, -7.208316651077762316 ) ) ;
#33612 = CARTESIAN_POINT ( 'NONE',  ( -5.559677335904731343, -36.09286816789840202, 2.500000000000000888 ) ) ;
#33613 = ORIENTED_EDGE ( 'NONE', *, *, #83129, .T. ) ;
#33614 = CARTESIAN_POINT ( 'NONE',  ( 11.44533298129242738, -77.48611261198139744, 3.750000000000000000 ) ) ;
#33615 = CARTESIAN_POINT ( 'NONE',  ( 19.84674366389459621, 48.50893115100078745, 7.409399052514197653E-17 ) ) ;
#33616 = LINE ( 'NONE', #87120, #70787 ) ;
#33617 = CARTESIAN_POINT ( 'NONE',  ( 4.219999999999999751, 36.75000000000000000, 2.500000000000000000 ) ) ;
#33618 = CARTESIAN_POINT ( 'NONE',  ( -3.750000000000000000, 10.25000000000000000, 2.750000000000000000 ) ) ;
#33619 = CARTESIAN_POINT ( 'NONE',  ( 14.92337183194729633, 62.67559781766745886, 8.527530157486181039 ) ) ;
#33620 = CARTESIAN_POINT ( 'NONE',  ( -0.3689425029237898834, 41.17874883491397497, -10.36894250292378850 ) ) ;
#33621 = CARTESIAN_POINT ( 'NONE',  ( 11.34661744925197624, 54.08985607419764818, 0.000000000000000000 ) ) ;
#33622 = ORIENTED_EDGE ( 'NONE', *, *, #90191, .F. ) ;
#33623 = DIRECTION ( 'NONE',  ( -0.000000000000000000, 0.000000000000000000, 1.000000000000000000 ) ) ;
#33624 = CARTESIAN_POINT ( 'NONE',  ( 19.84674366389459621, 33.50893115100078745, 7.409399052514197653E-17 ) ) ;
#33625 = VECTOR ( 'NONE', #87248, 1000.000000000000000 ) ;
#33626 = CARTESIAN_POINT ( 'NONE',  ( 10.00000000000000178, 5.373634669930420493, 12.81628187352647608 ) ) ;
#33627 = CARTESIAN_POINT ( 'NONE',  ( 0.5774900079438607392, 68.48035201082150536, 5.440088680355550821 ) ) ;
#33628 = CARTESIAN_POINT ( 'NONE',  ( -10.64017930668192058, 14.63595249122789177, -10.57291749337230868 ) ) ;
#33629 = CARTESIAN_POINT ( 'NONE',  ( 18.52753015748617571, 58.09226448433411605, 4.923371831947298993 ) ) ;
#33630 = CARTESIAN_POINT ( 'NONE',  ( 14.29730467489533652, 15.00000000000000000, -2.416004766803220072 ) ) ;
#33631 = PRESENTATION_LAYER_ASSIGNMENT (  '', '', ( #8116 ) ) ;
#33632 = EDGE_CURVE ( 'NONE', #48866, #32363, #19276, .T. ) ;
#33633 = B_SPLINE_CURVE_WITH_KNOTS ( 'NONE', 3,
 ( #94657, #32173, #64140, #25207 ),
 .UNSPECIFIED., .F., .F.,
 ( 4, 4 ),
 ( 2.521264072383755851E-16, 0.002392975128318428242 ),
 .UNSPECIFIED. ) ;
#33634 = ORIENTED_EDGE ( 'NONE', *, *, #18349, .T. ) ;
#33635 = ADVANCED_FACE ( 'NONE', ( #58113 ), #66622, .F. ) ;
#33636 = CARTESIAN_POINT ( 'NONE',  ( 22.26659068614895176, 59.72041550158063927, -7.082119434687042414 ) ) ;
#33637 = CARTESIAN_POINT ( 'NONE',  ( 2.035157376598824452, 43.68868534415484106, 7.964842623401179544 ) ) ;
#33638 = VECTOR ( 'NONE', #39363, 1000.000000000000114 ) ;
#33640 = CARTESIAN_POINT ( 'NONE',  ( 3.840373378095567336, 13.17686044187654559, -11.29165764256138260 ) ) ;
#33639 = CARTESIAN_POINT ( 'NONE',  ( -2.816281873526473856, 19.33196800326375708, 3.434112377981055619 ) ) ;
#33641 = PLANE ( 'NONE',  #29675 ) ;
#33643 = CIRCLE ( 'NONE', #94334, 0.2499999999999973910 ) ;
#33642 = CYLINDRICAL_SURFACE ( 'NONE', #13388, 0.2500000000000002220 ) ;
#33644 = CARTESIAN_POINT ( 'NONE',  ( 0.1077916266722764582, 62.24062864464239908, -6.478736007406002528 ) ) ;
#33645 = CARTESIAN_POINT ( 'NONE',  ( 1.472469842513823179, 51.42559781766745886, 4.923371831947296329 ) ) ;
#33646 = FILL_AREA_STYLE ('',( #9199 ) ) ;
#33647 = CARTESIAN_POINT ( 'NONE',  ( -14.16423886937410082, 26.80374883491398919, 4.336808689942017736E-15 ) ) ;
#33648 = CARTESIAN_POINT ( 'NONE',  ( 16.40814093676324603, 2.456968003263753531, -11.09922568453594671 ) ) ;
#33649 = CARTESIAN_POINT ( 'NONE',  ( -8.957305892888854260, -19.72688805319553751, -4.000000000000000000 ) ) ;
#33651 = DIRECTION ( 'NONE',  ( 1.000000000000000000, 0.000000000000000000, 0.000000000000000000 ) ) ;
#33650 = CARTESIAN_POINT ( 'NONE',  ( 0.5774900079438607392, 28.48035201082150891, 5.440088680355550821 ) ) ;
#33652 = DIRECTION ( 'NONE',  ( 0.000000000000000000, 0.000000000000000000, -1.000000000000000000 ) ) ;
#33653 = CARTESIAN_POINT ( 'NONE',  ( 17.08211943468705840, 40.13708216824731068, -12.26659068614894466 ) ) ;
#33654 = CARTESIAN_POINT ( 'NONE',  ( 20.36894250292379382, 23.67874883491397142, 10.36894250292379205 ) ) ;
#33655 = CARTESIAN_POINT ( 'NONE',  ( 4.559911319644449179, 12.23035201082150714, -9.422509992056141925 ) ) ;
#33656 = CARTESIAN_POINT ( 'NONE',  ( 18.52753015748618282, 38.92559781766745175, -4.923371831947291888 ) ) ;
#33657 = CARTESIAN_POINT ( 'NONE',  ( 13.43411237798106583, 37.66530133659708923, -12.81628187352647252 ) ) ;
#33658 = CARTESIAN_POINT ( 'NONE',  ( 20.88017736071110875, 15.77201867748817143, -2.915334737309920765 ) ) ;
#33659 = CARTESIAN_POINT ( 'NONE',  ( 1.472469842513823179, 41.42559781766745886, 4.923371831947296329 ) ) ;
#33660 = CARTESIAN_POINT ( 'NONE',  ( 10.00000000000000000, 36.81368534415484106, -10.88017736071110342 ) ) ;
#33661 = CARTESIAN_POINT ( 'NONE',  ( -1.099225684535947600, 8.706968003263753531, -6.408140936763238038 ) ) ;
#33663 = CARTESIAN_POINT ( 'NONE',  ( 1.472469842513823179, 60.59226448433412315, -4.923371831947296329 ) ) ;
#33662 = CARTESIAN_POINT ( 'NONE',  ( 22.26659068614894466, 23.88708216824730357, 7.082119434687054849 ) ) ;
#33664 = LINE ( 'NONE', #64160, #35971 ) ;
#33665 = CARTESIAN_POINT ( 'NONE',  ( 7.361572987183170547, 22.05059781766745530, 9.846743663894590881 ) ) ;
#33666 = CARTESIAN_POINT ( 'NONE',  ( 22.81628187352648496, 46.83196800326376064, -3.434112377981050290 ) ) ;
#33667 = CARTESIAN_POINT ( 'NONE',  ( 1.472469842513823179, 60.59226448433412315, -4.923371831947296329 ) ) ;
#33668 = EDGE_LOOP ( 'NONE', ( #47264, #76003, #31252, #75178, #72537, #45835 ) ) ;
#33669 = CARTESIAN_POINT ( 'NONE',  ( 20.15039907845753220, 60.60158574516643881, -6.262539305110077947 ) ) ;
#33670 = CARTESIAN_POINT ( 'NONE',  ( 4.380000000000000782, -0.01592157648205478476, 3.750000000000001776 ) ) ;
#33671 = CARTESIAN_POINT ( 'NONE',  ( -0.3689425029237881626, 67.42874883491396076, 10.36894250292379027 ) ) ;
#33672 = CARTESIAN_POINT ( 'NONE',  ( 2.917880565312950480, 10.97041550158063572, -12.26659068614894821 ) ) ;
#33673 = CARTESIAN_POINT ( 'NONE',  ( 7.361572987183170547, 2.050597817667451750, 9.846743663894590881 ) ) ;
#33674 = CARTESIAN_POINT ( 'NONE',  ( 0.1532563361054083140, 46.00893115100079456, 1.131784320476157264E-15 ) ) ;
#33675 = CARTESIAN_POINT ( 'NONE',  ( 12.91533473730992121, 24.52201867748816966, 10.88017736071110164 ) ) ;
#33676 = CARTESIAN_POINT ( 'NONE',  ( 14.03351048042395632, 15.00000000000000000, 2.474486531753810059 ) ) ;
#33677 = CARTESIAN_POINT ( 'NONE',  ( 0.1532563361054082862, 66.21726448433413736, 2.638427012816831674 ) ) ;
#33678 = AXIS2_PLACEMENT_3D ( 'NONE', #31323, #92816, #47804 ) ;
#33679 = ORIENTED_EDGE ( 'NONE', *, *, #17005, .F. ) ;
#33680 = CARTESIAN_POINT ( 'NONE',  ( 1.457314710996591600, 0.000000000000000000, -5.254907083456943795 ) ) ;
#33681 = VERTEX_POINT ( 'NONE', #97639 ) ;
#33682 = ORIENTED_EDGE ( 'NONE', *, *, #90448, .F. ) ;
#33683 = VECTOR ( 'NONE', #21509, 1000.000000000000000 ) ;
#33684 = DIRECTION ( 'NONE',  ( 0.000000000000000000, -1.000000000000000000, -0.000000000000000000 ) ) ;
#33685 = CARTESIAN_POINT ( 'NONE',  ( 13.79529636645030344, 8.262082168247300018, 14.16423886937410614 ) ) ;
#33686 = CARTESIAN_POINT ( 'NONE',  ( 10.00000000000000000, 45.55374883491397497, -14.16423886937410082 ) ) ;
#33687 = CARTESIAN_POINT ( 'NONE',  ( 10.00000000000000000, 59.75893115100078745, -9.846743663894594434 ) ) ;
#33688 = CARTESIAN_POINT ( 'NONE',  ( 5.076628168052704559, 40.17559781766745175, -8.527530157486179263 ) ) ;
#33689 = CARTESIAN_POINT ( 'NONE',  ( -0.03932841506541377707, 38.12161441960502373, 6.397827110479010315 ) ) ;
#33691 = CARTESIAN_POINT ( 'NONE',  ( 17.20831665107776587, 62.88393115100078745, 7.208316651077764980 ) ) ;
#33690 = CARTESIAN_POINT ( 'NONE',  ( 19.42250999205614548, 30.98035201082150536, -5.440088680355545492 ) ) ;
#33692 = SURFACE_SIDE_STYLE ('',( #64190 ) ) ;
#33693 = CARTESIAN_POINT ( 'NONE',  ( 22.26659068614894466, 43.88708216824729647, 7.082119434687054849 ) ) ;
#33694 = CARTESIAN_POINT ( 'NONE',  ( 10.00000000000000000, 11.81368534415483751, -10.88017736071110342 ) ) ;
#33695 = DIRECTION ( 'NONE',  ( -0.000000000000000000, -1.000000000000000000, -0.000000000000000000 ) ) ;
#33696 = CARTESIAN_POINT ( 'NONE',  ( 0.7375392941518260637, 14.63595249122790065, -14.98185688723471287 ) ) ;
#33697 = CARTESIAN_POINT ( 'NONE',  ( -0.8801773607110991993, 62.85535201082150536, -2.915334737309923874 ) ) ;
#33698 = CARTESIAN_POINT ( 'NONE',  ( 5.076628168052704559, 30.17559781766745175, -8.527530157486179263 ) ) ;
#33699 = CARTESIAN_POINT ( 'NONE',  ( -7.366168427725257040, -80.69295184796105502, 4.000000000000000000 ) ) ;
#33700 = ORIENTED_EDGE ( 'NONE', *, *, #48004, .F. ) ;
#33701 = CARTESIAN_POINT ( 'NONE',  ( -7.750000000000000000, 79.82179676972448590, -6.250000000000000000 ) ) ;
#33702 = EDGE_LOOP ( 'NONE', ( #81537, #3598, #24014 ) ) ;
#33703 = COLOUR_RGB ( '', 0.08235294, 0.09019608, 0.10196078) ;
#33704 = CARTESIAN_POINT ( 'NONE',  ( 7.361572987183170547, 22.05059781766745530, 9.846743663894590881 ) ) ;
#33705 = VERTEX_POINT ( 'NONE', #97149 ) ;
#33706 = CARTESIAN_POINT ( 'NONE',  ( -0.3689425029237881626, 32.42874883491395366, 10.36894250292379027 ) ) ;
#33707 = CARTESIAN_POINT ( 'NONE',  ( 19.84674366389459266, 28.71726448433411960, -2.638427012816827677 ) ) ;
#33708 = CARTESIAN_POINT ( 'NONE',  ( -0.8801773607110991993, 52.85535201082151247, -2.915334737309923874 ) ) ;
#33709 = DIRECTION ( 'NONE',  ( -0.000000000000000000, -1.000000000000000000, -0.000000000000000000 ) ) ;
#33710 = TOROIDAL_SURFACE ( 'NONE', #19381, 6.599999999999995204, 0.2500000000000000000 ) ;
#33711 = CARTESIAN_POINT ( 'NONE',  ( 15.44008868035555793, 36.39701867748816966, -9.422509992056140149 ) ) ;
#33712 = CARTESIAN_POINT ( 'NONE',  ( 0.1532563361054100626, 50.80059781766745175, -2.638427012816831230 ) ) ;
#33713 = CARTESIAN_POINT ( 'NONE',  ( 11.09922568453595026, -3.793031996736244249, 6.408140936763232709 ) ) ;
#33714 = ORIENTED_EDGE ( 'NONE', *, *, #28997, .F. ) ;
#33715 =( GEOMETRIC_REPRESENTATION_CONTEXT ( 3 ) GLOBAL_UNCERTAINTY_ASSIGNED_CONTEXT ( ( #98417 ) ) GLOBAL_UNIT_ASSIGNED_CONTEXT ( ( #12541, #65026, #64538 ) ) REPRESENTATION_CONTEXT ( 'NONE', 'WORKASPACE' ) );
#33716 = CARTESIAN_POINT ( 'NONE',  ( 13.79529636645030344, 3.262082168247301350, 14.16423886937410614 ) ) ;
#33717 = ORIENTED_EDGE ( 'NONE', *, *, #9261, .T. ) ;
#33718 = CARTESIAN_POINT ( 'NONE',  ( -2.816281873526473856, 34.33196800326376064, 3.434112377981055619 ) ) ;
#33719 = CARTESIAN_POINT ( 'NONE',  ( -0.3689425029237898834, 1.178748834913967869, -10.36894250292378850 ) ) ;
#33720 = CARTESIAN_POINT ( 'NONE',  ( 10.00000000000000178, 27.25893115100078390, 9.846743663894594434 ) ) ;
#33721 = FILL_AREA_STYLE_COLOUR ( '', #27514 ) ;
#33722 = DIRECTION ( 'NONE',  ( -0.000000000000000000, -1.000000000000000000, -0.000000000000000000 ) ) ;
#33723 = CARTESIAN_POINT ( 'NONE',  ( 0.1532563361054083140, 31.00893115100078390, 1.131784320476157264E-15 ) ) ;
#33724 = ADVANCED_FACE ( 'NONE', ( #52115 ), #79946, .T. ) ;
#33725 = CARTESIAN_POINT ( 'NONE',  ( 12.91533473730993009, 61.60535201082150536, -10.88017736071109987 ) ) ;
#33726 = CARTESIAN_POINT ( 'NONE',  ( 14.71525861348291286, 14.63595249122789177, -2.908807992686589294 ) ) ;
#33727 = CARTESIAN_POINT ( 'NONE',  ( -0.8801773607110991993, 67.85535201082151957, -2.915334737309923874 ) ) ;
#33728 = CARTESIAN_POINT ( 'NONE',  ( 19.39235739573469175, 29.87576471608601381, 6.499999999999992895 ) ) ;
#33729 = DIRECTION ( 'NONE',  ( -0.000000000000000000, -1.000000000000000000, -0.000000000000000000 ) ) ;
#33730 = CARTESIAN_POINT ( 'NONE',  ( 7.361572987183169658, -0.03273551566588185635, -9.846743663894592657 ) ) ;
#33731 = CARTESIAN_POINT ( 'NONE',  ( 13.43411237798105340, 10.58196800326375353, 12.81628187352647963 ) ) ;
#33732 = CARTESIAN_POINT ( 'NONE',  ( 14.92337183194729633, 42.67559781766745886, 8.527530157486181039 ) ) ;
#33733 = CARTESIAN_POINT ( 'NONE',  ( -6.767445849361073407, 14.49999999999999112, -13.38662304974512729 ) ) ;
#33734 = CARTESIAN_POINT ( 'NONE',  ( 20.36894250292379738, 4.928748834913967869, -10.36894250292379027 ) ) ;
#33735 = CARTESIAN_POINT ( 'NONE',  ( 0.1532563361054100626, 30.80059781766744820, -2.638427012816831230 ) ) ;
#33736 = CARTESIAN_POINT ( 'NONE',  ( 10.00000000000000178, 35.37363466993042493, 12.81628187352647608 ) ) ;
#33737 = CARTESIAN_POINT ( 'NONE',  ( -14.89999999999998970, 98.50000000000000000, -8.000000000000000000 ) ) ;
#33738 = CARTESIAN_POINT ( 'NONE',  ( 7.084665262690076126, 64.10535201082150536, 10.88017736071109987 ) ) ;
#33739 = CARTESIAN_POINT ( 'NONE',  ( 10.00000000000000178, 0.3736346699304200492, 12.81628187352647608 ) ) ;
#33740 = CIRCLE ( 'NONE', #52892, 0.5000000000000004441 ) ;
#33741 = CARTESIAN_POINT ( 'NONE',  ( 9.399392868737814766, 4.153235915537064750E-16, -11.04089732309474314 ) ) ;
#33742 = CARTESIAN_POINT ( 'NONE',  ( 1.472469842513823179, 21.42559781766745175, 4.923371831947296329 ) ) ;
#33743 = CARTESIAN_POINT ( 'NONE',  ( -0.8801773607111009756, 28.06368534415484106, 1.068504757029289695E-15 ) ) ;
#33744 = CARTESIAN_POINT ( 'NONE',  ( 6.565887622018943937, 28.08196800326375353, -12.81628187352647608 ) ) ;
#33745 = CARTESIAN_POINT ( 'NONE',  ( 18.52753015748618282, 23.92559781766745530, -4.923371831947291888 ) ) ;
#33746 = DIRECTION ( 'NONE',  ( -1.000000000000000000, -0.000000000000000000, -0.000000000000000000 ) ) ;
#33747 = VECTOR ( 'NONE', #46844, 1000.000000000000000 ) ;
#33748 = ADVANCED_FACE ( 'NONE', ( #29104 ), #96905, .T. ) ;
#33749 = CARTESIAN_POINT ( 'NONE',  ( 19.42250999205614548, 30.98035201082150536, -5.440088680355545492 ) ) ;
#33750 = ORIENTED_EDGE ( 'NONE', *, *, #30483, .T. ) ;
#33751 = CARTESIAN_POINT ( 'NONE',  ( -0.8801773607111009756, 63.06368534415484106, 1.068504757029289695E-15 ) ) ;
#33752 = CARTESIAN_POINT ( 'NONE',  ( 7.084665262690076126, 7.022018677488169658, -10.88017736071110164 ) ) ;
#33754 = CARTESIAN_POINT ( 'NONE',  ( 20.88017736071110519, 25.56368534415483751, 2.639326808657452039E-16 ) ) ;
#33753 = CARTESIAN_POINT ( 'NONE',  ( 7.361572987183169658, 44.96726448433412315, -9.846743663894592657 ) ) ;
#33755 = CARTESIAN_POINT ( 'NONE',  ( 17.96484262340118221, 46.18868534415484106, -7.964842623401177768 ) ) ;
#33757 =( LENGTH_UNIT ( ) NAMED_UNIT ( * ) SI_UNIT ( .MILLI., .METRE. ) );
#33756 = CARTESIAN_POINT ( 'NONE',  ( 20.88017736071110875, 15.77201867748817143, -2.915334737309920765 ) ) ;
#33758 = DIRECTION ( 'NONE',  ( 0.6246950475544238435, 0.7808688094430307203, 0.000000000000000000 ) ) ;
#33759 = CARTESIAN_POINT ( 'NONE',  ( 14.92337183194729988, 39.34226448433412315, -8.527530157486177487 ) ) ;
#33760 = CARTESIAN_POINT ( 'NONE',  ( 6.204703633549690345, 55.76208216824730357, -14.16423886937410259 ) ) ;
#33761 = CARTESIAN_POINT ( 'NONE',  ( -0.2850016562179802371, 14.76967010231060762, -14.93805486374025193 ) ) ;
#33762 = CARTESIAN_POINT ( 'NONE',  ( 10.00000000000000000, 20.55374883491396787, -14.16423886937410082 ) ) ;
#33763 = CARTESIAN_POINT ( 'NONE',  ( -5.069238524696924486, -24.95996629666330335, 2.750000000000002220 ) ) ;
#33764 = ORIENTED_EDGE ( 'NONE', *, *, #78386, .T. ) ;
#33765 = CARTESIAN_POINT ( 'NONE',  ( 22.26659068614894466, 63.88708216824730357, 7.082119434687054849 ) ) ;
#33766 = CARTESIAN_POINT ( 'NONE',  ( 2.791683348922240793, 36.63393115100078035, 7.208316651077764092 ) ) ;
#33768 = SURFACE_STYLE_USAGE ( .BOTH. , #49287 ) ;
#33767 = CARTESIAN_POINT ( 'NONE',  ( -13.48086198287156101, -0.03417435944610275333, -8.610676897597642210 ) ) ;
#33769 = CARTESIAN_POINT ( 'NONE',  ( 2.035157376598824452, 53.68868534415484817, 7.964842623401179544 ) ) ;
#33770 = CARTESIAN_POINT ( 'NONE',  ( 6.565887622018943937, 63.08196800326376064, -12.81628187352647608 ) ) ;
#33771 = CARTESIAN_POINT ( 'NONE',  ( 4.559911319644449179, 37.23035201082150536, -9.422509992056141925 ) ) ;
#33772 = CARTESIAN_POINT ( 'NONE',  ( 11.22915323889574601, -0.03417435944610275333, 8.773176023390684364 ) ) ;
#33773 = CARTESIAN_POINT ( 'NONE',  ( 21.09922568453594849, 6.206968003263753531, 6.408140936763242479 ) ) ;
#33774 = CARTESIAN_POINT ( 'NONE',  ( 1.472469842513823179, 16.42559781766745175, 4.923371831947296329 ) ) ;
#33775 = ORIENTED_EDGE ( 'NONE', *, *, #3643, .T. ) ;
#33776 = CARTESIAN_POINT ( 'NONE',  ( -4.000000000000000000, 36.75000000000000000, -2.750000000000000000 ) ) ;
#33777 = CARTESIAN_POINT ( 'NONE',  ( 10.58981376305282041, 15.00000000000000000, 9.535111140613782510 ) ) ;
#33778 = CARTESIAN_POINT ( 'NONE',  ( 12.91533473730993009, 6.605352010821504471, -10.88017736071109987 ) ) ;
#33779 = CARTESIAN_POINT ( 'NONE',  ( 17.08211943468705840, 25.13708216824730357, -12.26659068614894466 ) ) ;
#33780 = CARTESIAN_POINT ( 'NONE',  ( 7.084665262690076126, 27.02201867748817676, -10.88017736071110164 ) ) ;
#33781 = CARTESIAN_POINT ( 'NONE',  ( 10.00000000000000000, 46.81368534415484106, -10.88017736071110342 ) ) ;
#33782 = FACE_BOUND ( 'NONE', #74144, .T. ) ;
#33783 = EDGE_CURVE ( 'NONE', #325, #98695, #57597, .T. ) ;
#33784 = CARTESIAN_POINT ( 'NONE',  ( -3.750000000000000000, 36.75000000000000000, -2.500000000000000000 ) ) ;
#33785 = CARTESIAN_POINT ( 'NONE',  ( 7.361572987183169658, 14.96726448433411960, -9.846743663894592657 ) ) ;
#33786 = CARTESIAN_POINT ( 'NONE',  ( -14.22901244993688152, 6.166399856011304496E-16, 3.387263120971218289 ) ) ;
#33787 = CARTESIAN_POINT ( 'NONE',  ( 12.63842701281683922, 14.55059781766744997, -9.846743663894590881 ) ) ;
#33788 = FACE_OUTER_BOUND ( 'NONE', #86240, .T. ) ;
#33789 = CIRCLE ( 'NONE', #59349, 14.49999999999999822 ) ;
#33790 = SURFACE_STYLE_USAGE ( .BOTH. , #80796 ) ;
#33791 = CARTESIAN_POINT ( 'NONE',  ( 0.1532563361054083140, 21.00893115100078745, 1.131784320476157264E-15 ) ) ;
#33792 = CARTESIAN_POINT ( 'NONE',  ( 19.84674366389459266, 53.71726448433411605, -2.638427012816827677 ) ) ;
#33793 = EDGE_CURVE ( 'NONE', #44015, #43096, #47568, .T. ) ;
#33794 = CARTESIAN_POINT ( 'NONE',  ( 3.591859063236761518, 49.95696800326375353, 11.09922568453594849 ) ) ;
#33795 = CARTESIAN_POINT ( 'NONE',  ( -0.8801773607111008646, 53.27201867748816966, 2.915334737309923430 ) ) ;
#33796 = CARTESIAN_POINT ( 'NONE',  ( 10.00000000000000178, 32.25893115100078745, 9.846743663894594434 ) ) ;
#33798 = CARTESIAN_POINT ( 'NONE',  ( 10.00000000000000000, 24.75893115100078745, -9.846743663894594434 ) ) ;
#33797 = CARTESIAN_POINT ( 'NONE',  ( -0.3689425029237881626, 47.42874883491396787, 10.36894250292379027 ) ) ;
#33799 = CARTESIAN_POINT ( 'NONE',  ( 0.1955144967548765322, 44.32703681773342907, -6.500000000002692957 ) ) ;
#33800 = CARTESIAN_POINT ( 'NONE',  ( -42.93999999999999773, 92.00000000000000000, -9.292893218813450318 ) ) ;
#33801 = CARTESIAN_POINT ( 'NONE',  ( 10.00000000000000000, 10.55374883491396787, -14.16423886937410082 ) ) ;
#33802 = CARTESIAN_POINT ( 'NONE',  ( 13.79529636645031943, 35.34541550158063927, -14.16423886937409904 ) ) ;
#33803 = CARTESIAN_POINT ( 'NONE',  ( 7.361572987183169658, 24.96726448433412315, -9.846743663894592657 ) ) ;
#33804 = CARTESIAN_POINT ( 'NONE',  ( 18.50749283717776805, 9.699555875704810148, 6.499999999999995559 ) ) ;
#33805 = CARTESIAN_POINT ( 'NONE',  ( 0.5774900079438607392, 28.48035201082150891, 5.440088680355550821 ) ) ;
#33806 = ADVANCED_FACE ( 'NONE', ( #69585 ), #23611, .T. ) ;
#33807 = CARTESIAN_POINT ( 'NONE',  ( 15.44008868035555260, 59.73035201082151247, 9.422509992056143702 ) ) ;
#33808 = CARTESIAN_POINT ( 'NONE',  ( 17.96484262340118221, 46.18868534415484106, -7.964842623401177768 ) ) ;
#33809 = ORIENTED_EDGE ( 'NONE', *, *, #44112, .F. ) ;
#33810 = CARTESIAN_POINT ( 'NONE',  ( 0.6178305044545838731, 49.74863466993041072, 9.382169495545420901 ) ) ;
#33811 = CARTESIAN_POINT ( 'NONE',  ( -0.8801773607111009756, 53.06368534415484106, 1.068504757029289695E-15 ) ) ;
#33812 = ORIENTED_EDGE ( 'NONE', *, *, #63228, .F. ) ;
#33813 = CARTESIAN_POINT ( 'NONE',  ( 13.61464873478173843, 14.49999999999999112, -6.296136897217843753 ) ) ;
#33814 = CARTESIAN_POINT ( 'NONE',  ( 2.035157376598822676, 67.43868534415484817, -7.964842623401177768 ) ) ;
#33815 = ORIENTED_EDGE ( 'NONE', *, *, #14605, .T. ) ;
#33816 = CARTESIAN_POINT ( 'NONE',  ( 19.42250999205614548, 65.98035201082151957, -5.440088680355545492 ) ) ;
#33817 = CARTESIAN_POINT ( 'NONE',  ( 19.42250999205614193, 5.147018677488171434, 5.440088680355555262 ) ) ;
#33818 = AXIS2_PLACEMENT_3D ( 'NONE', #36178, #50185, #57193 ) ;
#33819 = DIRECTION ( 'NONE',  ( -0.000000000000000000, 0.000000000000000000, 1.000000000000000000 ) ) ;
#33820 = DIRECTION ( 'NONE',  ( 1.000000000000000000, -0.000000000000000000, 0.000000000000000000 ) ) ;
#33821 = CARTESIAN_POINT ( 'NONE',  ( 12.91533473730993009, 11.60535201082150714, -10.88017736071109987 ) ) ;
#33822 = CARTESIAN_POINT ( 'NONE',  ( 19.84674366389459266, 13.30059781766745353, 2.638427012816836559 ) ) ;
#33823 = B_SPLINE_CURVE_WITH_KNOTS ( 'NONE', 3,
 ( #70910, #54405, #63386, #1935, #85410, #15933 ),
 .UNSPECIFIED., .F., .F.,
 ( 4, 2, 4 ),
 ( 0.0002800001171688671947, 0.0006862053477355151403, 0.001092410578302163140 ),
 .UNSPECIFIED. ) ;
#33824 = CARTESIAN_POINT ( 'NONE',  ( 10.00000000000000000, 10.55374883491396787, -14.16423886937410082 ) ) ;
#33825 = CARTESIAN_POINT ( 'NONE',  ( 12.63842701281683034, 2.467264484334118269, 9.846743663894596210 ) ) ;
#33826 = CARTESIAN_POINT ( 'NONE',  ( -0.8801773607111009756, 13.06368534415483929, 1.068504757029289695E-15 ) ) ;
#33827 = CARTESIAN_POINT ( 'NONE',  ( 0.1532563361054100626, 50.80059781766745175, -2.638427012816831230 ) ) ;
#33828 = VERTEX_POINT ( 'NONE', #24592 ) ;
#33829 = CARTESIAN_POINT ( 'NONE',  ( 12.63842701281683034, 47.46726448433412315, 9.846743663894596210 ) ) ;
#33830 = ORIENTED_EDGE ( 'NONE', *, *, #52976, .T. ) ;
#33831 = CARTESIAN_POINT ( 'NONE',  ( 0.5774900079438607392, 48.48035201082150536, 5.440088680355550821 ) ) ;
#33832 = CARTESIAN_POINT ( 'NONE',  ( 7.361572987183169658, 49.96726448433410894, -9.846743663894592657 ) ) ;
#33834 = CARTESIAN_POINT ( 'NONE',  ( -2.393480905992944496, 15.00000000000000000, -14.80781041047754520 ) ) ;
#33833 = FILL_AREA_STYLE ('',( #3373 ) ) ;
#33835 = CARTESIAN_POINT ( 'NONE',  ( -0.8801773607111009756, 63.06368534415484106, 1.068504757029289695E-15 ) ) ;
#33836 = CARTESIAN_POINT ( 'NONE',  ( 7.084665262690076126, 4.105352010821503583, 10.88017736071109987 ) ) ;
#33837 = EDGE_CURVE ( 'NONE', #55756, #71742, #86385, .T. ) ;
#33838 = MECHANICAL_DESIGN_GEOMETRIC_PRESENTATION_REPRESENTATION (  '', ( #43423 ), #5257 ) ;
#33839 = CARTESIAN_POINT ( 'NONE',  ( 3.591859063236761518, 34.95696800326375353, 11.09922568453594849 ) ) ;
#33840 = CARTESIAN_POINT ( 'NONE',  ( 0.000000000000000000, 15.00000000000000000, 0.000000000000000000 ) ) ;
#33841 = EDGE_CURVE ( 'NONE', #59170, #71199, #17729, .T. ) ;
#33842 = ORIENTED_EDGE ( 'NONE', *, *, #48415, .T. ) ;
#33843 = CARTESIAN_POINT ( 'NONE',  ( -1.099225684535947600, 44.54030133659708923, 6.408140936763237150 ) ) ;
#33844 = CARTESIAN_POINT ( 'NONE',  ( 4.559911319644449179, 37.23035201082150536, -9.422509992056141925 ) ) ;
#33845 = TOROIDAL_SURFACE ( 'NONE', #89748, 2.900000000000001243, 0.1000000000000000056 ) ;
#33846 = ORIENTED_EDGE ( 'NONE', *, *, #25034, .F. ) ;
#33847 = AXIS2_PLACEMENT_3D ( 'NONE', #63480, #39519, #47978 ) ;
#33848 = AXIS2_PLACEMENT_3D ( 'NONE', #76470, #38484, #77440 ) ;
#33849 = CARTESIAN_POINT ( 'NONE',  ( 0.1532563361054083140, 61.00893115100078745, 1.131784320476157264E-15 ) ) ;
#33851 = CARTESIAN_POINT ( 'NONE',  ( 12.63842701281683034, 57.46726448433411605, 9.846743663894596210 ) ) ;
#33850 = CARTESIAN_POINT ( 'NONE',  ( 18.52753015748617571, 18.09226448433411960, 4.923371831947298993 ) ) ;
#33852 = CARTESIAN_POINT ( 'NONE',  ( 19.72487221294569792, 32.80223176428832232, -6.500000000000008882 ) ) ;
#33853 = DIRECTION ( 'NONE',  ( -1.000000000000000000, 3.556618985922298287E-15, 0.000000000000000000 ) ) ;
#33854 = DIRECTION ( 'NONE',  ( 0.000000000000000000, 0.000000000000000000, 1.000000000000000000 ) ) ;
#33855 = CARTESIAN_POINT ( 'NONE',  ( -12.87890026492928541, 14.95077488074853456, -7.195834080858529269 ) ) ;
#33857 = CARTESIAN_POINT ( 'NONE',  ( -10.84451454130491399, 15.00000000000000000, -9.625305416630974165 ) ) ;
#33856 = CARTESIAN_POINT ( 'NONE',  ( 7.361572987183169658, 24.96726448433412315, -9.846743663894592657 ) ) ;
#33858 = CARTESIAN_POINT ( 'NONE',  ( 0.000000000000000000, 0.5000000000000004441, 0.000000000000000000 ) ) ;
#33860 = ORIENTED_EDGE ( 'NONE', *, *, #89863, .F. ) ;
#33859 = CARTESIAN_POINT ( 'NONE',  ( 5.076628168052704559, 65.17559781766745175, -8.527530157486179263 ) ) ;
#33861 = AXIS2_PLACEMENT_3D ( 'NONE', #78813, #33296, #94296 ) ;
#33862 = B_SPLINE_CURVE_WITH_KNOTS ( 'NONE', 3,
 ( #10902, #79880, #79396, #41907, #25905, #86893 ),
 .UNSPECIFIED., .F., .F.,
 ( 4, 2, 4 ),
 ( 0.0002800001171688651347, 0.0006862053477355225129, 0.001092410578302179837 ),
 .UNSPECIFIED. ) ;
#33863 =( NAMED_UNIT ( * ) SI_UNIT ( $, .STERADIAN. ) SOLID_ANGLE_UNIT ( ) );
#33864 = CARTESIAN_POINT ( 'NONE',  ( 16.40814093676324603, 22.45696800326375353, -11.09922568453594671 ) ) ;
#33865 = EDGE_CURVE ( 'NONE', #43087, #68316, #24093, .T. ) ;
#33866 = CARTESIAN_POINT ( 'NONE',  ( 19.84674366389459266, 43.71726448433410894, -2.638427012816827677 ) ) ;
#33867 = CARTESIAN_POINT ( 'NONE',  ( -1.780824192092276048, 14.49999999999999112, -14.89391369643522545 ) ) ;
#33868 = CARTESIAN_POINT ( 'NONE',  ( 20.36894250292379738, 54.92874883491396076, -10.36894250292379027 ) ) ;
#33869 = CARTESIAN_POINT ( 'NONE',  ( 10.00000000000000000, 14.75893115100078568, -9.846743663894594434 ) ) ;
#33870 = ORIENTED_EDGE ( 'NONE', *, *, #42565, .T. ) ;
#33871 = CARTESIAN_POINT ( 'NONE',  ( 0.2751277870542980231, 5.302231764288316107, 6.500000000000002665 ) ) ;
#33872 = EDGE_CURVE ( 'NONE', #66451, #10816, #1105, .T. ) ;
#33873 = CARTESIAN_POINT ( 'NONE',  ( 17.08211943468705130, 63.47041550158063927, 12.26659068614894998 ) ) ;
#33874 = CARTESIAN_POINT ( 'NONE',  ( 2.791683348922237240, 60.38393115100078745, -7.208316651077763204 ) ) ;
#33875 = CARTESIAN_POINT ( 'NONE',  ( 2.035157376598824452, 8.688685344154839285, 7.964842623401179544 ) ) ;
#33876 = CARTESIAN_POINT ( 'NONE',  ( 10.00000000000000178, 43.05374883491397497, 14.16423886937410082 ) ) ;
#33877 = CARTESIAN_POINT ( 'NONE',  ( 10.00000000000000000, 45.55374883491397497, -14.16423886937410082 ) ) ;
#33878 = DIRECTION ( 'NONE',  ( 0.8241261886220204724, 0.000000000000000000, -0.5664062369248259454 ) ) ;
#33880 = CARTESIAN_POINT ( 'NONE',  ( 7.361572987183170547, 52.05059781766745175, 9.846743663894590881 ) ) ;
#33879 = CARTESIAN_POINT ( 'NONE',  ( 0.000000000000000000, 15.00000000000000000, 0.000000000000000000 ) ) ;
#33881 = ORIENTED_EDGE ( 'NONE', *, *, #5580, .F. ) ;
#33882 = CARTESIAN_POINT ( 'NONE',  ( 20.88017736071110519, 40.56368534415484106, 2.639326808657452039E-16 ) ) ;
#33883 = CARTESIAN_POINT ( 'NONE',  ( 8.900383361500256996, -1.049454312711732840, 3.750000000000000000 ) ) ;
#33884 = CARTESIAN_POINT ( 'NONE',  ( 10.00000000000000178, 52.25893115100078745, 9.846743663894594434 ) ) ;
#33885 = FACE_OUTER_BOUND ( 'NONE', #78584, .T. ) ;
#33886 = CARTESIAN_POINT ( 'NONE',  ( 10.36894250292378850, 4.928748834913970533, -10.36894250292379027 ) ) ;
#33887 = CARTESIAN_POINT ( 'NONE',  ( 2.791683348922237240, 60.38393115100078745, -7.208316651077763204 ) ) ;
#33888 = CARTESIAN_POINT ( 'NONE',  ( 1.472469842513823179, 60.59226448433412315, -4.923371831947296329 ) ) ;
#33889 = CIRCLE ( 'NONE', #83452, 0.5000000000000066613 ) ;
#33890 = EDGE_LOOP ( 'NONE', ( #93096, #16778, #18205, #57808 ) ) ;
#33891 = CARTESIAN_POINT ( 'NONE',  ( 17.08211943468705840, 30.13708216824730357, -12.26659068614894466 ) ) ;
#33892 = CARTESIAN_POINT ( 'NONE',  ( 1.472469842513823179, 1.425597817667451528, 4.923371831947296329 ) ) ;
#33894 = CARTESIAN_POINT ( 'NONE',  ( -10.70613742633244669, 15.00000000000000000, -9.778988772285387654 ) ) ;
#33893 = CARTESIAN_POINT ( 'NONE',  ( -3.585386599742077962, -2.690194976740517330, -2.750000000000402789 ) ) ;
#33895 = CARTESIAN_POINT ( 'NONE',  ( -0.8801773607110991993, 12.85535201082150358, -2.915334737309923874 ) ) ;
#33896 = CARTESIAN_POINT ( 'NONE',  ( 10.00000000000000178, 25.37363466993041783, 12.81628187352647608 ) ) ;
#33897 = CARTESIAN_POINT ( 'NONE',  ( 3.836325488036183451, 0.5000000000000004441, -14.50112432709422627 ) ) ;
#33898 = CARTESIAN_POINT ( 'NONE',  ( 10.00000000000000000, 9.758931151000785675, -9.846743663894594434 ) ) ;
#33899 = CARTESIAN_POINT ( 'NONE',  ( 5.115475850186006923, -17.53855045867880591, -3.750000000001609823 ) ) ;
#33900 = CARTESIAN_POINT ( 'NONE',  ( 2.917880565312950480, 30.97041550158063572, -12.26659068614894821 ) ) ;
#33901 = DIRECTION ( 'NONE',  ( 0.000000000000000000, 0.000000000000000000, 1.000000000000000000 ) ) ;
#33902 = CARTESIAN_POINT ( 'NONE',  ( 19.72487221294571569, 50.71833443783938122, -6.499999999999983125 ) ) ;
#33903 = CARTESIAN_POINT ( 'NONE',  ( 17.96484262340118221, 4.938685344154837509, 7.964842623401181321 ) ) ;
#33904 = DIRECTION ( 'NONE',  ( 0.000000000000000000, -1.000000000000000000, 0.000000000000000000 ) ) ;
#33905 = CARTESIAN_POINT ( 'NONE',  ( 19.42250999205614548, 40.98035201082150536, -5.440088680355545492 ) ) ;
#33906 = CARTESIAN_POINT ( 'NONE',  ( 17.96484262340118221, 34.93868534415482685, 7.964842623401181321 ) ) ;
#33907 = CARTESIAN_POINT ( 'NONE',  ( 5.076628168052703671, 66.84226448433412315, 8.527530157486179263 ) ) ;
#33908 = CARTESIAN_POINT ( 'NONE',  ( 0.1532563361054082862, 61.21726448433412315, 2.638427012816831674 ) ) ;
#33909 = CARTESIAN_POINT ( 'NONE',  ( 1.274849032793998305, 2.555090184799397424, -6.499999999999581668 ) ) ;
#33910 = CARTESIAN_POINT ( 'NONE',  ( 0.1532563361054082862, 6.217264484334118713, 2.638427012816831674 ) ) ;
#33911 = ORIENTED_EDGE ( 'NONE', *, *, #51830, .F. ) ;
#33912 = CARTESIAN_POINT ( 'NONE',  ( -0.8801773607110991993, 47.85535201082150536, -2.915334737309923874 ) ) ;
#33913 = EDGE_CURVE ( 'NONE', #34811, #11994, #35252, .T. ) ;
#33914 = AXIS2_PLACEMENT_3D ( 'NONE', #41463, #94923, #34908 ) ;
#33915 = CARTESIAN_POINT ( 'NONE',  ( 22.81628187352647785, 11.41530133659708390, 3.434112377981063169 ) ) ;
#33916 = CARTESIAN_POINT ( 'NONE',  ( 17.96484262340118221, 56.18868534415484817, -7.964842623401177768 ) ) ;
#33917 = CARTESIAN_POINT ( 'NONE',  ( 17.20831665107776587, 27.88393115100078390, 7.208316651077764980 ) ) ;
#33918 = CARTESIAN_POINT ( 'NONE',  ( -2.816281873526471635, 38.91530133659708213, -3.434112377981056508 ) ) ;
#33919 = AXIS2_PLACEMENT_3D ( 'NONE', #26252, #42250, #81221 ) ;
#33921 = DIRECTION ( 'NONE',  ( -1.000000000000000000, 0.000000000000000000, 0.000000000000000000 ) ) ;
#33920 = CARTESIAN_POINT ( 'NONE',  ( 19.84674366389459266, 8.717264484334116048, -2.638427012816827677 ) ) ;
#33922 = CIRCLE ( 'NONE', #59494, 15.00000000000000000 ) ;
#33923 = VERTEX_POINT ( 'NONE', #84591 ) ;
#33924 = CARTESIAN_POINT ( 'NONE',  ( 1.711636803080560432, 56.84492782695772917, -6.500000000000039080 ) ) ;
#33925 = CARTESIAN_POINT ( 'NONE',  ( 2.377183314879977249, 15.78593319516823001, -6.500000000000010658 ) ) ;
#33926 = DIRECTION ( 'NONE',  ( 0.000000000000000000, 0.000000000000000000, 1.000000000000000000 ) ) ;
#33927 = CARTESIAN_POINT ( 'NONE',  ( 18.52753015748617571, 18.09226448433411960, 4.923371831947298993 ) ) ;
#33928 = COLOUR_RGB ( '', 0.09019608, 0.27058824, 0.51372549) ;
#33929 = CARTESIAN_POINT ( 'NONE',  ( 12.91533473730993009, 11.60535201082150536, -10.88017736071109987 ) ) ;
#33930 = CARTESIAN_POINT ( 'NONE',  ( 4.559911319644449179, 8.897018677488173211, 9.422509992056141925 ) ) ;
#33931 = EDGE_LOOP ( 'NONE', ( #52152, #34193, #76285, #39256, #50267, #71037 ) ) ;
#33932 = VECTOR ( 'NONE', #3305, 1000.000000000000000 ) ;
#33933 = CARTESIAN_POINT ( 'NONE',  ( 7.084665262690076126, 19.10535201082150181, 10.88017736071109987 ) ) ;
#33934 = CARTESIAN_POINT ( 'NONE',  ( 20.88017736071110519, 20.56368534415484106, 2.639326808657452039E-16 ) ) ;
#33935 = DIRECTION ( 'NONE',  ( 0.000000000000000000, 1.000000000000000000, -0.000000000000000000 ) ) ;
#33936 = COLOUR_RGB ( '', 0.08235294, 0.09019608, 0.10196078) ;
#33937 = VERTEX_POINT ( 'NONE', #53094 ) ;
#33938 = CARTESIAN_POINT ( 'NONE',  ( 18.52753015748618282, 63.92559781766745886, -4.923371831947291888 ) ) ;
#33939 = CARTESIAN_POINT ( 'NONE',  ( 17.96484262340118221, 19.93868534415484106, 7.964842623401181321 ) ) ;
#33940 = CARTESIAN_POINT ( 'NONE',  ( 14.92337183194729633, 62.67559781766745886, 8.527530157486181039 ) ) ;
#33941 = CARTESIAN_POINT ( 'NONE',  ( 20.15039907845753220, 49.72266099184918176, 6.262539305110078836 ) ) ;
#33942 = CARTESIAN_POINT ( 'NONE',  ( 0.6178305044545838731, 49.74863466993041072, 9.382169495545420901 ) ) ;
#33943 = CARTESIAN_POINT ( 'NONE',  ( -7.551349515323020789, 15.00000000000000000, -12.08468537022916323 ) ) ;
#33944 = CARTESIAN_POINT ( 'NONE',  ( 10.00000000000000178, 33.05374883491396787, 14.16423886937410082 ) ) ;
#33945 = CARTESIAN_POINT ( 'NONE',  ( 17.96484262340118221, 39.93868534415484106, 7.964842623401181321 ) ) ;
#33946 = CARTESIAN_POINT ( 'NONE',  ( 17.96484262340118221, 19.93868534415484106, 7.964842623401181321 ) ) ;
#33947 = CARTESIAN_POINT ( 'NONE',  ( 5.076628168052704559, 50.17559781766745886, -8.527530157486179263 ) ) ;
#33948 =( LENGTH_UNIT ( ) NAMED_UNIT ( * ) SI_UNIT ( .MILLI., .METRE. ) );
#33950 = EDGE_CURVE ( 'NONE', #52793, #49695, #36844, .T. ) ;
#33949 = CARTESIAN_POINT ( 'NONE',  ( 14.92337183194729633, 37.67559781766745175, 8.527530157486181039 ) ) ;
#33951 = DIRECTION ( 'NONE',  ( 0.000000000000000000, 0.000000000000000000, 1.000000000000000000 ) ) ;
#33952 = CARTESIAN_POINT ( 'NONE',  ( 10.00000000000000000, 14.75893115100078568, -9.846743663894594434 ) ) ;
#33953 = CARTESIAN_POINT ( 'NONE',  ( -12.81628187352647252, -30.66803199673624292, 3.434112377981066722 ) ) ;
#33954 = ORIENTED_EDGE ( 'NONE', *, *, #19291, .T. ) ;
#33955 = CARTESIAN_POINT ( 'NONE',  ( 0.5774900079438607392, 13.48035201082150358, 5.440088680355550821 ) ) ;
#33956 = CARTESIAN_POINT ( 'NONE',  ( 0.1532563361054082862, 11.21726448433411605, 2.638427012816831674 ) ) ;
#33957 = CARTESIAN_POINT ( 'NONE',  ( -1.099225684535947600, 3.706968003263753531, -6.408140936763238038 ) ) ;
#33958 = CARTESIAN_POINT ( 'NONE',  ( 20.88017736071110875, 50.77201867748817676, -2.915334737309920765 ) ) ;
#33960 = CARTESIAN_POINT ( 'NONE',  ( 3.591859063236763294, 38.29030133659708923, -11.09922568453595026 ) ) ;
#33959 = CARTESIAN_POINT ( 'NONE',  ( 19.42250999205614548, 25.98035201082150891, -5.440088680355545492 ) ) ;
#33961 = CARTESIAN_POINT ( 'NONE',  ( 24.16423886937410614, 34.51208216824731068, -3.795296366450302550 ) ) ;
#33962 = FACE_OUTER_BOUND ( 'NONE', #89585, .T. ) ;
#33963 = AXIS2_PLACEMENT_3D ( 'NONE', #67207, #8189, #16180 ) ;
#33964 = EDGE_CURVE ( 'NONE', #71557, #37014, #91152, .T. ) ;
#33965 = CARTESIAN_POINT ( 'NONE',  ( 19.38216949554541202, 60.99863466993042493, 9.382169495545424454 ) ) ;
#33966 = EDGE_CURVE ( 'NONE', #42118, #97832, #75881, .T. ) ;
#33967 = ORIENTED_EDGE ( 'NONE', *, *, #39973, .T. ) ;
#33968 = CARTESIAN_POINT ( 'NONE',  ( 7.361572987183170547, 57.05059781766744464, 9.846743663894590881 ) ) ;
#33969 = CARTESIAN_POINT ( 'NONE',  ( 17.96484262340118221, 34.93868534415482685, 7.964842623401181321 ) ) ;
#33970 = EDGE_LOOP ( 'NONE', ( #13195, #40141, #23444, #4983 ) ) ;
#33972 = CARTESIAN_POINT ( 'NONE',  ( -5.795997163830251431, 0.000000000000000000, 13.01802277140702024 ) ) ;
#33971 = CARTESIAN_POINT ( 'NONE',  ( 1.472469842513823179, 5.592264484334118713, -4.923371831947296329 ) ) ;
#33973 = CARTESIAN_POINT ( 'NONE',  ( 12.63842701281683034, 12.46726448433411782, 9.846743663894596210 ) ) ;
#33974 = CARTESIAN_POINT ( 'NONE',  ( 17.20831665107776587, 24.13393115100078035, -7.208316651077762316 ) ) ;
#33975 = CARTESIAN_POINT ( 'NONE',  ( 10.00000000000000000, 4.758931151000784787, -9.846743663894594434 ) ) ;
#33976 = CARTESIAN_POINT ( 'NONE',  ( 1.472469842513823179, 6.425597817667451750, 4.923371831947296329 ) ) ;
#33978 = CARTESIAN_POINT ( 'NONE',  ( -5.147851794455697849, -3.098870037529856607E-15, -13.68970903997134236 ) ) ;
#33977 = CARTESIAN_POINT ( 'NONE',  ( 15.44008868035555793, 61.39701867748817676, -9.422509992056140149 ) ) ;
#33979 = CARTESIAN_POINT ( 'NONE',  ( 12.91533473730993009, 56.60535201082151247, -10.88017736071109987 ) ) ;
#33982 = ORIENTED_EDGE ( 'NONE', *, *, #510, .F. ) ;
#33981 = AXIS2_PLACEMENT_3D ( 'NONE', #94806, #43280, #73775 ) ;
#33980 = CARTESIAN_POINT ( 'NONE',  ( 7.361572987183169658, 14.96726448433411960, -9.846743663894592657 ) ) ;
#33983 = CARTESIAN_POINT ( 'NONE',  ( 14.09394518620612224, 3.883508853191620072E-16, -3.407449058785360752 ) ) ;
#33985 = EDGE_CURVE ( 'NONE', #61040, #86598, #15120, .T. ) ;
#33984 = CARTESIAN_POINT ( 'NONE',  ( 10.00000000000000178, 52.25893115100078745, 9.846743663894594434 ) ) ;
#33986 = VERTEX_POINT ( 'NONE', #28382 ) ;
#33987 = DIRECTION ( 'NONE',  ( -0.000000000000000000, 0.000000000000000000, 1.000000000000000000 ) ) ;
#33988 = TOROIDAL_SURFACE ( 'NONE', #59562, 18.53834841531100608, 7.000000000000000000 ) ;
#33989 = CARTESIAN_POINT ( 'NONE',  ( 10.00000000000000178, 8.053748834913967869, 14.16423886937410082 ) ) ;
#33990 = AXIS2_PLACEMENT_3D ( 'NONE', #86157, #1690, #62646 ) ;
#33991 = CIRCLE ( 'NONE', #49998, 15.00000000000000000 ) ;
#33992 = CARTESIAN_POINT ( 'NONE',  ( 14.49999999999999822, 75.00000000000000000, -8.525133428036872019 ) ) ;
#33993 = ADVANCED_FACE ( 'NONE', ( #70572 ), #94539, .F. ) ;
#33994 = VECTOR ( 'NONE', #61095, 1000.000000000000000 ) ;
#33995 = CARTESIAN_POINT ( 'NONE',  ( 20.36894250292379382, 23.67874883491397142, 10.36894250292379205 ) ) ;
#33996 = CARTESIAN_POINT ( 'NONE',  ( 24.16423886937410614, 29.30374883491396787, 8.672049930838204340E-16 ) ) ;
#33997 = CARTESIAN_POINT ( 'NONE',  ( 6.204703633549690345, 2.845415501580634388, 14.16423886937410082 ) ) ;
#33998 = CARTESIAN_POINT ( 'NONE',  ( -12.80781515976318907, -0.03417435944610275333, 6.246788841744232990 ) ) ;
#33999 = CARTESIAN_POINT ( 'NONE',  ( 15.44008868035555260, 34.73035201082151247, 9.422509992056143702 ) ) ;
#34000 = FILL_AREA_STYLE ('',( #3054 ) ) ;
#34001 = EDGE_LOOP ( 'NONE', ( #27264, #62923, #48456, #40857 ) ) ;
#34003 =( GEOMETRIC_REPRESENTATION_CONTEXT ( 3 ) GLOBAL_UNCERTAINTY_ASSIGNED_CONTEXT ( ( #14268 ) ) GLOBAL_UNIT_ASSIGNED_CONTEXT ( ( #6832, #45319, #30802 ) ) REPRESENTATION_CONTEXT ( 'NONE', 'WORKASPACE' ) );
#34002 = CARTESIAN_POINT ( 'NONE',  ( 5.076628168052703671, 21.84226448433411960, 8.527530157486179263 ) ) ;
#34005 = CARTESIAN_POINT ( 'NONE',  ( 10.00000000000000000, 9.758931151000785675, -9.846743663894594434 ) ) ;
#34004 = CARTESIAN_POINT ( 'NONE',  ( 20.88017736071110164, 55.35535201082149825, 2.915334737309930979 ) ) ;
#34006 = ORIENTED_EDGE ( 'NONE', *, *, #84469, .F. ) ;
#34007 = CARTESIAN_POINT ( 'NONE',  ( 6.565887622018943937, 40.16530133659708923, 12.81628187352647430 ) ) ;
#34008 = CARTESIAN_POINT ( 'NONE',  ( 0.1532563361054083140, 31.00893115100078390, 1.131784320476157264E-15 ) ) ;
#34009 = DIRECTION ( 'NONE',  ( 0.000000000000000000, -1.000000000000000000, 0.000000000000000000 ) ) ;
#34010 = CARTESIAN_POINT ( 'NONE',  ( 7.084665262690076126, 57.02201867748817676, -10.88017736071110164 ) ) ;
#34011 = CARTESIAN_POINT ( 'NONE',  ( 3.591859063236763294, 28.29030133659708568, -11.09922568453595026 ) ) ;
#34012 = CARTESIAN_POINT ( 'NONE',  ( -3.927832320392339316, 0.000000000000000000, 13.69797916712101404 ) ) ;
#34013 = CARTESIAN_POINT ( 'NONE',  ( 19.84674366389459266, 28.30059781766745886, 2.638427012816836559 ) ) ;
#34014 = CARTESIAN_POINT ( 'NONE',  ( 24.16423886937410614, 14.51208216824730179, -3.795296366450302550 ) ) ;
#34015 = ORIENTED_EDGE ( 'NONE', *, *, #38300, .T. ) ;
#34016 = CARTESIAN_POINT ( 'NONE',  ( 12.91533473730992121, 39.52201867748817676, 10.88017736071110164 ) ) ;
#34017 = CARTESIAN_POINT ( 'NONE',  ( 0.5774900079438590739, 52.64701867748817676, -5.440088680355550821 ) ) ;
#34018 = CARTESIAN_POINT ( 'NONE',  ( -4.164238869374098151, 46.59541550158063927, -3.795296366450310543 ) ) ;
#34019 = CARTESIAN_POINT ( 'NONE',  ( 10.00000000000000178, 57.25893115100078745, 9.846743663894594434 ) ) ;
#34020 = CARTESIAN_POINT ( 'NONE',  ( 19.84674366389459266, 8.717264484334116048, -2.638427012816827677 ) ) ;
#34022 = CARTESIAN_POINT ( 'NONE',  ( -12.94148294176548930, 90.75484370785778765, 7.596443435273323885 ) ) ;
#34021 = CARTESIAN_POINT ( 'NONE',  ( 14.62617646268092209, 14.49999999999999112, 3.327906561566971622 ) ) ;
#34023 = CARTESIAN_POINT ( 'NONE',  ( 2.035157376598824452, 43.68868534415484106, 7.964842623401179544 ) ) ;
#34024 = DIRECTION ( 'NONE',  ( -1.048050535246147774E-13, 0.000000000000000000, 1.000000000000000000 ) ) ;
#34025 = CARTESIAN_POINT ( 'NONE',  ( 19.38216949554541202, 20.99863466993042138, 9.382169495545424454 ) ) ;
#34026 = CARTESIAN_POINT ( 'NONE',  ( 22.81628187352648496, 21.83196800326374643, -3.434112377981050290 ) ) ;
#34027 = CARTESIAN_POINT ( 'NONE',  ( 14.92337183194729633, 47.67559781766745175, 8.527530157486181039 ) ) ;
#34028 = CARTESIAN_POINT ( 'NONE',  ( -2.915334737309917656, 14.10535201082150714, 10.88017736071110164 ) ) ;
#34029 = CARTESIAN_POINT ( 'NONE',  ( 0.5774900079438607392, 3.480352010821504027, 5.440088680355550821 ) ) ;
#34030 = CARTESIAN_POINT ( 'NONE',  ( 19.42250999205614193, 65.14701867748817676, 5.440088680355555262 ) ) ;
#34031 = DIRECTION ( 'NONE',  ( 0.000000000000000000, 0.000000000000000000, -1.000000000000000000 ) ) ;
#34032 = FACE_OUTER_BOUND ( 'NONE', #40127, .T. ) ;
#34033 = CARTESIAN_POINT ( 'NONE',  ( 7.084665262690076126, 64.10535201082150536, 10.88017736071109987 ) ) ;
#34035 = CARTESIAN_POINT ( 'NONE',  ( 19.42250999205614548, 65.98035201082151957, -5.440088680355545492 ) ) ;
#34034 = CIRCLE ( 'NONE', #3745, 0.2500000000000002220 ) ;
#34036 = CARTESIAN_POINT ( 'NONE',  ( 0.000000000000000000, 15.00000000000000000, 0.000000000000000000 ) ) ;
#34037 = CARTESIAN_POINT ( 'NONE',  ( 0.1532563361054083140, 26.00893115100078745, 1.131784320476157264E-15 ) ) ;
#34038 = CARTESIAN_POINT ( 'NONE',  ( 4.559911319644449179, 23.89701867748817321, 9.422509992056141925 ) ) ;
#34039 = CARTESIAN_POINT ( 'NONE',  ( 19.84674366389459621, 63.50893115100078745, 7.409399052514197653E-17 ) ) ;
#34041 = DIRECTION ( 'NONE',  ( 0.000000000000000000, -1.000000000000000000, 0.000000000000000000 ) ) ;
#34040 = CARTESIAN_POINT ( 'NONE',  ( 19.42250999205614548, 30.98035201082150536, -5.440088680355545492 ) ) ;
#34042 = CARTESIAN_POINT ( 'NONE',  ( 64.56412365047461321, 11.99999999999999467, -9.500000000000000000 ) ) ;
#34043 = CARTESIAN_POINT ( 'NONE',  ( 0.6178305044545838731, 44.74863466993042493, 9.382169495545420901 ) ) ;
#34044 = ORIENTED_EDGE ( 'NONE', *, *, #27761, .F. ) ;
#34045 = CARTESIAN_POINT ( 'NONE',  ( 17.96484262340118221, 51.18868534415483396, -7.964842623401177768 ) ) ;
#34047 = SURFACE_STYLE_USAGE ( .BOTH. , #3589 ) ;
#34046 = CARTESIAN_POINT ( 'NONE',  ( 22.81628187352647785, 16.41530133659708923, 3.434112377981063169 ) ) ;
#34048 = CARTESIAN_POINT ( 'NONE',  ( -0.8801773607110991993, 22.85535201082150181, -2.915334737309923874 ) ) ;
#34049 = CARTESIAN_POINT ( 'NONE',  ( -4.164238869374099039, 46.80374883491397497, 8.674139862899312516E-16 ) ) ;
#34050 = CARTESIAN_POINT ( 'NONE',  ( 19.84674366389459266, 43.71726448433410894, -2.638427012816827677 ) ) ;
#34051 = CARTESIAN_POINT ( 'NONE',  ( 2.791683348922237240, 0.3839311510007847872, -7.208316651077763204 ) ) ;
#34052 = CARTESIAN_POINT ( 'NONE',  ( 10.00000000000000178, 69.31368534415484817, 10.88017736071110342 ) ) ;
#34053 = CARTESIAN_POINT ( 'NONE',  ( -6.000000000000007994, 41.24999999999999289, 6.250000000000000000 ) ) ;
#34054 = CARTESIAN_POINT ( 'NONE',  ( -4.164238869374099039, 31.80374883491396432, 8.674139862899312516E-16 ) ) ;
#34055 = EDGE_CURVE ( 'NONE', #64180, #57542, #2592, .T. ) ;
#34056 = DIRECTION ( 'NONE',  ( 0.9997628902338883128, -0.02177529129959722073, 0.000000000000000000 ) ) ;
#34057 = CARTESIAN_POINT ( 'NONE',  ( -55.15243902439023316, 44.12195121951212684, -8.000000000000000000 ) ) ;
#34058 = VERTEX_POINT ( 'NONE', #63542 ) ;
#34059 = ORIENTED_EDGE ( 'NONE', *, *, #44238, .F. ) ;
#34060 = CARTESIAN_POINT ( 'NONE',  ( 17.08211943468705130, 53.47041550158063217, 12.26659068614894998 ) ) ;
#34061 = CARTESIAN_POINT ( 'NONE',  ( -2.266590686148945544, 52.22041550158064638, 7.082119434687048631 ) ) ;
#34062 = CARTESIAN_POINT ( 'NONE',  ( 5.076628168052704559, 20.17559781766745175, -8.527530157486179263 ) ) ;
#34063 = CARTESIAN_POINT ( 'NONE',  ( 19.38216949554541557, 12.24863466993041961, -9.382169495545420901 ) ) ;
#34064 = DIRECTION ( 'NONE',  ( -0.7933533402912367194, 0.000000000000000000, 0.6087614290087187685 ) ) ;
#34066 = CARTESIAN_POINT ( 'NONE',  ( 0.6081133539230537677, 58.33703382326400799, 6.499999999999968914 ) ) ;
#34065 = COLOUR_RGB ( '', 0.09019608, 0.27058824, 0.51372549) ;
#34068 = CARTESIAN_POINT ( 'NONE',  ( 3.591859063236763294, 33.29030133659708213, -11.09922568453595026 ) ) ;
#34067 =( NAMED_UNIT ( * ) PLANE_ANGLE_UNIT ( ) SI_UNIT ( $, .RADIAN. ) );
#34069 = CARTESIAN_POINT ( 'NONE',  ( 2.917880565312948704, 37.63708216824731068, 12.26659068614894643 ) ) ;
#34070 = AXIS2_PLACEMENT_3D ( 'NONE', #77165, #14722, #223 ) ;
#34071 = PLANE ( 'NONE',  #17331 ) ;
#34072 = CARTESIAN_POINT ( 'NONE',  ( -0.8801773607110991993, 67.85535201082151957, -2.915334737309923874 ) ) ;
#34073 = VECTOR ( 'NONE', #18954, 1000.000000000000114 ) ;
#34074 = CARTESIAN_POINT ( 'NONE',  ( -7.208316651077764980, 5.383931151000783899, -7.208316651077759651 ) ) ;
#34075 = ORIENTED_EDGE ( 'NONE', *, *, #97402, .T. ) ;
#34076 = FACE_OUTER_BOUND ( 'NONE', #62763, .T. ) ;
#34077 = CARTESIAN_POINT ( 'NONE',  ( 0.1532563361054082862, 16.21726448433411960, 2.638427012816831674 ) ) ;
#34078 = VECTOR ( 'NONE', #27728, 1000.000000000000000 ) ;
#34080 = EDGE_CURVE ( 'NONE', #3379, #36801, #70401, .T. ) ;
#34079 = CARTESIAN_POINT ( 'NONE',  ( 3.969999999999999751, 10.25000000000000000, 3.750000000000000000 ) ) ;
#34081 = VERTEX_POINT ( 'NONE', #5401 ) ;
#34082 = CARTESIAN_POINT ( 'NONE',  ( 10.00000000000000000, 10.55374883491396787, -14.16423886937410082 ) ) ;
#34084 = CARTESIAN_POINT ( 'NONE',  ( -0.8801773607110991993, 12.85535201082150358, -2.915334737309923874 ) ) ;
#34083 = CARTESIAN_POINT ( 'NONE',  ( -0.8801773607110991993, 2.855352010821504471, -2.915334737309923874 ) ) ;
#34086 = CARTESIAN_POINT ( 'NONE',  ( 22.81628187352647785, 6.415301336597088344, 3.434112377981063169 ) ) ;
#34085 = CARTESIAN_POINT ( 'NONE',  ( 12.63842701281683034, 52.46726448433413026, 9.846743663894596210 ) ) ;
#34087 =( NAMED_UNIT ( * ) SI_UNIT ( $, .STERADIAN. ) SOLID_ANGLE_UNIT ( ) );
#34088 = CARTESIAN_POINT ( 'NONE',  ( 9.838578643762659226, 27.00180849546941175, -3.000000000000000888 ) ) ;
#34089 = EDGE_CURVE ( 'NONE', #13116, #44015, #33531, .T. ) ;
#34090 = CARTESIAN_POINT ( 'NONE',  ( 21.09922568453594849, 21.20696800326375353, 6.408140936763242479 ) ) ;
#34091 = ADVANCED_FACE ( 'NONE', ( #12877 ), #71067, .T. ) ;
#34092 = ORIENTED_EDGE ( 'NONE', *, *, #59394, .T. ) ;
#34093 = CARTESIAN_POINT ( 'NONE',  ( 6.204703633549690345, 60.76208216824730357, -14.16423886937410259 ) ) ;
#34094 = EDGE_LOOP ( 'NONE', ( #58155, #18633, #93929, #64555 ) ) ;
#34095 = CARTESIAN_POINT ( 'NONE',  ( -0.3689425029237898834, 61.17874883491396076, -10.36894250292378850 ) ) ;
#34096 = ORIENTED_EDGE ( 'NONE', *, *, #5720, .T. ) ;
#34097 = CARTESIAN_POINT ( 'NONE',  ( 17.96484262340118221, 29.93868534415484106, 7.964842623401181321 ) ) ;
#34098 = CARTESIAN_POINT ( 'NONE',  ( 2.035157376598822676, 47.43868534415484817, -7.964842623401177768 ) ) ;
#34099 = CARTESIAN_POINT ( 'NONE',  ( -0.8801773607111008646, 33.27201867748817676, 2.915334737309923430 ) ) ;
#34100 = FACE_OUTER_BOUND ( 'NONE', #19364, .T. ) ;
#34101 = CARTESIAN_POINT ( 'NONE',  ( 19.42250999205614548, 35.98035201082151247, -5.440088680355545492 ) ) ;
#34102 = DIRECTION ( 'NONE',  ( 0.000000000000000000, -1.000000000000000000, 0.000000000000000000 ) ) ;
#34103 = CARTESIAN_POINT ( 'NONE',  ( 14.92337183194729988, 14.34226448433411782, -8.527530157486177487 ) ) ;
#34104 = ORIENTED_EDGE ( 'NONE', *, *, #47623, .F. ) ;
#34105 = CARTESIAN_POINT ( 'NONE',  ( 10.85666693321173071, -52.68303261953400352, 4.000000000000000000 ) ) ;
#34106 = CARTESIAN_POINT ( 'NONE',  ( 0.1532563361054082862, 51.21726448433412315, 2.638427012816831674 ) ) ;
#34107 = FACE_OUTER_BOUND ( 'NONE', #95811, .T. ) ;
#34108 = CARTESIAN_POINT ( 'NONE',  ( 22.81628187352647785, 51.41530133659708923, 3.434112377981063169 ) ) ;
#34109 = EDGE_CURVE ( 'NONE', #49327, #2489, #92725, .T. ) ;
#34110 = DIRECTION ( 'NONE',  ( 0.000000000000000000, 1.000000000000000000, 0.000000000000000000 ) ) ;
#34111 = ORIENTED_EDGE ( 'NONE', *, *, #4795, .F. ) ;
#34112 = CARTESIAN_POINT ( 'NONE',  ( 0.2751277870542967463, 70.00000000000000000, -6.500000000000000888 ) ) ;
#34113 = CARTESIAN_POINT ( 'NONE',  ( -43.85366042784433205, 106.6334074295720313, 4.577838255903318831 ) ) ;
#34114 = FILL_AREA_STYLE ('',( #49134 ) ) ;
#34115 = CARTESIAN_POINT ( 'NONE',  ( -4.164238869374099039, 61.80374883491397497, 8.674139862899312516E-16 ) ) ;
#34116 = LINE ( 'NONE', #57121, #61059 ) ;
#34117 = ORIENTED_EDGE ( 'NONE', *, *, #59868, .T. ) ;
#34118 = DIRECTION ( 'NONE',  ( -0.000000000000000000, -1.000000000000000000, -0.000000000000000000 ) ) ;
#34119 = CARTESIAN_POINT ( 'NONE',  ( 19.84674366389459621, 38.50893115100078745, 7.409399052514197653E-17 ) ) ;
#34120 = CARTESIAN_POINT ( 'NONE',  ( 3.591859063236761518, 64.95696800326376774, 11.09922568453594849 ) ) ;
#34121 = CARTESIAN_POINT ( 'NONE',  ( 16.40814093676323893, 10.79030133659708923, 11.09922568453595026 ) ) ;
#34122 = CARTESIAN_POINT ( 'NONE',  ( 12.63842701281683034, 2.467264484334118269, 9.846743663894596210 ) ) ;
#34123 = CARTESIAN_POINT ( 'NONE',  ( 17.20831665107776587, 12.88393115100078390, 7.208316651077764980 ) ) ;
#34124 = CARTESIAN_POINT ( 'NONE',  ( 2.791683348922240793, 56.63393115100078035, 7.208316651077764092 ) ) ;
#34125 = LINE ( 'NONE', #95127, #25171 ) ;
#34126 = MECHANICAL_DESIGN_GEOMETRIC_PRESENTATION_REPRESENTATION (  '', ( #56498 ), #40522 ) ;
#34127 = ORIENTED_EDGE ( 'NONE', *, *, #36268, .T. ) ;
#34128 = CARTESIAN_POINT ( 'NONE',  ( -0.8801773607110991993, 2.855352010821504471, -2.915334737309923874 ) ) ;
#34129 = DIRECTION ( 'NONE',  ( -0.9953961983671791858, 0.000000000000000000, 0.09584575252022038694 ) ) ;
#34130 = CARTESIAN_POINT ( 'NONE',  ( 20.88017736071110875, 40.77201867748818387, -2.915334737309920765 ) ) ;
#34132 = CARTESIAN_POINT ( 'NONE',  ( 20.88017736071110164, 65.35535201082150536, 2.915334737309930979 ) ) ;
#34131 = CARTESIAN_POINT ( 'NONE',  ( 21.09922568453594849, 26.20696800326375353, 6.408140936763242479 ) ) ;
#34133 = DIRECTION ( 'NONE',  ( 0.000000000000000000, 0.000000000000000000, 1.000000000000000000 ) ) ;
#34134 = CARTESIAN_POINT ( 'NONE',  ( 19.80427997160309417, 17.75733960839544778, -6.499999999999988454 ) ) ;
#34135 = CARTESIAN_POINT ( 'NONE',  ( 20.15039907845753930, 0.07447313448805115144, -6.262539305110068177 ) ) ;
#34136 = CARTESIAN_POINT ( 'NONE',  ( 0.1532563361054082862, 51.21726448433412315, 2.638427012816831674 ) ) ;
#34137 = CARTESIAN_POINT ( 'NONE',  ( 1.472469842513823179, 20.59226448433411960, -4.923371831947296329 ) ) ;
#34138 = CARTESIAN_POINT ( 'NONE',  ( 5.440088680355549045, -18.60298132251182324, -9.422509992056141925 ) ) ;
#34139 = CARTESIAN_POINT ( 'NONE',  ( 10.00000000000000000, 17.87363466993041783, -12.81628187352647608 ) ) ;
#34140 = CARTESIAN_POINT ( 'NONE',  ( -11.42353084958745590, -90.30959216423875091, -3.750000000000000000 ) ) ;
#34142 = DIRECTION ( 'NONE',  ( 1.257568779154408793E-17, 1.000000000000000000, -0.000000000000000000 ) ) ;
#34141 = CARTESIAN_POINT ( 'NONE',  ( 4.559911319644449179, 28.89701867748817321, 9.422509992056141925 ) ) ;
#34143 = CARTESIAN_POINT ( 'NONE',  ( 0.000000000000000000, 0.5000000000000004441, 0.000000000000000000 ) ) ;
#34144 = CARTESIAN_POINT ( 'NONE',  ( 22.26659068614894466, 53.88708216824731068, 7.082119434687054849 ) ) ;
#34145 = CARTESIAN_POINT ( 'NONE',  ( -0.3689425029237898834, 26.17874883491396432, -10.36894250292378850 ) ) ;
#34146 = CARTESIAN_POINT ( 'NONE',  ( 10.00000000000000178, 37.25893115100078745, 9.846743663894594434 ) ) ;
#34147 = CARTESIAN_POINT ( 'NONE',  ( 0.6178305044545818747, 33.49863466993042493, -9.382169495545419124 ) ) ;
#34148 = CARTESIAN_POINT ( 'NONE',  ( 10.00000000000000178, 29.31368534415483751, 10.88017736071110342 ) ) ;
#34149 = CARTESIAN_POINT ( 'NONE',  ( 0.1532563361054083140, 56.00893115100078745, 1.131784320476157264E-15 ) ) ;
#34150 = CARTESIAN_POINT ( 'NONE',  ( 10.00000000000000178, 39.31368534415484106, 10.88017736071110342 ) ) ;
#34151 = CARTESIAN_POINT ( 'NONE',  ( 22.81628187352647785, 6.415301336597088344, 3.434112377981063169 ) ) ;
#34152 = CARTESIAN_POINT ( 'NONE',  ( -0.3689425029237881626, 27.42874883491397142, 10.36894250292379027 ) ) ;
#34153 = DIRECTION ( 'NONE',  ( 0.000000000000000000, 0.000000000000000000, 1.000000000000000000 ) ) ;
#34154 = UNCERTAINTY_MEASURE_WITH_UNIT (LENGTH_MEASURE( 1.000000000000000082E-05 ), #53786, 'distance_accuracy_value', 'NONE');
#34155 =( BOUNDED_CURVE ( )  B_SPLINE_CURVE ( 2, ( #67168, #68652, #14177, #67675, #75655, #89669, #36680, #59661, #13674 ),
 .UNSPECIFIED., .F., .T. ) 
 B_SPLINE_CURVE_WITH_KNOTS ( ( 3, 2, 2, 2, 3 ),
 ( 0.7596570216176964374, 0.7619047619047618625, 0.7678571428571429047, 0.7738095238095238360, 0.7760572640965892610 ),
 .UNSPECIFIED. ) 
 CURVE ( )  GEOMETRIC_REPRESENTATION_ITEM ( )  RATIONAL_B_SPLINE_CURVE ( ( 0.9839835555609424134, 0.9871328979762474809, 1.000000000000000000, 0.9659258262890683122, 1.000000000000000000, 0.9659258262890683122, 1.000000000000000000, 0.9871328979762474809, 0.9839835555609424134 ) ) 
 REPRESENTATION_ITEM ( '' )  );
#34156 = CARTESIAN_POINT ( 'NONE',  ( 7.361572987183170547, 27.05059781766745175, 9.846743663894590881 ) ) ;
#34157 = CARTESIAN_POINT ( 'NONE',  ( 0.6178305044545818747, 48.49863466993042493, -9.382169495545419124 ) ) ;
#34158 = CARTESIAN_POINT ( 'NONE',  ( 6.565887622018943937, 0.1653013365970866511, 12.81628187352647430 ) ) ;
#34159 = ORIENTED_EDGE ( 'NONE', *, *, #51023, .T. ) ;
#34160 = DIRECTION ( 'NONE',  ( 0.000000000000000000, 1.000000000000000000, 0.000000000000000000 ) ) ;
#34161 = CARTESIAN_POINT ( 'NONE',  ( 4.526800700887880780, -5.190657137169758073, 2.750000000000000000 ) ) ;
#34162 = CARTESIAN_POINT ( 'NONE',  ( 6.204703633549690345, 62.84541550158063927, 14.16423886937410082 ) ) ;
#34163 = CARTESIAN_POINT ( 'NONE',  ( 2.035157376598822676, 62.43868534415483396, -7.964842623401177768 ) ) ;
#34164 = CARTESIAN_POINT ( 'NONE',  ( 6.204703633549690345, 17.84541550158063217, 14.16423886937410082 ) ) ;
#34165 = EDGE_CURVE ( 'NONE', #935, #67657, #20889, .T. ) ;
#34166 = CARTESIAN_POINT ( 'NONE',  ( 12.63842701281683034, 2.467264484334118269, 9.846743663894596210 ) ) ;
#34167 = CARTESIAN_POINT ( 'NONE',  ( 5.076628168052704559, 50.17559781766745886, -8.527530157486179263 ) ) ;
#34168 = CARTESIAN_POINT ( 'NONE',  ( 15.44008868035555260, 34.73035201082151247, 9.422509992056143702 ) ) ;
#34169 = CARTESIAN_POINT ( 'NONE',  ( 0.000000000000000000, 0.000000000000000000, 0.000000000000000000 ) ) ;
#34170 = CARTESIAN_POINT ( 'NONE',  ( 5.076628168052704559, 65.17559781766745175, -8.527530157486179263 ) ) ;
#34171 = ADVANCED_FACE ( 'NONE', ( #89375 ), #20931, .T. ) ;
#34172 = ORIENTED_EDGE ( 'NONE', *, *, #85151, .F. ) ;
#34173 = CARTESIAN_POINT ( 'NONE',  ( -4.838527690343430443, 0.5000000000000004441, -14.19819177887733375 ) ) ;
#34174 = ORIENTED_EDGE ( 'NONE', *, *, #98116, .F. ) ;
#34175 = ORIENTED_EDGE ( 'NONE', *, *, #52775, .F. ) ;
#34176 = DIRECTION ( 'NONE',  ( 0.2334453638559155775, 0.000000000000000000, -0.9723699203976741146 ) ) ;
#34177 = CARTESIAN_POINT ( 'NONE',  ( 22.26659068614894466, 8.887082168247300018, 7.082119434687054849 ) ) ;
#34178 = CARTESIAN_POINT ( 'NONE',  ( -2.266590686148945544, 7.220415501580634832, 7.082119434687048631 ) ) ;
#34179 = CARTESIAN_POINT ( 'NONE',  ( 22.26659068614894466, 58.88708216824729647, 7.082119434687054849 ) ) ;
#34180 = CARTESIAN_POINT ( 'NONE',  ( 0.1532563361054100626, 55.80059781766745175, -2.638427012816831230 ) ) ;
#34181 = CARTESIAN_POINT ( 'NONE',  ( 19.84674366389459266, 38.30059781766745175, 2.638427012816836559 ) ) ;
#34182 = CARTESIAN_POINT ( 'NONE',  ( -0.1503990784575328643, 0.1277717457861260453, 6.262539305110068177 ) ) ;
#34184 = CARTESIAN_POINT ( 'NONE',  ( 2.791683348922240793, 66.63393115100079456, 7.208316651077764092 ) ) ;
#34183 = CARTESIAN_POINT ( 'NONE',  ( 7.084665262690076126, 29.10535201082150181, 10.88017736071109987 ) ) ;
#34185 = CARTESIAN_POINT ( 'NONE',  ( -0.3689425029237881626, 7.428748834913967869, 10.36894250292379027 ) ) ;
#34186 = CARTESIAN_POINT ( 'NONE',  ( -0.3689425029237881626, 57.42874883491397497, 10.36894250292379027 ) ) ;
#34187 = CARTESIAN_POINT ( 'NONE',  ( 7.084665262690076126, 7.022018677488170546, -10.88017736071110164 ) ) ;
#34188 = CARTESIAN_POINT ( 'NONE',  ( -0.3289641300567998083, 68.07879003517447813, 5.963430220938281678 ) ) ;
#34189 = DIRECTION ( 'NONE',  ( 1.000000000000000000, 0.000000000000000000, 0.000000000000000000 ) ) ;
#34190 = CARTESIAN_POINT ( 'NONE',  ( 19.42250999205614548, 65.98035201082151957, -5.440088680355545492 ) ) ;
#34191 = CARTESIAN_POINT ( 'NONE',  ( 17.20831665107776587, 29.13393115100078390, -7.208316651077762316 ) ) ;
#34192 = CARTESIAN_POINT ( 'NONE',  ( 3.469446951953614189E-15, -37.74106884899921255, 9.846743663894594434 ) ) ;
#34193 = ORIENTED_EDGE ( 'NONE', *, *, #48499, .T. ) ;
#34194 = CARTESIAN_POINT ( 'NONE',  ( 15.00000000000000000, 0.000000000000000000, -6.000000000000000000 ) ) ;
#34195 = EDGE_LOOP ( 'NONE', ( #81072, #90169, #49004, #32955, #23681, #20579 ) ) ;
#34196 = CARTESIAN_POINT ( 'NONE',  ( 2.791683348922240793, 26.63393115100078745, 7.208316651077764092 ) ) ;
#34197 = EDGE_LOOP ( 'NONE', ( #68514, #63608, #23184, #82740, #37807, #4793 ) ) ;
#34198 = CARTESIAN_POINT ( 'NONE',  ( 17.08211943468705130, 28.47041550158063572, 12.26659068614894998 ) ) ;
#34199 = CARTESIAN_POINT ( 'NONE',  ( 12.63842701281683034, 37.46726448433411605, 9.846743663894596210 ) ) ;
#34200 = CARTESIAN_POINT ( 'NONE',  ( 19.42250999205614193, 55.14701867748817676, 5.440088680355555262 ) ) ;
#34201 = PRESENTATION_STYLE_ASSIGNMENT (( #33228 ) ) ;
#34202 = CARTESIAN_POINT ( 'NONE',  ( 2.035157376598824452, 58.68868534415482685, 7.964842623401179544 ) ) ;
#34203 = ADVANCED_FACE ( 'NONE', ( #18551 ), #11047, .T. ) ;
#34204 = CARTESIAN_POINT ( 'NONE',  ( 5.076628168052704559, 40.17559781766745175, -8.527530157486179263 ) ) ;
#34205 = VECTOR ( 'NONE', #95999, 1000.000000000000000 ) ;
#34206 = CARTESIAN_POINT ( 'NONE',  ( 22.81628187352647785, 61.41530133659709634, 3.434112377981063169 ) ) ;
#34207 = CARTESIAN_POINT ( 'NONE',  ( -3.434112377981047626, 5.165301336597089232, 12.81628187352647963 ) ) ;
#34208 = EDGE_CURVE ( 'NONE', #73831, #16571, #10366, .T. ) ;
#34209 = ORIENTED_EDGE ( 'NONE', *, *, #44488, .F. ) ;
#34210 = CARTESIAN_POINT ( 'NONE',  ( -4.164238869374098151, 26.59541550158063217, -3.795296366450310543 ) ) ;
#34211 = VERTEX_POINT ( 'NONE', #73875 ) ;
#34212 = CARTESIAN_POINT ( 'NONE',  ( 21.09922568453595559, 32.04030133659708923, -6.408140936763230044 ) ) ;
#34213 = CARTESIAN_POINT ( 'NONE',  ( 10.00000000000000000, 24.75893115100078745, -9.846743663894594434 ) ) ;
#34214 = CARTESIAN_POINT ( 'NONE',  ( 17.96484262340118221, 4.938685344154837509, 7.964842623401181321 ) ) ;
#34215 = CARTESIAN_POINT ( 'NONE',  ( 17.20831665107776587, 29.13393115100078390, -7.208316651077762316 ) ) ;
#34216 = CARTESIAN_POINT ( 'NONE',  ( 9.997910040112534702, 4.470079180682592273E-16, 10.50199004140724490 ) ) ;
#34217 = CARTESIAN_POINT ( 'NONE',  ( -0.8801773607111008646, 68.27201867748817676, 2.915334737309923430 ) ) ;
#34218 = CARTESIAN_POINT ( 'NONE',  ( -45.94000000000001194, 103.9981609152045507, 5.961202730336935041 ) ) ;
#34219 = EDGE_CURVE ( 'NONE', #86126, #14329, #58873, .T. ) ;
#34220 = CARTESIAN_POINT ( 'NONE',  ( 1.707155281725210916, 2.901890803972826394, 6.499999999999999112 ) ) ;
#34221 = CARTESIAN_POINT ( 'NONE',  ( 19.84674366389459266, 3.717264484334118713, -2.638427012816827677 ) ) ;
#34222 = CARTESIAN_POINT ( 'NONE',  ( 22.81628187352647785, 26.41530133659708923, 3.434112377981063169 ) ) ;
#34223 = CARTESIAN_POINT ( 'NONE',  ( 3.193136578977092466, 6.674619624363884700E-16, -14.27383009353652277 ) ) ;
#34224 = CARTESIAN_POINT ( 'NONE',  ( 1.472469842513823179, 40.59226448433411605, -4.923371831947296329 ) ) ;
#34225 = CARTESIAN_POINT ( 'NONE',  ( -2.816281873526471635, 63.91530133659708923, -3.434112377981056508 ) ) ;
#34226 = CARTESIAN_POINT ( 'NONE',  ( 17.08211943468705130, 23.47041550158063572, 12.26659068614894998 ) ) ;
#34227 = CARTESIAN_POINT ( 'NONE',  ( 18.52753015748618282, 33.92559781766745886, -4.923371831947291888 ) ) ;
#34228 = CARTESIAN_POINT ( 'NONE',  ( 22.81628187352647785, 31.62363466993042138, 6.195893100308588602E-16 ) ) ;
#34230 = CYLINDRICAL_SURFACE ( 'NONE', #59267, 0.5000000000000004441 ) ;
#34229 = LINE ( 'NONE', #27233, #46868 ) ;
#34231 = CARTESIAN_POINT ( 'NONE',  ( 10.00000000000000000, 56.81368534415484106, -10.88017736071110342 ) ) ;
#34232 = CARTESIAN_POINT ( 'NONE',  ( -2.816281873526471635, 8.915301336597083903, -3.434112377981056508 ) ) ;
#34233 = PLANE ( 'NONE',  #90241 ) ;
#34234 = AXIS2_PLACEMENT_3D ( 'NONE', #39754, #31736, #93224 ) ;
#34235 = CARTESIAN_POINT ( 'NONE',  ( 7.361572987183169658, 29.96726448433411960, -9.846743663894592657 ) ) ;
#34236 = CARTESIAN_POINT ( 'NONE',  ( -0.8801773607111008646, 23.27201867748817676, 2.915334737309923430 ) ) ;
#34237 = CARTESIAN_POINT ( 'NONE',  ( 3.591859063236761518, 24.95696800326375353, 11.09922568453594849 ) ) ;
#34238 = CARTESIAN_POINT ( 'NONE',  ( 14.92337183194729633, 17.67559781766745175, 8.527530157486181039 ) ) ;
#34239 = DIRECTION ( 'NONE',  ( 0.000000000000000000, 0.000000000000000000, 1.000000000000000000 ) ) ;
#34240 = DIRECTION ( 'NONE',  ( -1.000000000000000000, -2.107602052970794797E-16, 0.000000000000000000 ) ) ;
#34241 = CARTESIAN_POINT ( 'NONE',  ( 12.91533473730992121, 34.52201867748817676, 10.88017736071110164 ) ) ;
#34242 = CARTESIAN_POINT ( 'NONE',  ( 19.42250999205614548, 65.98035201082151957, -5.440088680355545492 ) ) ;
#34243 = CARTESIAN_POINT ( 'NONE',  ( 4.559911319644449179, 7.230352010821504471, -9.422509992056141925 ) ) ;
#34245 = CARTESIAN_POINT ( 'NONE',  ( 0.5774900079438590739, 32.64701867748816966, -5.440088680355550821 ) ) ;
#34244 = CARTESIAN_POINT ( 'NONE',  ( 7.361572987183170547, 42.05059781766745886, 9.846743663894590881 ) ) ;
#34246 = DIRECTION ( 'NONE',  ( 0.000000000000000000, 0.000000000000000000, 1.000000000000000000 ) ) ;
#34247 = CARTESIAN_POINT ( 'NONE',  ( 19.42250999205614193, 50.14701867748817676, 5.440088680355555262 ) ) ;
#34249 = CARTESIAN_POINT ( 'NONE',  ( -0.000000000000000000, 74.64896322088237923, -5.938123570160299458 ) ) ;
#34248 = CARTESIAN_POINT ( 'NONE',  ( 2.035157376598822676, 12.43868534415483751, -7.964842623401177768 ) ) ;
#34250 = CARTESIAN_POINT ( 'NONE',  ( 14.92337183194729988, 4.342264484334117824, -8.527530157486177487 ) ) ;
#34251 = CARTESIAN_POINT ( 'NONE',  ( 5.076628168052704559, 50.17559781766745886, -8.527530157486179263 ) ) ;
#34253 = CARTESIAN_POINT ( 'NONE',  ( 6.034179729230694456, -36.06068107361731023, 3.750000000000000888 ) ) ;
#34252 = CARTESIAN_POINT ( 'NONE',  ( 13.79529636645030344, 48.26208216824728936, 14.16423886937410614 ) ) ;
#34254 = CARTESIAN_POINT ( 'NONE',  ( 14.17193700899790265, 15.00000000000000000, -1.489530601564018175 ) ) ;
#34255 = PRESENTATION_STYLE_ASSIGNMENT (( #63289 ) ) ;
#34256 = CARTESIAN_POINT ( 'NONE',  ( 24.16423886937410614, 34.30374883491396787, 8.672049930838204340E-16 ) ) ;
#34257 = CARTESIAN_POINT ( 'NONE',  ( 15.55000000000000071, 99.99999999999998579, -8.525133428036873795 ) ) ;
#34258 = ORIENTED_EDGE ( 'NONE', *, *, #3234, .T. ) ;
#34259 =( GEOMETRIC_REPRESENTATION_CONTEXT ( 3 ) GLOBAL_UNCERTAINTY_ASSIGNED_CONTEXT ( ( #19502 ) ) GLOBAL_UNIT_ASSIGNED_CONTEXT ( ( #89351, #81836, #97365 ) ) REPRESENTATION_CONTEXT ( 'NONE', 'WORKASPACE' ) );
#34260 = CARTESIAN_POINT ( 'NONE',  ( 2.917880565312950480, 65.97041550158063217, -12.26659068614894821 ) ) ;
#34261 = CARTESIAN_POINT ( 'NONE',  ( 18.52753015748617571, 38.09226448433412315, 4.923371831947298993 ) ) ;
#34263 =( NAMED_UNIT ( * ) SI_UNIT ( $, .STERADIAN. ) SOLID_ANGLE_UNIT ( ) );
#34262 = CARTESIAN_POINT ( 'NONE',  ( 2.241241388159942801E-47, 3.851859888774471706E-31, -7.000000000000000000 ) ) ;
#34264 = CARTESIAN_POINT ( 'NONE',  ( -0.8801773607111009756, 53.06368534415484106, 1.068504757029289695E-15 ) ) ;
#34265 = CARTESIAN_POINT ( 'NONE',  ( 6.565887622018943937, 60.16530133659707502, 12.81628187352647430 ) ) ;
#34266 = CARTESIAN_POINT ( 'NONE',  ( 0.5774900079438590739, 37.64701867748817676, -5.440088680355550821 ) ) ;
#34267 = CARTESIAN_POINT ( 'NONE',  ( 22.81628187352648496, 56.83196800326374643, -3.434112377981050290 ) ) ;
#34268 = CARTESIAN_POINT ( 'NONE',  ( 22.81628187352647785, 6.623634669930420493, 6.195893100308588602E-16 ) ) ;
#34269 = CARTESIAN_POINT ( 'NONE',  ( 18.52753015748618282, 8.925597817667451750, -4.923371831947291888 ) ) ;
#34270 = VERTEX_POINT ( 'NONE', #56065 ) ;
#34271 =( GEOMETRIC_REPRESENTATION_CONTEXT ( 3 ) GLOBAL_UNCERTAINTY_ASSIGNED_CONTEXT ( ( #56523 ) ) GLOBAL_UNIT_ASSIGNED_CONTEXT ( ( #17464, #24968, #8473 ) ) REPRESENTATION_CONTEXT ( 'NONE', 'WORKASPACE' ) );
#34272 = CARTESIAN_POINT ( 'NONE',  ( -0.3689425029237881626, 62.42874883491396787, 10.36894250292379027 ) ) ;
#34273 = CARTESIAN_POINT ( 'NONE',  ( 6.204703633549690345, 30.76208216824730357, -14.16423886937410259 ) ) ;
#34274 = CARTESIAN_POINT ( 'NONE',  ( 10.00000000000000000, 26.81368534415484106, -10.88017736071110342 ) ) ;
#34275 = CARTESIAN_POINT ( 'NONE',  ( 17.96484262340118221, 49.93868534415484106, 7.964842623401181321 ) ) ;
#34276 = PLANE ( 'NONE',  #55948 ) ;
#34277 = CARTESIAN_POINT ( 'NONE',  ( 14.99999999999998046, 69.99999999999998579, 4.000000000000000000 ) ) ;
#34278 = CARTESIAN_POINT ( 'NONE',  ( 10.00000000000000000, 4.758931151000784787, -9.846743663894594434 ) ) ;
#34279 = SURFACE_STYLE_USAGE ( .BOTH. , #66774 ) ;
#34280 = CARTESIAN_POINT ( 'NONE',  ( 0.000000000000000000, 15.00000000000000000, 0.000000000000000000 ) ) ;
#34281 = CARTESIAN_POINT ( 'NONE',  ( -46.58925734348296999, 101.6427229076536491, 8.029849069859604782 ) ) ;
#34282 = CARTESIAN_POINT ( 'NONE',  ( 2.791683348922237240, 25.38393115100078390, -7.208316651077763204 ) ) ;
#34283 = CARTESIAN_POINT ( 'NONE',  ( 12.63842701281683922, 44.55059781766745175, -9.846743663894590881 ) ) ;
#34284 = EDGE_CURVE ( 'NONE', #25669, #58411, #48046, .T. ) ;
#34285 = CARTESIAN_POINT ( 'NONE',  ( -0.8801773607111008646, 28.27201867748817321, 2.915334737309923430 ) ) ;
#34286 = UNCERTAINTY_MEASURE_WITH_UNIT (LENGTH_MEASURE( 1.000000000000000082E-05 ), #74458, 'distance_accuracy_value', 'NONE');
#34287 = CARTESIAN_POINT ( 'NONE',  ( 13.43411237798105340, 45.58196800326374643, 12.81628187352647963 ) ) ;
#34288 = AXIS2_PLACEMENT_3D ( 'NONE', #29247, #59247, #82245 ) ;
#34289 = DIRECTION ( 'NONE',  ( 0.000000000000000000, 1.000000000000000000, 0.000000000000000000 ) ) ;
#34290 = ADVANCED_FACE ( 'NONE', ( #29846, #36378 ), #91845, .F. ) ;
#34291 = CARTESIAN_POINT ( 'NONE',  ( 19.42250999205614193, 60.14701867748817676, 5.440088680355555262 ) ) ;
#34292 = CARTESIAN_POINT ( 'NONE',  ( 14.92337183194729988, 24.34226448433411960, -8.527530157486177487 ) ) ;
#34294 = CARTESIAN_POINT ( 'NONE',  ( 17.20831665107776587, 19.13393115100078035, -7.208316651077762316 ) ) ;
#34293 = CARTESIAN_POINT ( 'NONE',  ( 22.26659068614894466, 53.88708216824731068, 7.082119434687054849 ) ) ;
#34295 = DIRECTION ( 'NONE',  ( -0.000000000000000000, -1.000000000000000000, -0.000000000000000000 ) ) ;
#34296 = CYLINDRICAL_SURFACE ( 'NONE', #18373, 0.2500000000000002220 ) ;
#34297 = CARTESIAN_POINT ( 'NONE',  ( 6.204703633549690345, 10.76208216824729824, -14.16423886937410259 ) ) ;
#34298 = CARTESIAN_POINT ( 'NONE',  ( 17.08211943468705130, 28.47041550158063572, 12.26659068614894998 ) ) ;
#34299 = CARTESIAN_POINT ( 'NONE',  ( 14.92337183194729988, 29.34226448433411960, -8.527530157486177487 ) ) ;
#34300 = CARTESIAN_POINT ( 'NONE',  ( 18.39792806157249672, 9.522241923386404849, 6.499999999999995559 ) ) ;
#34301 = CARTESIAN_POINT ( 'NONE',  ( 17.96484262340118221, 24.93868534415484461, 7.964842623401181321 ) ) ;
#34302 = CARTESIAN_POINT ( 'NONE',  ( 2.035157376598824452, 63.68868534415484106, 7.964842623401179544 ) ) ;
#34303 = DIRECTION ( 'NONE',  ( 0.000000000000000000, 1.000000000000000000, 0.000000000000000000 ) ) ;
#34304 = ORIENTED_EDGE ( 'NONE', *, *, #40653, .F. ) ;
#34305 = CARTESIAN_POINT ( 'NONE',  ( -2.816281873526471635, 38.91530133659708213, -3.434112377981056508 ) ) ;
#34306 = CARTESIAN_POINT ( 'NONE',  ( 4.559911319644449179, 57.23035201082150536, -9.422509992056141925 ) ) ;
#34307 = ORIENTED_EDGE ( 'NONE', *, *, #51780, .F. ) ;
#34308 = CIRCLE ( 'NONE', #42261, 14.49999999999999822 ) ;
#34309 =( LENGTH_UNIT ( ) NAMED_UNIT ( * ) SI_UNIT ( .MILLI., .METRE. ) );
#34310 = CARTESIAN_POINT ( 'NONE',  ( 10.00000000000000178, 64.31368534415483396, 10.88017736071110342 ) ) ;
#34311 = ORIENTED_EDGE ( 'NONE', *, *, #30810, .F. ) ;
#34312 = CARTESIAN_POINT ( 'NONE',  ( 7.084665262690076126, 62.02201867748816966, -10.88017736071110164 ) ) ;
#34313 = CARTESIAN_POINT ( 'NONE',  ( 13.82671409943296226, -0.03417435944610275333, -3.447387012295225261 ) ) ;
#34314 = ADVANCED_FACE ( 'NONE', ( #13879 ), #24149, .T. ) ;
#34315 = CARTESIAN_POINT ( 'NONE',  ( 2.603489959281588106, 1.582109641433292690, 6.500000000000000888 ) ) ;
#34316 = CARTESIAN_POINT ( 'NONE',  ( 0.000000000000000000, -97.00000000000000000, 4.000000000000000000 ) ) ;
#34317 = CARTESIAN_POINT ( 'NONE',  ( 7.084665262690076126, 12.02201867748817321, -10.88017736071110164 ) ) ;
#34318 = CARTESIAN_POINT ( 'NONE',  ( 10.00000000000000178, 7.258931151000785675, 9.846743663894594434 ) ) ;
#34319 = CARTESIAN_POINT ( 'NONE',  ( 2.917880565312950480, 20.97041550158063217, -12.26659068614894821 ) ) ;
#34320 = CARTESIAN_POINT ( 'NONE',  ( 7.361572987183170547, 7.050597817667451750, 9.846743663894590881 ) ) ;
#34321 = EDGE_CURVE ( 'NONE', #79527, #17231, #28899, .T. ) ;
#34322 = CARTESIAN_POINT ( 'NONE',  ( -0.8801773607111008646, 23.27201867748817676, 2.915334737309923430 ) ) ;
#34323 = CARTESIAN_POINT ( 'NONE',  ( 19.84674366389459266, 53.71726448433411605, -2.638427012816827677 ) ) ;
#34324 = EDGE_LOOP ( 'NONE', ( #30289, #72320, #51081, #20442, #39287, #54113 ) ) ;
#34325 = B_SPLINE_CURVE_WITH_KNOTS ( 'NONE', 3,
 ( #90474, #52971, #28984, #73997, #29472, #51502 ),
 .UNSPECIFIED., .F., .F.,
 ( 4, 2, 4 ),
 ( 0.0002800245631527670145, 0.0006862300328564149843, 0.001092435502560062900 ),
 .UNSPECIFIED. ) ;
#34326 = CARTESIAN_POINT ( 'NONE',  ( 2.791683348922240793, 66.63393115100079456, 7.208316651077764092 ) ) ;
#34327 = VERTEX_POINT ( 'NONE', #29353 ) ;
#34328 = LINE ( 'NONE', #32866, #20622 ) ;
#34329 = VECTOR ( 'NONE', #23811, 1000.000000000000000 ) ;
#34330 = CARTESIAN_POINT ( 'NONE',  ( 10.00000000000000000, 56.81368534415484106, -10.88017736071110342 ) ) ;
#34331 = CARTESIAN_POINT ( 'NONE',  ( 7.361572987183169658, 54.96726448433413026, -9.846743663894592657 ) ) ;
#34332 = CARTESIAN_POINT ( 'NONE',  ( -1.099225684535947600, 38.70696800326375353, -6.408140936763238038 ) ) ;
#34334 = CARTESIAN_POINT ( 'NONE',  ( 6.879999999999995453, 70.25000000000000000, -6.500000000000000888 ) ) ;
#34333 = CARTESIAN_POINT ( 'NONE',  ( 20.88017736071110519, 10.56368534415483751, 2.639326808657452039E-16 ) ) ;
#34335 = CARTESIAN_POINT ( 'NONE',  ( 15.44008868035555260, 64.73035201082151957, 9.422509992056143702 ) ) ;
#34336 = CARTESIAN_POINT ( 'NONE',  ( -4.164238869374099039, 66.80374883491396076, 8.674139862899312516E-16 ) ) ;
#34337 = CARTESIAN_POINT ( 'NONE',  ( -0.8801773607111009756, 53.06368534415484106, 1.068504757029289695E-15 ) ) ;
#34338 = CARTESIAN_POINT ( 'NONE',  ( -1.099225684535947600, 38.70696800326375353, -6.408140936763238038 ) ) ;
#34339 = CARTESIAN_POINT ( 'NONE',  ( 20.88017736071110164, 35.35535201082150536, 2.915334737309930979 ) ) ;
#34340 = DIRECTION ( 'NONE',  ( 0.000000000000000000, 0.000000000000000000, -1.000000000000000000 ) ) ;
#34341 = ORIENTED_EDGE ( 'NONE', *, *, #16959, .F. ) ;
#34342 = AXIS2_PLACEMENT_3D ( 'NONE', #37350, #74829, #27847 ) ;
#34343 = CARTESIAN_POINT ( 'NONE',  ( 21.09922568453595559, 37.04030133659708923, -6.408140936763230044 ) ) ;
#34344 = CARTESIAN_POINT ( 'NONE',  ( 19.42250999205614193, 40.14701867748817676, 5.440088680355555262 ) ) ;
#34345 = ORIENTED_EDGE ( 'NONE', *, *, #76004, .F. ) ;
#34346 = DIRECTION ( 'NONE',  ( 0.000000000000000000, 0.000000000000000000, 1.000000000000000000 ) ) ;
#34347 = DIRECTION ( 'NONE',  ( -0.000000000000000000, 1.000000000000000000, -0.000000000000000000 ) ) ;
#34348 = EDGE_CURVE ( 'NONE', #23697, #73387, #22373, .T. ) ;
#34349 =( BOUNDED_CURVE ( )  B_SPLINE_CURVE ( 2, ( #35804, #5808, #66796, #42326, #19812, #41847, #72313, #72800, #81305 ),
 .UNSPECIFIED., .F., .T. ) 
 B_SPLINE_CURVE_WITH_KNOTS ( ( 3, 2, 2, 2, 3 ),
 ( 0.7953713073319822469, 0.7976190476190476719, 0.8035714285714286031, 0.8095238095238095344, 0.8117715498108749594 ),
 .UNSPECIFIED. ) 
 CURVE ( )  GEOMETRIC_REPRESENTATION_ITEM ( )  RATIONAL_B_SPLINE_CURVE ( ( 0.9839835555609424134, 0.9871328979762477029, 1.000000000000000000, 0.9659258262890683122, 1.000000000000000000, 0.9659258262890683122, 1.000000000000000000, 0.9871328979762474809, 0.9839835555609424134 ) ) 
 REPRESENTATION_ITEM ( '' )  );
#34350 = CARTESIAN_POINT ( 'NONE',  ( 2.791683348922240793, 56.63393115100078035, 7.208316651077764092 ) ) ;
#34352 = CARTESIAN_POINT ( 'NONE',  ( 7.361572987183170547, 52.05059781766745175, 9.846743663894590881 ) ) ;
#34351 = LINE ( 'NONE', #64842, #524 ) ;
#34353 = CARTESIAN_POINT ( 'NONE',  ( -0.8801773607111008646, 28.27201867748817321, 2.915334737309923430 ) ) ;
#34354 = DIRECTION ( 'NONE',  ( 0.000000000000000000, 0.000000000000000000, 1.000000000000000000 ) ) ;
#34355 = CARTESIAN_POINT ( 'NONE',  ( 0.1532563361054083140, 41.00893115100078745, 1.131784320476157264E-15 ) ) ;
#34356 = CARTESIAN_POINT ( 'NONE',  ( 1.379999999999981908, 20.99999999999999645, 0.000000000000000000 ) ) ;
#34357 = LINE ( 'NONE', #55905, #88367 ) ;
#34358 = EDGE_CURVE ( 'NONE', #16203, #32248, #3376, .T. ) ;
#34360 = CARTESIAN_POINT ( 'NONE',  ( 18.52753015748617571, 13.09226448433411960, 4.923371831947298993 ) ) ;
#34359 = CARTESIAN_POINT ( 'NONE',  ( 10.00000000000000000, 24.75893115100078745, -9.846743663894594434 ) ) ;
#34361 = CARTESIAN_POINT ( 'NONE',  ( 5.361923921558569894, 0.000000000000000000, 0.9937738586172348842 ) ) ;
#34363 = ORIENTED_EDGE ( 'NONE', *, *, #69233, .T. ) ;
#34362 = CARTESIAN_POINT ( 'NONE',  ( 17.20831665107776587, 62.88393115100078745, 7.208316651077764980 ) ) ;
#34364 = FACE_OUTER_BOUND ( 'NONE', #36612, .T. ) ;
#34365 = CARTESIAN_POINT ( 'NONE',  ( 0.6178305044545838731, 44.74863466993042493, 9.382169495545420901 ) ) ;
#34366 = CIRCLE ( 'NONE', #47144, 0.2499999999999997224 ) ;
#34367 = CARTESIAN_POINT ( 'NONE',  ( 2.791683348922237240, 40.38393115100078035, -7.208316651077763204 ) ) ;
#34368 = SURFACE_STYLE_FILL_AREA ( #13354 ) ;
#34369 = CARTESIAN_POINT ( 'NONE',  ( 24.16423886937409904, 64.09541550158064638, 3.795296366450317205 ) ) ;
#34370 = CARTESIAN_POINT ( 'NONE',  ( 7.361572987183169658, 14.96726448433411960, -9.846743663894592657 ) ) ;
#34371 = CARTESIAN_POINT ( 'NONE',  ( 20.00000000000000711, 89.81050759285638208, 4.994480956907769276 ) ) ;
#34372 = CARTESIAN_POINT ( 'NONE',  ( 2.917880565312950480, 50.97041550158064638, -12.26659068614894821 ) ) ;
#34373 = CARTESIAN_POINT ( 'NONE',  ( 0.1532563361054082862, 61.21726448433412315, 2.638427012816831674 ) ) ;
#34374 = CARTESIAN_POINT ( 'NONE',  ( 7.084665262690076126, 2.022018677488171434, -10.88017736071110164 ) ) ;
#34375 = CARTESIAN_POINT ( 'NONE',  ( 17.08211943468705840, 30.13708216824730357, -12.26659068614894466 ) ) ;
#34377 = CARTESIAN_POINT ( 'NONE',  ( -43.18635350015717478, 107.2769236248421549, -4.500000000000000888 ) ) ;
#34376 = CARTESIAN_POINT ( 'NONE',  ( 13.79529636645030344, 38.26208216824729647, 14.16423886937410614 ) ) ;
#34378 = CARTESIAN_POINT ( 'NONE',  ( 5.129999999999990123, 76.07179676972444327, -6.250000000000000000 ) ) ;
#34380 = CARTESIAN_POINT ( 'NONE',  ( 0.1532563361054083140, 61.00893115100078745, 1.131784320476157264E-15 ) ) ;
#34379 = CARTESIAN_POINT ( 'NONE',  ( 3.640395162852214650, 107.5383484153110061, 5.000000000000000000 ) ) ;
#34381 = ORIENTED_EDGE ( 'NONE', *, *, #18509, .F. ) ;
#34382 = CARTESIAN_POINT ( 'NONE',  ( 19.42250999205614548, 55.98035201082150536, -5.440088680355545492 ) ) ;
#34383 = AXIS2_PLACEMENT_3D ( 'NONE', #17539, #92526, #78514 ) ;
#34384 = CARTESIAN_POINT ( 'NONE',  ( 19.54820696779682976, 96.99593637789192258, -5.000000000000000000 ) ) ;
#34385 = CARTESIAN_POINT ( 'NONE',  ( 10.00000000000000178, 65.37363466993042493, 12.81628187352647608 ) ) ;
#34386 = CARTESIAN_POINT ( 'NONE',  ( 19.84674366389459266, 58.71726448433411605, -2.638427012816827677 ) ) ;
#34387 = CARTESIAN_POINT ( 'NONE',  ( -0.1556627343491930049, 2.117582368135750848E-16, 14.62580308442190713 ) ) ;
#34388 = ORIENTED_EDGE ( 'NONE', *, *, #91431, .F. ) ;
#34389 = AXIS2_PLACEMENT_3D ( 'NONE', #23750, #84248, #22754 ) ;
#34390 = CARTESIAN_POINT ( 'NONE',  ( -0.3689425029237881626, 22.42874883491397142, 10.36894250292379027 ) ) ;
#34391 = CARTESIAN_POINT ( 'NONE',  ( -14.22901244993679448, 15.00000000000000888, -3.387263120971507835 ) ) ;
#34393 = CARTESIAN_POINT ( 'NONE',  ( -6.382347221874291598, 14.49999999999999112, -13.57444820018240783 ) ) ;
#34392 = CARTESIAN_POINT ( 'NONE',  ( -4.818768077841676600, -24.96217769842146694, -2.500000000000000000 ) ) ;
#34394 = CARTESIAN_POINT ( 'NONE',  ( 0.5774900079438607392, 13.48035201082150358, 5.440088680355550821 ) ) ;
#34395 = CARTESIAN_POINT ( 'NONE',  ( -2.816281873526471635, 28.91530133659708213, -3.434112377981056508 ) ) ;
#34396 = CARTESIAN_POINT ( 'NONE',  ( 12.63842701281683922, 14.55059781766744997, -9.846743663894590881 ) ) ;
#34397 = CARTESIAN_POINT ( 'NONE',  ( 21.09922568453594849, 46.20696800326376064, 6.408140936763242479 ) ) ;
#34398 = ORIENTED_EDGE ( 'NONE', *, *, #17197, .T. ) ;
#34399 = CARTESIAN_POINT ( 'NONE',  ( 6.757940885659567520, -58.32678904743372073, -3.999999999999999556 ) ) ;
#34400 = CARTESIAN_POINT ( 'NONE',  ( -0.3689425029237881626, 22.42874883491397142, 10.36894250292379027 ) ) ;
#34401 = CARTESIAN_POINT ( 'NONE',  ( 20.15039907845753220, 61.74884699246888431, 6.262539305110078836 ) ) ;
#34402 = CARTESIAN_POINT ( 'NONE',  ( 20.88017736071110519, 10.56368534415483929, 2.639326808657452039E-16 ) ) ;
#34403 = LINE ( 'NONE', #50401, #44790 ) ;
#34404 = CARTESIAN_POINT ( 'NONE',  ( 19.42250999205614548, 35.98035201082151247, -5.440088680355545492 ) ) ;
#34405 = CARTESIAN_POINT ( 'NONE',  ( 12.91533473730992121, 39.52201867748817676, 10.88017736071110164 ) ) ;
#34406 = CARTESIAN_POINT ( 'NONE',  ( 3.591859063236763294, 18.29030133659708568, -11.09922568453595026 ) ) ;
#34407 = DIRECTION ( 'NONE',  ( -0.000000000000000000, 1.000000000000000000, -0.000000000000000000 ) ) ;
#34408 = DIRECTION ( 'NONE',  ( -0.000000000000000000, -0.000000000000000000, -1.000000000000000000 ) ) ;
#34409 = CARTESIAN_POINT ( 'NONE',  ( 2.791683348922237240, 15.38393115100078212, -7.208316651077763204 ) ) ;
#34410 = ORIENTED_EDGE ( 'NONE', *, *, #76121, .T. ) ;
#34411 = FILL_AREA_STYLE_COLOUR ( '', #82816 ) ;
#34412 = CARTESIAN_POINT ( 'NONE',  ( -0.8801773607110991993, 37.85535201082151247, -2.915334737309923874 ) ) ;
#34413 = EDGE_CURVE ( 'NONE', #42198, #19862, #7862, .T. ) ;
#34414 = VECTOR ( 'NONE', #11085, 1000.000000000000114 ) ;
#34415 = UNCERTAINTY_MEASURE_WITH_UNIT (LENGTH_MEASURE( 1.000000000000000082E-05 ), #44707, 'distance_accuracy_value', 'NONE');
#34416 = CARTESIAN_POINT ( 'NONE',  ( 10.00000000000000178, 5.373634669930420493, 12.81628187352647608 ) ) ;
#34417 = CARTESIAN_POINT ( 'NONE',  ( 10.00000000000000000, 61.81368534415484106, -10.88017736071110342 ) ) ;
#34418 = AXIS2_PLACEMENT_3D ( 'NONE', #93453, #92462, #38989 ) ;
#34419 = CARTESIAN_POINT ( 'NONE',  ( 10.00000000000000000, 24.75893115100078745, -9.846743663894594434 ) ) ;
#34420 = CARTESIAN_POINT ( 'NONE',  ( 16.40814093676323893, 45.79030133659708923, 11.09922568453595026 ) ) ;
#34422 = CARTESIAN_POINT ( 'NONE',  ( 12.14357320772536575, 54.02013147999952736, 0.000000000000000000 ) ) ;
#34421 = CARTESIAN_POINT ( 'NONE',  ( 1.472469842513823179, 0.5922644843341181575, -4.923371831947296329 ) ) ;
#34423 = VERTEX_POINT ( 'NONE', #75353 ) ;
#34424 = CARTESIAN_POINT ( 'NONE',  ( 2.035157376598824452, 13.68868534415483751, 7.964842623401179544 ) ) ;
#34425 = CARTESIAN_POINT ( 'NONE',  ( 13.43411237798105340, 55.58196800326374643, 12.81628187352647963 ) ) ;
#34426 = CARTESIAN_POINT ( 'NONE',  ( 0.1532563361054082862, 26.21726448433411605, 2.638427012816831674 ) ) ;
#34427 = CARTESIAN_POINT ( 'NONE',  ( 19.42250999205614193, 25.14701867748817321, 5.440088680355555262 ) ) ;
#34428 = CARTESIAN_POINT ( 'NONE',  ( 2.035157376598822676, 2.438685344154838397, -7.964842623401177768 ) ) ;
#34429 = ORIENTED_EDGE ( 'NONE', *, *, #20593, .F. ) ;
#34430 = CARTESIAN_POINT ( 'NONE',  ( 20.88017736071110519, 15.56368534415483751, 2.639326808657452039E-16 ) ) ;
#34431 = CARTESIAN_POINT ( 'NONE',  ( 2.035157376598822676, 17.43868534415483751, -7.964842623401177768 ) ) ;
#34433 = CARTESIAN_POINT ( 'NONE',  ( 15.44008868035555793, 26.39701867748817321, -9.422509992056140149 ) ) ;
#34432 = DIRECTION ( 'NONE',  ( -0.000000000000000000, -1.000000000000000000, -0.000000000000000000 ) ) ;
#34434 = ORIENTED_EDGE ( 'NONE', *, *, #4119, .T. ) ;
#34435 = CARTESIAN_POINT ( 'NONE',  ( 1.472469842513823179, 65.59226448433412315, -4.923371831947296329 ) ) ;
#34436 = CARTESIAN_POINT ( 'NONE',  ( 12.91533473730993009, 26.60535201082150536, -10.88017736071109987 ) ) ;
#34437 = CARTESIAN_POINT ( 'NONE',  ( 17.20831665107776587, 54.13393115100079456, -7.208316651077762316 ) ) ;
#34438 = CIRCLE ( 'NONE', #82335, 3.940000000000000835 ) ;
#34439 = CARTESIAN_POINT ( 'NONE',  ( 3.969999999999999751, 37.00000000000000000, -2.500000000000000000 ) ) ;
#34440 = ADVANCED_FACE ( 'NONE', ( #28857 ), #62449, .T. ) ;
#34441 = CARTESIAN_POINT ( 'NONE',  ( 22.81628187352647785, 61.41530133659709634, 3.434112377981063169 ) ) ;
#34442 = DIRECTION ( 'NONE',  ( 0.000000000000000000, 1.000000000000000000, -0.000000000000000000 ) ) ;
#34443 = CARTESIAN_POINT ( 'NONE',  ( 6.204703633549690345, 30.76208216824730357, -14.16423886937410259 ) ) ;
#34444 = CARTESIAN_POINT ( 'NONE',  ( 7.084665262690076126, 37.02201867748817676, -10.88017736071110164 ) ) ;
#34445 = CARTESIAN_POINT ( 'NONE',  ( 0.5774900079438590739, 12.64701867748817321, -5.440088680355550821 ) ) ;
#34446 = CARTESIAN_POINT ( 'NONE',  ( 5.076628168052704559, 55.17559781766745175, -8.527530157486179263 ) ) ;
#34447 = CARTESIAN_POINT ( 'NONE',  ( 1.472469842513823179, 46.42559781766745175, 4.923371831947296329 ) ) ;
#34448 = EDGE_CURVE ( 'NONE', #55756, #80099, #68855, .T. ) ;
#34449 = CARTESIAN_POINT ( 'NONE',  ( 0.1916775849787266117, 22.25868815902069286, -6.499999999999991118 ) ) ;
#34450 = CARTESIAN_POINT ( 'NONE',  ( 12.63842701281683034, 7.467264484334118713, 9.846743663894596210 ) ) ;
#34451 = CARTESIAN_POINT ( 'NONE',  ( 12.81628187352647608, -28.58469866340290721, 3.434112377981052511 ) ) ;
#34452 = ORIENTED_EDGE ( 'NONE', *, *, #74844, .T. ) ;
#34453 = CARTESIAN_POINT ( 'NONE',  ( 17.96484262340118221, 11.18868534415483929, -7.964842623401177768 ) ) ;
#34454 = CARTESIAN_POINT ( 'NONE',  ( 7.361572987183170547, 7.050597817667451750, 9.846743663894590881 ) ) ;
#34455 = CARTESIAN_POINT ( 'NONE',  ( -2.816281873526471635, -1.084698663402913210, -3.434112377981056508 ) ) ;
#34457 = CARTESIAN_POINT ( 'NONE',  ( 19.42250999205614548, 50.98035201082151247, -5.440088680355545492 ) ) ;
#34456 = CARTESIAN_POINT ( 'NONE',  ( 20.88017736071110519, 65.56368534415483396, 2.639326808657452039E-16 ) ) ;
#34459 = CARTESIAN_POINT ( 'NONE',  ( 0.6178305044545818747, 63.49863466993043204, -9.382169495545419124 ) ) ;
#34458 = CARTESIAN_POINT ( 'NONE',  ( 19.42250999205614548, 20.98035201082150891, -5.440088680355545492 ) ) ;
#34460 = CARTESIAN_POINT ( 'NONE',  ( 10.00000000000000000, 30.55374883491397142, -14.16423886937410082 ) ) ;
#34461 = TOROIDAL_SURFACE ( 'NONE', #55158, 2.750000000000000888, 0.2500000000000000000 ) ;
#34462 = CARTESIAN_POINT ( 'NONE',  ( 20.32896413005680003, 11.77164270246084143, 5.963430220938287007 ) ) ;
#34463 = CARTESIAN_POINT ( 'NONE',  ( 19.38216949554541202, 55.99863466993041072, 9.382169495545424454 ) ) ;
#34464 = ORIENTED_EDGE ( 'NONE', *, *, #73798, .F. ) ;
#34465 = CARTESIAN_POINT ( 'NONE',  ( 16.40814093676324603, 2.456968003263753531, -11.09922568453594671 ) ) ;
#34466 = DIRECTION ( 'NONE',  ( 1.000000000000000000, 0.000000000000000000, 0.000000000000000000 ) ) ;
#34467 = CARTESIAN_POINT ( 'NONE',  ( 12.91533473730992121, 34.52201867748817676, 10.88017736071110164 ) ) ;
#34468 = CARTESIAN_POINT ( 'NONE',  ( 2.791683348922240793, 66.63393115100079456, 7.208316651077764092 ) ) ;
#34469 = VERTEX_POINT ( 'NONE', #89864 ) ;
#34470 = CARTESIAN_POINT ( 'NONE',  ( 0.1532563361054083140, 6.008931151000784787, 1.131784320476157264E-15 ) ) ;
#34471 = CARTESIAN_POINT ( 'NONE',  ( 1.472469842513823179, 10.59226448433411782, -4.923371831947296329 ) ) ;
#34472 = CARTESIAN_POINT ( 'NONE',  ( 14.92337183194729988, 19.34226448433411960, -8.527530157486177487 ) ) ;
#34473 = CARTESIAN_POINT ( 'NONE',  ( 5.076628168052704559, 10.17559781766745175, -8.527530157486179263 ) ) ;
#34474 = EDGE_CURVE ( 'NONE', #24437, #18090, #67366, .T. ) ;
#34476 = CARTESIAN_POINT ( 'NONE',  ( -4.838527690343711107, 0.3639308167276193995, 14.19819177887727157 ) ) ;
#34475 = CARTESIAN_POINT ( 'NONE',  ( 0.5774900079438590739, 57.64701867748817676, -5.440088680355550821 ) ) ;
#34477 = CARTESIAN_POINT ( 'NONE',  ( 0.5774900079438607392, 63.48035201082149825, 5.440088680355550821 ) ) ;
#34478 = VECTOR ( 'NONE', #64925, 1000.000000000000000 ) ;
#34480 = ORIENTED_EDGE ( 'NONE', *, *, #62201, .T. ) ;
#34479 = CARTESIAN_POINT ( 'NONE',  ( 10.00000000000000000, 14.75893115100078568, -9.846743663894594434 ) ) ;
#34481 = CARTESIAN_POINT ( 'NONE',  ( -9.011287250621867528, 0.2306972965111889207, 11.91783356064781607 ) ) ;
#34482 = CARTESIAN_POINT ( 'NONE',  ( 1.472469842513823179, 56.42559781766745886, 4.923371831947296329 ) ) ;
#34483 = VERTEX_POINT ( 'NONE', #60351 ) ;
#34484 = AXIS2_PLACEMENT_3D ( 'NONE', #84187, #21716, #38682 ) ;
#34485 = CARTESIAN_POINT ( 'NONE',  ( 13.79529636645031943, 25.34541550158063572, -14.16423886937409904 ) ) ;
#34486 = B_SPLINE_CURVE_WITH_KNOTS ( 'NONE', 3,
 ( #12554, #43537, #58537, #7034, #13541, #21050 ),
 .UNSPECIFIED., .F., .F.,
 ( 4, 2, 4 ),
 ( 0.000000000000000000, 0.0002701661927229383718, 0.0005403323854458767436 ),
 .UNSPECIFIED. ) ;
#34487 = UNCERTAINTY_MEASURE_WITH_UNIT (LENGTH_MEASURE( 1.000000000000000082E-05 ), #88319, 'distance_accuracy_value', 'NONE');
#34488 = CARTESIAN_POINT ( 'NONE',  ( 4.922013193295439848, 0.000000000000000000, -2.347679864819448348 ) ) ;
#34489 = CARTESIAN_POINT ( 'NONE',  ( 2.917880565312950480, 10.97041550158063572, -12.26659068614894821 ) ) ;
#34490 = CARTESIAN_POINT ( 'NONE',  ( 22.26659068614895176, 34.72041550158063927, -7.082119434687042414 ) ) ;
#34491 = FILL_AREA_STYLE ('',( #5005 ) ) ;
#34492 = CARTESIAN_POINT ( 'NONE',  ( -4.164238869374099039, 1.803748834913967647, 8.674139862899312516E-16 ) ) ;
#34493 = CARTESIAN_POINT ( 'NONE',  ( 20.88017736071110519, 40.56368534415484106, 2.639326808657452039E-16 ) ) ;
#34494 = EDGE_LOOP ( 'NONE', ( #92126, #95843, #96026, #22804 ) ) ;
#34495 = CARTESIAN_POINT ( 'NONE',  ( 1.472469842513823179, 16.42559781766745175, 4.923371831947296329 ) ) ;
#34497 = CARTESIAN_POINT ( 'NONE',  ( 19.84674366389459266, 18.71726448433411960, -2.638427012816827677 ) ) ;
#34496 = CARTESIAN_POINT ( 'NONE',  ( 7.084665262690076126, 59.10535201082150536, 10.88017736071109987 ) ) ;
#34498 = CARTESIAN_POINT ( 'NONE',  ( 7.084665262690076126, 14.10535201082150358, 10.88017736071109987 ) ) ;
#34499 = CARTESIAN_POINT ( 'NONE',  ( -2.816281873526473856, 44.12363466993042493, 9.499525473075851096E-16 ) ) ;
#34500 = CARTESIAN_POINT ( 'NONE',  ( 7.361572987183170547, 47.05059781766745175, 9.846743663894590881 ) ) ;
#34501 = CARTESIAN_POINT ( 'NONE',  ( -1.114591949025129258, 15.00000000000000000, 14.45709807627963706 ) ) ;
#34502 = CARTESIAN_POINT ( 'NONE',  ( 16.40814093676324603, 27.45696800326375708, -11.09922568453594671 ) ) ;
#34503 = CARTESIAN_POINT ( 'NONE',  ( -7.082119434687058401, -34.02958449841936073, -12.26659068614894110 ) ) ;
#34504 = CARTESIAN_POINT ( 'NONE',  ( 12.63842701281683922, 19.55059781766745175, -9.846743663894590881 ) ) ;
#34505 = CARTESIAN_POINT ( 'NONE',  ( 24.16423886937409904, 14.09541550158063217, 3.795296366450317205 ) ) ;
#34506 = ORIENTED_EDGE ( 'NONE', *, *, #94333, .F. ) ;
#34507 = ORIENTED_EDGE ( 'NONE', *, *, #88960, .F. ) ;
#34508 = CARTESIAN_POINT ( 'NONE',  ( 6.000000000000000000, 61.00000000000000711, 5.000000000000000000 ) ) ;
#34509 = CARTESIAN_POINT ( 'NONE',  ( 7.084665262690076126, 44.10535201082151247, 10.88017736071109987 ) ) ;
#34510 = CARTESIAN_POINT ( 'NONE',  ( 10.00000000000000000, 46.81368534415484106, -10.88017736071110342 ) ) ;
#34511 = CARTESIAN_POINT ( 'NONE',  ( 22.26659068614894466, 43.88708216824729647, 7.082119434687054849 ) ) ;
#34512 = CARTESIAN_POINT ( 'NONE',  ( 5.076628168052704559, 60.17559781766745175, -8.527530157486179263 ) ) ;
#34513 = CARTESIAN_POINT ( 'NONE',  ( 1.472469842513823179, 6.425597817667451750, 4.923371831947296329 ) ) ;
#34514 = CARTESIAN_POINT ( 'NONE',  ( -1.099225684535947600, 63.70696800326376774, -6.408140936763238038 ) ) ;
#34515 = CARTESIAN_POINT ( 'NONE',  ( 0.5774900079438590739, 47.64701867748817676, -5.440088680355550821 ) ) ;
#34516 = CARTESIAN_POINT ( 'NONE',  ( -6.732636091893173358, -88.11213685669363826, -2.500000000000000000 ) ) ;
#34517 = CARTESIAN_POINT ( 'NONE',  ( 19.84674366389459266, 58.71726448433411605, -2.638427012816827677 ) ) ;
#34518 = CARTESIAN_POINT ( 'NONE',  ( -9.422509992056136596, 18.48035201082151602, 5.440088680355559703 ) ) ;
#34519 = CARTESIAN_POINT ( 'NONE',  ( -0.8801773607111008646, 68.27201867748817676, 2.915334737309923430 ) ) ;
#34520 = AXIS2_PLACEMENT_3D ( 'NONE', #63069, #93569, #26072 ) ;
#34521 = PRESENTATION_STYLE_ASSIGNMENT (( #11543 ) ) ;
#34522 = EDGE_CURVE ( 'NONE', #63596, #18620, #51875, .T. ) ;
#34523 = CARTESIAN_POINT ( 'NONE',  ( 4.559911319644449179, 67.23035201082150536, -9.422509992056141925 ) ) ;
#34524 = CARTESIAN_POINT ( 'NONE',  ( 2.035157376598824452, 68.68868534415484817, 7.964842623401179544 ) ) ;
#34525 = CARTESIAN_POINT ( 'NONE',  ( 0.1532563361054100626, 30.80059781766744820, -2.638427012816831230 ) ) ;
#34526 = EDGE_CURVE ( 'NONE', #89588, #60892, #70468, .T. ) ;
#34527 = CARTESIAN_POINT ( 'NONE',  ( 19.42250999205614548, 20.98035201082150891, -5.440088680355545492 ) ) ;
#34528 =( GEOMETRIC_REPRESENTATION_CONTEXT ( 3 ) GLOBAL_UNCERTAINTY_ASSIGNED_CONTEXT ( ( #30105 ) ) GLOBAL_UNIT_ASSIGNED_CONTEXT ( ( #11867, #10888, #34849 ) ) REPRESENTATION_CONTEXT ( 'NONE', 'WORKASPACE' ) );
#34529 = CARTESIAN_POINT ( 'NONE',  ( 18.52753015748617571, 63.09226448433412315, 4.923371831947298993 ) ) ;
#34531 = CARTESIAN_POINT ( 'NONE',  ( 0.6081133539230650920, 13.33703382326400089, 6.500000000000005329 ) ) ;
#34530 = CARTESIAN_POINT ( 'NONE',  ( 20.88017736071110164, 35.35535201082150536, 2.915334737309930979 ) ) ;
#34532 = DIRECTION ( 'NONE',  ( 0.000000000000000000, 0.000000000000000000, 1.000000000000000000 ) ) ;
#34533 = CARTESIAN_POINT ( 'NONE',  ( 6.565887622018943937, 40.16530133659708923, 12.81628187352647430 ) ) ;
#34534 = EDGE_LOOP ( 'NONE', ( #24062, #26822, #19295, #14213 ) ) ;
#34535 = CARTESIAN_POINT ( 'NONE',  ( 19.42250999205614193, 45.14701867748817676, 5.440088680355555262 ) ) ;
#34537 = CARTESIAN_POINT ( 'NONE',  ( 20.10384461210892582, 51.74302437010795330, 6.337995344473751125 ) ) ;
#34536 = CARTESIAN_POINT ( 'NONE',  ( -1.099225684535947600, 18.70696800326375353, -6.408140936763238038 ) ) ;
#34538 = CARTESIAN_POINT ( 'NONE',  ( 14.92337183194729633, 2.675597817667451750, 8.527530157486181039 ) ) ;
#34539 = CARTESIAN_POINT ( 'NONE',  ( 20.88017736071110875, 30.77201867748816966, -2.915334737309920765 ) ) ;
#34540 = CARTESIAN_POINT ( 'NONE',  ( -4.164238869374099039, 61.80374883491397497, 8.674139862899312516E-16 ) ) ;
#34541 = CARTESIAN_POINT ( 'NONE',  ( 2.791683348922237240, 50.38393115100078035, -7.208316651077763204 ) ) ;
#34542 = CARTESIAN_POINT ( 'NONE',  ( -0.8801773607111009756, 68.06368534415484817, 1.068504757029289695E-15 ) ) ;
#34543 = CARTESIAN_POINT ( 'NONE',  ( 0.5774900079438590739, 62.64701867748817676, -5.440088680355550821 ) ) ;
#34544 = CARTESIAN_POINT ( 'NONE',  ( -9.402796353260987061, 14.49999999999999112, -11.68706210897776465 ) ) ;
#34545 = CARTESIAN_POINT ( 'NONE',  ( 6.204703633549690345, 32.84541550158063927, 14.16423886937410082 ) ) ;
#34546 = EDGE_CURVE ( 'NONE', #56832, #96185, #59856, .T. ) ;
#34547 = STYLED_ITEM ( 'NONE', ( #90225 ), #35455 ) ;
#34548 = CARTESIAN_POINT ( 'NONE',  ( 0.000000000000000000, 14.49999999999999822, 0.000000000000000000 ) ) ;
#34549 = CARTESIAN_POINT ( 'NONE',  ( -4.139459722423021404, -8.271751626981556527, -4.000000000000000888 ) ) ;
#34550 = VECTOR ( 'NONE', #7799, 999.9999999999998863 ) ;
#34551 = ORIENTED_EDGE ( 'NONE', *, *, #8255, .F. ) ;
#34552 = CARTESIAN_POINT ( 'NONE',  ( 24.16423886937409904, 49.09541550158063217, 3.795296366450317205 ) ) ;
#34553 = CARTESIAN_POINT ( 'NONE',  ( 22.26659068614895176, 44.72041550158063927, -7.082119434687042414 ) ) ;
#34554 = CARTESIAN_POINT ( 'NONE',  ( 14.92337183194729988, 14.34226448433411782, -8.527530157486177487 ) ) ;
#34555 = ADVANCED_FACE ( 'NONE', ( #69339 ), #16341, .T. ) ;
#34556 = CARTESIAN_POINT ( 'NONE',  ( 6.565887622018943937, 15.16530133659708568, 12.81628187352647430 ) ) ;
#34557 = CARTESIAN_POINT ( 'NONE',  ( 24.35999999999999233, 44.99999999999997158, 10.00000000000000000 ) ) ;
#34559 = CARTESIAN_POINT ( 'NONE',  ( 22.81628187352647785, 51.62363466993042493, 6.195893100308588602E-16 ) ) ;
#34558 = CARTESIAN_POINT ( 'NONE',  ( 7.084665262690076126, 69.10535201082151957, 10.88017736071109987 ) ) ;
#34560 = CARTESIAN_POINT ( 'NONE',  ( 17.08211943468705130, 38.47041550158063217, 12.26659068614894998 ) ) ;
#34561 = DIRECTION ( 'NONE',  ( -0.000000000000000000, -1.000000000000000000, -0.000000000000000000 ) ) ;
#34562 = CARTESIAN_POINT ( 'NONE',  ( 5.076628168052703671, 11.84226448433411960, 8.527530157486179263 ) ) ;
#34563 = ADVANCED_FACE ( 'NONE', ( #46824 ), #36917, .T. ) ;
#34564 = CARTESIAN_POINT ( 'NONE',  ( -8.527530157486173934, 1.425597817667455303, 4.923371831947302546 ) ) ;
#34565 = ORIENTED_EDGE ( 'NONE', *, *, #9261, .F. ) ;
#34566 = DIRECTION ( 'NONE',  ( -0.8788171126619679363, 0.000000000000000000, 0.4771587602596037980 ) ) ;
#34567 = CARTESIAN_POINT ( 'NONE',  ( 2.791683348922237240, 15.38393115100078212, -7.208316651077763204 ) ) ;
#34568 = VERTEX_POINT ( 'NONE', #47307 ) ;
#34569 = CIRCLE ( 'NONE', #95240, 9.900000000000002132 ) ;
#34571 = CARTESIAN_POINT ( 'NONE',  ( 17.96484262340118221, 31.18868534415483751, -7.964842623401177768 ) ) ;
#34570 = CARTESIAN_POINT ( 'NONE',  ( 20.88017736071110875, 5.772018677488170546, -2.915334737309920765 ) ) ;
#34573 = CARTESIAN_POINT ( 'NONE',  ( 22.81628187352647785, 1.415301336597087012, 3.434112377981063169 ) ) ;
#34572 = CARTESIAN_POINT ( 'NONE',  ( 18.52753015748617571, 48.09226448433412315, 4.923371831947298993 ) ) ;
#34574 = CARTESIAN_POINT ( 'NONE',  ( 0.000000000000000000, -97.00000000000000000, 3.750000000000000000 ) ) ;
#34575 = AXIS2_PLACEMENT_3D ( 'NONE', #20252, #51237, #20746 ) ;
#34576 = AXIS2_PLACEMENT_3D ( 'NONE', #63869, #2436, #32894 ) ;
#34577 = COLOUR_RGB ( '', 0.66274510, 0.83137255, 0.94901961) ;
#34578 = CARTESIAN_POINT ( 'NONE',  ( -2.816281873526473856, 19.33196800326375708, 3.434112377981055619 ) ) ;
#34579 = ORIENTED_EDGE ( 'NONE', *, *, #10994, .T. ) ;
#34580 = CARTESIAN_POINT ( 'NONE',  ( 0.1532563361054083140, 36.00893115100078745, 1.131784320476157264E-15 ) ) ;
#34581 = CARTESIAN_POINT ( 'NONE',  ( 10.00000000000000178, 58.05374883491397497, 14.16423886937410082 ) ) ;
#34582 = EDGE_LOOP ( 'NONE', ( #37499, #15103, #10632, #27076, #25332, #65317 ) ) ;
#34583 = CARTESIAN_POINT ( 'NONE',  ( -2.266590686148945544, 57.22041550158063217, 7.082119434687048631 ) ) ;
#34584 = EDGE_LOOP ( 'NONE', ( #57855, #93053, #95783, #69284 ) ) ;
#34585 = CARTESIAN_POINT ( 'NONE',  ( -0.8801773607111008646, 33.27201867748817676, 2.915334737309923430 ) ) ;
#34586 = CARTESIAN_POINT ( 'NONE',  ( 2.035157376598824452, 43.68868534415484106, 7.964842623401179544 ) ) ;
#34587 = CARTESIAN_POINT ( 'NONE',  ( 17.96484262340118221, 46.18868534415484106, -7.964842623401177768 ) ) ;
#34588 = CLOSED_SHELL ( 'NONE', ( #76087, #22850, #28688, #23065, #72063, #88141, #34290, #338, #62238, #73821, #77671, #75536, #15449, #85801, #31168, #70564, #36696, #79008, #26239, #32009, #93248, #8605, #40293, #39543, #45738, #48205, #53109, #62546, #40209, #21229, #34555, #91778, #77793, #54181, #23818, #70030, #93805, #3998, #28113, #34171, #8927, #97002, #29249, #7501, #4904, #37531, #85303, #64461, #25306, #1599, #14817, #78771, #5280, #38408, #75768, #6041, #84328, #40190, #5376, #19076, #24677, #34689, #67420, #2757, #1655, #22199, #87730, #46532, #23717, #49325, #35906, #61760, #55262, #32972, #92206, #31757, #73580, #71571, #47917, #94743, #92359 ) ) ;
#34589 = DIRECTION ( 'NONE',  ( -1.000000000000000000, 0.000000000000000000, 0.000000000000000000 ) ) ;
#34590 = CARTESIAN_POINT ( 'NONE',  ( 17.96484262340118221, 46.18868534415484106, -7.964842623401177768 ) ) ;
#34591 = DIRECTION ( 'NONE',  ( 0.000000000000000000, 0.000000000000000000, 1.000000000000000000 ) ) ;
#34592 = ADVANCED_FACE ( 'NONE', ( #16832 ), #55816, .T. ) ;
#34594 = ORIENTED_EDGE ( 'NONE', *, *, #92397, .T. ) ;
#34593 = FACE_OUTER_BOUND ( 'NONE', #60630, .T. ) ;
#34595 = CARTESIAN_POINT ( 'NONE',  ( 19.84674366389459621, 18.50893115100078745, 7.409399052514197653E-17 ) ) ;
#34596 = ORIENTED_EDGE ( 'NONE', *, *, #2317, .F. ) ;
#34597 = CARTESIAN_POINT ( 'NONE',  ( 10.76560087618683603, -96.07989234454169036, 4.000000000000000000 ) ) ;
#34598 = CARTESIAN_POINT ( 'NONE',  ( 5.076628168052703671, 51.84226448433412315, 8.527530157486179263 ) ) ;
#34599 = DIRECTION ( 'NONE',  ( 1.000000000000000000, 0.000000000000000000, 0.000000000000000000 ) ) ;
#34600 = VECTOR ( 'NONE', #67540, 1000.000000000000000 ) ;
#34601 = CARTESIAN_POINT ( 'NONE',  ( 0.6178305044545818747, 53.49863466993041072, -9.382169495545419124 ) ) ;
#34602 = PLANE ( 'NONE',  #26729 ) ;
#34603 = ORIENTED_EDGE ( 'NONE', *, *, #21710, .T. ) ;
#34604 = FACE_OUTER_BOUND ( 'NONE', #4653, .T. ) ;
#34605 = CARTESIAN_POINT ( 'NONE',  ( -5.810137351020829399, -36.09275136659677230, 3.750000000000001332 ) ) ;
#34606 = CARTESIAN_POINT ( 'NONE',  ( 0.2751277870542967463, 70.00000000000000000, -6.000000000000000000 ) ) ;
#34607 = CARTESIAN_POINT ( 'NONE',  ( -0.3689425029237898834, 66.17874883491396076, -10.36894250292378850 ) ) ;
#34608 = CARTESIAN_POINT ( 'NONE',  ( 2.791683348922240793, 66.63393115100079456, 7.208316651077764092 ) ) ;
#34609 = ORIENTED_EDGE ( 'NONE', *, *, #91797, .F. ) ;
#34610 = CARTESIAN_POINT ( 'NONE',  ( 0.000000000000000000, 15.00000000000000000, 0.000000000000000000 ) ) ;
#34611 = CARTESIAN_POINT ( 'NONE',  ( 18.52753015748618282, 28.92559781766745175, -4.923371831947291888 ) ) ;
#34612 = CARTESIAN_POINT ( 'NONE',  ( 11.61481287315787370, -90.96947208220468895, 3.750000000000000000 ) ) ;
#34613 = CARTESIAN_POINT ( 'NONE',  ( 21.09922568453594849, 1.206968003263753531, 6.408140936763242479 ) ) ;
#34614 = CARTESIAN_POINT ( 'NONE',  ( 4.559911319644449179, 62.23035201082150536, -9.422509992056141925 ) ) ;
#34615 = CARTESIAN_POINT ( 'NONE',  ( 5.419894505350582925, 0.5000000000000004441, -13.98659156302458761 ) ) ;
#34616 = CARTESIAN_POINT ( 'NONE',  ( 0.1532563361054083140, 16.00893115100078390, 1.131784320476157264E-15 ) ) ;
#34617 = CARTESIAN_POINT ( 'NONE',  ( 1.472469842513823179, 61.42559781766745175, 4.923371831947296329 ) ) ;
#34618 = CARTESIAN_POINT ( 'NONE',  ( 2.603489959281581889, 20.43575266056827999, -6.499999999999995559 ) ) ;
#34619 = AXIS2_PLACEMENT_3D ( 'NONE', #70765, #47746, #78242 ) ;
#34620 = TOROIDAL_SURFACE ( 'NONE', #84119, 2.750000000000001776, 0.2500000000000000000 ) ;
#34621 = ORIENTED_EDGE ( 'NONE', *, *, #86987, .T. ) ;
#34622 = CARTESIAN_POINT ( 'NONE',  ( 20.88017736071110875, 15.77201867748817143, -2.915334737309920765 ) ) ;
#34623 = CARTESIAN_POINT ( 'NONE',  ( 1.472469842513823179, 11.42559781766745175, 4.923371831947296329 ) ) ;
#34624 = CARTESIAN_POINT ( 'NONE',  ( 4.559911319644449179, 43.89701867748816966, 9.422509992056141925 ) ) ;
#34626 = CARTESIAN_POINT ( 'NONE',  ( 10.16173502257720607, 12.81517340034854868, -5.532277395377471763 ) ) ;
#34625 = CARTESIAN_POINT ( 'NONE',  ( 3.591859063236763294, 23.29030133659708568, -11.09922568453595026 ) ) ;
#34627 = CARTESIAN_POINT ( 'NONE',  ( 20.88017736071110164, 5.355352010821502695, 2.915334737309930979 ) ) ;
#34628 = LINE ( 'NONE', #65127, #43711 ) ;
#34629 = CARTESIAN_POINT ( 'NONE',  ( 19.72487221294571569, 59.78217586085237656, 6.499999999999986677 ) ) ;
#34630 = CARTESIAN_POINT ( 'NONE',  ( 12.63842701281683034, 47.46726448433412315, 9.846743663894596210 ) ) ;
#34631 = CARTESIAN_POINT ( 'NONE',  ( 12.63842701281683922, 19.55059781766745175, -9.846743663894590881 ) ) ;
#34632 = CARTESIAN_POINT ( 'NONE',  ( 10.88017736071110164, -29.64464798917849109, 2.915334737309921209 ) ) ;
#34633 = CARTESIAN_POINT ( 'NONE',  ( 21.09922568453595559, 22.04030133659708923, -6.408140936763230044 ) ) ;
#34634 = CARTESIAN_POINT ( 'NONE',  ( -11.01424773186859696, -93.41215259627330170, -4.000000000000000000 ) ) ;
#34635 = EDGE_CURVE ( 'NONE', #22152, #84653, #40131, .T. ) ;
#34637 = FACE_OUTER_BOUND ( 'NONE', #77820, .T. ) ;
#34636 = CARTESIAN_POINT ( 'NONE',  ( 15.44008868035555260, 24.73035201082150891, 9.422509992056143702 ) ) ;
#34638 = DIRECTION ( 'NONE',  ( 6.938893903907221278E-15, 1.000000000000000000, 0.000000000000000000 ) ) ;
#34639 = CARTESIAN_POINT ( 'NONE',  ( 2.917880565312948704, 47.63708216824730357, 12.26659068614894643 ) ) ;
#34640 = VECTOR ( 'NONE', #65478, 1000.000000000000000 ) ;
#34641 = CARTESIAN_POINT ( 'NONE',  ( 0.2751277870542909176, 64.36607318730132477, -6.499999999999992006 ) ) ;
#34642 = CARTESIAN_POINT ( 'NONE',  ( 2.791683348922237240, 40.38393115100078035, -7.208316651077763204 ) ) ;
#34643 = AXIS2_PLACEMENT_3D ( 'NONE', #93091, #9602, #46608 ) ;
#34644 = CARTESIAN_POINT ( 'NONE',  ( 19.38216949554541202, 35.99863466993041072, 9.382169495545424454 ) ) ;
#34645 = CARTESIAN_POINT ( 'NONE',  ( 4.559911319644449179, 28.89701867748817321, 9.422509992056141925 ) ) ;
#34646 = EDGE_CURVE ( 'NONE', #95455, #19933, #17815, .T. ) ;
#34647 = CARTESIAN_POINT ( 'NONE',  ( 12.63842701281683034, 52.46726448433413026, 9.846743663894596210 ) ) ;
#34648 = CARTESIAN_POINT ( 'NONE',  ( 15.44008868035555793, 56.39701867748817676, -9.422509992056140149 ) ) ;
#34649 = CARTESIAN_POINT ( 'NONE',  ( 21.09922568453595559, 12.04030133659708746, -6.408140936763230044 ) ) ;
#34650 = CARTESIAN_POINT ( 'NONE',  ( 13.79529636645030344, 28.26208216824729647, 14.16423886937410614 ) ) ;
#34652 = ADVANCED_FACE ( 'NONE', ( #39826 ), #78803, .F. ) ;
#34651 = DIRECTION ( 'NONE',  ( -0.000000000000000000, -0.000000000000000000, -1.000000000000000000 ) ) ;
#34653 = EDGE_CURVE ( 'NONE', #295, #25266, #84805, .T. ) ;
#34654 = CARTESIAN_POINT ( 'NONE',  ( 10.00000000000000178, 22.25893115100078745, 9.846743663894594434 ) ) ;
#34655 = CARTESIAN_POINT ( 'NONE',  ( -2.816281873526473856, 59.12363466993042493, 9.499525473075851096E-16 ) ) ;
#34656 = CARTESIAN_POINT ( 'NONE',  ( 10.00000000000000000, -2.126365330069579951, -12.81628187352647608 ) ) ;
#34657 = ORIENTED_EDGE ( 'NONE', *, *, #98641, .T. ) ;
#34658 = CARTESIAN_POINT ( 'NONE',  ( 4.903136312256997087, -13.39483660680936339, 3.750000000000001776 ) ) ;
#34659 = CARTESIAN_POINT ( 'NONE',  ( 20.88017736071110875, 20.77201867748816611, -2.915334737309920765 ) ) ;
#34660 = CARTESIAN_POINT ( 'NONE',  ( 17.96484262340118221, 61.18868534415482685, -7.964842623401177768 ) ) ;
#34661 = CARTESIAN_POINT ( 'NONE',  ( -2.266590686148945544, 22.22041550158063572, 7.082119434687048631 ) ) ;
#34662 = CARTESIAN_POINT ( 'NONE',  ( 7.084665262690076126, 64.10535201082150536, 10.88017736071109987 ) ) ;
#34663 = CARTESIAN_POINT ( 'NONE',  ( 17.20831665107776587, 54.13393115100079456, -7.208316651077762316 ) ) ;
#34664 = CARTESIAN_POINT ( 'NONE',  ( 4.559911319644449179, 37.23035201082150536, -9.422509992056141925 ) ) ;
#34665 = LINE ( 'NONE', #65162, #60701 ) ;
#34666 = CARTESIAN_POINT ( 'NONE',  ( -42.16485527613927076, 107.5383484153110061, -5.000000000000000000 ) ) ;
#34667 = AXIS2_PLACEMENT_3D ( 'NONE', #2742, #78715, #31724 ) ;
#34668 = ADVANCED_FACE ( 'NONE', ( #63292 ), #23854, .F. ) ;
#34669 = ORIENTED_EDGE ( 'NONE', *, *, #47968, .T. ) ;
#34670 = CARTESIAN_POINT ( 'NONE',  ( 7.771322705631394712, 15.00000000000000000, 12.24159072199921283 ) ) ;
#34671 = ORIENTED_EDGE ( 'NONE', *, *, #41465, .F. ) ;
#34672 = VERTEX_POINT ( 'NONE', #31812 ) ;
#34673 = CARTESIAN_POINT ( 'NONE',  ( 9.742785792574936821, 10.00513551118487499, 5.624999999999997335 ) ) ;
#34674 = CARTESIAN_POINT ( 'NONE',  ( 10.00000000000000000, 10.55374883491396787, -14.16423886937410082 ) ) ;
#34675 = CARTESIAN_POINT ( 'NONE',  ( 10.00000000000000000, 15.55374883491396787, -14.16423886937410082 ) ) ;
#34676 = CARTESIAN_POINT ( 'NONE',  ( 0.5774900079438607392, 48.48035201082150536, 5.440088680355550821 ) ) ;
#34677 = CARTESIAN_POINT ( 'NONE',  ( 22.26659068614895176, 59.72041550158063927, -7.082119434687042414 ) ) ;
#34678 = CARTESIAN_POINT ( 'NONE',  ( 7.361572987183170547, 57.05059781766744464, 9.846743663894590881 ) ) ;
#34679 = CARTESIAN_POINT ( 'NONE',  ( 5.076628168052704559, 35.17559781766745175, -8.527530157486179263 ) ) ;
#34680 = CARTESIAN_POINT ( 'NONE',  ( -0.7375392941519317569, 0.5000000000000004441, 14.98185688723470044 ) ) ;
#34682 = CARTESIAN_POINT ( 'NONE',  ( 0.1532563361054100626, 60.80059781766744464, -2.638427012816831230 ) ) ;
#34681 = CARTESIAN_POINT ( 'NONE',  ( 4.559911319644449179, 38.89701867748817676, 9.422509992056141925 ) ) ;
#34683 = CARTESIAN_POINT ( 'NONE',  ( -4.164238869374099927, 7.012082168247302683, 3.795296366450308767 ) ) ;
#34684 = CARTESIAN_POINT ( 'NONE',  ( 10.00000000000000178, 48.05374883491396787, 14.16423886937410082 ) ) ;
#34685 = COLOUR_RGB ( '', 0.09019608, 0.27058824, 0.51372549) ;
#34686 = CARTESIAN_POINT ( 'NONE',  ( 12.91533473730993009, 6.605352010821504471, -10.88017736071109987 ) ) ;
#34687 = CARTESIAN_POINT ( 'NONE',  ( 19.84674366389459621, 38.50893115100078745, 7.409399052514197653E-17 ) ) ;
#34688 = CYLINDRICAL_SURFACE ( 'NONE', #57133, 0.2500000000000002220 ) ;
#34689 = ADVANCED_FACE ( 'NONE', ( #93308 ), #65657, .T. ) ;
#34690 = CARTESIAN_POINT ( 'NONE',  ( -9.846743663894596210, -39.19940218233254825, -2.638427012816824124 ) ) ;
#34691 = ORIENTED_EDGE ( 'NONE', *, *, #69650, .F. ) ;
#34692 = FACE_OUTER_BOUND ( 'NONE', #26223, .T. ) ;
#34693 = VERTEX_POINT ( 'NONE', #48296 ) ;
#34694 = CARTESIAN_POINT ( 'NONE',  ( 14.92337183194729633, 17.67559781766745175, 8.527530157486181039 ) ) ;
#34695 = ORIENTED_EDGE ( 'NONE', *, *, #8089, .F. ) ;
#34696 = CARTESIAN_POINT ( 'NONE',  ( 6.204703633549690345, 27.84541550158063217, 14.16423886937410082 ) ) ;
#34697 = CARTESIAN_POINT ( 'NONE',  ( 2.791683348922237240, 30.38393115100078390, -7.208316651077763204 ) ) ;
#34698 = CARTESIAN_POINT ( 'NONE',  ( 4.559911319644449179, 62.23035201082150536, -9.422509992056141925 ) ) ;
#34699 = CARTESIAN_POINT ( 'NONE',  ( 17.85999999999999588, 33.98752635800203592, -10.00000000000000000 ) ) ;
#34700 = CARTESIAN_POINT ( 'NONE',  ( 10.00000000000000178, 49.31368534415484106, 10.88017736071110342 ) ) ;
#34701 = B_SPLINE_CURVE_WITH_KNOTS ( 'NONE', 3,
 ( #65100, #95621, #27110, #80621, #12115, #7092 ),
 .UNSPECIFIED., .F., .F.,
 ( 4, 2, 4 ),
 ( 3.409110551495867094E-05, 0.0004400426677367964921, 0.0008459942299586342522 ),
 .UNSPECIFIED. ) ;
#34702 = CARTESIAN_POINT ( 'NONE',  ( 11.09922568453595026, 6.206968003263757083, 6.408140936763232709 ) ) ;
#34703 = EDGE_LOOP ( 'NONE', ( #50499, #57589, #2160, #9434 ) ) ;
#34704 = CARTESIAN_POINT ( 'NONE',  ( -4.164238869374099039, 16.80374883491396787, 8.674139862899312516E-16 ) ) ;
#34705 = ORIENTED_EDGE ( 'NONE', *, *, #1141, .F. ) ;
#34706 = CARTESIAN_POINT ( 'NONE',  ( -2.816281873526473856, 49.33196800326374643, 3.434112377981055619 ) ) ;
#34707 = AXIS2_PLACEMENT_3D ( 'NONE', #53549, #44070, #90070 ) ;
#34708 = CARTESIAN_POINT ( 'NONE',  ( 20.88017736071110164, 20.35535201082150891, 2.915334737309930979 ) ) ;
#34709 = CARTESIAN_POINT ( 'NONE',  ( 18.52753015748618282, 28.92559781766745175, -4.923371831947291888 ) ) ;
#34711 = CARTESIAN_POINT ( 'NONE',  ( 10.00000000000000178, 19.31368534415484106, 10.88017736071110342 ) ) ;
#34710 = B_SPLINE_CURVE_WITH_KNOTS ( 'NONE', 3,
 ( #27483, #36970, #13983, #35969, #44457, #73469, #66470, #27972, #81469, #57975, #4510, #97000, #59948, #20986, #59458, #28475, #58467, #89471 ),
 .UNSPECIFIED., .F., .F.,
 ( 4, 2, 2, 2, 2, 2, 2, 2, 4 ),
 ( 0.000000000000000000, 0.002783920674699109140, 0.005567841349398218280, 0.01113568269879643309, 0.02227136539759286271, 0.04454273079518572542, 0.06681409619277858813, 0.07794977889157500561, 0.08908546159037145085 ),
 .UNSPECIFIED. ) ;
#34712 = CARTESIAN_POINT ( 'NONE',  ( 22.81628187352647785, 56.41530133659708213, 3.434112377981063169 ) ) ;
#34713 = FACE_OUTER_BOUND ( 'NONE', #51047, .T. ) ;
#34714 = CARTESIAN_POINT ( 'NONE',  ( 0.1532563361054082862, 36.21726448433410894, 2.638427012816831674 ) ) ;
#34715 = CIRCLE ( 'NONE', #60282, 14.49999999999999822 ) ;
#34716 = VECTOR ( 'NONE', #15707, 1000.000000000000000 ) ;
#34717 = AXIS2_PLACEMENT_3D ( 'NONE', #5562, #59035, #1021 ) ;
#34718 = CARTESIAN_POINT ( 'NONE',  ( 21.92686044187656691, 22.18830936912750929, 4.562052436263911564E-16 ) ) ;
#34719 = DIRECTION ( 'NONE',  ( 0.000000000000000000, 0.000000000000000000, -1.000000000000000000 ) ) ;
#34720 = DIRECTION ( 'NONE',  ( 1.000000000000000000, 0.000000000000000000, 0.000000000000000000 ) ) ;
#34721 = CARTESIAN_POINT ( 'NONE',  ( -0.1503990784575327533, 7.222660991849186196, -6.262539305110070842 ) ) ;
#34722 = CARTESIAN_POINT ( 'NONE',  ( 17.20831665107776587, 4.133931151000785675, -7.208316651077762316 ) ) ;
#34723 = CARTESIAN_POINT ( 'NONE',  ( 13.43411237798105340, 30.58196800326374998, 12.81628187352647963 ) ) ;
#34724 =( NAMED_UNIT ( * ) PLANE_ANGLE_UNIT ( ) SI_UNIT ( $, .RADIAN. ) );
#34725 = EDGE_CURVE ( 'NONE', #38271, #68316, #15856, .T. ) ;
#34726 = CARTESIAN_POINT ( 'NONE',  ( 12.63842701281683922, 39.55059781766744464, -9.846743663894590881 ) ) ;
#34727 = DIRECTION ( 'NONE',  ( 0.000000000000000000, 1.000000000000000000, 0.000000000000000000 ) ) ;
#34728 = CARTESIAN_POINT ( 'NONE',  ( 24.16423886937409904, 19.09541550158063927, 3.795296366450317205 ) ) ;
#34729 = CARTESIAN_POINT ( 'NONE',  ( 7.361572987183169658, 34.96726448433411605, -9.846743663894592657 ) ) ;
#34730 = CARTESIAN_POINT ( 'NONE',  ( -2.816281873526471635, 38.91530133659708213, -3.434112377981056508 ) ) ;
#34732 = SURFACE_STYLE_FILL_AREA ( #10774 ) ;
#34731 = CARTESIAN_POINT ( 'NONE',  ( 17.85158348494336522, 14.73726573380441174, -6.499999999999984901 ) ) ;
#34733 = CARTESIAN_POINT ( 'NONE',  ( 7.084665262690076126, 57.02201867748817676, -10.88017736071110164 ) ) ;
#34734 = CARTESIAN_POINT ( 'NONE',  ( 19.38216949554541202, 10.99863466993042138, 9.382169495545424454 ) ) ;
#34735 = CARTESIAN_POINT ( 'NONE',  ( -14.99847009497944583, 0.5000000000000004441, 0.2142307401079343032 ) ) ;
#34736 = EDGE_CURVE ( 'NONE', #52255, #5105, #78305, .T. ) ;
#34737 = CARTESIAN_POINT ( 'NONE',  ( 18.52753015748617571, 33.09226448433411605, 4.923371831947298993 ) ) ;
#34738 = CARTESIAN_POINT ( 'NONE',  ( 4.559911319644449179, 22.23035201082150536, -9.422509992056141925 ) ) ;
#34739 = CARTESIAN_POINT ( 'NONE',  ( 16.40814093676324603, 32.45696800326375353, -11.09922568453594671 ) ) ;
#34740 = CARTESIAN_POINT ( 'NONE',  ( 0.1532563361054100626, 35.80059781766745175, -2.638427012816831230 ) ) ;
#34741 = SHAPE_DEFINITION_REPRESENTATION ( #83359, #57512 ) ;
#34742 = DIRECTION ( 'NONE',  ( 1.000000000000000000, 0.000000000000000000, 0.000000000000000000 ) ) ;
#34744 = B_SPLINE_CURVE_WITH_KNOTS ( 'NONE', 3,
 ( #31315, #9815, #92322, #23847, #78799, #92810, #70821, #54313 ),
 .UNSPECIFIED., .F., .F.,
 ( 4, 2, 2, 4 ),
 ( -1.048808863134852564E-05, 0.0008972750855482683431, 0.001351156672638076373, 0.001805038259727884294 ),
 .UNSPECIFIED. ) ;
#34743 = CARTESIAN_POINT ( 'NONE',  ( 15.44008868035555260, 34.73035201082151247, 9.422509992056143702 ) ) ;
#34745 = B_SPLINE_CURVE_WITH_KNOTS ( 'NONE', 3,
 ( #70503, #55500, #86001, #69518, #24524, #17512 ),
 .UNSPECIFIED., .F., .F.,
 ( 4, 2, 4 ),
 ( 3.409110551496079191E-05, 0.0004400426677367849453, 0.0008459942299586090987 ),
 .UNSPECIFIED. ) ;
#34746 = ORIENTED_EDGE ( 'NONE', *, *, #20028, .T. ) ;
#34747 = CARTESIAN_POINT ( 'NONE',  ( -11.24999999999999822, 3.130135511184870545, 3.014428414850141458 ) ) ;
#34748 = CARTESIAN_POINT ( 'NONE',  ( 4.559911319644449179, 2.230352010821504471, -9.422509992056141925 ) ) ;
#34750 = CARTESIAN_POINT ( 'NONE',  ( 19.42250999205614548, 30.98035201082150536, -5.440088680355545492 ) ) ;
#34749 = CARTESIAN_POINT ( 'NONE',  ( 10.00000000000000178, 62.25893115100078745, 9.846743663894594434 ) ) ;
#34751 = DIRECTION ( 'NONE',  ( 0.000000000000000000, 1.000000000000000000, 0.000000000000000000 ) ) ;
#34752 = CARTESIAN_POINT ( 'NONE',  ( 10.00000000000000000, 56.81368534415484106, -10.88017736071110342 ) ) ;
#34754 =( NAMED_UNIT ( * ) SI_UNIT ( $, .STERADIAN. ) SOLID_ANGLE_UNIT ( ) );
#34753 = CARTESIAN_POINT ( 'NONE',  ( -0.8801773607110991993, 27.85535201082150181, -2.915334737309923874 ) ) ;
#34755 = CARTESIAN_POINT ( 'NONE',  ( 19.84674366389459266, 3.717264484334118713, -2.638427012816827677 ) ) ;
#34756 = CARTESIAN_POINT ( 'NONE',  ( -46.56032276184168239, 103.8061269828102837, -5.692785089662786291 ) ) ;
#34757 = CARTESIAN_POINT ( 'NONE',  ( 12.63842701281683922, 54.55059781766745175, -9.846743663894590881 ) ) ;
#34759 = CARTESIAN_POINT ( 'NONE',  ( 21.92686044187657046, 20.16212336850780673, 4.562052436263912550E-16 ) ) ;
#34758 = CARTESIAN_POINT ( 'NONE',  ( -0.3689425029237898834, 51.17874883491397497, -10.36894250292378850 ) ) ;
#34760 = CARTESIAN_POINT ( 'NONE',  ( 12.83294900548058415, 0.5000000000000004441, 7.766300266068450142 ) ) ;
#34761 = CARTESIAN_POINT ( 'NONE',  ( 22.26659068614895176, 14.72041550158063572, -7.082119434687042414 ) ) ;
#34762 = CARTESIAN_POINT ( 'NONE',  ( 22.26659068614894466, 43.88708216824729647, 7.082119434687054849 ) ) ;
#34763 = CIRCLE ( 'NONE', #14028, 15.00000000000000000 ) ;
#34764 = CARTESIAN_POINT ( 'NONE',  ( 3.591859063236763294, 8.290301336597087456, -11.09922568453595026 ) ) ;
#34765 = ADVANCED_FACE ( 'NONE', ( #17334 ), #97608, .T. ) ;
#34766 = CARTESIAN_POINT ( 'NONE',  ( -6.607077432771771619, -50.94230397256625764, 2.750000000000001332 ) ) ;
#34767 = ORIENTED_EDGE ( 'NONE', *, *, #38798, .T. ) ;
#34768 = CARTESIAN_POINT ( 'NONE',  ( 17.96484262340118221, 4.938685344154837509, 7.964842623401181321 ) ) ;
#34769 = CARTESIAN_POINT ( 'NONE',  ( 19.84674366389459266, 38.71726448433412315, -2.638427012816827677 ) ) ;
#34771 = FACE_OUTER_BOUND ( 'NONE', #4878, .T. ) ;
#34770 = DIRECTION ( 'NONE',  ( -0.3665012267242880317, 0.000000000000000000, -0.9304175679820281264 ) ) ;
#34772 = CARTESIAN_POINT ( 'NONE',  ( 12.91533473730993009, 56.60535201082151247, -10.88017736071109987 ) ) ;
#34773 = CARTESIAN_POINT ( 'NONE',  ( 17.35999999999999943, 37.99999999999997868, 9.500000000000000000 ) ) ;
#34774 = EDGE_CURVE ( 'NONE', #75803, #92371, #16148, .T. ) ;
#34775 = LINE ( 'NONE', #28757, #21119 ) ;
#34776 = CARTESIAN_POINT ( 'NONE',  ( 22.81628187352647785, 26.62363466993042138, 6.195893100308588602E-16 ) ) ;
#34777 = CARTESIAN_POINT ( 'NONE',  ( 0.1532563361054083140, 26.00893115100078745, 1.131784320476157264E-15 ) ) ;
#34778 = ORIENTED_EDGE ( 'NONE', *, *, #68187, .T. ) ;
#34779 = PRESENTATION_STYLE_ASSIGNMENT (( #10326 ) ) ;
#34780 = FILL_AREA_STYLE_COLOUR ( '', #76595 ) ;
#34781 = CARTESIAN_POINT ( 'NONE',  ( 4.559911319644449179, 3.897018677488171434, 9.422509992056141925 ) ) ;
#34782 = CARTESIAN_POINT ( 'NONE',  ( 22.26659068614895176, 34.72041550158063927, -7.082119434687042414 ) ) ;
#34783 = CARTESIAN_POINT ( 'NONE',  ( 19.42250999205614548, 30.98035201082150536, -5.440088680355545492 ) ) ;
#34784 = CARTESIAN_POINT ( 'NONE',  ( 12.91533473730992121, 54.52201867748816255, 10.88017736071110164 ) ) ;
#34785 = FACE_OUTER_BOUND ( 'NONE', #10549, .T. ) ;
#34786 = CARTESIAN_POINT ( 'NONE',  ( 17.39651004071841456, 49.08210964143329136, -6.500000000000001776 ) ) ;
#34787 = CARTESIAN_POINT ( 'NONE',  ( 2.791683348922237240, 15.38393115100078212, -7.208316651077763204 ) ) ;
#34788 = DIRECTION ( 'NONE',  ( 0.000000000000000000, 1.000000000000000000, 0.000000000000000000 ) ) ;
#34789 = CARTESIAN_POINT ( 'NONE',  ( 7.361572987183170547, 37.05059781766744464, 9.846743663894590881 ) ) ;
#34790 = CARTESIAN_POINT ( 'NONE',  ( 1.472469842513823179, 66.42559781766745175, 4.923371831947296329 ) ) ;
#34791 = AXIS2_PLACEMENT_3D ( 'NONE', #1356, #75349, #90841 ) ;
#34792 = CARTESIAN_POINT ( 'NONE',  ( 17.96484262340118221, 24.93868534415484461, 7.964842623401181321 ) ) ;
#34793 =( GEOMETRIC_REPRESENTATION_CONTEXT ( 3 ) GLOBAL_UNCERTAINTY_ASSIGNED_CONTEXT ( ( #64299 ) ) GLOBAL_UNIT_ASSIGNED_CONTEXT ( ( #77680, #95528, #2210 ) ) REPRESENTATION_CONTEXT ( 'NONE', 'WORKASPACE' ) );
#34794 = STYLED_ITEM ( 'NONE', ( #65056 ), #70016 ) ;
#34795 = ORIENTED_EDGE ( 'NONE', *, *, #2208, .T. ) ;
#34796 = CARTESIAN_POINT ( 'NONE',  ( -2.816281873526471635, 38.91530133659708213, -3.434112377981056508 ) ) ;
#34797 = CARTESIAN_POINT ( 'NONE',  ( 7.084665262690076126, 69.10535201082151957, 10.88017736071109987 ) ) ;
#34798 = CARTESIAN_POINT ( 'NONE',  ( 0.1532563361054100626, 25.80059781766744820, -2.638427012816831230 ) ) ;
#34800 = CARTESIAN_POINT ( 'NONE',  ( 12.63842701281683922, 19.55059781766745175, -9.846743663894590881 ) ) ;
#34799 = CARTESIAN_POINT ( 'NONE',  ( 13.79529636645030344, 63.26208216824730357, 14.16423886937410614 ) ) ;
#34801 = CARTESIAN_POINT ( 'NONE',  ( -7.750355510519348456, 84.07179676972448590, -4.000000000000000000 ) ) ;
#34802 = CARTESIAN_POINT ( 'NONE',  ( 12.63842701281683034, 62.46726448433410894, 9.846743663894596210 ) ) ;
#34803 = CARTESIAN_POINT ( 'NONE',  ( 22.26659068614894466, 23.88708216824730357, 7.082119434687054849 ) ) ;
#34804 = CARTESIAN_POINT ( 'NONE',  ( -2.266590686148945544, 26.38708216824730357, -7.082119434687050408 ) ) ;
#34805 = CARTESIAN_POINT ( 'NONE',  ( 5.076628168052703671, 41.84226448433411605, 8.527530157486179263 ) ) ;
#34806 = CARTESIAN_POINT ( 'NONE',  ( 18.61655166652077753, 9.877183271974288914, 6.499999999999968914 ) ) ;
#34807 = CARTESIAN_POINT ( 'NONE',  ( 19.42250999205614548, 30.98035201082150536, -5.440088680355545492 ) ) ;
#34808 = ADVANCED_FACE ( 'NONE', ( #25811 ), #61823, .T. ) ;
#34809 = CARTESIAN_POINT ( 'NONE',  ( 12.91533473730992121, 64.52201867748817676, 10.88017736071110164 ) ) ;
#34810 = CARTESIAN_POINT ( 'NONE',  ( -0.1503990784575328643, 0.07447313448805115144, 6.262539305110068177 ) ) ;
#34811 = VERTEX_POINT ( 'NONE', #2831 ) ;
#34812 = CARTESIAN_POINT ( 'NONE',  ( 0.6178305044545818747, 48.49863466993042493, -9.382169495545419124 ) ) ;
#34813 = CARTESIAN_POINT ( 'NONE',  ( 10.00000000000000178, 49.31368534415484106, 10.88017736071110342 ) ) ;
#34814 = VERTEX_POINT ( 'NONE', #54319 ) ;
#34815 = FILL_AREA_STYLE_COLOUR ( '', #43504 ) ;
#34816 = DIRECTION ( 'NONE',  ( 0.8070303256584298035, -0.5905099943842175847, 0.000000000000000000 ) ) ;
#34817 = ORIENTED_EDGE ( 'NONE', *, *, #13929, .T. ) ;
#34818 = CARTESIAN_POINT ( 'NONE',  ( 0.5774900079438607392, 68.48035201082150536, 5.440088680355550821 ) ) ;
#34819 = CARTESIAN_POINT ( 'NONE',  ( 20.88017736071110164, 10.35535201082150714, 2.915334737309930979 ) ) ;
#34820 = CARTESIAN_POINT ( 'NONE',  ( 2.913501739333662854, 4.325554204331052541E-16, 14.20427779279537184 ) ) ;
#34821 = CARTESIAN_POINT ( 'NONE',  ( 0.000000000000000000, 0.000000000000000000, 0.000000000000000000 ) ) ;
#34822 = CARTESIAN_POINT ( 'NONE',  ( 0.5774900079438607392, 3.480352010821504916, 5.440088680355550821 ) ) ;
#34823 = CARTESIAN_POINT ( 'NONE',  ( 19.84674366389459621, 3.508931151000785231, 7.409399052514197653E-17 ) ) ;
#34824 = CARTESIAN_POINT ( 'NONE',  ( 6.204703633549690345, 15.76208216824730179, -14.16423886937410259 ) ) ;
#34825 = CARTESIAN_POINT ( 'NONE',  ( -0.8801773607111009756, 18.06368534415484106, 1.068504757029289695E-15 ) ) ;
#34826 = CARTESIAN_POINT ( 'NONE',  ( 5.076628168052704559, 60.17559781766745175, -8.527530157486179263 ) ) ;
#34827 = ORIENTED_EDGE ( 'NONE', *, *, #36258, .T. ) ;
#34828 = CARTESIAN_POINT ( 'NONE',  ( 10.00000000000000000, 64.75893115100078035, -9.846743663894594434 ) ) ;
#34829 = VERTEX_POINT ( 'NONE', #95782 ) ;
#34830 = CARTESIAN_POINT ( 'NONE',  ( -19.00000000000000000, 75.76920769491739804, -3.000000000000000000 ) ) ;
#34831 = CARTESIAN_POINT ( 'NONE',  ( 10.00000000000000000, 46.81368534415484106, -10.88017736071110342 ) ) ;
#34832 = CARTESIAN_POINT ( 'NONE',  ( 1.472469842513823179, 65.59226448433412315, -4.923371831947296329 ) ) ;
#34834 = CARTESIAN_POINT ( 'NONE',  ( -6.305254017448156389, 1.877203152459836266, -10.07310051930115513 ) ) ;
#34833 = CARTESIAN_POINT ( 'NONE',  ( 2.035157376598822676, 7.438685344154837509, -7.964842623401177768 ) ) ;
#34835 = CARTESIAN_POINT ( 'NONE',  ( 19.42250999205614548, 55.98035201082150536, -5.440088680355545492 ) ) ;
#34836 = CARTESIAN_POINT ( 'NONE',  ( 2.035157376598824452, 3.688685344154837953, 7.964842623401179544 ) ) ;
#34837 = CARTESIAN_POINT ( 'NONE',  ( 13.43411237798105340, 45.58196800326374643, 12.81628187352647963 ) ) ;
#34838 = CARTESIAN_POINT ( 'NONE',  ( 10.00000000000000178, 24.31368534415484106, 10.88017736071110342 ) ) ;
#34839 = CARTESIAN_POINT ( 'NONE',  ( -15.00000000000000000, 83.99999999999998579, -3.750000000000000000 ) ) ;
#34840 = ORIENTED_EDGE ( 'NONE', *, *, #54391, .T. ) ;
#34841 = CARTESIAN_POINT ( 'NONE',  ( 22.81628187352647785, 36.41530133659707502, 3.434112377981063169 ) ) ;
#34842 = CARTESIAN_POINT ( 'NONE',  ( 10.00000000000000178, 39.31368534415484106, 10.88017736071110342 ) ) ;
#34843 = CARTESIAN_POINT ( 'NONE',  ( 12.63842701281683034, 52.46726448433413026, 9.846743663894596210 ) ) ;
#34844 = ORIENTED_EDGE ( 'NONE', *, *, #82507, .T. ) ;
#34845 = CARTESIAN_POINT ( 'NONE',  ( 5.076628168052703671, 66.84226448433412315, 8.527530157486179263 ) ) ;
#34847 = CARTESIAN_POINT ( 'NONE',  ( 0.1532563361054083140, 51.00893115100078745, 1.131784320476157264E-15 ) ) ;
#34846 = CARTESIAN_POINT ( 'NONE',  ( -13.82671409943291785, 15.00000000000000000, -3.447387012295409114 ) ) ;
#34848 = CARTESIAN_POINT ( 'NONE',  ( 12.91533473730993009, 26.60535201082150536, -10.88017736071109987 ) ) ;
#34849 =( NAMED_UNIT ( * ) SI_UNIT ( $, .STERADIAN. ) SOLID_ANGLE_UNIT ( ) );
#34850 = CARTESIAN_POINT ( 'NONE',  ( 10.00000000000000178, 37.25893115100078745, 9.846743663894594434 ) ) ;
#34851 = CARTESIAN_POINT ( 'NONE',  ( -10.14667048435152097, 15.00000000000000000, 10.35833375027034542 ) ) ;
#34852 = CARTESIAN_POINT ( 'NONE',  ( -10.70613742633264565, 4.864377723017530212E-16, 9.778988772285165609 ) ) ;
#34853 = ADVANCED_FACE ( 'NONE', ( #58241 ), #20272, .F. ) ;
#34856 = CARTESIAN_POINT ( 'NONE',  ( 19.84674366389459266, 13.30059781766745353, 2.638427012816836559 ) ) ;
#34855 = PRESENTATION_LAYER_ASSIGNMENT (  '', '', ( #66781 ) ) ;
#34854 = CARTESIAN_POINT ( 'NONE',  ( 10.00000000000000178, 47.25893115100078745, 9.846743663894594434 ) ) ;
#34858 = ORIENTED_EDGE ( 'NONE', *, *, #89671, .T. ) ;
#34857 = CARTESIAN_POINT ( 'NONE',  ( 14.92337183194729988, 54.34226448433412315, -8.527530157486177487 ) ) ;
#34859 = B_SPLINE_CURVE_WITH_KNOTS ( 'NONE', 3,
 ( #63479, #93983, #25505, #55992, #86493, #17993 ),
 .UNSPECIFIED., .F., .F.,
 ( 4, 2, 4 ),
 ( 3.409110551475769374E-05, 0.0004400426677365839884, 0.0008459942299584103645 ),
 .UNSPECIFIED. ) ;
#34860 = VECTOR ( 'NONE', #8039, 1000.000000000000000 ) ;
#34861 = SURFACE_STYLE_USAGE ( .BOTH. , #97866 ) ;
#34862 = CARTESIAN_POINT ( 'NONE',  ( 7.108715748589077066, 14.95077488074853456, 12.92719074505371246 ) ) ;
#34863 = CARTESIAN_POINT ( 'NONE',  ( -1.099225684535947600, 34.54030133659708923, 6.408140936763237150 ) ) ;
#34864 = CARTESIAN_POINT ( 'NONE',  ( 7.361572987183170547, 42.05059781766745886, 9.846743663894590881 ) ) ;
#34865 = LINE ( 'NONE', #73851, #69618 ) ;
#34866 = CARTESIAN_POINT ( 'NONE',  ( 2.917880565312950480, 55.97041550158063217, -12.26659068614894821 ) ) ;
#34867 = CARTESIAN_POINT ( 'NONE',  ( 19.84674366389459266, 38.30059781766745175, 2.638427012816836559 ) ) ;
#34868 = DIRECTION ( 'NONE',  ( -1.000000000000000000, -0.000000000000000000, -0.000000000000000000 ) ) ;
#34869 = CARTESIAN_POINT ( 'NONE',  ( 6.204703633549690345, 55.76208216824730357, -14.16423886937410259 ) ) ;
#34870 = CARTESIAN_POINT ( 'NONE',  ( 7.361572987183170547, 67.05059781766746596, 9.846743663894590881 ) ) ;
#34871 = CARTESIAN_POINT ( 'NONE',  ( 20.88017736071110519, 5.563685344154838397, 2.639326808657452039E-16 ) ) ;
#34872 = CARTESIAN_POINT ( 'NONE',  ( 6.204703633549690345, 30.76208216824730357, -14.16423886937410259 ) ) ;
#34874 = DIRECTION ( 'NONE',  ( 1.000000000000000000, 0.000000000000000000, -0.000000000000000000 ) ) ;
#34873 = CARTESIAN_POINT ( 'NONE',  ( 10.00000000000000000, 50.55374883491396787, -14.16423886937410082 ) ) ;
#34875 = LINE ( 'NONE', #51863, #80338 ) ;
#34876 = CARTESIAN_POINT ( 'NONE',  ( 14.92337183194729633, 7.675597817667451750, 8.527530157486181039 ) ) ;
#34878 = CARTESIAN_POINT ( 'NONE',  ( 19.38216949554541202, 5.998634669930420493, 9.382169495545424454 ) ) ;
#34877 = CARTESIAN_POINT ( 'NONE',  ( 0.5774900079438607392, 28.48035201082150891, 5.440088680355550821 ) ) ;
#34879 = ORIENTED_EDGE ( 'NONE', *, *, #83431, .T. ) ;
#34880 = CARTESIAN_POINT ( 'NONE',  ( 2.035157376598822676, 52.43868534415483396, -7.964842623401177768 ) ) ;
#34881 = CARTESIAN_POINT ( 'NONE',  ( 66.56412365047464164, 26.99999999999998224, -9.500000000000000000 ) ) ;
#34882 = DIRECTION ( 'NONE',  ( 0.000000000000000000, 0.000000000000000000, 1.000000000000000000 ) ) ;
#34883 = CARTESIAN_POINT ( 'NONE',  ( 19.84674366389459266, 53.30059781766744464, 2.638427012816836559 ) ) ;
#34884 = SURFACE_STYLE_FILL_AREA ( #58364 ) ;
#34885 = EDGE_CURVE ( 'NONE', #93321, #27291, #45952, .T. ) ;
#34886 = VERTEX_POINT ( 'NONE', #65755 ) ;
#34887 = CARTESIAN_POINT ( 'NONE',  ( 17.08211943468705840, 25.13708216824730357, -12.26659068614894466 ) ) ;
#34888 = CARTESIAN_POINT ( 'NONE',  ( 0.2751277870542906956, 37.28217586085238366, -6.499999999999992006 ) ) ;
#34889 = SURFACE_STYLE_USAGE ( .BOTH. , #97394 ) ;
#34890 = CARTESIAN_POINT ( 'NONE',  ( 19.42250999205614548, 25.98035201082150891, -5.440088680355545492 ) ) ;
#34891 = CARTESIAN_POINT ( 'NONE',  ( 10.00000000000000178, 35.37363466993042493, 12.81628187352647608 ) ) ;
#34892 = ADVANCED_FACE ( 'NONE', ( #72273 ), #50255, .F. ) ;
#34893 = CARTESIAN_POINT ( 'NONE',  ( 11.35178980618978173, 14.63606909211789464, -9.804941009311937350 ) ) ;
#34894 = CARTESIAN_POINT ( 'NONE',  ( 12.63842701281683922, 9.550597817667449974, -9.846743663894590881 ) ) ;
#34895 = CARTESIAN_POINT ( 'NONE',  ( 0.000000000000000000, 0.000000000000000000, 0.000000000000000000 ) ) ;
#34896 = ORIENTED_EDGE ( 'NONE', *, *, #89157, .F. ) ;
#34897 = CARTESIAN_POINT ( 'NONE',  ( 7.007893109692266087, -58.32153039260716554, -4.000000000000000000 ) ) ;
#34898 = CARTESIAN_POINT ( 'NONE',  ( 20.36894250292379382, 33.67874883491396076, 10.36894250292379205 ) ) ;
#34899 = SURFACE_STYLE_FILL_AREA ( #42419 ) ;
#34900 = CARTESIAN_POINT ( 'NONE',  ( 0.5774900079438590739, 12.64701867748817321, -5.440088680355550821 ) ) ;
#34901 = CARTESIAN_POINT ( 'NONE',  ( -26.69000000000001194, 92.00000000000000000, 9.500000000000000000 ) ) ;
#34902 = PRESENTATION_LAYER_ASSIGNMENT (  '', '', ( #89220 ) ) ;
#34903 = CARTESIAN_POINT ( 'NONE',  ( 12.26500600480481040, 44.99999999999999289, 0.000000000000000000 ) ) ;
#34904 = CARTESIAN_POINT ( 'NONE',  ( 19.42250999205614193, 45.14701867748817676, 5.440088680355555262 ) ) ;
#34905 = CARTESIAN_POINT ( 'NONE',  ( 2.035157376598824452, 48.68868534415483396, 7.964842623401179544 ) ) ;
#34906 = CARTESIAN_POINT ( 'NONE',  ( 6.565887622018943937, 13.08196800326374998, -12.81628187352647608 ) ) ;
#34907 = DIRECTION ( 'NONE',  ( -0.9636304532086248376, 0.000000000000000000, 0.2672383760782501838 ) ) ;
#34908 = DIRECTION ( 'NONE',  ( -1.000000000000000000, 0.000000000000000000, 0.000000000000000000 ) ) ;
#34909 = CARTESIAN_POINT ( 'NONE',  ( 7.361572987183169658, 4.967264484334119601, -9.846743663894592657 ) ) ;
#34910 = CARTESIAN_POINT ( 'NONE',  ( -15.00000000000000000, 84.07179676972448590, 4.000000000000000000 ) ) ;
#34911 = CARTESIAN_POINT ( 'NONE',  ( -0.8801773607110991993, 42.85535201082150536, -2.915334737309923874 ) ) ;
#34912 = CARTESIAN_POINT ( 'NONE',  ( -2.816281873526471635, 8.915301336597083903, -3.434112377981056508 ) ) ;
#34913 = CARTESIAN_POINT ( 'NONE',  ( -0.8801773607110991993, 57.85535201082149825, -2.915334737309923874 ) ) ;
#34914 = CARTESIAN_POINT ( 'NONE',  ( 1.472469842513823179, 20.59226448433411960, -4.923371831947296329 ) ) ;
#34915 = CARTESIAN_POINT ( 'NONE',  ( 0.6178305044545838731, 49.74863466993041072, 9.382169495545420901 ) ) ;
#34916 = CARTESIAN_POINT ( 'NONE',  ( 19.84674366389459266, 8.300597817667451750, 2.638427012816836559 ) ) ;
#34917 = VERTEX_POINT ( 'NONE', #42776 ) ;
#34918 = DIRECTION ( 'NONE',  ( 0.000000000000000000, -1.000000000000000000, 0.000000000000000000 ) ) ;
#34919 = CARTESIAN_POINT ( 'NONE',  ( 19.72487221294570858, 26.86607318730131055, 6.500000000000000888 ) ) ;
#34920 = CARTESIAN_POINT ( 'NONE',  ( 15.44008868035555260, 14.73035201082150536, 9.422509992056143702 ) ) ;
#34921 = CARTESIAN_POINT ( 'NONE',  ( 6.565887622018943937, 63.08196800326376064, -12.81628187352647608 ) ) ;
#34922 = CARTESIAN_POINT ( 'NONE',  ( 5.076628168052703671, 31.84226448433412315, 8.527530157486179263 ) ) ;
#34923 = AXIS2_PLACEMENT_3D ( 'NONE', #66395, #96929, #19428 ) ;
#34924 = CARTESIAN_POINT ( 'NONE',  ( 0.5774900079438590739, 12.64701867748817143, -5.440088680355550821 ) ) ;
#34925 = CARTESIAN_POINT ( 'NONE',  ( -0.8801773607111008646, 3.272018677488171434, 2.915334737309923430 ) ) ;
#34926 = VERTEX_POINT ( 'NONE', #80772 ) ;
#34927 = CARTESIAN_POINT ( 'NONE',  ( 15.44008868035555260, 14.73035201082150536, 9.422509992056143702 ) ) ;
#34928 = EDGE_CURVE ( 'NONE', #875, #62733, #3802, .T. ) ;
#34929 = COLOUR_RGB ( '', 0.31764706, 0.68627451, 0.89019608) ;
#34930 = CARTESIAN_POINT ( 'NONE',  ( 20.88017736071110164, 35.35535201082150536, 2.915334737309930979 ) ) ;
#34932 = CARTESIAN_POINT ( 'NONE',  ( 15.44008868035555793, 21.39701867748817321, -9.422509992056140149 ) ) ;
#34931 = CARTESIAN_POINT ( 'NONE',  ( 6.382347221874423937, 0.5000000000000004441, -13.57444820018227638 ) ) ;
#34933 = VECTOR ( 'NONE', #16301, 1000.000000000000000 ) ;
#34934 = EDGE_LOOP ( 'NONE', ( #15302, #30043, #82146, #66062, #70525, #4719 ) ) ;
#34935 = CARTESIAN_POINT ( 'NONE',  ( 15.44008868035555260, 19.73035201082150536, 9.422509992056143702 ) ) ;
#34936 = CARTESIAN_POINT ( 'NONE',  ( 10.00000000000000000, 64.75893115100078035, -9.846743663894594434 ) ) ;
#34937 = CARTESIAN_POINT ( 'NONE',  ( -1.099225684535947600, 58.70696800326375353, -6.408140936763238038 ) ) ;
#34938 = FACE_OUTER_BOUND ( 'NONE', #31248, .T. ) ;
#34939 = CARTESIAN_POINT ( 'NONE',  ( -2.266590686148945544, 37.22041550158063217, 7.082119434687048631 ) ) ;
#34940 = CARTESIAN_POINT ( 'NONE',  ( -0.8801773607110991993, 42.85535201082150536, -2.915334737309923874 ) ) ;
#34941 = CARTESIAN_POINT ( 'NONE',  ( 10.00000000000000000, 21.81368534415484106, -10.88017736071110342 ) ) ;
#34942 = FACE_OUTER_BOUND ( 'NONE', #41421, .T. ) ;
#34943 = CARTESIAN_POINT ( 'NONE',  ( 9.879999999999990123, 20.99999999999999645, 0.000000000000000000 ) ) ;
#34944 = CARTESIAN_POINT ( 'NONE',  ( 1.472469842513823179, 55.59226448433412315, -4.923371831947296329 ) ) ;
#34945 = CARTESIAN_POINT ( 'NONE',  ( 18.52753015748617571, 18.09226448433411960, 4.923371831947298993 ) ) ;
#34946 = CARTESIAN_POINT ( 'NONE',  ( 9.382169495545419124, -29.00136533006957862, 9.382169495545417348 ) ) ;
#34947 =( BOUNDED_CURVE ( )  B_SPLINE_CURVE ( 2, ( #31534, #23082, #8069, #38566, #22092, #69061, #77045, #52569, #31042 ),
 .UNSPECIFIED., .F., .F. ) 
 B_SPLINE_CURVE_WITH_KNOTS ( ( 3, 2, 2, 2, 3 ),
 ( 0.1525141644748393699, 0.1547619047619047672, 0.1607142857142857262, 0.1666666666666666574, 0.1689144069537320547 ),
 .UNSPECIFIED. ) 
 CURVE ( )  GEOMETRIC_REPRESENTATION_ITEM ( )  RATIONAL_B_SPLINE_CURVE ( ( 0.9839835555609424134, 0.9871328979762477029, 1.000000000000000000, 0.9659258262890683122, 1.000000000000000000, 0.9659258262890683122, 1.000000000000000000, 0.9871328979762477029, 0.9839835555609424134 ) ) 
 REPRESENTATION_ITEM ( '' )  );
#34948 = CARTESIAN_POINT ( 'NONE',  ( -0.8801773607111009756, 13.06368534415483929, 1.068504757029289695E-15 ) ) ;
#34949 = CARTESIAN_POINT ( 'NONE',  ( 14.92337183194729633, 7.675597817667451750, 8.527530157486181039 ) ) ;
#34950 = CARTESIAN_POINT ( 'NONE',  ( 6.565887622018943937, 13.08196800326374998, -12.81628187352647608 ) ) ;
#34951 = CARTESIAN_POINT ( 'NONE',  ( 0.5774900079438607392, 63.48035201082149825, 5.440088680355550821 ) ) ;
#34953 = CARTESIAN_POINT ( 'NONE',  ( 3.591859063236763294, 63.29030133659708923, -11.09922568453595026 ) ) ;
#34952 = CARTESIAN_POINT ( 'NONE',  ( 15.44008868035555260, 24.73035201082150891, 9.422509992056143702 ) ) ;
#34954 = CARTESIAN_POINT ( 'NONE',  ( 20.36894250292379382, 33.67874883491396076, 10.36894250292379205 ) ) ;
#34955 = SURFACE_SIDE_STYLE ('',( #11972 ) ) ;
#34956 =( BOUNDED_CURVE ( )  B_SPLINE_CURVE ( 3, ( #50367, #13360, #51857, #74340 ),
 .UNSPECIFIED., .F., .F. ) 
 B_SPLINE_CURVE_WITH_KNOTS ( ( 4, 4 ),
 ( 4.712388980384689674, 6.283185307179586232 ),
 .UNSPECIFIED. ) 
 CURVE ( )  GEOMETRIC_REPRESENTATION_ITEM ( )  RATIONAL_B_SPLINE_CURVE ( ( 1.000000000000000000, 0.8047378541243649375, 0.8047378541243649375, 1.000000000000000000 ) ) 
 REPRESENTATION_ITEM ( '' )  );
#34957 = CARTESIAN_POINT ( 'NONE',  ( 13.43411237798105340, 60.58196800326376064, 12.81628187352647963 ) ) ;
#34958 = ORIENTED_EDGE ( 'NONE', *, *, #91567, .F. ) ;
#34959 = CARTESIAN_POINT ( 'NONE',  ( -1.099225684535947600, 3.706968003263753531, -6.408140936763238038 ) ) ;
#34960 = CARTESIAN_POINT ( 'NONE',  ( -0.3289641300568005855, 14.27164270246084143, -5.963430220938281678 ) ) ;
#34961 = CARTESIAN_POINT ( 'NONE',  ( 7.084665262690076126, 34.10535201082151247, 10.88017736071109987 ) ) ;
#34962 = PLANE ( 'NONE',  #88833 ) ;
#34963 = ORIENTED_EDGE ( 'NONE', *, *, #56725, .F. ) ;
#34964 = CARTESIAN_POINT ( 'NONE',  ( 12.63842701281683034, 12.46726448433411782, 9.846743663894596210 ) ) ;
#34965 = VECTOR ( 'NONE', #31594, 1000.000000000000000 ) ;
#34966 = CARTESIAN_POINT ( 'NONE',  ( 5.076628168052703671, 11.84226448433411960, 8.527530157486179263 ) ) ;
#34967 = CARTESIAN_POINT ( 'NONE',  ( 2.791683348922240793, 16.63393115100078745, 7.208316651077764092 ) ) ;
#34968 = CARTESIAN_POINT ( 'NONE',  ( 19.84674366389459266, 13.71726448433411782, -2.638427012816827677 ) ) ;
#34969 = CARTESIAN_POINT ( 'NONE',  ( 12.63842701281683034, 2.467264484334118269, 9.846743663894596210 ) ) ;
#34970 = EDGE_CURVE ( 'NONE', #93851, #54718, #4784, .T. ) ;
#34972 = LINE ( 'NONE', #81956, #21621 ) ;
#34971 = CARTESIAN_POINT ( 'NONE',  ( 17.20831665107776587, 2.883931151000785231, 7.208316651077764980 ) ) ;
#34973 = CARTESIAN_POINT ( 'NONE',  ( 14.92337183194729988, 4.342264484334117824, -8.527530157486177487 ) ) ;
#34974 = CARTESIAN_POINT ( 'NONE',  ( 14.92337183194729633, 17.67559781766745175, 8.527530157486181039 ) ) ;
#34975 = CARTESIAN_POINT ( 'NONE',  ( -23.44000000000000838, 92.00000000000000000, 9.500000000000000000 ) ) ;
#34976 = CARTESIAN_POINT ( 'NONE',  ( 0.6178305044545838731, 4.748634669930420493, 9.382169495545420901 ) ) ;
#34977 = ORIENTED_EDGE ( 'NONE', *, *, #83021, .F. ) ;
#34978 = ORIENTED_EDGE ( 'NONE', *, *, #51562, .F. ) ;
#34979 = CARTESIAN_POINT ( 'NONE',  ( 20.88017736071110164, 5.355352010821502695, 2.915334737309930979 ) ) ;
#34980 = CARTESIAN_POINT ( 'NONE',  ( -2.266590686148945544, 16.38708216824730357, -7.082119434687050408 ) ) ;
#34981 = PLANE ( 'NONE',  #2480 ) ;
#34982 = CARTESIAN_POINT ( 'NONE',  ( 17.08211943468705130, 13.47041550158063572, 12.26659068614894998 ) ) ;
#34983 = CARTESIAN_POINT ( 'NONE',  ( 10.00000000000000178, 38.05374883491396787, 14.16423886937410082 ) ) ;
#34984 = CARTESIAN_POINT ( 'NONE',  ( -4.164238869374099927, 2.012082168247300906, 3.795296366450308767 ) ) ;
#34985 = CARTESIAN_POINT ( 'NONE',  ( 19.42250999205614193, 40.14701867748817676, 5.440088680355555262 ) ) ;
#34986 = DIRECTION ( 'NONE',  ( 0.000000000000000000, 1.000000000000000000, 0.000000000000000000 ) ) ;
#34987 = CARTESIAN_POINT ( 'NONE',  ( 0.1532563361054083140, 16.00893115100078390, 1.131784320476157264E-15 ) ) ;
#34989 = CARTESIAN_POINT ( 'NONE',  ( 10.00000000000000178, 27.25893115100078390, 9.846743663894594434 ) ) ;
#34988 = CARTESIAN_POINT ( 'NONE',  ( -0.8801773607111009756, 63.06368534415484106, 1.068504757029289695E-15 ) ) ;
#34990 = ORIENTED_EDGE ( 'NONE', *, *, #24734, .T. ) ;
#34991 = CARTESIAN_POINT ( 'NONE',  ( 12.91533473730993009, 11.60535201082150714, -10.88017736071109987 ) ) ;
#34992 = CARTESIAN_POINT ( 'NONE',  ( 21.09922568453595559, 52.04030133659708923, -6.408140936763230044 ) ) ;
#34993 = CARTESIAN_POINT ( 'NONE',  ( 10.00000000000000000, 49.75893115100078745, -9.846743663894594434 ) ) ;
#34994 =( GEOMETRIC_REPRESENTATION_CONTEXT ( 3 ) GLOBAL_UNCERTAINTY_ASSIGNED_CONTEXT ( ( #35285 ) ) GLOBAL_UNIT_ASSIGNED_CONTEXT ( ( #67058, #69039, #37563 ) ) REPRESENTATION_CONTEXT ( 'NONE', 'WORKASPACE' ) );
#34995 = CARTESIAN_POINT ( 'NONE',  ( 5.500000000000000000, 11.00000000000000000, 6.500000000000000888 ) ) ;
#34996 = CARTESIAN_POINT ( 'NONE',  ( 16.40814093676324603, 22.45696800326375353, -11.09922568453594671 ) ) ;
#34997 = CARTESIAN_POINT ( 'NONE',  ( -14.16423886937410082, -28.19625116508602503, 4.336808689942017736E-15 ) ) ;
#34998 = CARTESIAN_POINT ( 'NONE',  ( 18.52753015748618282, 43.92559781766745175, -4.923371831947291888 ) ) ;
#34999 = CARTESIAN_POINT ( 'NONE',  ( -0.3689425029237881626, 17.42874883491397142, 10.36894250292379027 ) ) ;
#35000 = EDGE_CURVE ( 'NONE', #7097, #37440, #36376, .T. ) ;
#35001 = ORIENTED_EDGE ( 'NONE', *, *, #26901, .F. ) ;
#35002 = CARTESIAN_POINT ( 'NONE',  ( 7.084665262690076126, 49.10535201082149825, 10.88017736071109987 ) ) ;
#35003 = CARTESIAN_POINT ( 'NONE',  ( 19.42250999205614548, 50.98035201082151247, -5.440088680355545492 ) ) ;
#35004 = CARTESIAN_POINT ( 'NONE',  ( -0.3689425029237898834, 46.17874883491397497, -10.36894250292378850 ) ) ;
#35005 = CARTESIAN_POINT ( 'NONE',  ( 0.1532563361054083140, 56.00893115100078745, 1.131784320476157264E-15 ) ) ;
#35006 = LINE ( 'NONE', #4544, #67252 ) ;
#35007 = CARTESIAN_POINT ( 'NONE',  ( -0.8801773607110991993, 37.85535201082151247, -2.915334737309923874 ) ) ;
#35008 = EDGE_CURVE ( 'NONE', #81310, #7169, #10592, .T. ) ;
#35009 = CYLINDRICAL_SURFACE ( 'NONE', #32649, 0.5000000000000004441 ) ;
#35010 = AXIS2_PLACEMENT_3D ( 'NONE', #66689, #97707, #51193 ) ;
#35011 = CARTESIAN_POINT ( 'NONE',  ( 22.81628187352648496, 21.83196800326374643, -3.434112377981050290 ) ) ;
#35012 = CARTESIAN_POINT ( 'NONE',  ( 19.84674366389459266, 58.30059781766745886, 2.638427012816836559 ) ) ;
#35013 = CARTESIAN_POINT ( 'NONE',  ( 5.440088680355549045, 21.39701867748818032, -9.422509992056141925 ) ) ;
#35014 = CARTESIAN_POINT ( 'NONE',  ( 17.96484262340118221, 6.188685344154836621, -7.964842623401177768 ) ) ;
#35015 = CARTESIAN_POINT ( 'NONE',  ( -0.8801773607111009756, 63.06368534415484106, 1.068504757029289695E-15 ) ) ;
#35016 = ORIENTED_EDGE ( 'NONE', *, *, #79791, .F. ) ;
#35017 = VECTOR ( 'NONE', #69989, 1000.000000000000000 ) ;
#35018 = CARTESIAN_POINT ( 'NONE',  ( 19.42250999205614193, 5.147018677488171434, 5.440088680355555262 ) ) ;
#35019 = CARTESIAN_POINT ( 'NONE',  ( 20.03932841506542673, 65.62161441960505215, -6.397827110478995216 ) ) ;
#35020 = CARTESIAN_POINT ( 'NONE',  ( 12.91533473730993009, 61.60535201082150536, -10.88017736071109987 ) ) ;
#35021 = CARTESIAN_POINT ( 'NONE',  ( 10.00000000000000178, 2.258931151000784787, 9.846743663894594434 ) ) ;
#35022 = CARTESIAN_POINT ( 'NONE',  ( 17.81748129626896215, 78.53842255729841781, -4.009548935143140369 ) ) ;
#35023 = CARTESIAN_POINT ( 'NONE',  ( 0.1532563361054082862, 31.21726448433412315, 2.638427012816831674 ) ) ;
#35024 = CARTESIAN_POINT ( 'NONE',  ( -0.8801773607110991993, 22.85535201082150181, -2.915334737309923874 ) ) ;
#35025 = CARTESIAN_POINT ( 'NONE',  ( 22.81628187352648496, 11.83196800326375531, -3.434112377981050290 ) ) ;
#35027 = CARTESIAN_POINT ( 'NONE',  ( -8.722765153436172980, 15.00000000000000888, -11.74102699209696432 ) ) ;
#35026 = CARTESIAN_POINT ( 'NONE',  ( 17.96484262340118221, 34.93868534415482685, 7.964842623401181321 ) ) ;
#35028 = CARTESIAN_POINT ( 'NONE',  ( 22.81628187352648496, 36.83196800326376064, -3.434112377981050290 ) ) ;
#35029 = ORIENTED_EDGE ( 'NONE', *, *, #78782, .F. ) ;
#35030 = CARTESIAN_POINT ( 'NONE',  ( 2.035157376598824452, 58.68868534415482685, 7.964842623401179544 ) ) ;
#35032 = CARTESIAN_POINT ( 'NONE',  ( 19.84674366389459266, 18.71726448433411960, -2.638427012816827677 ) ) ;
#35031 = CARTESIAN_POINT ( 'NONE',  ( 3.591859063236763294, 18.29030133659708568, -11.09922568453595026 ) ) ;
#35033 = CARTESIAN_POINT ( 'NONE',  ( 0.5774900079438590739, 22.64701867748817321, -5.440088680355550821 ) ) ;
#35034 = CARTESIAN_POINT ( 'NONE',  ( 17.08211943468705130, 58.47041550158063927, 12.26659068614894998 ) ) ;
#35035 = CARTESIAN_POINT ( 'NONE',  ( 7.361572987183169658, 49.96726448433410894, -9.846743663894592657 ) ) ;
#35036 = AXIS2_PLACEMENT_3D ( 'NONE', #25600, #55082, #46602 ) ;
#35037 = CARTESIAN_POINT ( 'NONE',  ( 17.20831665107776587, 4.133931151000785675, -7.208316651077762316 ) ) ;
#35038 = ADVANCED_FACE ( 'NONE', ( #64759 ), #60107, .F. ) ;
#35039 = CARTESIAN_POINT ( 'NONE',  ( 12.91533473730992121, 59.52201867748816966, 10.88017736071110164 ) ) ;
#35040 = FILL_AREA_STYLE ('',( #42559 ) ) ;
#35041 = CARTESIAN_POINT ( 'NONE',  ( 17.08211943468705130, 33.47041550158063927, 12.26659068614894998 ) ) ;
#35042 = EDGE_CURVE ( 'NONE', #6459, #56172, #65745, .T. ) ;
#35043 = CARTESIAN_POINT ( 'NONE',  ( 20.15039907845753575, 7.627771745786129820, -6.262539305110077059 ) ) ;
#35044 = SURFACE_STYLE_USAGE ( .BOTH. , #67041 ) ;
#35045 = VERTEX_POINT ( 'NONE', #95263 ) ;
#35046 = ORIENTED_EDGE ( 'NONE', *, *, #54951, .T. ) ;
#35047 = CARTESIAN_POINT ( 'NONE',  ( 17.08211943468705130, 48.47041550158063927, 12.26659068614894998 ) ) ;
#35048 = CARTESIAN_POINT ( 'NONE',  ( 22.26659068614895176, 49.72041550158063927, -7.082119434687042414 ) ) ;
#35049 = CARTESIAN_POINT ( 'NONE',  ( 18.52753015748617571, 18.09226448433411960, 4.923371831947298993 ) ) ;
#35050 = CARTESIAN_POINT ( 'NONE',  ( -2.816281873526473856, 24.12363466993042138, 9.499525473075851096E-16 ) ) ;
#35051 = DIRECTION ( 'NONE',  ( 1.000000000000000000, 0.000000000000000000, 0.000000000000000000 ) ) ;
#35052 = CARTESIAN_POINT ( 'NONE',  ( -0.4957494408796453977, 15.11603861882761812, 10.00000000000000000 ) ) ;
#35053 =( NAMED_UNIT ( * ) SI_UNIT ( $, .STERADIAN. ) SOLID_ANGLE_UNIT ( ) );
#35054 = CARTESIAN_POINT ( 'NONE',  ( -4.164238869374099039, 46.80374883491397497, 8.674139862899312516E-16 ) ) ;
#35055 = CARTESIAN_POINT ( 'NONE',  ( 10.19513985507833276, 0.5000000000000004441, -11.00268709613217055 ) ) ;
#35056 = CARTESIAN_POINT ( 'NONE',  ( 12.63842701281683922, 9.550597817667449974, -9.846743663894590881 ) ) ;
#35057 = EDGE_CURVE ( 'NONE', #50602, #81607, #13248, .T. ) ;
#35058 = CARTESIAN_POINT ( 'NONE',  ( -13.14228782657329653, 0.5000000000000004441, -7.230509711182418364 ) ) ;
#35059 = CARTESIAN_POINT ( 'NONE',  ( 9.846743663894590881, 3.300597817667453526, 2.638427012816828565 ) ) ;
#35060 = VERTEX_POINT ( 'NONE', #42277 ) ;
#35061 = SURFACE_STYLE_USAGE ( .BOTH. , #72567 ) ;
#35062 = ORIENTED_EDGE ( 'NONE', *, *, #18270, .T. ) ;
#35063 = DIRECTION ( 'NONE',  ( 0.000000000000000000, 1.000000000000000000, 0.000000000000000000 ) ) ;
#35064 = ORIENTED_EDGE ( 'NONE', *, *, #46528, .F. ) ;
#35066 = CARTESIAN_POINT ( 'NONE',  ( 0.5774900079438590739, 27.64701867748817676, -5.440088680355550821 ) ) ;
#35065 = CARTESIAN_POINT ( 'NONE',  ( -0.8801773607111008646, 13.27201867748817321, 2.915334737309923430 ) ) ;
#35068 = CARTESIAN_POINT ( 'NONE',  ( 21.09922568453595559, 17.04030133659708923, -6.408140936763230044 ) ) ;
#35067 = CARTESIAN_POINT ( 'NONE',  ( 0.1532563361054083140, 46.00893115100079456, 1.131784320476157264E-15 ) ) ;
#35069 = SURFACE_STYLE_FILL_AREA ( #71622 ) ;
#35070 = CARTESIAN_POINT ( 'NONE',  ( 9.879999999999988347, 26.99999999999999645, -2.900000000000000799 ) ) ;
#35071 = CARTESIAN_POINT ( 'NONE',  ( 0.6178305044545838731, 19.74863466993042138, 9.382169495545420901 ) ) ;
#35072 = ORIENTED_EDGE ( 'NONE', *, *, #59271, .T. ) ;
#35073 = CARTESIAN_POINT ( 'NONE',  ( 5.076628168052704559, 35.17559781766745175, -8.527530157486179263 ) ) ;
#35074 = CARTESIAN_POINT ( 'NONE',  ( -4.164238869374098151, 66.59541550158060375, -3.795296366450310543 ) ) ;
#35075 = ORIENTED_EDGE ( 'NONE', *, *, #63155, .F. ) ;
#35076 = CARTESIAN_POINT ( 'NONE',  ( 19.42250999205614193, 10.14701867748816966, 5.440088680355555262 ) ) ;
#35077 = ORIENTED_EDGE ( 'NONE', *, *, #19140, .T. ) ;
#35078 = CARTESIAN_POINT ( 'NONE',  ( 4.559911319644449179, 48.89701867748817676, 9.422509992056141925 ) ) ;
#35079 = VECTOR ( 'NONE', #80422, 1000.000000000000000 ) ;
#35080 = CARTESIAN_POINT ( 'NONE',  ( -0.8801773607111009756, 43.06368534415484106, 1.068504757029289695E-15 ) ) ;
#35081 = CARTESIAN_POINT ( 'NONE',  ( 20.88017736071110519, 45.56368534415484106, 2.639326808657452039E-16 ) ) ;
#35082 =( NAMED_UNIT ( * ) SI_UNIT ( $, .STERADIAN. ) SOLID_ANGLE_UNIT ( ) );
#35083 = CARTESIAN_POINT ( 'NONE',  ( -0.8801773607110991993, 42.85535201082150536, -2.915334737309923874 ) ) ;
#35084 =( GEOMETRIC_REPRESENTATION_CONTEXT ( 3 ) GLOBAL_UNCERTAINTY_ASSIGNED_CONTEXT ( ( #26187 ) ) GLOBAL_UNIT_ASSIGNED_CONTEXT ( ( #59311, #69786, #61769 ) ) REPRESENTATION_CONTEXT ( 'NONE', 'WORKASPACE' ) );
#35085 = CARTESIAN_POINT ( 'NONE',  ( 21.92686044187656691, 64.95379003517449235, 3.195792623639537755 ) ) ;
#35086 = VECTOR ( 'NONE', #45158, 1000.000000000000000 ) ;
#35087 = EDGE_CURVE ( 'NONE', #89457, #8159, #32998, .T. ) ;
#35089 = ORIENTED_EDGE ( 'NONE', *, *, #1974, .F. ) ;
#35088 = PLANE ( 'NONE',  #71273 ) ;
#35090 = CARTESIAN_POINT ( 'NONE',  ( 2.791683348922240793, 26.63393115100078745, 7.208316651077764092 ) ) ;
#35091 = EDGE_LOOP ( 'NONE', ( #72136, #33102, #95414 ) ) ;
#35092 = CARTESIAN_POINT ( 'NONE',  ( 12.63842701281683034, 57.46726448433411605, 9.846743663894596210 ) ) ;
#35093 = EDGE_CURVE ( 'NONE', #43087, #55079, #80889, .T. ) ;
#35094 = CARTESIAN_POINT ( 'NONE',  ( 4.838527690343521925, 0.3640475087720984604, 14.19819177887730888 ) ) ;
#35095 = FACE_OUTER_BOUND ( 'NONE', #51797, .T. ) ;
#35096 = ORIENTED_EDGE ( 'NONE', *, *, #98248, .F. ) ;
#35097 = VECTOR ( 'NONE', #43850, 1000.000000000000000 ) ;
#35098 = CARTESIAN_POINT ( 'NONE',  ( 18.72515096720579209, 51.07228050351030646, -6.499999999999869438 ) ) ;
#35099 = FACE_OUTER_BOUND ( 'NONE', #89104, .T. ) ;
#35100 = CARTESIAN_POINT ( 'NONE',  ( 0.1532563361054082862, 61.21726448433412315, 2.638427012816831674 ) ) ;
#35101 = CARTESIAN_POINT ( 'NONE',  ( -0.3689425029237881626, 67.42874883491396076, 10.36894250292379027 ) ) ;
#35102 = FACE_OUTER_BOUND ( 'NONE', #68189, .T. ) ;
#35103 = ORIENTED_EDGE ( 'NONE', *, *, #87810, .T. ) ;
#35104 = CARTESIAN_POINT ( 'NONE',  ( 0.000000000000000000, 15.00000000000000000, 0.000000000000000000 ) ) ;
#35105 = CARTESIAN_POINT ( 'NONE',  ( 17.20831665107776587, 34.13393115100078745, -7.208316651077762316 ) ) ;
#35106 = CARTESIAN_POINT ( 'NONE',  ( 22.81628187352648496, 61.83196800326376774, -3.434112377981050290 ) ) ;
#35107 = CARTESIAN_POINT ( 'NONE',  ( 16.40814093676323893, 0.7903013365970867898, 11.09922568453595026 ) ) ;
#35108 = CARTESIAN_POINT ( 'NONE',  ( 10.00000000000000000, 14.75893115100078568, -9.846743663894594434 ) ) ;
#35109 = DIRECTION ( 'NONE',  ( 1.000000000000000000, 0.000000000000000000, 0.000000000000000000 ) ) ;
#35110 = CARTESIAN_POINT ( 'NONE',  ( 17.20831665107776587, 9.133931151000787452, -7.208316651077762316 ) ) ;
#35111 = CARTESIAN_POINT ( 'NONE',  ( 0.1532563361054100626, 55.80059781766745175, -2.638427012816831230 ) ) ;
#35112 = DIRECTION ( 'NONE',  ( 0.8070303256584298035, -0.5905099943842175847, 0.000000000000000000 ) ) ;
#35113 = EDGE_CURVE ( 'NONE', #47034, #55759, #27749, .T. ) ;
#35114 = ORIENTED_EDGE ( 'NONE', *, *, #85593, .T. ) ;
#35115 = CARTESIAN_POINT ( 'NONE',  ( 15.44008868035555793, 6.397018677488171434, -9.422509992056140149 ) ) ;
#35116 = CARTESIAN_POINT ( 'NONE',  ( 6.204703633549690345, 10.76208216824729824, -14.16423886937410259 ) ) ;
#35117 = CARTESIAN_POINT ( 'NONE',  ( 12.63842701281683922, 14.55059781766744997, -9.846743663894590881 ) ) ;
#35118 = CARTESIAN_POINT ( 'NONE',  ( 20.88017736071110164, 55.35535201082149825, 2.915334737309930979 ) ) ;
#35120 = CARTESIAN_POINT ( 'NONE',  ( 10.00000000000000178, 69.31368534415484817, 10.88017736071110342 ) ) ;
#35119 = CARTESIAN_POINT ( 'NONE',  ( 6.565887622018943937, 30.16530133659708568, 12.81628187352647430 ) ) ;
#35121 = CARTESIAN_POINT ( 'NONE',  ( 2.035157376598822676, 2.438685344154837953, -7.964842623401177768 ) ) ;
#35122 = EDGE_CURVE ( 'NONE', #87107, #56172, #24543, .T. ) ;
#35123 = FACE_OUTER_BOUND ( 'NONE', #98630, .T. ) ;
#35124 = DIRECTION ( 'NONE',  ( -0.000000000000000000, -1.000000000000000000, -0.000000000000000000 ) ) ;
#35125 = CARTESIAN_POINT ( 'NONE',  ( 16.40814093676324603, 7.456968003263754419, -11.09922568453594671 ) ) ;
#35126 = CARTESIAN_POINT ( 'NONE',  ( 3.591859063236761518, -0.04303199673624671928, 11.09922568453594849 ) ) ;
#35127 = CARTESIAN_POINT ( 'NONE',  ( 7.361572987183169658, 9.967264484334119601, -9.846743663894592657 ) ) ;
#35128 = CARTESIAN_POINT ( 'NONE',  ( -10.88017736071110164, -27.14464798917849109, -2.915334737309917212 ) ) ;
#35129 = CARTESIAN_POINT ( 'NONE',  ( 19.38216949554541202, 25.99863466993042138, 9.382169495545424454 ) ) ;
#35130 = CARTESIAN_POINT ( 'NONE',  ( 14.74963345907815437, 0.04922511925147114720, -0.3072669459660632985 ) ) ;
#35131 = CARTESIAN_POINT ( 'NONE',  ( 0.5774900079438590739, 22.64701867748817321, -5.440088680355550821 ) ) ;
#35132 = LINE ( 'NONE', #42173, #46818 ) ;
#35133 = CARTESIAN_POINT ( 'NONE',  ( 2.917880565312948704, 52.63708216824730357, 12.26659068614894643 ) ) ;
#35134 = CARTESIAN_POINT ( 'NONE',  ( -3.749999999999993783, 43.00000000000000711, 4.000000000000000000 ) ) ;
#35135 = CARTESIAN_POINT ( 'NONE',  ( 22.81628187352647785, 51.41530133659708923, 3.434112377981063169 ) ) ;
#35136 = CARTESIAN_POINT ( 'NONE',  ( -0.8801773607111008646, 28.27201867748817321, 2.915334737309923430 ) ) ;
#35137 = PRESENTATION_LAYER_ASSIGNMENT (  '', '', ( #33568 ) ) ;
#35138 = CARTESIAN_POINT ( 'NONE',  ( 2.791683348922237240, 55.38393115100078745, -7.208316651077763204 ) ) ;
#35139 = CARTESIAN_POINT ( 'NONE',  ( 20.88017736071110519, 55.56368534415484817, 2.639326808657452039E-16 ) ) ;
#35140 = CARTESIAN_POINT ( 'NONE',  ( 24.16423886937409904, 29.09541550158063572, 3.795296366450317205 ) ) ;
#35141 = DIRECTION ( 'NONE',  ( -0.000000000000000000, -1.000000000000000000, -0.000000000000000000 ) ) ;
#35142 = UNCERTAINTY_MEASURE_WITH_UNIT (LENGTH_MEASURE( 1.000000000000000082E-05 ), #48010, 'distance_accuracy_value', 'NONE');
#35143 = CARTESIAN_POINT ( 'NONE',  ( 12.63842701281683034, 32.46726448433412315, 9.846743663894596210 ) ) ;
#35144 = SURFACE_STYLE_USAGE ( .BOTH. , #66136 ) ;
#35145 = CARTESIAN_POINT ( 'NONE',  ( -1.099225684535947600, -1.293031996736246469, -6.408140936763238038 ) ) ;
#35146 = ORIENTED_EDGE ( 'NONE', *, *, #59717, .F. ) ;
#35147 = CARTESIAN_POINT ( 'NONE',  ( 20.88017736071110519, 30.56368534415484106, 2.639326808657452039E-16 ) ) ;
#35148 = LINE ( 'NONE', #5169, #78027 ) ;
#35149 = CARTESIAN_POINT ( 'NONE',  ( 6.937721053838227014, -80.66520463107747219, 3.750000000000001776 ) ) ;
#35150 = VECTOR ( 'NONE', #75623, 1000.000000000000000 ) ;
#35151 = CARTESIAN_POINT ( 'NONE',  ( 12.91533473730993009, 11.60535201082150714, -10.88017736071109987 ) ) ;
#35152 = CARTESIAN_POINT ( 'NONE',  ( 2.917880565312950480, 25.97041550158063572, -12.26659068614894821 ) ) ;
#35153 = CARTESIAN_POINT ( 'NONE',  ( 19.84674366389459266, 8.300597817667451750, 2.638427012816836559 ) ) ;
#35154 = CARTESIAN_POINT ( 'NONE',  ( 7.361572987183169658, 64.96726448433412315, -9.846743663894592657 ) ) ;
#35155 = CARTESIAN_POINT ( 'NONE',  ( 12.91533473730992121, 39.52201867748817676, 10.88017736071110164 ) ) ;
#35156 = CARTESIAN_POINT ( 'NONE',  ( 19.72487221294570858, 64.78217586085237656, 6.499999999999992895 ) ) ;
#35157 = LINE ( 'NONE', #96179, #84017 ) ;
#35158 = CIRCLE ( 'NONE', #86283, 1.500000000000001332 ) ;
#35159 = EDGE_CURVE ( 'NONE', #75802, #49611, #88883, .T. ) ;
#35160 = VERTEX_POINT ( 'NONE', #5273 ) ;
#35161 = SURFACE_SIDE_STYLE ('',( #3217 ) ) ;
#35162 = CARTESIAN_POINT ( 'NONE',  ( 2.791683348922237240, 40.38393115100078035, -7.208316651077763204 ) ) ;
#35163 = ORIENTED_EDGE ( 'NONE', *, *, #61875, .F. ) ;
#35164 = VERTEX_POINT ( 'NONE', #81250 ) ;
#35165 = CARTESIAN_POINT ( 'NONE',  ( 1.983216688680843109, 15.00000000000000000, 14.11131997956739070 ) ) ;
#35166 = CARTESIAN_POINT ( 'NONE',  ( 10.00000000000000178, 8.053748834913967869, 14.16423886937410082 ) ) ;
#35167 = CARTESIAN_POINT ( 'NONE',  ( 10.00000000000000178, 13.05374883491396787, 14.16423886937410082 ) ) ;
#35168 = CARTESIAN_POINT ( 'NONE',  ( -0.8801773607111009756, 43.06368534415484106, 1.068504757029289695E-15 ) ) ;
#35169 = CARTESIAN_POINT ( 'NONE',  ( -4.164238869374098151, 51.59541550158063217, -3.795296366450310543 ) ) ;
#35170 = CARTESIAN_POINT ( 'NONE',  ( 10.00000000000000178, 37.25893115100078745, 9.846743663894594434 ) ) ;
#35171 =( LENGTH_UNIT ( ) NAMED_UNIT ( * ) SI_UNIT ( .MILLI., .METRE. ) );
#35173 = CARTESIAN_POINT ( 'NONE',  ( -1.099225684535947600, 9.540301336597087456, 6.408140936763237150 ) ) ;
#35172 = CARTESIAN_POINT ( 'NONE',  ( -0.8801773607111008646, 33.27201867748817676, 2.915334737309923430 ) ) ;
#35174 = CARTESIAN_POINT ( 'NONE',  ( -2.266590686148945544, 6.387082168247300906, -7.082119434687050408 ) ) ;
#35175 = CARTESIAN_POINT ( 'NONE',  ( 24.16423886937410614, 49.30374883491396787, 8.672049930838204340E-16 ) ) ;
#35176 = CARTESIAN_POINT ( 'NONE',  ( 0.5774900079438607392, 3.480352010821504916, 5.440088680355550821 ) ) ;
#35177 = CARTESIAN_POINT ( 'NONE',  ( -0.3289641300568009741, 67.24545670184114954, -5.963430220938281678 ) ) ;
#35178 = FACE_OUTER_BOUND ( 'NONE', #63679, .T. ) ;
#35179 = CARTESIAN_POINT ( 'NONE',  ( 4.923371831947301658, -32.32440218233254825, 8.527530157486175710 ) ) ;
#35180 = VERTEX_POINT ( 'NONE', #43247 ) ;
#35181 = DIRECTION ( 'NONE',  ( -0.000000000000000000, -0.000000000000000000, -1.000000000000000000 ) ) ;
#35182 = ORIENTED_EDGE ( 'NONE', *, *, #91387, .F. ) ;
#35183 = VERTEX_POINT ( 'NONE', #58232 ) ;
#35184 = CARTESIAN_POINT ( 'NONE',  ( -4.164238869374099927, 52.01208216824729647, 3.795296366450308767 ) ) ;
#35185 = CARTESIAN_POINT ( 'NONE',  ( 7.361572987183170547, 52.05059781766745175, 9.846743663894590881 ) ) ;
#35186 = CARTESIAN_POINT ( 'NONE',  ( 4.559911319644449179, 52.23035201082151247, -9.422509992056141925 ) ) ;
#35187 = CARTESIAN_POINT ( 'NONE',  ( 19.80448550324510038, 36.82703681773342907, 6.500000000002679634 ) ) ;
#35188 = CARTESIAN_POINT ( 'NONE',  ( 10.00000000000000000, 56.81368534415484106, -10.88017736071110342 ) ) ;
#35189 = PRESENTATION_LAYER_ASSIGNMENT (  '', '', ( #124 ) ) ;
#35190 = CARTESIAN_POINT ( 'NONE',  ( 21.09922568453594849, 56.20696800326375353, 6.408140936763242479 ) ) ;
#35191 = CARTESIAN_POINT ( 'NONE',  ( 12.81628187352647252, 6.831968003263756195, -3.434112377981059172 ) ) ;
#35192 = ORIENTED_EDGE ( 'NONE', *, *, #36865, .F. ) ;
#35193 = CARTESIAN_POINT ( 'NONE',  ( 10.00000000000000000, 15.55374883491396787, -14.16423886937410082 ) ) ;
#35194 = EDGE_LOOP ( 'NONE', ( #78004, #14791, #71061, #57122 ) ) ;
#35195 = CARTESIAN_POINT ( 'NONE',  ( 16.40814093676324603, 22.45696800326375353, -11.09922568453594671 ) ) ;
#35196 = ORIENTED_EDGE ( 'NONE', *, *, #5571, .T. ) ;
#35197 = CARTESIAN_POINT ( 'NONE',  ( 16.40814093676323893, 50.79030133659708923, 11.09922568453595026 ) ) ;
#35198 = CARTESIAN_POINT ( 'NONE',  ( 7.361572987183170547, 42.05059781766745886, 9.846743663894590881 ) ) ;
#35199 = CARTESIAN_POINT ( 'NONE',  ( -0.8801773607111008646, 8.272018677488171434, 2.915334737309923430 ) ) ;
#35200 = CARTESIAN_POINT ( 'NONE',  ( -1.099225684535947600, 49.54030133659708923, 6.408140936763237150 ) ) ;
#35201 = CARTESIAN_POINT ( 'NONE',  ( -45.94000000000000483, 103.9981609152045650, -5.961202730336930600 ) ) ;
#35202 = CARTESIAN_POINT ( 'NONE',  ( 14.92337183194729988, 39.34226448433412315, -8.527530157486177487 ) ) ;
#35205 = ORIENTED_EDGE ( 'NONE', *, *, #21764, .F. ) ;
#35204 = VECTOR ( 'NONE', #62667, 1000.000000000000000 ) ;
#35203 = DIRECTION ( 'NONE',  ( -0.000000000000000000, -1.000000000000000000, -0.000000000000000000 ) ) ;
#35206 = CARTESIAN_POINT ( 'NONE',  ( -0.2838433074297238012, 13.12729635533385597, -9.500000000000000000 ) ) ;
#35207 = DIRECTION ( 'NONE',  ( 0.000000000000000000, -1.000000000000000000, 0.000000000000000000 ) ) ;
#35208 = ADVANCED_FACE ( 'NONE', ( #96772 ), #44231, .F. ) ;
#35209 = CARTESIAN_POINT ( 'NONE',  ( 13.61802159414299140, -2.298423902374543181E-15, 5.334603887713582182 ) ) ;
#35210 = CARTESIAN_POINT ( 'NONE',  ( 19.84674366389459621, 23.50893115100078390, 7.409399052514197653E-17 ) ) ;
#35211 = ADVANCED_FACE ( 'NONE', ( #28248 ), #58743, .F. ) ;
#35212 = CARTESIAN_POINT ( 'NONE',  ( -1.099225684535947600, 24.54030133659708923, 6.408140936763237150 ) ) ;
#35213 = COLOUR_RGB ( '', 0.08235294, 0.09019608, 0.10196078) ;
#35214 = DIRECTION ( 'NONE',  ( 0.000000000000000000, 1.000000000000000000, 0.000000000000000000 ) ) ;
#35215 = AXIS2_PLACEMENT_3D ( 'NONE', #73031, #55593, #40591 ) ;
#35216 = ORIENTED_EDGE ( 'NONE', *, *, #51977, .F. ) ;
#35217 = CARTESIAN_POINT ( 'NONE',  ( 17.20831665107776587, 57.88393115100078745, 7.208316651077764980 ) ) ;
#35218 = CARTESIAN_POINT ( 'NONE',  ( 64.56412365047462742, 26.99999999999999645, 10.00000000000000000 ) ) ;
#35219 = CARTESIAN_POINT ( 'NONE',  ( 22.26659068614894466, 23.88708216824730357, 7.082119434687054849 ) ) ;
#35220 = CARTESIAN_POINT ( 'NONE',  ( 19.84674366389459266, 28.71726448433411960, -2.638427012816827677 ) ) ;
#35221 =( BOUNDED_SURFACE ( )  B_SPLINE_SURFACE ( 1, 2, ( 
 ( #36653, #59634, #83130, #82635, #67139, #74129, #5170, #97664, #91119, #14152, #44636, #37153, #98159, #45120, #37643, #45626, #96673, #68140, #98667, #20658, #51154, #97175, #13146, #43645, #5665, #36147, #66651, #76613, #32587, #54102, #32082, #47091, #85104, #84131, #53613, #39124, #1133, #93086, #15643, #31595, #69611, #9104, #92111, #46125, #78094, #70107, #9597, #93582, #25118, #8615, #62581, #55601, #17118, #8129, #54591, #38623, #30609, #23140, #69124, #24617, #61115, #62089, #16615, #77589, #47600, #31104, #16119, #23642, #2127, #656, #46603, #84615, #92598, #86095, #77102, #24121, #39618, #40100, #91624, #1632, #55083, #85603, #70601, #7651, #63082, #17606, #76125, #38144, #68630, #160, #50055, #11075, #72064, #11561, #10101, #58036, #18580, #26560, #41596, #33559, #35033, #34048, #27049, #42554, #40598, #96059, #87071, #64544, #72543, #95051, #57056, #65536, #94567, #3103, #80559, #73037, #48572, #87558, #49072, #88544, #48076, #86586, #57547, #33076, #41095, #79071, #18095, #12053, #19067, #49546, #79575, #80058, #4573, #42080, #71592, #4076, #27542, #71095, #78589, #34539, #88046, #65033, #95560, #2621, #63572, #94081, #19558, #25601, #56093, #64055, #26086, #56581, #89039, #75020, #37034, #58531, #74523, #81040, #67531, #68024, #52031, #6525, #12548, #82524, #96561, #13536, #97062, #82026, #28036, #74025, #52516, #20550, #51035, #60011, #98047, #28535, #44020, #81528, #98552, #6043, #14040, #60509, #36543, #43050, #21540, #66535, #75515, #30002, #97554, #13034, #29503, #43530, #5556, #36032, #59029, #89535, #21045, #67032, #29015, #51534, #20045, #22040, #44521, #5056, #59525, #90506, #83022, #90018, #50546, #14539, #73529, #45009, #7029, #37535, #35540, #66032, #10344, #60998, #94320, #55346, #17364, #55846, #53003, #3333, #62841, #70857, #85853, #77843, #79326, #47833, #71346, #86833, #83517, #41355, #32339, #78336, #17844, #9857, #40356, #10836, #39857, #47340, #25841, #18337, #91509, #2372, #93341, #33795, #91001, #23028, #2864, #76008, #85352, #53500, #16866, #56339, #32827, #63326, #24863, #93834, #48817, #25360, #9352, #86341, #71824, #15036, #22532, #48329, #33315, #78833, #40844, #7536, #38027, #50, #63810, #70363, #1880, #50290, #95814, #27294, #34291, #20302, #81291, #3832, #19799, #26316, #12787, #13288, #96316, #50802, #87312, #27791, #41835, #57793, #42315, #88301, #72302, #19313, #96813, #64788, #95305, #5312, #43287, #72788, #80803, #26809, #43776, #12300, #58276, #5798, #42808, #49310, #65783, #11807, #51288, #64302, #73292, #57303, #73782, #87795, #49799, #80307, #4325, #34797, #65287 ),
 ( #4816, #35790, #35290, #88794, #66278, #94813, #28289, #89289, #58783, #81773, #79812, #11316, #14794, #29757, #21794, #23279, #60265, #15288, #30744, #28777, #84273, #75270, #22289, #60754, #90764, #52762, #53755, #82773, #90261, #68768, #61251, #36789, #83270, #6780, #76746, #36288, #74777, #45770, #21291, #29272, #67283, #6286, #300, #45267, #75762, #37294, #67781, #91756, #7283, #97811, #37784, #15772, #97305, #46261, #98303, #76263, #68281, #98802, #66786, #38275, #59275, #30250, #13785, #91254, #22780, #53259, #83765, #59768, #7780, #89774, #52274, #51784, #82270, #44272, #14293, #44765, #63212, #69263, #40235, #84752, #1763, #85243, #70247, #16257, #62228, #40726, #77237, #46739, #48213, #25251, #16749, #32219, #69751, #86720, #62720, #70743, #48704, #93220, #783, #9735, #54723, #63701, #56226, #85737, #8741, #17738, #31732, #39262, #1279, #92735, #47224, #24259, #55223, #17250, #77727, #18224, #10233, #2259, #92249, #24744, #32714, #93716, #47726, #8263, #78723, #38763, #55735, #9239, #71228, #78224, #86227, #2751, #39750, #33207, #94204, #25734, #31236, #61731, #23774, #54239, #49200, #27179, #88178, #26691, #89170, #81176, #42690, #64186, #72674, #80688, #73169, #57682, #58668, #50684, #20681, #96192, #72191, #12676, #50178, #19691, #27677, #18718, #43176, #42207, #4209, #4708, #41235, #79208, #49681, #12184, #34679, #64673, #66162, #65175, #58162, #73663, #71713, #28174, #19198, #95695, #35170, #65671, #88673, #96695, #57187, #34181, #5190, #35678, #79704, #20181, #80185, #10718, #3224, #11202, #33688, #94706, #3720, #41722, #95183, #26212, #56705, #87195, #11698, #87684, #76141, #22164, #89663, #6659, #68644, #13168, #30622, #52161, #60636, #37175, #14170, #61129, #53139, #43666, #52646, #28664, #98178, #67668, #82654, #44654, #21173, #7158, #68161, #51676, #29634, #74152, #98681, #174, #83149, #37661, #5686, #14674, #59156, #75149, #29148, #60142, #82154, #6169, #83648, #13666, #44150, #91137, #30130, #59654, #90639, #74658, #91639, #45140, #75646, #51175, #22663, #36171, #15163, #97686, #7667, #81659, #45644, #36673, #38158, #67161, #90145, #21675, #66671, #97196, #16133, #78606, #93101, #62103, #76627, #92131, #23656, #10115, #1152, #78109, #24631, #32097, #31118, #668, #85120, #47106, #40116, #61613, #77606, #16631, #55098, #8629, #54118, #25137, #17135, #55615, #40613, #71112, #54604, #9615, #2639, #63098, #84631, #1645, #46619, #8146, #69140, #77117, #70617, #38639, #9119, #62596, #85618, #93600, #39138, #92613, #69628, #48093, #31612, #24137, #39634, #70123, #33093, #47614, #2142, #32602, #86112 ) ),
 .UNSPECIFIED., .F., .F., .T. ) 
 B_SPLINE_SURFACE_WITH_KNOTS ( ( 2, 2 ),
 ( 3, 2, 2, 2, 2, 2, 2, 2, 2, 2, 2, 2, 2, 2, 2, 2, 2, 2, 2, 2, 2, 2, 2, 2, 2, 2, 2, 2, 2, 2, 2, 2, 2, 2, 2, 2, 2, 2, 2, 2, 2, 2, 2, 2, 2, 2, 2, 2, 2, 2, 2, 2, 2, 2, 2, 2, 2, 2, 2, 2, 2, 2, 2, 2, 2, 2, 2, 2, 2, 2, 2, 2, 2, 2, 2, 2, 2, 2, 2, 2, 2, 2, 2, 2, 2, 2, 2, 2, 2, 2, 2, 2, 2, 2, 2, 2, 2, 2, 2, 2, 2, 2, 2, 2, 2, 2, 2, 2, 2, 2, 2, 2, 2, 2, 2, 2, 2, 2, 2, 2, 2, 2, 2, 2, 2, 2, 2, 2, 2, 2, 2, 2, 2, 2, 2, 2, 2, 2, 2, 2, 2, 2, 2, 2, 2, 2, 2, 2, 2, 2, 2, 2, 2, 2, 2, 2, 2, 2, 2, 2, 2, 2, 3 ),
 ( 0.000000000000000000, 1.000000000000000000 ),
 ( 0.000000000000000000, 0.005952380952380952051, 0.01190476190476190410, 0.01785714285714285615, 0.02380952380952380820, 0.02976190476190476025, 0.03571428571428571230, 0.04166666666666666435, 0.04761904761904761640, 0.05357142857142856845, 0.05952380952380952051, 0.06547619047619047949, 0.07142857142857142461, 0.07738095238095238360, 0.08333333333333332871, 0.08928571428571428770, 0.09523809523809523281, 0.1011904761904761918, 0.1071428571428571369, 0.1130952380952380959, 0.1190476190476190410, 0.1250000000000000000, 0.1309523809523809590, 0.1369047619047619180, 0.1428571428571428492, 0.1488095238095238082, 0.1547619047619047672, 0.1607142857142857262, 0.1666666666666666574, 0.1726190476190476164, 0.1785714285714285754, 0.1845238095238095344, 0.1904761904761904656, 0.1964285714285714246, 0.2023809523809523836, 0.2083333333333333426, 0.2142857142857142738, 0.2202380952380952328, 0.2261904761904761918, 0.2321428571428571508, 0.2380952380952380820, 0.2440476190476190410, 0.2500000000000000000, 0.2559523809523809312, 0.2619047619047619180, 0.2678571428571428492, 0.2738095238095238360, 0.2797619047619047672, 0.2857142857142856984, 0.2916666666666666852, 0.2976190476190476164, 0.3035714285714285476, 0.3095238095238095344, 0.3154761904761904656, 0.3214285714285714524, 0.3273809523809523836, 0.3333333333333333148, 0.3392857142857143016, 0.3452380952380952328, 0.3511904761904761640, 0.3571428571428571508, 0.3630952380952380820, 0.3690476190476190688, 0.3750000000000000000, 0.3809523809523809312, 0.3869047619047619180, 0.3928571428571428492, 0.3988095238095238360, 0.4047619047619047672, 0.4107142857142856984, 0.4166666666666666852, 0.4226190476190476164, 0.4285714285714285476, 0.4345238095238095344, 0.4404761904761904656, 0.4464285714285714524, 0.4523809523809523836, 0.4583333333333333148, 0.4642857142857143016, 0.4702380952380952328, 0.4761904761904761640, 0.4821428571428571508, 0.4880952380952380820, 0.4940476190476190688, 0.5000000000000000000, 0.5059523809523809312, 0.5119047619047618625, 0.5178571428571429047, 0.5238095238095238360, 0.5297619047619047672, 0.5357142857142856984, 0.5416666666666666297, 0.5476190476190476719, 0.5535714285714286031, 0.5595238095238095344, 0.5654761904761904656, 0.5714285714285713969, 0.5773809523809523281, 0.5833333333333333703, 0.5892857142857143016, 0.5952380952380952328, 0.6011904761904761640, 0.6071428571428570953, 0.6130952380952381375, 0.6190476190476190688, 0.6250000000000000000, 0.6309523809523809312, 0.6369047619047618625, 0.6428571428571429047, 0.6488095238095238360, 0.6547619047619047672, 0.6607142857142856984, 0.6666666666666666297, 0.6726190476190476719, 0.6785714285714286031, 0.6845238095238095344, 0.6904761904761904656, 0.6964285714285713969, 0.7023809523809523281, 0.7083333333333333703, 0.7142857142857143016, 0.7202380952380952328, 0.7261904761904761640, 0.7321428571428570953, 0.7380952380952381375, 0.7440476190476190688, 0.7500000000000000000, 0.7559523809523809312, 0.7619047619047618625, 0.7678571428571429047, 0.7738095238095238360, 0.7797619047619047672, 0.7857142857142856984, 0.7916666666666666297, 0.7976190476190476719, 0.8035714285714286031, 0.8095238095238095344, 0.8154761904761904656, 0.8214285714285713969, 0.8273809523809523281, 0.8333333333333333703, 0.8392857142857143016, 0.8452380952380952328, 0.8511904761904761640, 0.8571428571428570953, 0.8630952380952381375, 0.8690476190476190688, 0.8750000000000000000, 0.8809523809523809312, 0.8869047619047618625, 0.8928571428571429047, 0.8988095238095238360, 0.9047619047619047672, 0.9107142857142856984, 0.9166666666666666297, 0.9226190476190476719, 0.9285714285714286031, 0.9345238095238095344, 0.9404761904761904656, 0.9464285714285713969, 0.9523809523809523281, 0.9583333333333333703, 0.9642857142857143016 ),
 .UNSPECIFIED. ) 
 GEOMETRIC_REPRESENTATION_ITEM ( )  RATIONAL_B_SPLINE_SURFACE ( (
 ( 1.000000000000000000, 0.9659258262890683122, 1.000000000000000000, 0.9659258262890683122, 1.000000000000000000, 0.9659258262890683122, 1.000000000000000000, 0.9659258262890683122, 1.000000000000000000, 0.9659258262890683122, 1.000000000000000000, 0.9659258262890683122, 1.000000000000000000, 0.9659258262890683122, 1.000000000000000000, 0.9659258262890683122, 1.000000000000000000, 0.9659258262890683122, 1.000000000000000000, 0.9659258262890683122, 1.000000000000000000, 0.9659258262890683122, 1.000000000000000000, 0.9659258262890683122, 1.000000000000000000, 0.9659258262890683122, 1.000000000000000000, 0.9659258262890683122, 1.000000000000000000, 0.9659258262890683122, 1.000000000000000000, 0.9659258262890683122, 1.000000000000000000, 0.9659258262890683122, 1.000000000000000000, 0.9659258262890683122, 1.000000000000000000, 0.9659258262890683122, 1.000000000000000000, 0.9659258262890683122, 1.000000000000000000, 0.9659258262890683122, 1.000000000000000000, 0.9659258262890683122, 1.000000000000000000, 0.9659258262890683122, 1.000000000000000000, 0.9659258262890683122, 1.000000000000000000, 0.9659258262890683122, 1.000000000000000000, 0.9659258262890683122, 1.000000000000000000, 0.9659258262890683122, 1.000000000000000000, 0.9659258262890683122, 1.000000000000000000, 0.9659258262890683122, 1.000000000000000000, 0.9659258262890683122, 1.000000000000000000, 0.9659258262890683122, 1.000000000000000000, 0.9659258262890683122, 1.000000000000000000, 0.9659258262890683122, 1.000000000000000000, 0.9659258262890683122, 1.000000000000000000, 0.9659258262890683122, 1.000000000000000000, 0.9659258262890683122, 1.000000000000000000, 0.9659258262890683122, 1.000000000000000000, 0.9659258262890683122, 1.000000000000000000, 0.9659258262890683122, 1.000000000000000000, 0.9659258262890683122, 1.000000000000000000, 0.9659258262890683122, 1.000000000000000000, 0.9659258262890683122, 1.000000000000000000, 0.9659258262890683122, 1.000000000000000000, 0.9659258262890683122, 1.000000000000000000, 0.9659258262890683122, 1.000000000000000000, 0.9659258262890683122, 1.000000000000000000, 0.9659258262890683122, 1.000000000000000000, 0.9659258262890683122, 1.000000000000000000, 0.9659258262890683122, 1.000000000000000000, 0.9659258262890683122, 1.000000000000000000, 0.9659258262890683122, 1.000000000000000000, 0.9659258262890683122, 1.000000000000000000, 0.9659258262890683122, 1.000000000000000000, 0.9659258262890683122, 1.000000000000000000, 0.9659258262890683122, 1.000000000000000000, 0.9659258262890683122, 1.000000000000000000, 0.9659258262890683122, 1.000000000000000000, 0.9659258262890683122, 1.000000000000000000, 0.9659258262890683122, 1.000000000000000000, 0.9659258262890683122, 1.000000000000000000, 0.9659258262890683122, 1.000000000000000000, 0.9659258262890683122, 1.000000000000000000, 0.9659258262890683122, 1.000000000000000000, 0.9659258262890683122, 1.000000000000000000, 0.9659258262890683122, 1.000000000000000000, 0.9659258262890683122, 1.000000000000000000, 0.9659258262890683122, 1.000000000000000000, 0.9659258262890683122, 1.000000000000000000, 0.9659258262890683122, 1.000000000000000000, 0.9659258262890683122, 1.000000000000000000, 0.9659258262890683122, 1.000000000000000000, 0.9659258262890683122, 1.000000000000000000, 0.9659258262890683122, 1.000000000000000000, 0.9659258262890683122, 1.000000000000000000, 0.9659258262890683122, 1.000000000000000000, 0.9659258262890683122, 1.000000000000000000, 0.9659258262890683122, 1.000000000000000000, 0.9659258262890683122, 1.000000000000000000, 0.9659258262890683122, 1.000000000000000000, 0.9659258262890683122, 1.000000000000000000, 0.9659258262890683122, 1.000000000000000000, 0.9659258262890683122, 1.000000000000000000, 0.9659258262890683122, 1.000000000000000000, 0.9659258262890683122, 1.000000000000000000, 0.9659258262890683122, 1.000000000000000000, 0.9659258262890683122, 1.000000000000000000, 0.9659258262890683122, 1.000000000000000000, 0.9659258262890683122, 1.000000000000000000, 0.9659258262890683122, 1.000000000000000000, 0.9659258262890683122, 1.000000000000000000, 0.9659258262890683122, 1.000000000000000000, 0.9659258262890683122, 1.000000000000000000, 0.9659258262890683122, 1.000000000000000000, 0.9659258262890683122, 1.000000000000000000, 0.9659258262890683122, 1.000000000000000000, 0.9659258262890683122, 1.000000000000000000, 0.9659258262890683122, 1.000000000000000000, 0.9659258262890683122, 1.000000000000000000, 0.9659258262890683122, 1.000000000000000000, 0.9659258262890683122, 1.000000000000000000, 0.9659258262890683122, 1.000000000000000000, 0.9659258262890683122, 1.000000000000000000, 0.9659258262890683122, 1.000000000000000000, 0.9659258262890683122, 1.000000000000000000, 0.9659258262890683122, 1.000000000000000000, 0.9659258262890683122, 1.000000000000000000, 0.9659258262890683122, 1.000000000000000000, 0.9659258262890683122, 1.000000000000000000, 0.9659258262890683122, 1.000000000000000000, 0.9659258262890683122, 1.000000000000000000, 0.9659258262890683122, 1.000000000000000000, 0.9659258262890683122, 1.000000000000000000, 0.9659258262890683122, 1.000000000000000000, 0.9659258262890683122, 1.000000000000000000, 0.9659258262890683122, 1.000000000000000000, 0.9659258262890683122, 1.000000000000000000, 0.9659258262890683122, 1.000000000000000000, 0.9659258262890683122, 1.000000000000000000, 0.9659258262890683122, 1.000000000000000000, 0.9659258262890683122, 1.000000000000000000, 0.9659258262890683122, 1.000000000000000000, 0.9659258262890683122, 1.000000000000000000, 0.9659258262890683122, 1.000000000000000000, 0.9659258262890683122, 1.000000000000000000, 0.9659258262890683122, 1.000000000000000000, 0.9659258262890683122, 1.000000000000000000, 0.9659258262890683122, 1.000000000000000000, 0.9659258262890683122, 1.000000000000000000, 0.9659258262890683122, 1.000000000000000000, 0.9659258262890683122, 1.000000000000000000, 0.9659258262890683122, 1.000000000000000000, 0.9659258262890683122, 1.000000000000000000, 0.9659258262890683122, 1.000000000000000000, 0.9659258262890683122, 1.000000000000000000, 0.9659258262890683122, 1.000000000000000000, 0.9659258262890683122, 1.000000000000000000, 0.9659258262890683122, 1.000000000000000000, 0.9659258262890683122, 1.000000000000000000, 0.9659258262890683122, 1.000000000000000000, 0.9659258262890683122, 1.000000000000000000, 0.9659258262890683122, 1.000000000000000000, 0.9659258262890683122, 1.000000000000000000, 0.9659258262890683122, 1.000000000000000000, 0.9659258262890683122, 1.000000000000000000, 0.9659258262890683122, 1.000000000000000000, 0.9659258262890683122, 1.000000000000000000, 0.9659258262890683122, 1.000000000000000000, 0.9659258262890683122, 1.000000000000000000, 0.9659258262890683122, 1.000000000000000000, 0.9659258262890683122, 1.000000000000000000, 0.9659258262890683122, 1.000000000000000000, 0.9659258262890683122, 1.000000000000000000, 0.9659258262890683122, 1.000000000000000000, 0.9659258262890683122, 1.000000000000000000, 0.9659258262890683122, 1.000000000000000000, 0.9659258262890683122, 1.000000000000000000, 0.9659258262890683122, 1.000000000000000000, 0.9659258262890683122, 1.000000000000000000, 0.9659258262890683122, 1.000000000000000000, 0.9659258262890683122, 1.000000000000000000, 0.9659258262890683122, 1.000000000000000000, 0.9659258262890683122, 1.000000000000000000),
 ( 1.000000000000000000, 0.9659258262890683122, 1.000000000000000000, 0.9659258262890683122, 1.000000000000000000, 0.9659258262890683122, 1.000000000000000000, 0.9659258262890683122, 1.000000000000000000, 0.9659258262890683122, 1.000000000000000000, 0.9659258262890683122, 1.000000000000000000, 0.9659258262890683122, 1.000000000000000000, 0.9659258262890683122, 1.000000000000000000, 0.9659258262890683122, 1.000000000000000000, 0.9659258262890683122, 1.000000000000000000, 0.9659258262890683122, 1.000000000000000000, 0.9659258262890683122, 1.000000000000000000, 0.9659258262890683122, 1.000000000000000000, 0.9659258262890683122, 1.000000000000000000, 0.9659258262890683122, 1.000000000000000000, 0.9659258262890683122, 1.000000000000000000, 0.9659258262890683122, 1.000000000000000000, 0.9659258262890683122, 1.000000000000000000, 0.9659258262890683122, 1.000000000000000000, 0.9659258262890683122, 1.000000000000000000, 0.9659258262890683122, 1.000000000000000000, 0.9659258262890683122, 1.000000000000000000, 0.9659258262890683122, 1.000000000000000000, 0.9659258262890683122, 1.000000000000000000, 0.9659258262890683122, 1.000000000000000000, 0.9659258262890683122, 1.000000000000000000, 0.9659258262890683122, 1.000000000000000000, 0.9659258262890683122, 1.000000000000000000, 0.9659258262890683122, 1.000000000000000000, 0.9659258262890683122, 1.000000000000000000, 0.9659258262890683122, 1.000000000000000000, 0.9659258262890683122, 1.000000000000000000, 0.9659258262890683122, 1.000000000000000000, 0.9659258262890683122, 1.000000000000000000, 0.9659258262890683122, 1.000000000000000000, 0.9659258262890683122, 1.000000000000000000, 0.9659258262890683122, 1.000000000000000000, 0.9659258262890683122, 1.000000000000000000, 0.9659258262890683122, 1.000000000000000000, 0.9659258262890683122, 1.000000000000000000, 0.9659258262890683122, 1.000000000000000000, 0.9659258262890683122, 1.000000000000000000, 0.9659258262890683122, 1.000000000000000000, 0.9659258262890683122, 1.000000000000000000, 0.9659258262890683122, 1.000000000000000000, 0.9659258262890683122, 1.000000000000000000, 0.9659258262890683122, 1.000000000000000000, 0.9659258262890683122, 1.000000000000000000, 0.9659258262890683122, 1.000000000000000000, 0.9659258262890683122, 1.000000000000000000, 0.9659258262890683122, 1.000000000000000000, 0.9659258262890683122, 1.000000000000000000, 0.9659258262890683122, 1.000000000000000000, 0.9659258262890683122, 1.000000000000000000, 0.9659258262890683122, 1.000000000000000000, 0.9659258262890683122, 1.000000000000000000, 0.9659258262890683122, 1.000000000000000000, 0.9659258262890683122, 1.000000000000000000, 0.9659258262890683122, 1.000000000000000000, 0.9659258262890683122, 1.000000000000000000, 0.9659258262890683122, 1.000000000000000000, 0.9659258262890683122, 1.000000000000000000, 0.9659258262890683122, 1.000000000000000000, 0.9659258262890683122, 1.000000000000000000, 0.9659258262890683122, 1.000000000000000000, 0.9659258262890683122, 1.000000000000000000, 0.9659258262890683122, 1.000000000000000000, 0.9659258262890683122, 1.000000000000000000, 0.9659258262890683122, 1.000000000000000000, 0.9659258262890683122, 1.000000000000000000, 0.9659258262890683122, 1.000000000000000000, 0.9659258262890683122, 1.000000000000000000, 0.9659258262890683122, 1.000000000000000000, 0.9659258262890683122, 1.000000000000000000, 0.9659258262890683122, 1.000000000000000000, 0.9659258262890683122, 1.000000000000000000, 0.9659258262890683122, 1.000000000000000000, 0.9659258262890683122, 1.000000000000000000, 0.9659258262890683122, 1.000000000000000000, 0.9659258262890683122, 1.000000000000000000, 0.9659258262890683122, 1.000000000000000000, 0.9659258262890683122, 1.000000000000000000, 0.9659258262890683122, 1.000000000000000000, 0.9659258262890683122, 1.000000000000000000, 0.9659258262890683122, 1.000000000000000000, 0.9659258262890683122, 1.000000000000000000, 0.9659258262890683122, 1.000000000000000000, 0.9659258262890683122, 1.000000000000000000, 0.9659258262890683122, 1.000000000000000000, 0.9659258262890683122, 1.000000000000000000, 0.9659258262890683122, 1.000000000000000000, 0.9659258262890683122, 1.000000000000000000, 0.9659258262890683122, 1.000000000000000000, 0.9659258262890683122, 1.000000000000000000, 0.9659258262890683122, 1.000000000000000000, 0.9659258262890683122, 1.000000000000000000, 0.9659258262890683122, 1.000000000000000000, 0.9659258262890683122, 1.000000000000000000, 0.9659258262890683122, 1.000000000000000000, 0.9659258262890683122, 1.000000000000000000, 0.9659258262890683122, 1.000000000000000000, 0.9659258262890683122, 1.000000000000000000, 0.9659258262890683122, 1.000000000000000000, 0.9659258262890683122, 1.000000000000000000, 0.9659258262890683122, 1.000000000000000000, 0.9659258262890683122, 1.000000000000000000, 0.9659258262890683122, 1.000000000000000000, 0.9659258262890683122, 1.000000000000000000, 0.9659258262890683122, 1.000000000000000000, 0.9659258262890683122, 1.000000000000000000, 0.9659258262890683122, 1.000000000000000000, 0.9659258262890683122, 1.000000000000000000, 0.9659258262890683122, 1.000000000000000000, 0.9659258262890683122, 1.000000000000000000, 0.9659258262890683122, 1.000000000000000000, 0.9659258262890683122, 1.000000000000000000, 0.9659258262890683122, 1.000000000000000000, 0.9659258262890683122, 1.000000000000000000, 0.9659258262890683122, 1.000000000000000000, 0.9659258262890683122, 1.000000000000000000, 0.9659258262890683122, 1.000000000000000000, 0.9659258262890683122, 1.000000000000000000, 0.9659258262890683122, 1.000000000000000000, 0.9659258262890683122, 1.000000000000000000, 0.9659258262890683122, 1.000000000000000000, 0.9659258262890683122, 1.000000000000000000, 0.9659258262890683122, 1.000000000000000000, 0.9659258262890683122, 1.000000000000000000, 0.9659258262890683122, 1.000000000000000000, 0.9659258262890683122, 1.000000000000000000, 0.9659258262890683122, 1.000000000000000000, 0.9659258262890683122, 1.000000000000000000, 0.9659258262890683122, 1.000000000000000000, 0.9659258262890683122, 1.000000000000000000, 0.9659258262890683122, 1.000000000000000000, 0.9659258262890683122, 1.000000000000000000, 0.9659258262890683122, 1.000000000000000000, 0.9659258262890683122, 1.000000000000000000, 0.9659258262890683122, 1.000000000000000000, 0.9659258262890683122, 1.000000000000000000, 0.9659258262890683122, 1.000000000000000000, 0.9659258262890683122, 1.000000000000000000, 0.9659258262890683122, 1.000000000000000000, 0.9659258262890683122, 1.000000000000000000, 0.9659258262890683122, 1.000000000000000000, 0.9659258262890683122, 1.000000000000000000, 0.9659258262890683122, 1.000000000000000000, 0.9659258262890683122, 1.000000000000000000, 0.9659258262890683122, 1.000000000000000000, 0.9659258262890683122, 1.000000000000000000, 0.9659258262890683122, 1.000000000000000000, 0.9659258262890683122, 1.000000000000000000, 0.9659258262890683122, 1.000000000000000000, 0.9659258262890683122, 1.000000000000000000, 0.9659258262890683122, 1.000000000000000000, 0.9659258262890683122, 1.000000000000000000, 0.9659258262890683122, 1.000000000000000000, 0.9659258262890683122, 1.000000000000000000, 0.9659258262890683122, 1.000000000000000000, 0.9659258262890683122, 1.000000000000000000, 0.9659258262890683122, 1.000000000000000000, 0.9659258262890683122, 1.000000000000000000) ) ) 
 REPRESENTATION_ITEM ( '' )  SURFACE ( )  );
#35222 = CARTESIAN_POINT ( 'NONE',  ( -2.816281873526471635, 48.91530133659708213, -3.434112377981056508 ) ) ;
#35224 = CARTESIAN_POINT ( 'NONE',  ( 19.80777595082615861, 15.68878173731740766, -6.500000000000005329 ) ) ;
#35223 = DIRECTION ( 'NONE',  ( -1.000000000000000000, 0.000000000000000000, 0.000000000000000000 ) ) ;
#35225 = CARTESIAN_POINT ( 'NONE',  ( 10.00000000000000178, 59.31368534415484106, 10.88017736071110342 ) ) ;
#35226 = CIRCLE ( 'NONE', #30448, 0.2500000000000002220 ) ;
#35227 = CARTESIAN_POINT ( 'NONE',  ( -2.816281873526471635, 13.91530133659708746, -3.434112377981056508 ) ) ;
#35228 = CARTESIAN_POINT ( 'NONE',  ( 0.000000000000000000, 0.5000000000000004441, 0.000000000000000000 ) ) ;
#35229 = CARTESIAN_POINT ( 'NONE',  ( 19.84674366389459266, 33.71726448433410894, -2.638427012816827677 ) ) ;
#35230 = CARTESIAN_POINT ( 'NONE',  ( 4.559911319644449179, 33.89701867748817676, 9.422509992056141925 ) ) ;
#35231 = CARTESIAN_POINT ( 'NONE',  ( 6.565887622018943937, 38.08196800326376064, -12.81628187352647608 ) ) ;
#35232 = CARTESIAN_POINT ( 'NONE',  ( 10.00000000000000178, 37.25893115100078745, 9.846743663894594434 ) ) ;
#35233 = CARTESIAN_POINT ( 'NONE',  ( -241.3571713825667473, -142.8543165515659723, -20.14837537411879254 ) ) ;
#35234 = CARTESIAN_POINT ( 'NONE',  ( -2.120353041430744323, 4.696395766537044518E-16, 14.34413130794943925 ) ) ;
#35235 = EDGE_CURVE ( 'NONE', #80582, #67582, #12258, .T. ) ;
#35236 = CARTESIAN_POINT ( 'NONE',  ( 15.44008868035555793, 31.39701867748817676, -9.422509992056140149 ) ) ;
#35237 = ORIENTED_EDGE ( 'NONE', *, *, #39252, .T. ) ;
#35238 = PLANE ( 'NONE',  #20167 ) ;
#35239 = CARTESIAN_POINT ( 'NONE',  ( -13.14228782657336581, 14.49999999999999112, -7.230509711182429022 ) ) ;
#35241 = CARTESIAN_POINT ( 'NONE',  ( 15.44008868035555793, 31.39701867748817676, -9.422509992056140149 ) ) ;
#35240 = CARTESIAN_POINT ( 'NONE',  ( 7.361572987183170547, 52.05059781766745175, 9.846743663894590881 ) ) ;
#35242 = LINE ( 'NONE', #96269, #40840 ) ;
#35243 = EDGE_CURVE ( 'NONE', #6299, #5362, #95772, .T. ) ;
#35244 = CARTESIAN_POINT ( 'NONE',  ( 15.44008868035555260, 54.73035201082150536, 9.422509992056143702 ) ) ;
#35246 = CARTESIAN_POINT ( 'NONE',  ( -4.023424921641842289, -0.03417435944610275333, 15.48190712851503648 ) ) ;
#35245 = CARTESIAN_POINT ( 'NONE',  ( 15.44008868035555260, 29.73035201082150891, 9.422509992056143702 ) ) ;
#35247 = FILL_AREA_STYLE ('',( #42764 ) ) ;
#35248 = CARTESIAN_POINT ( 'NONE',  ( 17.20831665107776587, 24.13393115100078035, -7.208316651077762316 ) ) ;
#35249 = DIRECTION ( 'NONE',  ( 0.000000000000000000, 0.000000000000000000, -1.000000000000000000 ) ) ;
#35250 = CARTESIAN_POINT ( 'NONE',  ( 0.1532563361054100626, 45.80059781766745886, -2.638427012816831230 ) ) ;
#35251 = CARTESIAN_POINT ( 'NONE',  ( -4.164238869374098151, 56.59541550158063927, -3.795296366450310543 ) ) ;
#35252 = CIRCLE ( 'NONE', #14523, 3.999999999999999112 ) ;
#35253 = CARTESIAN_POINT ( 'NONE',  ( 11.24699797944280100, 54.09857164847241506, -2.899999999999999467 ) ) ;
#35254 = CARTESIAN_POINT ( 'NONE',  ( 2.917880565312950480, 15.97041550158063217, -12.26659068614894821 ) ) ;
#35255 = CARTESIAN_POINT ( 'NONE',  ( -2.266590686148945544, 42.22041550158063217, 7.082119434687048631 ) ) ;
#35256 = CARTESIAN_POINT ( 'NONE',  ( 19.38216949554541557, 2.248634669930420049, -9.382169495545420901 ) ) ;
#35258 = CARTESIAN_POINT ( 'NONE',  ( 11.36220558718857276, 15.00000000000000000, 9.008345252845320061 ) ) ;
#35257 = AXIS2_PLACEMENT_3D ( 'NONE', #22598, #67100, #53075 ) ;
#35259 = ORIENTED_EDGE ( 'NONE', *, *, #30368, .T. ) ;
#35260 = CARTESIAN_POINT ( 'NONE',  ( 12.91533473730992121, 19.52201867748816611, 10.88017736071110164 ) ) ;
#35261 = CARTESIAN_POINT ( 'NONE',  ( 19.84674366389459266, 38.30059781766745175, 2.638427012816836559 ) ) ;
#35263 = CARTESIAN_POINT ( 'NONE',  ( -10.34223742324318884, 89.23976162705962167, -5.715022854599768110 ) ) ;
#35262 = DIRECTION ( 'NONE',  ( 0.000000000000000000, -0.000000000000000000, -1.000000000000000000 ) ) ;
#35264 = CARTESIAN_POINT ( 'NONE',  ( 19.42250999205614193, 55.14701867748817676, 5.440088680355555262 ) ) ;
#35265 = DIRECTION ( 'NONE',  ( 0.000000000000000000, 0.000000000000000000, 1.000000000000000000 ) ) ;
#35266 = UNCERTAINTY_MEASURE_WITH_UNIT (LENGTH_MEASURE( 1.000000000000000082E-05 ), #55945, 'distance_accuracy_value', 'NONE');
#35267 = CARTESIAN_POINT ( 'NONE',  ( -2.816281873526473856, 59.12363466993042493, 9.499525473075851096E-16 ) ) ;
#35268 = CARTESIAN_POINT ( 'NONE',  ( -2.816281873526473856, 29.33196800326376064, 3.434112377981055619 ) ) ;
#35269 = CARTESIAN_POINT ( 'NONE',  ( 12.63842701281683922, 34.55059781766745886, -9.846743663894590881 ) ) ;
#35270 = ORIENTED_EDGE ( 'NONE', *, *, #75307, .F. ) ;
#35271 = FILL_AREA_STYLE ('',( #26788 ) ) ;
#35272 = CARTESIAN_POINT ( 'NONE',  ( -3.468686501387172161, 0.000000000000000000, 4.207853202970306405 ) ) ;
#35273 = CARTESIAN_POINT ( 'NONE',  ( 20.88017736071110519, 5.563685344154838397, 2.639326808657452039E-16 ) ) ;
#35274 = CARTESIAN_POINT ( 'NONE',  ( 19.42250999205614193, 20.14701867748817321, 5.440088680355555262 ) ) ;
#35275 = CARTESIAN_POINT ( 'NONE',  ( 24.16423886937410614, 44.51208216824730357, -3.795296366450302550 ) ) ;
#35276 = CARTESIAN_POINT ( 'NONE',  ( 20.88017736071110519, 35.56368534415484106, 2.639326808657452039E-16 ) ) ;
#35277 = CARTESIAN_POINT ( 'NONE',  ( 12.91533473730993009, 61.60535201082150536, -10.88017736071109987 ) ) ;
#35278 = CARTESIAN_POINT ( 'NONE',  ( 14.67697702673042848, -0.03417435944610275333, -6.361111679013412790 ) ) ;
#35279 = LINE ( 'NONE', #36275, #17766 ) ;
#35280 = CARTESIAN_POINT ( 'NONE',  ( 12.63842701281683034, 22.46726448433411605, 9.846743663894596210 ) ) ;
#35281 = CARTESIAN_POINT ( 'NONE',  ( 19.84674366389459266, 13.30059781766745353, 2.638427012816836559 ) ) ;
#35282 = CARTESIAN_POINT ( 'NONE',  ( 10.00000000000000178, 32.25893115100078745, 9.846743663894594434 ) ) ;
#35283 = CARTESIAN_POINT ( 'NONE',  ( 17.20831665107776587, 64.13393115100079456, -7.208316651077762316 ) ) ;
#35284 = CARTESIAN_POINT ( 'NONE',  ( 4.559911319644449179, 22.23035201082150536, -9.422509992056141925 ) ) ;
#35285 = UNCERTAINTY_MEASURE_WITH_UNIT (LENGTH_MEASURE( 1.000000000000000082E-05 ), #67058, 'distance_accuracy_value', 'NONE');
#35286 = CIRCLE ( 'NONE', #38525, 19.99999999999999645 ) ;
#35287 = ORIENTED_EDGE ( 'NONE', *, *, #17045, .T. ) ;
#35288 = CARTESIAN_POINT ( 'NONE',  ( 6.565887622018943937, 40.16530133659708923, 12.81628187352647430 ) ) ;
#35289 = FILL_AREA_STYLE_COLOUR ( '', #17329 ) ;
#35290 = CARTESIAN_POINT ( 'NONE',  ( 5.076628168052704559, 0.1755978176674514724, -8.527530157486179263 ) ) ;
#35291 = CARTESIAN_POINT ( 'NONE',  ( 3.591859063236763294, 43.29030133659708923, -11.09922568453595026 ) ) ;
#35293 = CARTESIAN_POINT ( 'NONE',  ( 2.791683348922240793, 31.63393115100078745, 7.208316651077764092 ) ) ;
#35292 = CARTESIAN_POINT ( 'NONE',  ( -4.164238869374099039, 56.80374883491397497, 8.674139862899312516E-16 ) ) ;
#35294 = DIRECTION ( 'NONE',  ( -4.336808689942013792E-16, 1.000000000000000000, 0.000000000000000000 ) ) ;
#35295 = CARTESIAN_POINT ( 'NONE',  ( 1.472469842513823179, 60.59226448433412315, -4.923371831947296329 ) ) ;
#35296 = CARTESIAN_POINT ( 'NONE',  ( 17.08211943468705130, 18.47041550158063572, 12.26659068614894998 ) ) ;
#35297 = CARTESIAN_POINT ( 'NONE',  ( 24.16423886937410614, 34.51208216824731068, -3.795296366450302550 ) ) ;
#35298 = CARTESIAN_POINT ( 'NONE',  ( 5.076628168052704559, 50.17559781766745886, -8.527530157486179263 ) ) ;
#35299 = MECHANICAL_DESIGN_GEOMETRIC_PRESENTATION_REPRESENTATION (  '', ( #225 ), #79983 ) ;
#35300 = DIRECTION ( 'NONE',  ( 1.000000000000000000, 0.000000000000000000, 0.000000000000000000 ) ) ;
#35301 = CARTESIAN_POINT ( 'NONE',  ( 4.559911319644449179, 42.23035201082151247, -9.422509992056141925 ) ) ;
#35302 = CARTESIAN_POINT ( 'NONE',  ( 0.5774900079438590739, 57.64701867748817676, -5.440088680355550821 ) ) ;
#35303 = DIRECTION ( 'NONE',  ( -0.000000000000000000, 0.000000000000000000, 1.000000000000000000 ) ) ;
#35304 = ORIENTED_EDGE ( 'NONE', *, *, #66128, .T. ) ;
#35305 = CARTESIAN_POINT ( 'NONE',  ( 13.43411237798105340, 45.58196800326374643, 12.81628187352647963 ) ) ;
#35306 = CARTESIAN_POINT ( 'NONE',  ( 14.92337183194729633, 2.675597817667451750, 8.527530157486181039 ) ) ;
#35307 = ORIENTED_EDGE ( 'NONE', *, *, #90944, .F. ) ;
#35308 = EDGE_CURVE ( 'NONE', #30282, #58661, #10661, .T. ) ;
#35309 = CARTESIAN_POINT ( 'NONE',  ( 2.917880565312948704, 2.637082168247300906, 12.26659068614894643 ) ) ;
#35310 = DIRECTION ( 'NONE',  ( 0.000000000000000000, 1.000000000000000000, 0.000000000000000000 ) ) ;
#35311 = CARTESIAN_POINT ( 'NONE',  ( -11.35178980618986877, 14.49999999999999112, 9.804941009311868072 ) ) ;
#35312 = ORIENTED_EDGE ( 'NONE', *, *, #53164, .T. ) ;
#35313 = FILL_AREA_STYLE_COLOUR ( '', #66838 ) ;
#35314 = CARTESIAN_POINT ( 'NONE',  ( 7.084665262690076126, 17.02201867748817676, -10.88017736071110164 ) ) ;
#35315 = CARTESIAN_POINT ( 'NONE',  ( -5.419894505350723257, 14.49999999999999112, 13.98659156302460183 ) ) ;
#35316 = ORIENTED_EDGE ( 'NONE', *, *, #69274, .T. ) ;
#35317 = CARTESIAN_POINT ( 'NONE',  ( 22.26659068614895176, 14.72041550158063572, -7.082119434687042414 ) ) ;
#35318 = CARTESIAN_POINT ( 'NONE',  ( 15.44008868035555260, 19.73035201082150536, 9.422509992056143702 ) ) ;
#35319 = CARTESIAN_POINT ( 'NONE',  ( 0.1532563361054100626, 55.80059781766745175, -2.638427012816831230 ) ) ;
#35320 = VERTEX_POINT ( 'NONE', #75725 ) ;
#35321 = CARTESIAN_POINT ( 'NONE',  ( 5.076628168052704559, 65.17559781766745175, -8.527530157486179263 ) ) ;
#35322 = VERTEX_POINT ( 'NONE', #52238 ) ;
#35323 = CARTESIAN_POINT ( 'NONE',  ( 4.559911319644449179, 48.89701867748817676, 9.422509992056141925 ) ) ;
#35324 = CARTESIAN_POINT ( 'NONE',  ( 2.189108318723745672, 15.00000000000000178, -14.46085460646898646 ) ) ;
#35325 = EDGE_CURVE ( 'NONE', #20839, #40449, #81695, .T. ) ;
#35326 = CARTESIAN_POINT ( 'NONE',  ( 6.565887622018943937, 35.16530133659708923, 12.81628187352647430 ) ) ;
#35328 = CARTESIAN_POINT ( 'NONE',  ( -9.997910040112461871, 4.266261872180168263E-16, -10.50199004140731773 ) ) ;
#35327 = CARTESIAN_POINT ( 'NONE',  ( 17.96484262340118221, 9.938685344154837509, 7.964842623401181321 ) ) ;
#35329 = CARTESIAN_POINT ( 'NONE',  ( 12.63842701281683034, 7.467264484334118713, 9.846743663894596210 ) ) ;
#35330 = CARTESIAN_POINT ( 'NONE',  ( 19.42250999205614548, 15.98035201082150714, -5.440088680355545492 ) ) ;
#35331 = AXIS2_PLACEMENT_3D ( 'NONE', #18795, #63773, #32299 ) ;
#35332 = EDGE_CURVE ( 'NONE', #9539, #59946, #63808, .T. ) ;
#35333 = CIRCLE ( 'NONE', #19495, 0.2500000000000002220 ) ;
#35334 = ORIENTED_EDGE ( 'NONE', *, *, #66707, .F. ) ;
#35335 = CARTESIAN_POINT ( 'NONE',  ( -2.816281873526473856, 49.12363466993042493, 9.499525473075851096E-16 ) ) ;
#35336 = CARTESIAN_POINT ( 'NONE',  ( 20.88017736071110875, 30.77201867748816966, -2.915334737309920765 ) ) ;
#35337 = CARTESIAN_POINT ( 'NONE',  ( 19.64275500434244748, 93.00187409791189452, 5.306653671078411350 ) ) ;
#35338 = CARTESIAN_POINT ( 'NONE',  ( 16.40814093676323893, 40.79030133659708923, 11.09922568453595026 ) ) ;
#35339 = CARTESIAN_POINT ( 'NONE',  ( 20.88017736071110519, 45.56368534415484106, 2.639326808657452039E-16 ) ) ;
#35340 = ADVANCED_FACE ( 'NONE', ( #23239 ), #46221, .F. ) ;
#35341 =( BOUNDED_CURVE ( )  B_SPLINE_CURVE ( 2, ( #58721, #20735, #13224, #43720, #74205, #31177, #75706, #59706, #30682 ),
 .UNSPECIFIED., .F., .F. ) 
 B_SPLINE_CURVE_WITH_KNOTS ( ( 3, 2, 2, 2, 3 ),
 ( 0.4044266512259456214, 0.4047619047619047672, 0.4107142857142856984, 0.4166666666666666297, 0.4170019202026257754 ),
 .UNSPECIFIED. ) 
 CURVE ( )  GEOMETRIC_REPRESENTATION_ITEM ( )  RATIONAL_B_SPLINE_CURVE ( ( 0.9963778908391760503, 0.9980808541467920403, 1.000000000000000000, 0.9659258262890683122, 1.000000000000000000, 0.9659258262890683122, 1.000000000000000000, 0.9980808541467920403, 0.9963778908391760503 ) ) 
 REPRESENTATION_ITEM ( '' )  );
#35342 = CARTESIAN_POINT ( 'NONE',  ( 0.1532563361054100626, 50.80059781766745175, -2.638427012816831230 ) ) ;
#35343 = EDGE_LOOP ( 'NONE', ( #9704, #47737, #5414, #61744, #51063, #32483 ) ) ;
#35344 = CARTESIAN_POINT ( 'NONE',  ( 12.63842701281683922, 9.550597817667449974, -9.846743663894590881 ) ) ;
#35345 = CARTESIAN_POINT ( 'NONE',  ( 3.591859063236763294, -1.709698663402913210, -11.09922568453595026 ) ) ;
#35347 = CARTESIAN_POINT ( 'NONE',  ( 7.361572987183169658, 44.96726448433412315, -9.846743663894592657 ) ) ;
#35346 = CARTESIAN_POINT ( 'NONE',  ( -3.836325488035988052, 0.5000000000000004441, -14.50112432709427424 ) ) ;
#35348 = CARTESIAN_POINT ( 'NONE',  ( 4.559911319644449179, 17.23035201082150536, -9.422509992056141925 ) ) ;
#35349 = CIRCLE ( 'NONE', #96039, 1.249999999999987121 ) ;
#35350 = CARTESIAN_POINT ( 'NONE',  ( 17.20831665107776587, 37.88393115100078745, 7.208316651077764980 ) ) ;
#35351 = CARTESIAN_POINT ( 'NONE',  ( -0.1503990784575277295, 39.24884699246889141, -6.262539305110077947 ) ) ;
#35352 = FACE_OUTER_BOUND ( 'NONE', #58046, .T. ) ;
#35354 = CARTESIAN_POINT ( 'NONE',  ( 14.92337183194729988, 9.342264484334119601, -8.527530157486177487 ) ) ;
#35353 = CARTESIAN_POINT ( 'NONE',  ( 1.472469842513823179, 40.59226448433411605, -4.923371831947296329 ) ) ;
#35355 = CARTESIAN_POINT ( 'NONE',  ( 19.84674366389459266, 28.30059781766745530, 2.638427012816836559 ) ) ;
#35357 = VERTEX_POINT ( 'NONE', #76228 ) ;
#35356 = CARTESIAN_POINT ( 'NONE',  ( 18.52753015748617571, 53.09226448433412315, 4.923371831947298993 ) ) ;
#35358 = PRESENTATION_LAYER_ASSIGNMENT (  '', '', ( #40153 ) ) ;
#35359 = DIRECTION ( 'NONE',  ( 1.927470528863119295E-16, -1.000000000000000000, 0.000000000000000000 ) ) ;
#35360 = CARTESIAN_POINT ( 'NONE',  ( 13.43411237798106583, 37.66530133659708923, -12.81628187352647252 ) ) ;
#35361 = CARTESIAN_POINT ( 'NONE',  ( 18.52753015748618282, 28.92559781766745175, -4.923371831947291888 ) ) ;
#35362 = CARTESIAN_POINT ( 'NONE',  ( 0.000000000000000000, 15.00000000000000000, 0.000000000000000000 ) ) ;
#35363 = CARTESIAN_POINT ( 'NONE',  ( 20.36894250292379738, 59.92874883491397497, -10.36894250292379027 ) ) ;
#35364 = CARTESIAN_POINT ( 'NONE',  ( 7.361572987183170547, 37.05059781766744464, 9.846743663894590881 ) ) ;
#35365 = ORIENTED_EDGE ( 'NONE', *, *, #29805, .T. ) ;
#35366 = STYLED_ITEM ( 'NONE', ( #29497 ), #46646 ) ;
#35367 = CARTESIAN_POINT ( 'NONE',  ( 19.99999999998935607, 80.90839911560571807, 4.954669604078111966 ) ) ;
#35368 = CARTESIAN_POINT ( 'NONE',  ( -4.164238869374099039, 51.80374883491396787, 8.674139862899312516E-16 ) ) ;
#35369 = CARTESIAN_POINT ( 'NONE',  ( 9.972640495195376431, 15.00000000000000000, -12.50695158660345818 ) ) ;
#35370 = ADVANCED_FACE ( 'NONE', ( #15738 ), #37256, .F. ) ;
#35371 = CARTESIAN_POINT ( 'NONE',  ( 17.96484262340118221, 16.18868534415483396, -7.964842623401177768 ) ) ;
#35372 = CARTESIAN_POINT ( 'NONE',  ( -2.266590686148945544, 42.22041550158063217, 7.082119434687048631 ) ) ;
#35373 = CARTESIAN_POINT ( 'NONE',  ( 20.36894250292379382, 48.67874883491396076, 10.36894250292379205 ) ) ;
#35374 = CARTESIAN_POINT ( 'NONE',  ( 7.595945211629608451, 15.00000000000000000, 12.35117874302463292 ) ) ;
#35375 = AXIS2_PLACEMENT_3D ( 'NONE', #17614, #48580, #19566 ) ;
#35376 = CARTESIAN_POINT ( 'NONE',  ( 1.472469842513823179, 11.42559781766745175, 4.923371831947296329 ) ) ;
#35377 = CARTESIAN_POINT ( 'NONE',  ( 1.472469842513823179, 66.42559781766745175, 4.923371831947296329 ) ) ;
#35378 = CARTESIAN_POINT ( 'NONE',  ( 7.084665262690076126, 47.02201867748818387, -10.88017736071110164 ) ) ;
#35379 = FACE_OUTER_BOUND ( 'NONE', #59781, .T. ) ;
#35380 = CARTESIAN_POINT ( 'NONE',  ( 12.63842701281683922, 54.55059781766745175, -9.846743663894590881 ) ) ;
#35381 = CARTESIAN_POINT ( 'NONE',  ( -5.204170427930421283E-15, 3.438309369127513726, -11.92686044187656513 ) ) ;
#35382 = EDGE_CURVE ( 'NONE', #70499, #38896, #36129, .T. ) ;
#35383 = LINE ( 'NONE', #20394, #13180 ) ;
#35384 = DIRECTION ( 'NONE',  ( 0.000000000000000000, 1.000000000000000000, 0.000000000000000000 ) ) ;
#35385 = VERTEX_POINT ( 'NONE', #98264 ) ;
#35386 = CARTESIAN_POINT ( 'NONE',  ( 17.08211943468705130, 43.47041550158063927, 12.26659068614894998 ) ) ;
#35388 =( LENGTH_UNIT ( ) NAMED_UNIT ( * ) SI_UNIT ( .MILLI., .METRE. ) );
#35387 = CARTESIAN_POINT ( 'NONE',  ( -6.732636091893170693, -88.11213685669366669, -2.500000000000000888 ) ) ;
#35389 = CARTESIAN_POINT ( 'NONE',  ( 15.44008868035555793, 21.39701867748817321, -9.422509992056140149 ) ) ;
#35390 = CARTESIAN_POINT ( 'NONE',  ( 22.81628187352647785, 36.41530133659707502, 3.434112377981063169 ) ) ;
#35391 = CARTESIAN_POINT ( 'NONE',  ( -10.32896413005680536, 9.271642702460850316, -5.963430220938272797 ) ) ;
#35392 = CARTESIAN_POINT ( 'NONE',  ( 1.274849032794294290, 53.57228050351032067, 6.499999999999979572 ) ) ;
#35393 = ORIENTED_EDGE ( 'NONE', *, *, #57943, .F. ) ;
#35394 = CARTESIAN_POINT ( 'NONE',  ( 4.920853330210497312, -13.83152733635706433, -3.750000000000804690 ) ) ;
#35395 = CARTESIAN_POINT ( 'NONE',  ( -7.551349515323020789, 15.00000000000000000, -12.08468537022916323 ) ) ;
#35396 = CARTESIAN_POINT ( 'NONE',  ( -4.021969307579356112, -6.415483651463659953, 3.999999999999999112 ) ) ;
#35397 = CARTESIAN_POINT ( 'NONE',  ( 2.035157376598822676, 22.43868534415483396, -7.964842623401177768 ) ) ;
#35398 = FACE_OUTER_BOUND ( 'NONE', #60793, .T. ) ;
#35399 = CYLINDRICAL_SURFACE ( 'NONE', #73552, 15.00000000000000000 ) ;
#35400 = CARTESIAN_POINT ( 'NONE',  ( 4.559911319644449179, 43.89701867748816966, 9.422509992056141925 ) ) ;
#35401 = CARTESIAN_POINT ( 'NONE',  ( 17.96484262340118221, 54.93868534415484106, 7.964842623401181321 ) ) ;
#35402 = CARTESIAN_POINT ( 'NONE',  ( 19.38216949554541557, 7.248634669930421381, -9.382169495545420901 ) ) ;
#35403 =( NAMED_UNIT ( * ) PLANE_ANGLE_UNIT ( ) SI_UNIT ( $, .RADIAN. ) );
#35404 = DIRECTION ( 'NONE',  ( 1.000000000000000000, 0.000000000000000000, 0.000000000000000000 ) ) ;
#35405 = CARTESIAN_POINT ( 'NONE',  ( 0.1532563361054082862, 21.21726448433412315, 2.638427012816831674 ) ) ;
#35406 = AXIS2_PLACEMENT_3D ( 'NONE', #6252, #12754, #87762 ) ;
#35407 = FILL_AREA_STYLE ('',( #34411 ) ) ;
#35408 = CARTESIAN_POINT ( 'NONE',  ( 12.91533473730992121, 39.52201867748817676, 10.88017736071110164 ) ) ;
#35409 = COLOUR_RGB ( '', 0.31764706, 0.68627451, 0.89019608) ;
#35410 = CARTESIAN_POINT ( 'NONE',  ( 6.565887622018943937, 3.081968003263753531, -12.81628187352647608 ) ) ;
#35411 = CARTESIAN_POINT ( 'NONE',  ( 12.91533473730993009, 61.60535201082150536, -10.88017736071109987 ) ) ;
#35412 = CARTESIAN_POINT ( 'NONE',  ( 7.361572987183170547, 22.05059781766745530, 9.846743663894590881 ) ) ;
#35413 = CARTESIAN_POINT ( 'NONE',  ( 3.591859063236761518, 49.95696800326375353, 11.09922568453594849 ) ) ;
#35414 = CARTESIAN_POINT ( 'NONE',  ( 0.1532563361054082862, 11.21726448433411605, 2.638427012816831674 ) ) ;
#35415 = ORIENTED_EDGE ( 'NONE', *, *, #35235, .T. ) ;
#35416 = FACE_OUTER_BOUND ( 'NONE', #14037, .T. ) ;
#35417 = CARTESIAN_POINT ( 'NONE',  ( 1.959929470562281395, 35.51528370094808196, -5.767676674365853629 ) ) ;
#35418 = CARTESIAN_POINT ( 'NONE',  ( -0.8801773607110991993, 17.85535201082150536, -2.915334737309923874 ) ) ;
#35420 = CARTESIAN_POINT ( 'NONE',  ( -0.3689425029237898834, 31.17874883491396787, -10.36894250292378850 ) ) ;
#35419 = CARTESIAN_POINT ( 'NONE',  ( 3.591859063236763294, 63.29030133659708923, -11.09922568453595026 ) ) ;
#35421 = CARTESIAN_POINT ( 'NONE',  ( 17.20831665107776587, 32.88393115100078745, 7.208316651077764980 ) ) ;
#35422 = CARTESIAN_POINT ( 'NONE',  ( 19.42250999205614548, 20.98035201082150891, -5.440088680355545492 ) ) ;
#35423 = CARTESIAN_POINT ( 'NONE',  ( 17.96484262340118221, 6.188685344154837509, -7.964842623401177768 ) ) ;
#35424 = ORIENTED_EDGE ( 'NONE', *, *, #39326, .T. ) ;
#35425 = CARTESIAN_POINT ( 'NONE',  ( 10.00000000000000178, 19.31368534415484106, 10.88017736071110342 ) ) ;
#35426 = ADVANCED_FACE ( 'NONE', ( #84711 ), #7742, .F. ) ;
#35427 = CARTESIAN_POINT ( 'NONE',  ( 17.96484262340118221, 34.93868534415482685, 7.964842623401181321 ) ) ;
#35428 = CARTESIAN_POINT ( 'NONE',  ( -12.60589901313233874, 14.49999999999999112, 8.129656208641975468 ) ) ;
#35429 = AXIS2_PLACEMENT_3D ( 'NONE', #88942, #74922, #51933 ) ;
#35430 = ORIENTED_EDGE ( 'NONE', *, *, #84910, .F. ) ;
#35431 = CARTESIAN_POINT ( 'NONE',  ( 20.15039907845753930, 9.722660991849181755, 6.262539305110064625 ) ) ;
#35432 = CARTESIAN_POINT ( 'NONE',  ( 4.559911319644449179, 27.23035201082150536, -9.422509992056141925 ) ) ;
#35433 = CARTESIAN_POINT ( 'NONE',  ( 4.441537491530695547, -2.700695904843435802, 4.000000000000000000 ) ) ;
#35434 = DIRECTION ( 'NONE',  ( 0.000000000000000000, 0.000000000000000000, -1.000000000000000000 ) ) ;
#35435 = CARTESIAN_POINT ( 'NONE',  ( 22.81628187352647785, 56.41530133659708213, 3.434112377981063169 ) ) ;
#35436 = CARTESIAN_POINT ( 'NONE',  ( 0.1955144967548966828, 9.327036817733409535, -6.500000000002781775 ) ) ;
#35437 = CARTESIAN_POINT ( 'NONE',  ( 24.16423886937409904, 29.09541550158063572, 3.795296366450317205 ) ) ;
#35438 = CARTESIAN_POINT ( 'NONE',  ( 12.91533473730993009, 46.60535201082150536, -10.88017736071109987 ) ) ;
#35439 = CARTESIAN_POINT ( 'NONE',  ( 4.559911319644449179, 33.89701867748817676, 9.422509992056141925 ) ) ;
#35440 = CARTESIAN_POINT ( 'NONE',  ( 14.92337183194729633, 62.67559781766745886, 8.527530157486181039 ) ) ;
#35441 = DIRECTION ( 'NONE',  ( 0.000000000000000000, 0.000000000000000000, 1.000000000000000000 ) ) ;
#35442 = CARTESIAN_POINT ( 'NONE',  ( 17.20831665107776587, 54.13393115100079456, -7.208316651077762316 ) ) ;
#35443 = EDGE_LOOP ( 'NONE', ( #98599, #63349, #31727, #22005, #10647, #48850 ) ) ;
#35444 = TOROIDAL_SURFACE ( 'NONE', #5114, 14.49999999999999822, 0.5000000000000000000 ) ;
#35445 = LINE ( 'NONE', #63960, #33516 ) ;
#35446 = CARTESIAN_POINT ( 'NONE',  ( 2.791683348922240793, 26.63393115100078745, 7.208316651077764092 ) ) ;
#35447 = CARTESIAN_POINT ( 'NONE',  ( -11.09922568453595382, -26.29303199673624292, -6.408140936763226492 ) ) ;
#35448 = AXIS2_PLACEMENT_3D ( 'NONE', #91575, #47546, #16568 ) ;
#35449 = CARTESIAN_POINT ( 'NONE',  ( 0.5774900079438590739, 17.64701867748817321, -5.440088680355550821 ) ) ;
#35450 = CARTESIAN_POINT ( 'NONE',  ( 1.472469842513823179, 30.59226448433411960, -4.923371831947296329 ) ) ;
#35451 = CARTESIAN_POINT ( 'NONE',  ( 20.88017736071110164, 60.35535201082151957, 2.915334737309930979 ) ) ;
#35453 = CARTESIAN_POINT ( 'NONE',  ( 19.38216949554541202, 55.99863466993041072, 9.382169495545424454 ) ) ;
#35452 = CARTESIAN_POINT ( 'NONE',  ( -0.8801773607111009756, 18.06368534415484106, 1.068504757029289695E-15 ) ) ;
#35454 = CARTESIAN_POINT ( 'NONE',  ( 2.917880565312950480, 50.97041550158064638, -12.26659068614894821 ) ) ;
#35455 = ADVANCED_FACE ( 'NONE', ( #6740 ), #30703, .F. ) ;
#35456 = CARTESIAN_POINT ( 'NONE',  ( 0.000000000000000000, 15.00000000000000000, 0.000000000000000000 ) ) ;
#35457 = ORIENTED_EDGE ( 'NONE', *, *, #62201, .F. ) ;
#35458 = CARTESIAN_POINT ( 'NONE',  ( 21.09922568453594849, 1.206968003263753531, 6.408140936763242479 ) ) ;
#35459 = SURFACE_SIDE_STYLE ('',( #19966 ) ) ;
#35460 = EDGE_CURVE ( 'NONE', #59552, #1757, #10176, .T. ) ;
#35461 = CARTESIAN_POINT ( 'NONE',  ( 2.035157376598822676, 32.43868534415483396, -7.964842623401177768 ) ) ;
#35462 = CARTESIAN_POINT ( 'NONE',  ( 19.84674366389459621, 63.50893115100078745, 7.409399052514197653E-17 ) ) ;
#35463 = ORIENTED_EDGE ( 'NONE', *, *, #83758, .T. ) ;
#35465 = FACE_OUTER_BOUND ( 'NONE', #54145, .T. ) ;
#35464 = CARTESIAN_POINT ( 'NONE',  ( 1.472469842513823179, 15.59226448433411960, -4.923371831947296329 ) ) ;
#35466 = CARTESIAN_POINT ( 'NONE',  ( 2.791683348922237240, 15.38393115100078212, -7.208316651077763204 ) ) ;
#35467 = CARTESIAN_POINT ( 'NONE',  ( 5.076628168052704559, 25.17559781766745175, -8.527530157486179263 ) ) ;
#35468 = CARTESIAN_POINT ( 'NONE',  ( 12.63842701281683034, 7.467264484334118713, 9.846743663894596210 ) ) ;
#35469 = CARTESIAN_POINT ( 'NONE',  ( 7.361572987183169658, 4.967264484334119601, -9.846743663894592657 ) ) ;
#35470 = CARTESIAN_POINT ( 'NONE',  ( -6.982525766850296911, -88.11956318484570261, 2.750000000000000444 ) ) ;
#35472 = DIRECTION ( 'NONE',  ( 0.000000000000000000, 0.000000000000000000, 1.000000000000000000 ) ) ;
#35471 = CARTESIAN_POINT ( 'NONE',  ( 5.076628168052704559, 0.1755978176674514724, -8.527530157486179263 ) ) ;
#35473 = CARTESIAN_POINT ( 'NONE',  ( 19.84674366389459266, 8.717264484334116048, -2.638427012816827677 ) ) ;
#35475 = ORIENTED_EDGE ( 'NONE', *, *, #4531, .T. ) ;
#35474 = CARTESIAN_POINT ( 'NONE',  ( 19.84674366389459621, 13.50893115100078568, 7.409399052514197653E-17 ) ) ;
#35476 = VECTOR ( 'NONE', #89176, 1000.000000000000000 ) ;
#35477 = CARTESIAN_POINT ( 'NONE',  ( 0.3093388210927633941, 0.5000000000000004441, 14.99680997725065978 ) ) ;
#35478 = CARTESIAN_POINT ( 'NONE',  ( -1.099225684535947600, -0.4596986634029132657, 6.408140936763237150 ) ) ;
#35479 = ORIENTED_EDGE ( 'NONE', *, *, #67432, .T. ) ;
#35480 = CARTESIAN_POINT ( 'NONE',  ( 12.91533473730993009, 6.605352010821504471, -10.88017736071109987 ) ) ;
#35481 = EDGE_CURVE ( 'NONE', #16271, #14086, #17697, .T. ) ;
#35482 = CARTESIAN_POINT ( 'NONE',  ( 24.16423886937409904, 14.09541550158063217, 3.795296366450317205 ) ) ;
#35483 = UNCERTAINTY_MEASURE_WITH_UNIT (LENGTH_MEASURE( 1.000000000000000082E-05 ), #40834, 'distance_accuracy_value', 'NONE');
#35484 = DIRECTION ( 'NONE',  ( 0.000000000000000000, 1.000000000000000000, 0.000000000000000000 ) ) ;
#35485 = CARTESIAN_POINT ( 'NONE',  ( -4.164238869374099039, 21.80374883491396787, 8.674139862899312516E-16 ) ) ;
#35486 = CARTESIAN_POINT ( 'NONE',  ( 10.00000000000000178, 43.05374883491397497, 14.16423886937410082 ) ) ;
#35487 = PRESENTATION_STYLE_ASSIGNMENT (( #96509 ) ) ;
#35489 = CARTESIAN_POINT ( 'NONE',  ( 0.5774900079438590739, 67.64701867748817676, -5.440088680355550821 ) ) ;
#35488 = CARTESIAN_POINT ( 'NONE',  ( 24.16423886937409904, 19.09541550158063927, 3.795296366450317205 ) ) ;
#35490 = CARTESIAN_POINT ( 'NONE',  ( 4.559911319644449179, 37.23035201082150536, -9.422509992056141925 ) ) ;
#35491 = DIRECTION ( 'NONE',  ( 0.000000000000000000, 0.000000000000000000, 1.000000000000000000 ) ) ;
#35492 = VERTEX_POINT ( 'NONE', #85202 ) ;
#35493 = CARTESIAN_POINT ( 'NONE',  ( 17.20831665107776587, 14.13393115100078568, -7.208316651077762316 ) ) ;
#35495 = CARTESIAN_POINT ( 'NONE',  ( 7.361572987183169658, 29.96726448433411960, -9.846743663894592657 ) ) ;
#35494 = CARTESIAN_POINT ( 'NONE',  ( -0.8801773607110991993, 52.85535201082151247, -2.915334737309923874 ) ) ;
#35496 = CARTESIAN_POINT ( 'NONE',  ( 20.88017736071110875, 5.772018677488170546, -2.915334737309920765 ) ) ;
#35497 = CARTESIAN_POINT ( 'NONE',  ( -2.816281873526471635, 48.91530133659708213, -3.434112377981056508 ) ) ;
#35498 = CARTESIAN_POINT ( 'NONE',  ( 17.20831665107776587, 52.88393115100078035, 7.208316651077764980 ) ) ;
#35499 = FACE_OUTER_BOUND ( 'NONE', #39167, .T. ) ;
#35500 = CARTESIAN_POINT ( 'NONE',  ( 19.38216949554541202, 40.99863466993042493, 9.382169495545424454 ) ) ;
#35501 = CARTESIAN_POINT ( 'NONE',  ( -12.26659068614894110, -32.77958449841936073, 7.082119434687058401 ) ) ;
#35502 = CIRCLE ( 'NONE', #54626, 0.5000000000000004441 ) ;
#35503 = CARTESIAN_POINT ( 'NONE',  ( 0.1532563361054082862, 36.21726448433410894, 2.638427012816831674 ) ) ;
#35504 = CARTESIAN_POINT ( 'NONE',  ( -2.266590686148945544, 32.22041550158063927, 7.082119434687048631 ) ) ;
#35505 = ORIENTED_EDGE ( 'NONE', *, *, #43351, .T. ) ;
#35506 = DIRECTION ( 'NONE',  ( 1.000000000000000000, 0.000000000000000000, 0.000000000000000000 ) ) ;
#35507 = CARTESIAN_POINT ( 'NONE',  ( 20.88017736071110519, 45.56368534415484106, 2.639326808657452039E-16 ) ) ;
#35508 = CARTESIAN_POINT ( 'NONE',  ( 20.88017736071110164, 60.35535201082151957, 2.915334737309930979 ) ) ;
#35510 = AXIS2_PLACEMENT_3D ( 'NONE', #86273, #25778, #2799 ) ;
#35509 = CARTESIAN_POINT ( 'NONE',  ( 13.79529636645030344, 48.26208216824728936, 14.16423886937410614 ) ) ;
#35511 = CARTESIAN_POINT ( 'NONE',  ( 5.076628168052703671, 66.84226448433412315, 8.527530157486179263 ) ) ;
#35512 = VECTOR ( 'NONE', #94140, 1000.000000000000000 ) ;
#35513 = CARTESIAN_POINT ( 'NONE',  ( -0.1049300847420659016, 57.21697413083879269, -6.336235997365754713 ) ) ;
#35514 = CARTESIAN_POINT ( 'NONE',  ( 17.96484262340118221, 41.18868534415484106, -7.964842623401177768 ) ) ;
#35515 = VECTOR ( 'NONE', #89055, 1000.000000000000000 ) ;
#35516 = CARTESIAN_POINT ( 'NONE',  ( 6.879999999999995453, 41.24999999999999289, 6.250000000000000000 ) ) ;
#35517 = CARTESIAN_POINT ( 'NONE',  ( 6.565887622018943937, 28.08196800326375353, -12.81628187352647608 ) ) ;
#35518 = CARTESIAN_POINT ( 'NONE',  ( 19.84674366389459621, 48.50893115100078745, 7.409399052514197653E-17 ) ) ;
#35519 = CARTESIAN_POINT ( 'NONE',  ( -5.204170427930421283E-15, 16.81368534415483751, -10.88017736071110342 ) ) ;
#35521 = AXIS2_PLACEMENT_3D ( 'NONE', #47312, #54323, #60847 ) ;
#35520 = CARTESIAN_POINT ( 'NONE',  ( 7.084665262690076126, 14.10535201082150358, 10.88017736071109987 ) ) ;
#35522 = VERTEX_POINT ( 'NONE', #94659 ) ;
#35523 = CARTESIAN_POINT ( 'NONE',  ( 12.99999999999999822, 75.00000000000000000, -8.525133428036872019 ) ) ;
#35524 = CARTESIAN_POINT ( 'NONE',  ( 12.91533473730992121, 64.52201867748817676, 10.88017736071110164 ) ) ;
#35525 = B_SPLINE_CURVE_WITH_KNOTS ( 'NONE', 3,
 ( #47749, #78246, #2282, #86250, #31261, #8770 ),
 .UNSPECIFIED., .F., .F.,
 ( 4, 2, 4 ),
 ( 3.409110551494648044E-05, 0.0004400426677367906374, 0.0008459942299586347943 ),
 .UNSPECIFIED. ) ;
#35526 = CARTESIAN_POINT ( 'NONE',  ( 4.559911319644449179, 67.23035201082150536, -9.422509992056141925 ) ) ;
#35527 = CARTESIAN_POINT ( 'NONE',  ( 17.78441314508118509, 78.67289652296345537, -4.000000000000000000 ) ) ;
#35528 = CARTESIAN_POINT ( 'NONE',  ( 18.52753015748618282, 33.92559781766745886, -4.923371831947291888 ) ) ;
#35529 = CARTESIAN_POINT ( 'NONE',  ( 17.96484262340118221, 26.18868534415483396, -7.964842623401177768 ) ) ;
#35530 = CARTESIAN_POINT ( 'NONE',  ( 16.40814093676324603, 7.456968003263754419, -11.09922568453594671 ) ) ;
#35532 = CARTESIAN_POINT ( 'NONE',  ( 14.16722289976685190, 14.63606870530283999, 4.928467845925642798 ) ) ;
#35531 = CARTESIAN_POINT ( 'NONE',  ( 17.96484262340118221, 29.93868534415484106, 7.964842623401181321 ) ) ;
#35533 = FILL_AREA_STYLE ('',( #50047 ) ) ;
#35534 = CARTESIAN_POINT ( 'NONE',  ( 3.591859063236761518, 34.95696800326375353, 11.09922568453594849 ) ) ;
#35535 = ORIENTED_EDGE ( 'NONE', *, *, #9396, .T. ) ;
#35536 = CARTESIAN_POINT ( 'NONE',  ( 19.42250999205614193, 65.14701867748817676, 5.440088680355555262 ) ) ;
#35538 = CYLINDRICAL_SURFACE ( 'NONE', #36634, 1.000000000000000888 ) ;
#35537 = CARTESIAN_POINT ( 'NONE',  ( 3.591859063236761518, 24.95696800326375353, 11.09922568453594849 ) ) ;
#35539 = PRESENTATION_STYLE_ASSIGNMENT (( #67031 ) ) ;
#35540 = CARTESIAN_POINT ( 'NONE',  ( 15.44008868035555793, 46.39701867748817676, -9.422509992056140149 ) ) ;
#35541 = CARTESIAN_POINT ( 'NONE',  ( -0.1023957841222607745, 15.13377557478295898, 6.340343622311898741 ) ) ;
#35542 = CARTESIAN_POINT ( 'NONE',  ( 20.36894250292379382, 63.67874883491396787, 10.36894250292379205 ) ) ;
#35543 = AXIS2_PLACEMENT_3D ( 'NONE', #68943, #83938, #75447 ) ;
#35544 = CARTESIAN_POINT ( 'NONE',  ( 7.361572987183169658, 54.96726448433413026, -9.846743663894592657 ) ) ;
#35545 = CARTESIAN_POINT ( 'NONE',  ( 0.1532563361054083140, 1.008931151000784787, 1.131784320476157264E-15 ) ) ;
#35546 = CARTESIAN_POINT ( 'NONE',  ( 20.88017736071110519, 60.56368534415484106, 2.639326808657452039E-16 ) ) ;
#35547 = DIRECTION ( 'NONE',  ( 0.000000000000000000, 1.000000000000000000, 0.000000000000000000 ) ) ;
#35548 = CARTESIAN_POINT ( 'NONE',  ( 2.917880565312950480, 30.97041550158063572, -12.26659068614894821 ) ) ;
#35549 =( BOUNDED_CURVE ( )  B_SPLINE_CURVE ( 2, ( #55374, #92867, #24397, #1904, #85875, #78362, #49334, #57817, #96839 ),
 .UNSPECIFIED., .F., .F. ) 
 B_SPLINE_CURVE_WITH_KNOTS ( ( 3, 2, 2, 2, 3 ),
 ( 0.1167998787605536576, 0.1190476190476190410, 0.1250000000000000000, 0.1309523809523809590, 0.1332001212394463563 ),
 .UNSPECIFIED. ) 
 CURVE ( )  GEOMETRIC_REPRESENTATION_ITEM ( )  RATIONAL_B_SPLINE_CURVE ( ( 0.9839835555609424134, 0.9871328979762477029, 1.000000000000000000, 0.9659258262890683122, 1.000000000000000000, 0.9659258262890683122, 1.000000000000000000, 0.9871328979762477029, 0.9839835555609424134 ) ) 
 REPRESENTATION_ITEM ( '' )  );
#35550 = ADVANCED_FACE ( 'NONE', ( #16707 ), #36563, .T. ) ;
#35551 = CARTESIAN_POINT ( 'NONE',  ( 8.956085929493502462, -3.116154469452326214, -3.750000000000000000 ) ) ;
#35552 = CARTESIAN_POINT ( 'NONE',  ( -3.628626191893884467, -3.642031182898920694, -3.750000000000000000 ) ) ;
#35553 =( BOUNDED_CURVE ( )  B_SPLINE_CURVE ( 2, ( #23232, #14748, #31683, #98756, #76222, #45221, #45720, #30697, #76701 ),
 .UNSPECIFIED., .F., .T. ) 
 B_SPLINE_CURVE_WITH_KNOTS ( ( 3, 2, 2, 2, 3 ),
 ( 0.1882284501891250961, 0.1904761904761904656, 0.1964285714285714246, 0.2023809523809523836, 0.2046286926680177809 ),
 .UNSPECIFIED. ) 
 CURVE ( )  GEOMETRIC_REPRESENTATION_ITEM ( )  RATIONAL_B_SPLINE_CURVE ( ( 0.9839835555609424134, 0.9871328979762477029, 1.000000000000000000, 0.9659258262890683122, 1.000000000000000000, 0.9659258262890683122, 1.000000000000000000, 0.9871328979762477029, 0.9839835555609424134 ) ) 
 REPRESENTATION_ITEM ( '' )  );
#35554 = ORIENTED_EDGE ( 'NONE', *, *, #52290, .F. ) ;
#35555 = CARTESIAN_POINT ( 'NONE',  ( 20.36894250292379738, 64.92874883491397497, -10.36894250292379027 ) ) ;
#35556 = CARTESIAN_POINT ( 'NONE',  ( 6.204703633549690345, 55.76208216824730357, -14.16423886937410259 ) ) ;
#35557 = CARTESIAN_POINT ( 'NONE',  ( 1.472469842513823179, 25.59226448433412315, -4.923371831947296329 ) ) ;
#35558 = CARTESIAN_POINT ( 'NONE',  ( -2.816281873526473856, 24.33196800326375353, 3.434112377981055619 ) ) ;
#35559 = FACE_OUTER_BOUND ( 'NONE', #67990, .T. ) ;
#35560 = CARTESIAN_POINT ( 'NONE',  ( 2.035157376598824452, 3.688685344154837953, 7.964842623401179544 ) ) ;
#35561 = CARTESIAN_POINT ( 'NONE',  ( 2.917880565312950480, 60.97041550158063927, -12.26659068614894821 ) ) ;
#35562 = EDGE_CURVE ( 'NONE', #4144, #63596, #28071, .T. ) ;
#35563 = CARTESIAN_POINT ( 'NONE',  ( -14.71525861348285957, 0.5000000000000004441, -2.908807992686776700 ) ) ;
#35564 = CARTESIAN_POINT ( 'NONE',  ( 2.791683348922240793, 6.633931151000785675, 7.208316651077764092 ) ) ;
#35565 = LINE ( 'NONE', #44547, #65809 ) ;
#35566 = CARTESIAN_POINT ( 'NONE',  ( 8.527530157486179263, 8.092264484334123154, 4.923371831947292776 ) ) ;
#35567 = ORIENTED_EDGE ( 'NONE', *, *, #32162, .F. ) ;
#35568 = ORIENTED_EDGE ( 'NONE', *, *, #5338, .F. ) ;
#35569 = SURFACE_STYLE_FILL_AREA ( #74052 ) ;
#35570 = ORIENTED_EDGE ( 'NONE', *, *, #78452, .T. ) ;
#35571 = CARTESIAN_POINT ( 'NONE',  ( 24.16423886937410614, 14.51208216824730179, -3.795296366450302550 ) ) ;
#35573 = CARTESIAN_POINT ( 'NONE',  ( 20.88017736071110875, 25.77201867748816966, -2.915334737309920765 ) ) ;
#35572 = CARTESIAN_POINT ( 'NONE',  ( 2.035157376598824452, 13.68868534415483751, 7.964842623401179544 ) ) ;
#35575 = CARTESIAN_POINT ( 'NONE',  ( 22.81628187352647785, 11.62363466993042138, 6.195893100308588602E-16 ) ) ;
#35574 = CARTESIAN_POINT ( 'NONE',  ( 0.1532563361054083140, 51.00893115100078745, 1.131784320476157264E-15 ) ) ;
#35576 = DIRECTION ( 'NONE',  ( 0.000000000000000000, 0.000000000000000000, 1.000000000000000000 ) ) ;
#35577 = CIRCLE ( 'NONE', #49920, 14.49999999999999822 ) ;
#35578 = EDGE_CURVE ( 'NONE', #18635, #71943, #12650, .T. ) ;
#35579 = CARTESIAN_POINT ( 'NONE',  ( 22.81628187352647785, 26.41530133659708923, 3.434112377981063169 ) ) ;
#35580 = ORIENTED_EDGE ( 'NONE', *, *, #69556, .F. ) ;
#35581 = AXIS2_PLACEMENT_3D ( 'NONE', #75197, #83697, #97737 ) ;
#35582 = CARTESIAN_POINT ( 'NONE',  ( 10.00000000000000178, 27.25893115100078390, 9.846743663894594434 ) ) ;
#35583 = AXIS2_PLACEMENT_3D ( 'NONE', #5995, #59470, #88994 ) ;
#35584 = CARTESIAN_POINT ( 'NONE',  ( -0.3689425029237881626, 62.42874883491396787, 10.36894250292379027 ) ) ;
#35585 = ORIENTED_EDGE ( 'NONE', *, *, #21195, .T. ) ;
#35586 = AXIS2_PLACEMENT_3D ( 'NONE', #49817, #25506, #54495 ) ;
#35587 = CARTESIAN_POINT ( 'NONE',  ( 10.00000000000000000, 1.813685344154838175, -10.88017736071110342 ) ) ;
#35588 = ORIENTED_EDGE ( 'NONE', *, *, #54641, .T. ) ;
#35589 = CARTESIAN_POINT ( 'NONE',  ( 17.96484262340118221, 46.18868534415484106, -7.964842623401177768 ) ) ;
#35590 = CARTESIAN_POINT ( 'NONE',  ( -0.8801773607111008646, 43.27201867748817676, 2.915334737309923430 ) ) ;
#35591 = CARTESIAN_POINT ( 'NONE',  ( 19.42250999205614193, 45.14701867748817676, 5.440088680355555262 ) ) ;
#35592 = MECHANICAL_DESIGN_GEOMETRIC_PRESENTATION_REPRESENTATION (  '', ( #21188 ), #67507 ) ;
#35593 = FILL_AREA_STYLE_COLOUR ( '', #79294 ) ;
#35594 = CARTESIAN_POINT ( 'NONE',  ( 15.44008868035555260, 44.73035201082151247, 9.422509992056143702 ) ) ;
#35596 = ORIENTED_EDGE ( 'NONE', *, *, #49470, .F. ) ;
#35595 = PRESENTATION_STYLE_ASSIGNMENT (( #5103 ) ) ;
#35597 = CARTESIAN_POINT ( 'NONE',  ( 19.84674366389459266, 28.71726448433411960, -2.638427012816827677 ) ) ;
#35598 = EDGE_LOOP ( 'NONE', ( #12706, #49972, #81813, #48245 ) ) ;
#35599 = CARTESIAN_POINT ( 'NONE',  ( 17.20831665107776587, 64.13393115100079456, -7.208316651077762316 ) ) ;
#35600 = DIRECTION ( 'NONE',  ( 0.000000000000000000, 0.000000000000000000, -1.000000000000000000 ) ) ;
#35601 = AXIS2_PLACEMENT_3D ( 'NONE', #89314, #3855, #5336 ) ;
#35602 = CARTESIAN_POINT ( 'NONE',  ( -6.982525766139713319, -88.11956320875633253, 2.750000000000000000 ) ) ;
#35603 = ORIENTED_EDGE ( 'NONE', *, *, #94153, .T. ) ;
#35604 = ADVANCED_FACE ( 'NONE', ( #28638 ), #16886, .T. ) ;
#35605 = CARTESIAN_POINT ( 'NONE',  ( -11.55579792925658111, 12.87141902714432362, 1.357825507271567922 ) ) ;
#35606 = DIRECTION ( 'NONE',  ( 0.7132504491541801217, 0.000000000000000000, 0.7009092642998523415 ) ) ;
#35608 = CARTESIAN_POINT ( 'NONE',  ( 17.20831665107776587, 39.13393115100079456, -7.208316651077762316 ) ) ;
#35607 = CARTESIAN_POINT ( 'NONE',  ( 20.15039907845753930, 2.627771745786128044, -6.262539305110069954 ) ) ;
#35609 = CARTESIAN_POINT ( 'NONE',  ( -2.266590686148945544, 56.38708216824731068, -7.082119434687050408 ) ) ;
#35610 = CARTESIAN_POINT ( 'NONE',  ( -8.000000000000000000, 79.82179676972448590, 4.250000000000000000 ) ) ;
#35611 = ORIENTED_EDGE ( 'NONE', *, *, #19983, .T. ) ;
#35612 = CARTESIAN_POINT ( 'NONE',  ( -3.195792623639539975, 3.646642702460842766, -11.92686044187656158 ) ) ;
#35613 = CARTESIAN_POINT ( 'NONE',  ( 1.472469842513823179, 30.59226448433411960, -4.923371831947296329 ) ) ;
#35614 = CARTESIAN_POINT ( 'NONE',  ( 8.879999999999995453, 40.74999999999999289, 3.750000000000000000 ) ) ;
#35616 = VECTOR ( 'NONE', #42652, 999.9999999999998863 ) ;
#35615 = CARTESIAN_POINT ( 'NONE',  ( -1.099225684535947600, 8.706968003263753531, -6.408140936763238038 ) ) ;
#35618 = EDGE_CURVE ( 'NONE', #19780, #85989, #80475, .T. ) ;
#35617 = CARTESIAN_POINT ( 'NONE',  ( 10.00000000000000178, 17.25893115100078745, 9.846743663894594434 ) ) ;
#35619 = CARTESIAN_POINT ( 'NONE',  ( 51.94498256489735155, 70.99147617202632432, -8.000000000000000000 ) ) ;
#35620 = CARTESIAN_POINT ( 'NONE',  ( 0.1532563361054082862, 11.21726448433411605, 2.638427012816831674 ) ) ;
#35621 = CARTESIAN_POINT ( 'NONE',  ( 1.472469842513823179, 65.59226448433412315, -4.923371831947296329 ) ) ;
#35622 = CARTESIAN_POINT ( 'NONE',  ( -12.07856007377816887, 4.482427100288500905E-16, -8.022367888855006512 ) ) ;
#35623 = VECTOR ( 'NONE', #8304, 1000.000000000000114 ) ;
#35624 = VERTEX_POINT ( 'NONE', #48581 ) ;
#35625 = CARTESIAN_POINT ( 'NONE',  ( 20.88017736071110875, 5.772018677488170546, -2.915334737309920765 ) ) ;
#35626 = CARTESIAN_POINT ( 'NONE',  ( 10.00000000000000178, 8.053748834913967869, 14.16423886937410082 ) ) ;
#35627 = CARTESIAN_POINT ( 'NONE',  ( 5.076628168052703671, 21.84226448433411960, 8.527530157486179263 ) ) ;
#35628 = CARTESIAN_POINT ( 'NONE',  ( 12.91533473730992121, 49.52201867748817676, 10.88017736071110164 ) ) ;
#35630 = CARTESIAN_POINT ( 'NONE',  ( -3.635384400432159158, -3.854802480546752896, -3.750000000000000000 ) ) ;
#35629 = CARTESIAN_POINT ( 'NONE',  ( 13.43411237798106583, 27.66530133659708568, -12.81628187352647252 ) ) ;
#35631 = CARTESIAN_POINT ( 'NONE',  ( 15.44008868035555260, 4.730352010821504471, 9.422509992056143702 ) ) ;
#35632 = CARTESIAN_POINT ( 'NONE',  ( -10.93781366033335622, 14.49999999999999112, -10.26470809774086490 ) ) ;
#35633 = FACE_OUTER_BOUND ( 'NONE', #70062, .T. ) ;
#35634 = CARTESIAN_POINT ( 'NONE',  ( 19.84674366389459266, 58.71726448433411605, -2.638427012816827677 ) ) ;
#35635 = CARTESIAN_POINT ( 'NONE',  ( 1.472469842513823179, 16.42559781766745175, 4.923371831947296329 ) ) ;
#35636 = CARTESIAN_POINT ( 'NONE',  ( 9.422509992056141925, -24.85298132251182679, 5.440088680355547268 ) ) ;
#35637 = CARTESIAN_POINT ( 'NONE',  ( 22.81628187352647785, 21.62363466993041783, 6.195893100308588602E-16 ) ) ;
#35638 = CARTESIAN_POINT ( 'NONE',  ( -10.85639881947519036, -98.10817599903623432, -4.000000000005668355 ) ) ;
#35639 = CARTESIAN_POINT ( 'NONE',  ( 17.96484262340118221, 24.93868534415484461, 7.964842623401181321 ) ) ;
#35640 = DIRECTION ( 'NONE',  ( 0.000000000000000000, 1.000000000000000000, 0.000000000000000000 ) ) ;
#35641 = CARTESIAN_POINT ( 'NONE',  ( -4.164238869374099927, 52.01208216824729647, 3.795296366450308767 ) ) ;
#35642 = LINE ( 'NONE', #81138, #3399 ) ;
#35643 = CARTESIAN_POINT ( 'NONE',  ( 10.00000000000000000, 31.81368534415483751, -10.88017736071110342 ) ) ;
#35644 = CARTESIAN_POINT ( 'NONE',  ( 18.52753015748618282, 48.92559781766745886, -4.923371831947291888 ) ) ;
#35645 = CARTESIAN_POINT ( 'NONE',  ( 17.96484262340118221, 51.18868534415483396, -7.964842623401177768 ) ) ;
#35646 = CARTESIAN_POINT ( 'NONE',  ( 17.08211943468705840, 30.13708216824730357, -12.26659068614894466 ) ) ;
#35647 = DIRECTION ( 'NONE',  ( 0.000000000000000000, 0.000000000000000000, -1.000000000000000000 ) ) ;
#35648 = AXIS2_PLACEMENT_3D ( 'NONE', #94372, #93883, #46900 ) ;
#35649 = CARTESIAN_POINT ( 'NONE',  ( 2.791683348922237240, 40.38393115100078035, -7.208316651077763204 ) ) ;
#35650 = CARTESIAN_POINT ( 'NONE',  ( 0.000000000000000000, 12.49999999999999112, 0.000000000000000000 ) ) ;
#35651 = CARTESIAN_POINT ( 'NONE',  ( 1.472469842513823179, 66.42559781766745175, 4.923371831947296329 ) ) ;
#35652 = ORIENTED_EDGE ( 'NONE', *, *, #14633, .T. ) ;
#35653 = CARTESIAN_POINT ( 'NONE',  ( 20.88017736071110875, 20.77201867748816611, -2.915334737309920765 ) ) ;
#35654 = AXIS2_PLACEMENT_3D ( 'NONE', #72150, #11656, #64632 ) ;
#35655 = LINE ( 'NONE', #94685, #49322 ) ;
#35656 = CARTESIAN_POINT ( 'NONE',  ( 10.00000000000000178, 14.31368534415483929, 10.88017736071110342 ) ) ;
#35657 = CARTESIAN_POINT ( 'NONE',  ( 19.84674366389459266, 3.300597817667451750, 2.638427012816836559 ) ) ;
#35658 = CARTESIAN_POINT ( 'NONE',  ( 20.36894250292379382, 18.67874883491397142, 10.36894250292379205 ) ) ;
#35659 = CARTESIAN_POINT ( 'NONE',  ( 1.472469842513823179, 16.42559781766745175, 4.923371831947296329 ) ) ;
#35660 = CARTESIAN_POINT ( 'NONE',  ( 5.076628168052703671, 66.84226448433412315, 8.527530157486179263 ) ) ;
#35661 = CARTESIAN_POINT ( 'NONE',  ( 10.00000000000000178, 34.31368534415484106, 10.88017736071110342 ) ) ;
#35662 = AXIS2_PLACEMENT_3D ( 'NONE', #9789, #41289, #9292 ) ;
#35663 = DIRECTION ( 'NONE',  ( 0.000000000000000000, 1.000000000000000000, 0.000000000000000000 ) ) ;
#35664 = DIRECTION ( 'NONE',  ( -1.000000000000000000, 0.000000000000000000, 0.000000000000000000 ) ) ;
#35665 = EDGE_CURVE ( 'NONE', #94935, #97969, #25609, .T. ) ;
#35666 = VERTEX_POINT ( 'NONE', #77598 ) ;
#35667 = CARTESIAN_POINT ( 'NONE',  ( 14.99999999999997868, 80.07179676972448590, -4.250000000000000000 ) ) ;
#35668 = CARTESIAN_POINT ( 'NONE',  ( 1.472469842513823179, 46.42559781766745175, 4.923371831947296329 ) ) ;
#35669 = VERTEX_POINT ( 'NONE', #56103 ) ;
#35670 = VERTEX_POINT ( 'NONE', #3597 ) ;
#35671 = B_SPLINE_CURVE_WITH_KNOTS ( 'NONE', 3,
 ( #87803, #19325, #88802, #80811, #5321, #80316 ),
 .UNSPECIFIED., .F., .F.,
 ( 4, 2, 4 ),
 ( 0.000000000000000000, 0.0002701661927229266624, 0.0005403323854458533249 ),
 .UNSPECIFIED. ) ;
#35672 = SURFACE_STYLE_USAGE ( .BOTH. , #89657 ) ;
#35673 = CARTESIAN_POINT ( 'NONE',  ( -4.164238869374099927, 22.01208216824730357, 3.795296366450308767 ) ) ;
#35674 = CARTESIAN_POINT ( 'NONE',  ( 2.917880565312948704, 7.637082168247301794, 12.26659068614894643 ) ) ;
#35675 = CARTESIAN_POINT ( 'NONE',  ( 19.42250999205614548, 60.98035201082151247, -5.440088680355545492 ) ) ;
#35676 = CARTESIAN_POINT ( 'NONE',  ( -2.266590686148945544, 51.38708216824730357, -7.082119434687050408 ) ) ;
#35677 = CARTESIAN_POINT ( 'NONE',  ( 2.791683348922237240, 65.38393115100078035, -7.208316651077763204 ) ) ;
#35678 = CARTESIAN_POINT ( 'NONE',  ( 19.84674366389459266, 38.71726448433412315, -2.638427012816827677 ) ) ;
#35679 =( NAMED_UNIT ( * ) SI_UNIT ( $, .STERADIAN. ) SOLID_ANGLE_UNIT ( ) );
#35681 = CARTESIAN_POINT ( 'NONE',  ( 16.40814093676324603, 2.456968003263753531, -11.09922568453594671 ) ) ;
#35680 = CARTESIAN_POINT ( 'NONE',  ( 17.96484262340118221, 34.93868534415482685, 7.964842623401181321 ) ) ;
#35682 = CARTESIAN_POINT ( 'NONE',  ( 24.16423886937410614, 9.303748834913967869, 8.672049930838204340E-16 ) ) ;
#35683 = CARTESIAN_POINT ( 'NONE',  ( -2.266590686148945544, 57.22041550158063217, 7.082119434687048631 ) ) ;
#35684 = CARTESIAN_POINT ( 'NONE',  ( 12.91533473730992121, 24.52201867748816966, 10.88017736071110164 ) ) ;
#35685 = CARTESIAN_POINT ( 'NONE',  ( -2.913501739333569152, 4.140530414402051497E-16, -14.20427779279538960 ) ) ;
#35686 = LINE ( 'NONE', #4716, #76341 ) ;
#35687 = CARTESIAN_POINT ( 'NONE',  ( 0.5774900079438590739, 42.64701867748816966, -5.440088680355550821 ) ) ;
#35688 = CARTESIAN_POINT ( 'NONE',  ( -7.208316651077756099, -38.36606884899921255, 7.208316651077766757 ) ) ;
#35689 = EDGE_LOOP ( 'NONE', ( #31413, #78671, #50659, #62019 ) ) ;
#35690 = PLANE ( 'NONE',  #76274 ) ;
#35691 = ORIENTED_EDGE ( 'NONE', *, *, #51256, .T. ) ;
#35692 = ORIENTED_EDGE ( 'NONE', *, *, #28706, .T. ) ;
#35693 = CARTESIAN_POINT ( 'NONE',  ( 20.36894250292379382, 43.67874883491397497, 10.36894250292379205 ) ) ;
#35694 = CARTESIAN_POINT ( 'NONE',  ( 1.472469842513823179, 40.59226448433411605, -4.923371831947296329 ) ) ;
#35695 = CARTESIAN_POINT ( 'NONE',  ( -0.8801773607110991993, 62.85535201082150536, -2.915334737309923874 ) ) ;
#35696 = CYLINDRICAL_SURFACE ( 'NONE', #17700, 15.00000000000000000 ) ;
#35697 = CARTESIAN_POINT ( 'NONE',  ( 12.91533473730992121, 54.52201867748816255, 10.88017736071110164 ) ) ;
#35698 = EDGE_CURVE ( 'NONE', #79084, #73802, #78103, .T. ) ;
#35699 = CARTESIAN_POINT ( 'NONE',  ( -11.09922568453594316, 4.540301336597093673, 6.408140936763246920 ) ) ;
#35700 = ORIENTED_EDGE ( 'NONE', *, *, #8806, .T. ) ;
#35701 = CARTESIAN_POINT ( 'NONE',  ( 22.26659068614894466, 13.88708216824730179, 7.082119434687054849 ) ) ;
#35702 = EDGE_CURVE ( 'NONE', #6101, #83218, #76926, .T. ) ;
#35703 = CARTESIAN_POINT ( 'NONE',  ( -2.816281873526473856, 24.33196800326375353, 3.434112377981055619 ) ) ;
#35704 = EDGE_LOOP ( 'NONE', ( #41128, #44411, #86293, #44295 ) ) ;
#35705 = CARTESIAN_POINT ( 'NONE',  ( -2.816281873526473856, 39.12363466993041783, 9.499525473075851096E-16 ) ) ;
#35706 = CARTESIAN_POINT ( 'NONE',  ( 0.1532563361054100626, 30.80059781766744820, -2.638427012816831230 ) ) ;
#35707 = CARTESIAN_POINT ( 'NONE',  ( 4.559911319644449179, 8.897018677488171434, 9.422509992056141925 ) ) ;
#35708 = CARTESIAN_POINT ( 'NONE',  ( 10.00000000000000000, 47.87363466993042493, -12.81628187352647608 ) ) ;
#35709 = CARTESIAN_POINT ( 'NONE',  ( 11.35178980618967337, 15.00000000000000000, 9.804941009311999522 ) ) ;
#35710 = CARTESIAN_POINT ( 'NONE',  ( 17.20831665107776587, 49.13393115100078745, -7.208316651077762316 ) ) ;
#35712 = VERTEX_POINT ( 'NONE', #64552 ) ;
#35711 = DIRECTION ( 'NONE',  ( 0.9961946980917453232, -0.08715574274766037244, 0.000000000000000000 ) ) ;
#35713 = CARTESIAN_POINT ( 'NONE',  ( -0.1042174387088653925, 3.107361737662015955, 6.337391062633415117 ) ) ;
#35714 = VECTOR ( 'NONE', #77725, 1000.000000000000114 ) ;
#35715 = DIRECTION ( 'NONE',  ( 0.000000000000000000, 1.000000000000000000, 0.000000000000000000 ) ) ;
#35716 = DIRECTION ( 'NONE',  ( -0.9981347984218674751, 0.000000000000000000, 0.06104853953484969814 ) ) ;
#35717 = LINE ( 'NONE', #96738, #68506 ) ;
#35718 = CARTESIAN_POINT ( 'NONE',  ( 18.52753015748618282, 18.92559781766745175, -4.923371831947291888 ) ) ;
#35719 = CARTESIAN_POINT ( 'NONE',  ( 22.81628187352647785, 26.62363466993042138, 6.195893100308588602E-16 ) ) ;
#35721 = CARTESIAN_POINT ( 'NONE',  ( 15.61289147378509057, -0.03417435944610275333, 3.480663193108788800 ) ) ;
#35720 =( GEOMETRIC_REPRESENTATION_CONTEXT ( 3 ) GLOBAL_UNCERTAINTY_ASSIGNED_CONTEXT ( ( #28480 ) ) GLOBAL_UNIT_ASSIGNED_CONTEXT ( ( #90379, #97930, #52396 ) ) REPRESENTATION_CONTEXT ( 'NONE', 'WORKASPACE' ) );
#35722 = EDGE_LOOP ( 'NONE', ( #93882, #96847, #13802, #13520, #40608, #3711 ) ) ;
#35723 = CARTESIAN_POINT ( 'NONE',  ( 1.472469842513823179, 51.42559781766745886, 4.923371831947296329 ) ) ;
#35724 = CARTESIAN_POINT ( 'NONE',  ( -10.97324858046209961, 7.322546142722302618E-32, 9.670892530813134158 ) ) ;
#35725 = CARTESIAN_POINT ( 'NONE',  ( 13.79529636645031943, 15.34541550158063750, -14.16423886937409904 ) ) ;
#35726 = CARTESIAN_POINT ( 'NONE',  ( 1.472469842513823179, 50.59226448433411605, -4.923371831947296329 ) ) ;
#35727 = CARTESIAN_POINT ( 'NONE',  ( 6.565887622018943937, 43.08196800326374643, -12.81628187352647608 ) ) ;
#35729 = CARTESIAN_POINT ( 'NONE',  ( 8.606322355891288467, 3.856550154308941175E-16, 11.66967075398812703 ) ) ;
#35728 = LINE ( 'NONE', #66216, #44823 ) ;
#35730 = CARTESIAN_POINT ( 'NONE',  ( 7.084665262690076126, 62.02201867748816966, -10.88017736071110164 ) ) ;
#35731 = DIRECTION ( 'NONE',  ( 0.08715574274765139351, 0.9961946980917461003, 0.000000000000000000 ) ) ;
#35732 = CARTESIAN_POINT ( 'NONE',  ( 1.472469842513823179, 31.42559781766745530, 4.923371831947296329 ) ) ;
#35734 = EDGE_CURVE ( 'NONE', #85215, #30617, #17615, .T. ) ;
#35733 = CARTESIAN_POINT ( 'NONE',  ( 7.084665262690076126, 39.10535201082150536, 10.88017736071109987 ) ) ;
#35735 = CARTESIAN_POINT ( 'NONE',  ( 21.09922568453595559, 42.04030133659708213, -6.408140936763230044 ) ) ;
#35736 = DIRECTION ( 'NONE',  ( 0.06018710160448186020, 0.6046271891226110418, 0.7942313737029922383 ) ) ;
#35737 = LINE ( 'NONE', #66225, #31546 ) ;
#35738 = CARTESIAN_POINT ( 'NONE',  ( 7.084665262690076126, 29.10535201082150181, 10.88017736071109987 ) ) ;
#35739 = VERTEX_POINT ( 'NONE', #95061 ) ;
#35740 = CARTESIAN_POINT ( 'NONE',  ( 6.000000000000000000, 11.00000000000000000, 6.500000000000000888 ) ) ;
#35741 = CARTESIAN_POINT ( 'NONE',  ( 7.084665262690076126, 22.02201867748817321, -10.88017736071110164 ) ) ;
#35743 = CARTESIAN_POINT ( 'NONE',  ( 4.559911319644449179, 42.23035201082151247, -9.422509992056141925 ) ) ;
#35742 = CARTESIAN_POINT ( 'NONE',  ( 14.92337183194729633, 52.67559781766745175, 8.527530157486181039 ) ) ;
#35744 = PLANE ( 'NONE',  #56811 ) ;
#35745 = CARTESIAN_POINT ( 'NONE',  ( -0.8801773607110991993, 57.85535201082149825, -2.915334737309923874 ) ) ;
#35747 = CARTESIAN_POINT ( 'NONE',  ( 0.000000000000000000, 72.39124140214553904, -5.153078942141819496 ) ) ;
#35746 = CARTESIAN_POINT ( 'NONE',  ( 19.42250999205614548, 30.98035201082150536, -5.440088680355545492 ) ) ;
#35748 = SURFACE_SIDE_STYLE ('',( #36246 ) ) ;
#35749 = CARTESIAN_POINT ( 'NONE',  ( 0.1532563361054083140, 31.00893115100078390, 1.131784320476157264E-15 ) ) ;
#35750 =( NAMED_UNIT ( * ) SI_UNIT ( $, .STERADIAN. ) SOLID_ANGLE_UNIT ( ) );
#35751 = CARTESIAN_POINT ( 'NONE',  ( -14.16423886937409726, 2.012082168247306679, 3.795296366450320757 ) ) ;
#35752 = CARTESIAN_POINT ( 'NONE',  ( 5.076628168052703671, 56.84226448433412315, 8.527530157486179263 ) ) ;
#35754 = CARTESIAN_POINT ( 'NONE',  ( 6.905580141755321755, -69.44847572026166915, 3.750000000000000444 ) ) ;
#35753 = CARTESIAN_POINT ( 'NONE',  ( 22.26659068614895176, 49.72041550158063927, -7.082119434687042414 ) ) ;
#35755 = CARTESIAN_POINT ( 'NONE',  ( 1.274849032794292736, 62.55509018479936145, -6.499999999999977796 ) ) ;
#35756 = CARTESIAN_POINT ( 'NONE',  ( 10.00000000000000000, 10.55374883491396787, -14.16423886937410082 ) ) ;
#35757 = CARTESIAN_POINT ( 'NONE',  ( -2.266590686148945544, 37.22041550158063217, 7.082119434687048631 ) ) ;
#35758 = CARTESIAN_POINT ( 'NONE',  ( -1.099225684535947600, -1.293031996736246469, -6.408140936763238038 ) ) ;
#35759 = VERTEX_POINT ( 'NONE', #10109 ) ;
#35760 = CARTESIAN_POINT ( 'NONE',  ( 20.88017736071110519, 15.56368534415483751, 2.639326808657452039E-16 ) ) ;
#35761 = CARTESIAN_POINT ( 'NONE',  ( 5.076628168052703671, 31.84226448433412315, 8.527530157486179263 ) ) ;
#35763 = CARTESIAN_POINT ( 'NONE',  ( -13.05265508282229980, 90.73577164613095647, -7.477963345816291962 ) ) ;
#35762 = CARTESIAN_POINT ( 'NONE',  ( 0.000000000000000000, -97.00000000000000000, 4.000000000000000000 ) ) ;
#35764 = DIRECTION ( 'NONE',  ( 0.000000000000000000, -1.000000000000000000, 0.000000000000000000 ) ) ;
#35765 = EDGE_CURVE ( 'NONE', #40706, #2502, #94576, .T. ) ;
#35766 = LINE ( 'NONE', #90242, #73847 ) ;
#35767 = CARTESIAN_POINT ( 'NONE',  ( 10.00000000000000178, 25.37363466993041783, 12.81628187352647608 ) ) ;
#35768 = CARTESIAN_POINT ( 'NONE',  ( 7.361572987183169658, 24.96726448433412315, -9.846743663894592657 ) ) ;
#35769 = ORIENTED_EDGE ( 'NONE', *, *, #52501, .F. ) ;
#35770 = CARTESIAN_POINT ( 'NONE',  ( 12.63842701281683034, 7.467264484334118713, 9.846743663894596210 ) ) ;
#35771 = CARTESIAN_POINT ( 'NONE',  ( -10.84451454130493708, 4.806230040756559413E-16, -9.625305416630981270 ) ) ;
#35772 = CARTESIAN_POINT ( 'NONE',  ( 19.42250999205614548, 5.980352010821504471, -5.440088680355545492 ) ) ;
#35773 = CARTESIAN_POINT ( 'NONE',  ( 0.5774900079438590739, 12.64701867748817143, -5.440088680355550821 ) ) ;
#35774 = CARTESIAN_POINT ( 'NONE',  ( 22.26659068614895176, 39.72041550158063217, -7.082119434687042414 ) ) ;
#35775 = CARTESIAN_POINT ( 'NONE',  ( 7.084665262690076126, 62.02201867748816966, -10.88017736071110164 ) ) ;
#35776 = CARTESIAN_POINT ( 'NONE',  ( 8.439016546559898302, 4.734672723634894724E-16, -11.79122553964973541 ) ) ;
#35777 = CARTESIAN_POINT ( 'NONE',  ( 20.24186590665277308, 40.59014588040356131, -6.114288769123051637 ) ) ;
#35778 = CARTESIAN_POINT ( 'NONE',  ( 12.63842701281683922, 24.55059781766745175, -9.846743663894590881 ) ) ;
#35779 =( NAMED_UNIT ( * ) PLANE_ANGLE_UNIT ( ) SI_UNIT ( $, .RADIAN. ) );
#35780 = CARTESIAN_POINT ( 'NONE',  ( 18.52753015748617571, 8.092264484334117824, 4.923371831947298993 ) ) ;
#35781 = CARTESIAN_POINT ( 'NONE',  ( -11.94665733272784003, 14.76984983275088936, 8.972157519073542531 ) ) ;
#35782 = CARTESIAN_POINT ( 'NONE',  ( 2.791683348922240793, 36.63393115100078035, 7.208316651077764092 ) ) ;
#35783 = CARTESIAN_POINT ( 'NONE',  ( 5.076628168052703671, 61.84226448433412315, 8.527530157486179263 ) ) ;
#35784 = CARTESIAN_POINT ( 'NONE',  ( 2.035157376598822676, 32.43868534415483396, -7.964842623401177768 ) ) ;
#35785 = EDGE_CURVE ( 'NONE', #68711, #14972, #88733, .T. ) ;
#35786 = ORIENTED_EDGE ( 'NONE', *, *, #44034, .F. ) ;
#35787 = CARTESIAN_POINT ( 'NONE',  ( 16.40814093676323893, 50.79030133659708923, 11.09922568453595026 ) ) ;
#35788 = SURFACE_SIDE_STYLE ('',( #97304 ) ) ;
#35789 = CIRCLE ( 'NONE', #16672, 1.249999999999987121 ) ;
#35790 = CARTESIAN_POINT ( 'NONE',  ( 7.361572987183169658, -0.03273551566588185635, -9.846743663894592657 ) ) ;
#35791 = CARTESIAN_POINT ( 'NONE',  ( 6.565887622018943937, 45.16530133659708923, 12.81628187352647430 ) ) ;
#35793 = CARTESIAN_POINT ( 'NONE',  ( 10.00000000000000000, 39.75893115100078745, -9.846743663894594434 ) ) ;
#35792 = CARTESIAN_POINT ( 'NONE',  ( 24.16423886937410614, 54.30374883491396787, 8.672049930838204340E-16 ) ) ;
#35794 = LINE ( 'NONE', #96817, #21496 ) ;
#35795 = ADVANCED_FACE ( 'NONE', ( #40607 ), #77524, .T. ) ;
#35796 = CARTESIAN_POINT ( 'NONE',  ( 18.52753015748618282, 58.92559781766745886, -4.923371831947291888 ) ) ;
#35797 = CARTESIAN_POINT ( 'NONE',  ( 24.16423886937409904, 19.09541550158063927, 3.795296366450317205 ) ) ;
#35798 = CARTESIAN_POINT ( 'NONE',  ( -4.164238869374098151, 46.59541550158063927, -3.795296366450310543 ) ) ;
#35799 = CARTESIAN_POINT ( 'NONE',  ( 14.92337183194729988, 39.34226448433412315, -8.527530157486177487 ) ) ;
#35800 = CARTESIAN_POINT ( 'NONE',  ( -14.94699059465103375, 0.3640475087720990710, 1.259949270174711700 ) ) ;
#35801 = CARTESIAN_POINT ( 'NONE',  ( -0.8801773607111008646, 38.27201867748816255, 2.915334737309923430 ) ) ;
#35802 = AXIS2_PLACEMENT_3D ( 'NONE', #33158, #3177, #24700 ) ;
#35803 = CARTESIAN_POINT ( 'NONE',  ( 2.035157376598824452, 53.68868534415484817, 7.964842623401179544 ) ) ;
#35804 = CARTESIAN_POINT ( 'NONE',  ( 2.603489959281588995, 55.43575266056826933, -6.500000000000003553 ) ) ;
#35805 = ORIENTED_EDGE ( 'NONE', *, *, #98641, .F. ) ;
#35806 = CARTESIAN_POINT ( 'NONE',  ( 6.565887622018943937, 43.08196800326374643, -12.81628187352647608 ) ) ;
#35807 = ORIENTED_EDGE ( 'NONE', *, *, #15810, .T. ) ;
#35808 = CARTESIAN_POINT ( 'NONE',  ( 17.96484262340118221, 66.18868534415483396, -7.964842623401177768 ) ) ;
#35809 = VERTEX_POINT ( 'NONE', #2631 ) ;
#35810 = CARTESIAN_POINT ( 'NONE',  ( -2.266590686148945544, 2.220415501580634388, 7.082119434687048631 ) ) ;
#35811 = CARTESIAN_POINT ( 'NONE',  ( 5.076628168052703671, 11.84226448433411960, 8.527530157486179263 ) ) ;
#35812 = CARTESIAN_POINT ( 'NONE',  ( -1.926860441876564023, 59.68830936912751639, 1.004413902775740781E-15 ) ) ;
#35813 = ORIENTED_EDGE ( 'NONE', *, *, #6089, .F. ) ;
#35814 = CARTESIAN_POINT ( 'NONE',  ( -0.1503990784575407469, 12.22266099184918531, -6.262539305110056631 ) ) ;
#35815 = CARTESIAN_POINT ( 'NONE',  ( 20.88017736071110875, 15.77201867748817143, -2.915334737309920765 ) ) ;
#35816 = LINE ( 'NONE', #66302, #6852 ) ;
#35817 = ADVANCED_FACE ( 'NONE', ( #63580 ), #45632, .T. ) ;
#35818 = CARTESIAN_POINT ( 'NONE',  ( -4.164238869374098151, 16.59541550158063927, -3.795296366450310543 ) ) ;
#35819 = CARTESIAN_POINT ( 'NONE',  ( 2.035157376598822676, 27.43868534415483396, -7.964842623401177768 ) ) ;
#35820 = CARTESIAN_POINT ( 'NONE',  ( 19.84674366389459621, 53.50893115100078745, 7.409399052514197653E-17 ) ) ;
#35821 = VERTEX_POINT ( 'NONE', #32595 ) ;
#35822 = EDGE_CURVE ( 'NONE', #84126, #47538, #70117, .T. ) ;
#35823 = CARTESIAN_POINT ( 'NONE',  ( 14.92337183194729633, 62.67559781766745886, 8.527530157486181039 ) ) ;
#35824 = ORIENTED_EDGE ( 'NONE', *, *, #11758, .F. ) ;
#35825 =( BOUNDED_CURVE ( )  B_SPLINE_CURVE ( 2, ( #74897, #35417, #73911, #58404, #50421, #51910, #20429, #43897, #59396 ),
 .UNSPECIFIED., .F., .F. ) 
 B_SPLINE_CURVE_WITH_KNOTS ( ( 3, 2, 2, 2, 3 ),
 ( 0.5096570216176964374, 0.5119047619047618625, 0.5178571428571429047, 0.5238095238095238360, 0.5260572640965892610 ),
 .UNSPECIFIED. ) 
 CURVE ( )  GEOMETRIC_REPRESENTATION_ITEM ( )  RATIONAL_B_SPLINE_CURVE ( ( 0.9839835555609424134, 0.9871328979762474809, 1.000000000000000000, 0.9659258262890683122, 1.000000000000000000, 0.9659258262890683122, 1.000000000000000000, 0.9871328979762474809, 0.9839835555609424134 ) ) 
 REPRESENTATION_ITEM ( '' )  );
#35826 = CARTESIAN_POINT ( 'NONE',  ( 15.44008868035555793, 66.39701867748817676, -9.422509992056140149 ) ) ;
#35827 = CARTESIAN_POINT ( 'NONE',  ( 19.84674366389459621, 58.50893115100078745, 7.409399052514197653E-17 ) ) ;
#35829 = CARTESIAN_POINT ( 'NONE',  ( -0.3077640640441539621, 0.000000000000000000, 5.999999999999999112 ) ) ;
#35828 = CARTESIAN_POINT ( 'NONE',  ( 7.084665262690076126, 12.02201867748817143, -10.88017736071110164 ) ) ;
#35830 = CARTESIAN_POINT ( 'NONE',  ( 5.076628168052704559, 0.1755978176674514724, -8.527530157486179263 ) ) ;
#35831 = CARTESIAN_POINT ( 'NONE',  ( 2.035157376598824452, 18.68868534415484106, 7.964842623401179544 ) ) ;
#35832 = AXIS2_PLACEMENT_3D ( 'NONE', #96320, #88305, #12791 ) ;
#35833 = VERTEX_POINT ( 'NONE', #85114 ) ;
#35834 = CARTESIAN_POINT ( 'NONE',  ( -2.816281873526473856, 54.12363466993041783, 9.499525473075851096E-16 ) ) ;
#35835 = CARTESIAN_POINT ( 'NONE',  ( 7.084665262690076126, 37.02201867748817676, -10.88017736071110164 ) ) ;
#35836 = LINE ( 'NONE', #12344, #89797 ) ;
#35837 = CARTESIAN_POINT ( 'NONE',  ( 13.43411237798106583, 42.66530133659707502, -12.81628187352647252 ) ) ;
#35838 = CARTESIAN_POINT ( 'NONE',  ( 20.88017736071110164, 50.35535201082151247, 2.915334737309930979 ) ) ;
#35839 = CARTESIAN_POINT ( 'NONE',  ( 18.52753015748618282, 53.92559781766745175, -4.923371831947291888 ) ) ;
#35840 = ORIENTED_EDGE ( 'NONE', *, *, #42103, .F. ) ;
#35841 = ORIENTED_EDGE ( 'NONE', *, *, #7702, .T. ) ;
#35842 = CARTESIAN_POINT ( 'NONE',  ( 17.20831665107776587, 22.88393115100078745, 7.208316651077764980 ) ) ;
#35843 = CARTESIAN_POINT ( 'NONE',  ( 6.565887622018943937, 0.1653013365970866511, 12.81628187352647430 ) ) ;
#35845 = CARTESIAN_POINT ( 'NONE',  ( 1.472469842513823179, 66.42559781766745175, 4.923371831947296329 ) ) ;
#35844 = CARTESIAN_POINT ( 'NONE',  ( 10.64017930668198453, 0.5000000000000004441, 10.57291749337222875 ) ) ;
#35846 = CARTESIAN_POINT ( 'NONE',  ( -0.8801773607110991993, 17.85535201082150536, -2.915334737309923874 ) ) ;
#35847 = CARTESIAN_POINT ( 'NONE',  ( 19.84674366389459266, 48.30059781766745175, 2.638427012816836559 ) ) ;
#35848 = PLANE ( 'NONE',  #53877 ) ;
#35849 = CARTESIAN_POINT ( 'NONE',  ( 10.00000000000000000, -0.2410688489992152128, -9.846743663894594434 ) ) ;
#35851 = VERTEX_POINT ( 'NONE', #55092 ) ;
#35850 = CARTESIAN_POINT ( 'NONE',  ( 22.81628187352647785, 6.623634669930420493, 6.195893100308588602E-16 ) ) ;
#35852 = CARTESIAN_POINT ( 'NONE',  ( 0.9413316022086133383, 63.45508385108958294, 6.499999999999978684 ) ) ;
#35853 = CARTESIAN_POINT ( 'NONE',  ( 0.6178305044545818747, 33.49863466993042493, -9.382169495545419124 ) ) ;
#35854 = CARTESIAN_POINT ( 'NONE',  ( 10.00000000000000000, 29.75893115100078745, -9.846743663894594434 ) ) ;
#35855 = CARTESIAN_POINT ( 'NONE',  ( 11.25000000000000000, 7.826366962315981723, -3.014428414850133908 ) ) ;
#35856 = CARTESIAN_POINT ( 'NONE',  ( 6.204703633549690345, 52.84541550158062506, 14.16423886937410082 ) ) ;
#35857 = CARTESIAN_POINT ( 'NONE',  ( 19.84674366389459266, 28.71726448433411960, -2.638427012816827677 ) ) ;
#35858 = COLOUR_RGB ( '', 0.66274510, 0.83137255, 0.94901961) ;
#35859 = CARTESIAN_POINT ( 'NONE',  ( 19.39188664607695856, 65.83703382326400799, -6.499999999999937828 ) ) ;
#35860 = VECTOR ( 'NONE', #21511, 1000.000000000000000 ) ;
#35861 = CARTESIAN_POINT ( 'NONE',  ( 10.00000000000000000, 55.55374883491396787, -14.16423886937410082 ) ) ;
#35862 = CARTESIAN_POINT ( 'NONE',  ( -6.430724159521292727, -88.51069574204372259, 3.750000000000000000 ) ) ;
#35863 = CARTESIAN_POINT ( 'NONE',  ( 17.96484262340118221, 26.18868534415483396, -7.964842623401177768 ) ) ;
#35864 = CARTESIAN_POINT ( 'NONE',  ( 13.79529636645031943, 30.34541550158063927, -14.16423886937409904 ) ) ;
#35866 = CARTESIAN_POINT ( 'NONE',  ( -10.70613742633264565, 4.864377723017530212E-16, 9.778988772285165609 ) ) ;
#35865 = CARTESIAN_POINT ( 'NONE',  ( 6.204703633549690345, 47.84541550158064638, 14.16423886937410082 ) ) ;
#35867 = CARTESIAN_POINT ( 'NONE',  ( 0.000000000000000000, 0.5000000000000004441, 0.000000000000000000 ) ) ;
#35868 = CARTESIAN_POINT ( 'NONE',  ( 14.92337183194729988, 9.342264484334119601, -8.527530157486177487 ) ) ;
#35869 = CARTESIAN_POINT ( 'NONE',  ( 10.00000000000000178, 67.25893115100079456, 9.846743663894594434 ) ) ;
#35870 = CARTESIAN_POINT ( 'NONE',  ( 18.17829156368507171, 14.16792564121896270, 6.500000000000019540 ) ) ;
#35871 = CARTESIAN_POINT ( 'NONE',  ( 15.44008868035555793, 56.39701867748817676, -9.422509992056140149 ) ) ;
#35872 = CARTESIAN_POINT ( 'NONE',  ( 2.791683348922237240, 60.38393115100078745, -7.208316651077763204 ) ) ;
#35873 = CARTESIAN_POINT ( 'NONE',  ( 10.32896413005679825, 2.604976035794182021, -5.963430220938286119 ) ) ;
#35874 = DIRECTION ( 'NONE',  ( 0.000000000000000000, 1.000000000000000000, 0.000000000000000000 ) ) ;
#35875 = CARTESIAN_POINT ( 'NONE',  ( -13.77612262535527954, 90.93158326518027934, 7.883772450803742338 ) ) ;
#35876 = VECTOR ( 'NONE', #89261, 1000.000000000000000 ) ;
#35877 = CARTESIAN_POINT ( 'NONE',  ( 10.00000000000000178, 43.05374883491397497, 14.16423886937410082 ) ) ;
#35879 = CARTESIAN_POINT ( 'NONE',  ( 2.962741594152983993, 15.00000000000000000, 13.93860331045674883 ) ) ;
#35878 = CARTESIAN_POINT ( 'NONE',  ( 6.829574850505127692, -88.00372650098204019, -3.749999999999998668 ) ) ;
#35880 = CARTESIAN_POINT ( 'NONE',  ( 12.91533473730993009, 16.60535201082150891, -10.88017736071109987 ) ) ;
#35881 = CARTESIAN_POINT ( 'NONE',  ( 10.00000000000000000, 42.87363466993042493, -12.81628187352647608 ) ) ;
#35882 = PRESENTATION_STYLE_ASSIGNMENT (( #36883 ) ) ;
#35883 = CARTESIAN_POINT ( 'NONE',  ( -2.816281873526471635, 38.91530133659708213, -3.434112377981056508 ) ) ;
#35884 = CARTESIAN_POINT ( 'NONE',  ( 16.40814093676323893, 60.79030133659709634, 11.09922568453595026 ) ) ;
#35885 = ORIENTED_EDGE ( 'NONE', *, *, #62162, .F. ) ;
#35886 = DIRECTION ( 'NONE',  ( -1.000000000000000000, -2.569960705150834273E-16, 0.000000000000000000 ) ) ;
#35887 = CARTESIAN_POINT ( 'NONE',  ( 1.915564264621337554, 4.132324795315745510E-16, 14.37291249357991774 ) ) ;
#35888 = CARTESIAN_POINT ( 'NONE',  ( -4.164238869374099039, 26.80374883491397142, 8.674139862899312516E-16 ) ) ;
#35889 = CARTESIAN_POINT ( 'NONE',  ( -4.164238869374099927, 7.012082168247302683, 3.795296366450308767 ) ) ;
#35890 = CARTESIAN_POINT ( 'NONE',  ( 5.800000000000003375, 99.99999999999998579, -8.000000000000000000 ) ) ;
#35891 = CARTESIAN_POINT ( 'NONE',  ( 4.559911319644449179, 17.23035201082150536, -9.422509992056141925 ) ) ;
#35892 = CARTESIAN_POINT ( 'NONE',  ( -22.17076923076924189, 84.15384615384614619, -9.500000000000000000 ) ) ;
#35893 = DIRECTION ( 'NONE',  ( 1.000000000000000000, 1.257402221000611116E-16, -0.000000000000000000 ) ) ;
#35894 = CARTESIAN_POINT ( 'NONE',  ( -0.8801773607110991993, 52.85535201082151247, -2.915334737309923874 ) ) ;
#35895 = CARTESIAN_POINT ( 'NONE',  ( 17.96484262340118221, 51.18868534415483396, -7.964842623401177768 ) ) ;
#35896 = CARTESIAN_POINT ( 'NONE',  ( 0.6178305044545838731, 9.748634669930416052, 9.382169495545420901 ) ) ;
#35897 = DIRECTION ( 'NONE',  ( 0.000000000000000000, 0.000000000000000000, -1.000000000000000000 ) ) ;
#35898 = CARTESIAN_POINT ( 'NONE',  ( 7.361572987183169658, 29.96726448433411960, -9.846743663894592657 ) ) ;
#35899 = ADVANCED_FACE ( 'NONE', ( #16623 ), #74309, .T. ) ;
#35900 = CARTESIAN_POINT ( 'NONE',  ( 18.61655166652076687, 49.87718327197428891, 6.499999999999981348 ) ) ;
#35901 = CIRCLE ( 'NONE', #16787, 0.5000000000000004441 ) ;
#35902 = CARTESIAN_POINT ( 'NONE',  ( 4.559911319644449179, 37.23035201082150536, -9.422509992056141925 ) ) ;
#35903 = EDGE_CURVE ( 'NONE', #71629, #2953, #39921, .T. ) ;
#35904 = CARTESIAN_POINT ( 'NONE',  ( 10.00000000000000178, 10.37363466993041961, 12.81628187352647608 ) ) ;
#35905 = LINE ( 'NONE', #82388, #96928 ) ;
#35906 = ADVANCED_FACE ( 'NONE', ( #27058 ), #65543, .T. ) ;
#35907 = CARTESIAN_POINT ( 'NONE',  ( 18.52753015748618282, 28.92559781766745175, -4.923371831947291888 ) ) ;
#35908 = CARTESIAN_POINT ( 'NONE',  ( 3.591859063236761518, 54.95696800326376064, 11.09922568453594849 ) ) ;
#35909 = CARTESIAN_POINT ( 'NONE',  ( 1.472469842513823179, 11.42559781766745175, 4.923371831947296329 ) ) ;
#35910 = EDGE_LOOP ( 'NONE', ( #86322, #11613, #38731, #49990 ) ) ;
#35911 = FACE_OUTER_BOUND ( 'NONE', #8157, .T. ) ;
#35912 = LINE ( 'NONE', #19442, #52589 ) ;
#35913 = CARTESIAN_POINT ( 'NONE',  ( 7.084665262690076126, 14.10535201082150358, 10.88017736071109987 ) ) ;
#35914 = CARTESIAN_POINT ( 'NONE',  ( -0.9940297508538862292, -0.03417435944610275333, 14.21528771620248932 ) ) ;
#35915 = CARTESIAN_POINT ( 'NONE',  ( 1.472469842513823179, 26.42559781766745175, 4.923371831947296329 ) ) ;
#35916 = CARTESIAN_POINT ( 'NONE',  ( 20.88017736071110164, 20.35535201082150891, 2.915334737309930979 ) ) ;
#35917 = CARTESIAN_POINT ( 'NONE',  ( 7.084665262690076126, 4.105352010821503583, 10.88017736071109987 ) ) ;
#35918 = ORIENTED_EDGE ( 'NONE', *, *, #15312, .T. ) ;
#35919 = AXIS2_PLACEMENT_3D ( 'NONE', #17467, #77447, #8960 ) ;
#35920 = CARTESIAN_POINT ( 'NONE',  ( 12.91533473730993009, 26.60535201082150536, -10.88017736071109987 ) ) ;
#35921 = CARTESIAN_POINT ( 'NONE',  ( 2.035157376598822676, 37.43868534415484106, -7.964842623401177768 ) ) ;
#35923 = CARTESIAN_POINT ( 'NONE',  ( 20.88017736071110875, 40.77201867748818387, -2.915334737309920765 ) ) ;
#35922 = CARTESIAN_POINT ( 'NONE',  ( 0.000000000000000000, 14.49999999999999822, 0.000000000000000000 ) ) ;
#35924 = ORIENTED_EDGE ( 'NONE', *, *, #25883, .T. ) ;
#35925 = CARTESIAN_POINT ( 'NONE',  ( 18.52753015748618282, 53.92559781766745175, -4.923371831947291888 ) ) ;
#35926 = CARTESIAN_POINT ( 'NONE',  ( 2.035157376598822676, 32.43868534415483396, -7.964842623401177768 ) ) ;
#35927 = PLANE ( 'NONE',  #16266 ) ;
#35928 = CARTESIAN_POINT ( 'NONE',  ( -15.00000000000004974, 91.00000000000000000, -7.750000000000000000 ) ) ;
#35929 = CARTESIAN_POINT ( 'NONE',  ( -7.750000000000000000, 43.00000000000000000, 6.500000000000000888 ) ) ;
#35930 = CARTESIAN_POINT ( 'NONE',  ( -19.00000000000000000, 75.76920769491739804, 3.000000000000000000 ) ) ;
#35931 = CARTESIAN_POINT ( 'NONE',  ( -0.3689425029237881626, 27.42874883491397142, 10.36894250292379027 ) ) ;
#35932 = CARTESIAN_POINT ( 'NONE',  ( 15.44008868035555793, 51.39701867748816966, -9.422509992056140149 ) ) ;
#35933 = CARTESIAN_POINT ( 'NONE',  ( 17.85158348494335812, 49.73726573380442773, -6.500000000000001776 ) ) ;
#35934 = AXIS2_PLACEMENT_3D ( 'NONE', #58838, #81831, #36845 ) ;
#35935 = CARTESIAN_POINT ( 'NONE',  ( -11.02682316214847980, -96.56463058013387979, -3.750000000000000000 ) ) ;
#35936 = CARTESIAN_POINT ( 'NONE',  ( 10.00000000000000000, 49.75893115100078745, -9.846743663894594434 ) ) ;
#35937 = ORIENTED_EDGE ( 'NONE', *, *, #51230, .F. ) ;
#35938 = EDGE_CURVE ( 'NONE', #48953, #57022, #6627, .T. ) ;
#35939 = CARTESIAN_POINT ( 'NONE',  ( 12.63842701281683922, 19.55059781766745175, -9.846743663894590881 ) ) ;
#35940 = CARTESIAN_POINT ( 'NONE',  ( -6.408140936763232709, -20.04303199673624292, 11.09922568453595026 ) ) ;
#35941 = CARTESIAN_POINT ( 'NONE',  ( 20.88017736071110875, 30.77201867748816966, -2.915334737309920765 ) ) ;
#35942 = CARTESIAN_POINT ( 'NONE',  ( 19.84674366389459266, 23.71726448433412315, -2.638427012816827677 ) ) ;
#35943 = CARTESIAN_POINT ( 'NONE',  ( -2.816281873526471635, 8.915301336597083903, -3.434112377981056508 ) ) ;
#35944 = CARTESIAN_POINT ( 'NONE',  ( 2.035157376598822676, 57.43868534415484106, -7.964842623401177768 ) ) ;
#35946 = CARTESIAN_POINT ( 'NONE',  ( 0.6178305044545818747, 58.49863466993042493, -9.382169495545419124 ) ) ;
#35945 = CARTESIAN_POINT ( 'NONE',  ( 15.44008868035555793, 36.39701867748816966, -9.422509992056140149 ) ) ;
#35947 = CARTESIAN_POINT ( 'NONE',  ( 24.16423886937409904, 39.09541550158062506, 3.795296366450317205 ) ) ;
#35948 = ADVANCED_FACE ( 'NONE', ( #88055 ), #64736, .T. ) ;
#35949 = AXIS2_PLACEMENT_3D ( 'NONE', #75738, #82746, #75244 ) ;
#35950 = FACE_OUTER_BOUND ( 'NONE', #68781, .T. ) ;
#35951 = VERTEX_POINT ( 'NONE', #61009 ) ;
#35952 = CARTESIAN_POINT ( 'NONE',  ( 19.38216949554541557, 2.248634669930420049, -9.382169495545420901 ) ) ;
#35953 = CARTESIAN_POINT ( 'NONE',  ( 12.91533473730993009, 41.60535201082149825, -10.88017736071109987 ) ) ;
#35954 = CARTESIAN_POINT ( 'NONE',  ( 1.472469842513823179, 65.59226448433412315, -4.923371831947296329 ) ) ;
#35955 = ORIENTED_EDGE ( 'NONE', *, *, #8756, .F. ) ;
#35956 = CARTESIAN_POINT ( 'NONE',  ( 0.1532563361054082862, 21.21726448433412315, 2.638427012816831674 ) ) ;
#35957 = CARTESIAN_POINT ( 'NONE',  ( 0.5774900079438607392, 63.48035201082149825, 5.440088680355550821 ) ) ;
#35958 = B_SPLINE_CURVE_WITH_KNOTS ( 'NONE', 3,
 ( #86036, #4019, #34481, #64975, #95500, #26991 ),
 .UNSPECIFIED., .F., .F.,
 ( 4, 2, 4 ),
 ( 3.409110551490396616E-05, 0.0004400426677367293800, 0.0008459942299585547802 ),
 .UNSPECIFIED. ) ;
#35959 = CARTESIAN_POINT ( 'NONE',  ( 0.1532563361054100626, 30.80059781766744820, -2.638427012816831230 ) ) ;
#35960 = CARTESIAN_POINT ( 'NONE',  ( 0.1532563361054100626, 30.80059781766744820, -2.638427012816831230 ) ) ;
#35961 = CARTESIAN_POINT ( 'NONE',  ( 12.63842701281683922, 19.55059781766745175, -9.846743663894590881 ) ) ;
#35962 = VECTOR ( 'NONE', #46327, 1000.000000000000000 ) ;
#35963 = LINE ( 'NONE', #37465, #72364 ) ;
#35965 = LINE ( 'NONE', #88976, #27951 ) ;
#35964 = CARTESIAN_POINT ( 'NONE',  ( 20.88017736071110875, 65.77201867748817676, -2.915334737309920765 ) ) ;
#35966 = CARTESIAN_POINT ( 'NONE',  ( 0.1532563361054082862, 11.21726448433411605, 2.638427012816831674 ) ) ;
#35968 = ORIENTED_EDGE ( 'NONE', *, *, #53164, .F. ) ;
#35967 = CARTESIAN_POINT ( 'NONE',  ( 14.92337183194729988, 39.34226448433412315, -8.527530157486177487 ) ) ;
#35969 = CARTESIAN_POINT ( 'NONE',  ( 4.691427381388423079, -2.693150427207441133, 4.000000000000000888 ) ) ;
#35970 = CARTESIAN_POINT ( 'NONE',  ( 17.20831665107776587, 62.88393115100078745, 7.208316651077764980 ) ) ;
#35971 = VECTOR ( 'NONE', #94179, 1000.000000000000000 ) ;
#35972 = CARTESIAN_POINT ( 'NONE',  ( 10.00000000000000000, 1.813685344154837731, -10.88017736071110342 ) ) ;
#35973 = CARTESIAN_POINT ( 'NONE',  ( 6.204703633549690345, 22.84541550158062861, 14.16423886937410082 ) ) ;
#35974 = DIRECTION ( 'NONE',  ( 0.000000000000000000, 0.000000000000000000, 1.000000000000000000 ) ) ;
#35975 = CARTESIAN_POINT ( 'NONE',  ( -0.3689425029237881626, 22.42874883491397142, 10.36894250292379027 ) ) ;
#35976 = CARTESIAN_POINT ( 'NONE',  ( -0.3689425029237898834, 51.17874883491397497, -10.36894250292378850 ) ) ;
#35977 = EDGE_CURVE ( 'NONE', #28751, #325, #68530, .T. ) ;
#35978 = CARTESIAN_POINT ( 'NONE',  ( 2.917880565312950480, 0.9704155015806342766, -12.26659068614894821 ) ) ;
#35979 = CARTESIAN_POINT ( 'NONE',  ( -4.164238869374098151, 11.59541550158063217, -3.795296366450310543 ) ) ;
#35980 = CARTESIAN_POINT ( 'NONE',  ( 10.00000000000000000, 41.81368534415484106, -10.88017736071110342 ) ) ;
#35981 = CARTESIAN_POINT ( 'NONE',  ( -11.62719953690074881, 14.49999999999999112, 9.476720473301769587 ) ) ;
#35982 = AXIS2_PLACEMENT_3D ( 'NONE', #57003, #58476, #80506 ) ;
#35983 = VERTEX_POINT ( 'NONE', #98561 ) ;
#35984 = CARTESIAN_POINT ( 'NONE',  ( 10.00000000000000000, 24.75893115100078745, -9.846743663894594434 ) ) ;
#35986 = CARTESIAN_POINT ( 'NONE',  ( 14.92337183194729988, 34.34226448433411605, -8.527530157486177487 ) ) ;
#35985 = CARTESIAN_POINT ( 'NONE',  ( 10.00000000000000000, 66.81368534415484817, -10.88017736071110342 ) ) ;
#35987 = ORIENTED_EDGE ( 'NONE', *, *, #5720, .F. ) ;
#35988 = CARTESIAN_POINT ( 'NONE',  ( 10.00000000000000000, 11.81368534415483751, -10.88017736071110342 ) ) ;
#35989 = CARTESIAN_POINT ( 'NONE',  ( 22.81628187352648496, 56.83196800326374643, -3.434112377981050290 ) ) ;
#35990 = CARTESIAN_POINT ( 'NONE',  ( 2.791683348922237240, 45.38393115100079456, -7.208316651077763204 ) ) ;
#35991 = EDGE_CURVE ( 'NONE', #82266, #17685, #95087, .T. ) ;
#35992 = DIRECTION ( 'NONE',  ( 0.000000000000000000, 0.000000000000000000, 1.000000000000000000 ) ) ;
#35993 = CARTESIAN_POINT ( 'NONE',  ( 21.09922568453594849, 46.20696800326376064, 6.408140936763242479 ) ) ;
#35995 = CIRCLE ( 'NONE', #91891, 14.49999999999999822 ) ;
#35994 = CARTESIAN_POINT ( 'NONE',  ( 7.082119434687047743, -24.86291783175269288, -12.26659068614894821 ) ) ;
#35996 = CARTESIAN_POINT ( 'NONE',  ( 4.559911319644449179, 48.89701867748817676, 9.422509992056141925 ) ) ;
#35997 = CARTESIAN_POINT ( 'NONE',  ( 5.076628168052704559, 35.17559781766745175, -8.527530157486179263 ) ) ;
#35998 = CARTESIAN_POINT ( 'NONE',  ( -0.3689425029237898834, 21.17874883491396432, -10.36894250292378850 ) ) ;
#35999 = ORIENTED_EDGE ( 'NONE', *, *, #76445, .T. ) ;
#36000 = CARTESIAN_POINT ( 'NONE',  ( -0.3689425029237898834, 6.178748834913968757, -10.36894250292378850 ) ) ;
#36001 = AXIS2_PLACEMENT_3D ( 'NONE', #97043, #59505, #7009 ) ;
#36002 = CARTESIAN_POINT ( 'NONE',  ( 12.91533473730993009, 56.60535201082151247, -10.88017736071109987 ) ) ;
#36003 = DIRECTION ( 'NONE',  ( 0.000000000000000000, 0.000000000000000000, -1.000000000000000000 ) ) ;
#36004 = CARTESIAN_POINT ( 'NONE',  ( 20.36894250292379738, 44.92874883491396787, -10.36894250292379027 ) ) ;
#36005 = CARTESIAN_POINT ( 'NONE',  ( 19.38216949554541202, 0.9986346699304200492, 9.382169495545424454 ) ) ;
#36006 = FACE_OUTER_BOUND ( 'NONE', #62462, .T. ) ;
#36007 = CARTESIAN_POINT ( 'NONE',  ( 20.88017736071110519, 50.56368534415484106, 2.639326808657452039E-16 ) ) ;
#36008 = CARTESIAN_POINT ( 'NONE',  ( 0.000000000000000000, 14.49999999999999822, 0.000000000000000000 ) ) ;
#36009 = CARTESIAN_POINT ( 'NONE',  ( 10.00000000000000000, 22.87363466993042138, -12.81628187352647608 ) ) ;
#36010 = CARTESIAN_POINT ( 'NONE',  ( 22.81628187352648496, 1.831968003263753753, -3.434112377981050290 ) ) ;
#36011 = CARTESIAN_POINT ( 'NONE',  ( -2.915334737309934532, 27.02201867748817321, -10.88017736071109987 ) ) ;
#36012 = CARTESIAN_POINT ( 'NONE',  ( -0.8801773607111008646, 18.27201867748817321, 2.915334737309923430 ) ) ;
#36013 = CARTESIAN_POINT ( 'NONE',  ( 12.91533473730993009, 6.605352010821504471, -10.88017736071109987 ) ) ;
#36014 = FACE_OUTER_BOUND ( 'NONE', #71366, .T. ) ;
#36015 = VERTEX_POINT ( 'NONE', #53509 ) ;
#36016 = FILL_AREA_STYLE ('',( #96541 ) ) ;
#36017 = CARTESIAN_POINT ( 'NONE',  ( 14.92337183194729633, 2.675597817667451750, 8.527530157486181039 ) ) ;
#36018 = EDGE_CURVE ( 'NONE', #35833, #47206, #84020, .T. ) ;
#36019 = VECTOR ( 'NONE', #50136, 1000.000000000000000 ) ;
#36020 = CARTESIAN_POINT ( 'NONE',  ( 10.00000000000000000, 39.75893115100078745, -9.846743663894594434 ) ) ;
#36021 = CARTESIAN_POINT ( 'NONE',  ( 0.5774900079438590739, 37.64701867748817676, -5.440088680355550821 ) ) ;
#36022 = EDGE_CURVE ( 'NONE', #37077, #29308, #83897, .T. ) ;
#36023 = CARTESIAN_POINT ( 'NONE',  ( 19.38216949554541557, 7.248634669930421381, -9.382169495545420901 ) ) ;
#36025 = CARTESIAN_POINT ( 'NONE',  ( 0.000000000000000000, 15.00000000000000000, 0.000000000000000000 ) ) ;
#36024 = CARTESIAN_POINT ( 'NONE',  ( -0.8801773607110991993, 37.85535201082151247, -2.915334737309923874 ) ) ;
#36026 = CYLINDRICAL_SURFACE ( 'NONE', #36955, 1.249999999999987121 ) ;
#36027 = CARTESIAN_POINT ( 'NONE',  ( 0.6178305044545818747, 43.49863466993042493, -9.382169495545419124 ) ) ;
#36028 = EDGE_LOOP ( 'NONE', ( #22415, #81915, #44588, #90617, #8198, #13532 ) ) ;
#36029 = CARTESIAN_POINT ( 'NONE',  ( 12.91533473730993009, 66.60535201082150536, -10.88017736071109987 ) ) ;
#36031 = CARTESIAN_POINT ( 'NONE',  ( 6.204703633549690345, 7.845415501580634832, 14.16423886937410082 ) ) ;
#36030 = CARTESIAN_POINT ( 'NONE',  ( 22.81628187352647785, 36.62363466993041783, 6.195893100308588602E-16 ) ) ;
#36032 = CARTESIAN_POINT ( 'NONE',  ( 7.084665262690076126, 42.02201867748816966, -10.88017736071110164 ) ) ;
#36033 = CARTESIAN_POINT ( 'NONE',  ( 0.1143410931637255656, 15.21691075486302580, 6.480892540919855449 ) ) ;
#36034 = CARTESIAN_POINT ( 'NONE',  ( 20.36894250292379738, 64.92874883491397497, -10.36894250292379027 ) ) ;
#36035 = CARTESIAN_POINT ( 'NONE',  ( 12.63842701281683034, 52.46726448433413026, 9.846743663894596210 ) ) ;
#36036 = CARTESIAN_POINT ( 'NONE',  ( 12.63842701281683034, 17.46726448433411250, 9.846743663894596210 ) ) ;
#36037 = CARTESIAN_POINT ( 'NONE',  ( -0.8801773607111008646, 68.27201867748817676, 2.915334737309923430 ) ) ;
#36038 = CARTESIAN_POINT ( 'NONE',  ( 17.75000000000000000, 84.07179676972448590, -12.00000000000000000 ) ) ;
#36039 = CARTESIAN_POINT ( 'NONE',  ( -4.164238869374099927, 32.01208216824730357, 3.795296366450308767 ) ) ;
#36040 = CARTESIAN_POINT ( 'NONE',  ( 0.000000000000000000, 35.00000000000000000, -11.92686044187656513 ) ) ;
#36041 = PRESENTATION_STYLE_ASSIGNMENT (( #81050 ) ) ;
#36042 = CARTESIAN_POINT ( 'NONE',  ( 13.61912076658548365, 6.962610826430346815E-16, -5.334594295380906459 ) ) ;
#36043 = ORIENTED_EDGE ( 'NONE', *, *, #85196, .F. ) ;
#36044 = ORIENTED_EDGE ( 'NONE', *, *, #46962, .T. ) ;
#36045 = CARTESIAN_POINT ( 'NONE',  ( 24.16423886937409904, 59.09541550158063217, 3.795296366450317205 ) ) ;
#36046 = CARTESIAN_POINT ( 'NONE',  ( -0.8801773607111008646, 3.272018677488171434, 2.915334737309923430 ) ) ;
#36047 = CARTESIAN_POINT ( 'NONE',  ( 19.84674366389459266, 23.71726448433412315, -2.638427012816827677 ) ) ;
#36049 = CARTESIAN_POINT ( 'NONE',  ( 3.591859063236761518, 29.95696800326375708, 11.09922568453594849 ) ) ;
#36048 = AXIS2_PLACEMENT_3D ( 'NONE', #1884, #85355, #70366 ) ;
#36050 = DIRECTION ( 'NONE',  ( 0.9961946980917462113, -0.08715574274765114371, -0.000000000000000000 ) ) ;
#36051 = LINE ( 'NONE', #36558, #49852 ) ;
#36052 = CARTESIAN_POINT ( 'NONE',  ( 0.5774900079438590739, 17.64701867748817321, -5.440088680355550821 ) ) ;
#36053 = CARTESIAN_POINT ( 'NONE',  ( 20.36894250292379382, 53.67874883491397497, 10.36894250292379205 ) ) ;
#36054 = EDGE_CURVE ( 'NONE', #46734, #11368, #8512, .T. ) ;
#36055 = CARTESIAN_POINT ( 'NONE',  ( 19.84674366389459266, 23.71726448433412315, -2.638427012816827677 ) ) ;
#36056 = CARTESIAN_POINT ( 'NONE',  ( 6.599999999999995204, -97.00000000000000000, -3.750000000000000000 ) ) ;
#36057 = CARTESIAN_POINT ( 'NONE',  ( 12.63842701281683034, 12.46726448433411782, 9.846743663894596210 ) ) ;
#36058 = EDGE_CURVE ( 'NONE', #98100, #71776, #70919, .T. ) ;
#36059 = DIRECTION ( 'NONE',  ( 0.4305110968083047940, 0.000000000000000000, -0.9025852843498560762 ) ) ;
#36060 = CARTESIAN_POINT ( 'NONE',  ( -4.923371831947302546, 10.17559781766745530, -8.527530157486173934 ) ) ;
#36061 = ORIENTED_EDGE ( 'NONE', *, *, #30998, .T. ) ;
#36062 = EDGE_LOOP ( 'NONE', ( #93131, #11710, #89600, #18995 ) ) ;
#36063 = DIRECTION ( 'NONE',  ( 0.000000000000000000, 0.000000000000000000, 1.000000000000000000 ) ) ;
#36064 = EDGE_LOOP ( 'NONE', ( #22235, #22759, #17650, #40755 ) ) ;
#36065 = CARTESIAN_POINT ( 'NONE',  ( 1.472469842513823179, 40.59226448433411605, -4.923371831947296329 ) ) ;
#36067 = CARTESIAN_POINT ( 'NONE',  ( 20.88017736071110519, 30.56368534415484106, 2.639326808657452039E-16 ) ) ;
#36066 = CARTESIAN_POINT ( 'NONE',  ( 15.44008868035555793, 16.39701867748817321, -9.422509992056140149 ) ) ;
#36069 = CARTESIAN_POINT ( 'NONE',  ( 19.38216949554541202, 10.99863466993042138, 9.382169495545424454 ) ) ;
#36068 = CARTESIAN_POINT ( 'NONE',  ( 18.52753015748618282, 58.92559781766745886, -4.923371831947291888 ) ) ;
#36070 = CARTESIAN_POINT ( 'NONE',  ( -4.164238869374098151, 11.59541550158063217, -3.795296366450310543 ) ) ;
#36071 = AXIS2_PLACEMENT_3D ( 'NONE', #51805, #27812, #20818 ) ;
#36073 = CARTESIAN_POINT ( 'NONE',  ( 13.43411237798105340, 30.58196800326374998, 12.81628187352647963 ) ) ;
#36072 = VECTOR ( 'NONE', #23696, 1000.000000000000000 ) ;
#36074 = ORIENTED_EDGE ( 'NONE', *, *, #13960, .F. ) ;
#36075 = CARTESIAN_POINT ( 'NONE',  ( 1.472469842513823179, 31.42559781766745530, 4.923371831947296329 ) ) ;
#36076 = CARTESIAN_POINT ( 'NONE',  ( 19.42250999205614193, 5.147018677488171434, 5.440088680355555262 ) ) ;
#36077 = ORIENTED_EDGE ( 'NONE', *, *, #3280, .F. ) ;
#36078 = CARTESIAN_POINT ( 'NONE',  ( 10.00000000000000000, 65.55374883491396076, -14.16423886937410082 ) ) ;
#36079 = ORIENTED_EDGE ( 'NONE', *, *, #35325, .F. ) ;
#36080 = CARTESIAN_POINT ( 'NONE',  ( -0.8801773607111008646, 53.27201867748816966, 2.915334737309923430 ) ) ;
#36081 = CARTESIAN_POINT ( 'NONE',  ( 0.5774900079438590739, 62.64701867748817676, -5.440088680355550821 ) ) ;
#36082 = CARTESIAN_POINT ( 'NONE',  ( 10.00000000000000178, 54.31368534415484106, 10.88017736071110342 ) ) ;
#36083 = CARTESIAN_POINT ( 'NONE',  ( 17.82550663882221542, 78.51652494792099901, -4.000000000000000888 ) ) ;
#36084 = CARTESIAN_POINT ( 'NONE',  ( 10.00000000000000178, 44.31368534415484106, 10.88017736071110342 ) ) ;
#36085 = CARTESIAN_POINT ( 'NONE',  ( 67.06412365047464164, 26.99999999999997868, -9.500000000000000000 ) ) ;
#36086 = CARTESIAN_POINT ( 'NONE',  ( 10.09792486685183199, 14.95037105583725534, 10.75589247084419675 ) ) ;
#36087 = CARTESIAN_POINT ( 'NONE',  ( 18.52753015748617571, 28.09226448433411960, 4.923371831947298993 ) ) ;
#36088 = VERTEX_POINT ( 'NONE', #62977 ) ;
#36089 = CARTESIAN_POINT ( 'NONE',  ( 17.20831665107776587, 52.88393115100078035, 7.208316651077764980 ) ) ;
#36090 = CYLINDRICAL_SURFACE ( 'NONE', #54844, 19.99999999999999645 ) ;
#36091 = CARTESIAN_POINT ( 'NONE',  ( -4.164238869374098151, 11.59541550158063217, -3.795296366450310543 ) ) ;
#36092 = EDGE_LOOP ( 'NONE', ( #16423, #66763, #15571, #26990 ) ) ;
#36093 = CARTESIAN_POINT ( 'NONE',  ( -10.65882794182087778, 13.06867033551286639, 5.232423767642232271 ) ) ;
#36094 = CARTESIAN_POINT ( 'NONE',  ( 18.18329248733322956, 47.60290668512021739, 6.499999999999960920 ) ) ;
#36095 = CARTESIAN_POINT ( 'NONE',  ( 20.36894250292379738, 54.92874883491396076, -10.36894250292379027 ) ) ;
#36096 = FACE_OUTER_BOUND ( 'NONE', #54961, .T. ) ;
#36097 = EDGE_LOOP ( 'NONE', ( #53274, #33118, #228, #42943 ) ) ;
#36098 = CARTESIAN_POINT ( 'NONE',  ( 9.402796353261129170, 14.63595249122791664, -11.68706210897758169 ) ) ;
#36099 = CARTESIAN_POINT ( 'NONE',  ( 2.791683348922240793, 51.63393115100078745, 7.208316651077764092 ) ) ;
#36100 = CARTESIAN_POINT ( 'NONE',  ( -12.98685442714202232, 15.00000000000000000, 6.449155920600843750 ) ) ;
#36101 = AXIS2_PLACEMENT_3D ( 'NONE', #57624, #88122, #12618 ) ;
#36102 = CARTESIAN_POINT ( 'NONE',  ( 6.565887622018943937, 18.08196800326375708, -12.81628187352647608 ) ) ;
#36103 = CARTESIAN_POINT ( 'NONE',  ( 7.361572987183169658, 14.96726448433411960, -9.846743663894592657 ) ) ;
#36104 = EDGE_CURVE ( 'NONE', #53783, #800, #53782, .T. ) ;
#36105 = CARTESIAN_POINT ( 'NONE',  ( 0.6261916924966959286, 0.5000000000000002220, 6.500000000000003553 ) ) ;
#36106 = CARTESIAN_POINT ( 'NONE',  ( 14.92337183194729988, 9.342264484334119601, -8.527530157486177487 ) ) ;
#36107 = CARTESIAN_POINT ( 'NONE',  ( 13.43411237798105340, 0.5819680032637533085, 12.81628187352647963 ) ) ;
#36108 = DIRECTION ( 'NONE',  ( -1.000000000000000000, 0.000000000000000000, 0.000000000000000000 ) ) ;
#36109 = VERTEX_POINT ( 'NONE', #9995 ) ;
#36110 = AXIS2_PLACEMENT_3D ( 'NONE', #21431, #75405, #89917 ) ;
#36111 = CARTESIAN_POINT ( 'NONE',  ( 7.084665262690076126, 9.105352010821503583, 10.88017736071109987 ) ) ;
#36112 = CARTESIAN_POINT ( 'NONE',  ( 2.917880565312948704, 2.637082168247300906, 12.26659068614894643 ) ) ;
#36113 = CARTESIAN_POINT ( 'NONE',  ( 18.52753015748617571, 23.09226448433411960, 4.923371831947298993 ) ) ;
#36114 = CARTESIAN_POINT ( 'NONE',  ( -0.8801773607111009756, 53.06368534415484106, 1.068504757029289695E-15 ) ) ;
#36116 = DIRECTION ( 'NONE',  ( -3.375077994860475883E-14, 0.000000000000000000, 1.000000000000000000 ) ) ;
#36115 = CARTESIAN_POINT ( 'NONE',  ( 22.81628187352647785, 26.41530133659708923, 3.434112377981063169 ) ) ;
#36117 = CARTESIAN_POINT ( 'NONE',  ( 44.01201084850834633, 60.14974815962801813, -8.000000000000000000 ) ) ;
#36118 = CARTESIAN_POINT ( 'NONE',  ( 0.000000000000000000, 14.49999999999999822, 0.000000000000000000 ) ) ;
#36119 = CARTESIAN_POINT ( 'NONE',  ( 22.81628187352647785, 1.415301336597087012, 3.434112377981063169 ) ) ;
#36120 = CARTESIAN_POINT ( 'NONE',  ( 19.84674366389459621, 8.508931151000785675, 7.409399052514197653E-17 ) ) ;
#36121 = CARTESIAN_POINT ( 'NONE',  ( 3.469446951953614189E-15, -30.68631465584515894, 10.88017736071110342 ) ) ;
#36122 = CARTESIAN_POINT ( 'NONE',  ( 3.591859063236763294, 23.29030133659708568, -11.09922568453595026 ) ) ;
#36123 = CARTESIAN_POINT ( 'NONE',  ( -10.82625193726620338, -96.00405735513218985, -4.000000000000000000 ) ) ;
#36125 = PLANE ( 'NONE',  #89509 ) ;
#36124 = CARTESIAN_POINT ( 'NONE',  ( 20.88017736071110164, 45.35535201082149115, 2.915334737309930979 ) ) ;
#36126 = VECTOR ( 'NONE', #39820, 1000.000000000000000 ) ;
#36127 = CARTESIAN_POINT ( 'NONE',  ( 64.56412365047462742, 13.99999999999999467, 10.00000000000000000 ) ) ;
#36128 = CARTESIAN_POINT ( 'NONE',  ( 6.934011249083991579, -73.15940021104376001, -3.750000000000000444 ) ) ;
#36129 = CIRCLE ( 'NONE', #25033, 0.2500000000000002220 ) ;
#36130 = CARTESIAN_POINT ( 'NONE',  ( 0.5774900079438590739, 32.64701867748816966, -5.440088680355550821 ) ) ;
#36131 = AXIS2_PLACEMENT_3D ( 'NONE', #15358, #55293, #47791 ) ;
#36132 = CIRCLE ( 'NONE', #61678, 7.250000000000002665 ) ;
#36133 = CARTESIAN_POINT ( 'NONE',  ( 20.88017736071110519, 35.56368534415484106, 2.639326808657452039E-16 ) ) ;
#36134 = CARTESIAN_POINT ( 'NONE',  ( 14.92337183194729988, 49.34226448433411605, -8.527530157486177487 ) ) ;
#36135 = ADVANCED_FACE ( 'NONE', ( #39992 ), #77484, .F. ) ;
#36136 = CARTESIAN_POINT ( 'NONE',  ( 17.96484262340118221, 49.93868534415484106, 7.964842623401181321 ) ) ;
#36137 = CARTESIAN_POINT ( 'NONE',  ( 10.00000000000000178, 33.05374883491396787, 14.16423886937410082 ) ) ;
#36138 = CARTESIAN_POINT ( 'NONE',  ( 0.000000000000000000, 0.5000000000000004441, 0.000000000000000000 ) ) ;
#36139 = VECTOR ( 'NONE', #24175, 1000.000000000000000 ) ;
#36140 = UNCERTAINTY_MEASURE_WITH_UNIT (LENGTH_MEASURE( 1.000000000000000082E-05 ), #35388, 'distance_accuracy_value', 'NONE');
#36141 = EDGE_CURVE ( 'NONE', #24045, #70993, #35995, .T. ) ;
#36142 = CARTESIAN_POINT ( 'NONE',  ( 2.791683348922240793, 36.63393115100078035, 7.208316651077764092 ) ) ;
#36143 = CARTESIAN_POINT ( 'NONE',  ( 0.6178305044545818747, 63.49863466993043204, -9.382169495545419124 ) ) ;
#36144 = CARTESIAN_POINT ( 'NONE',  ( 13.43411237798106583, 2.665301336597086568, -12.81628187352647252 ) ) ;
#36145 = EDGE_LOOP ( 'NONE', ( #42787, #59867, #58811, #18138 ) ) ;
#36146 = CARTESIAN_POINT ( 'NONE',  ( 10.00000000000000000, 21.81368534415484106, -10.88017736071110342 ) ) ;
#36147 = CARTESIAN_POINT ( 'NONE',  ( 7.084665262690076126, 7.022018677488169658, -10.88017736071110164 ) ) ;
#36148 = CARTESIAN_POINT ( 'NONE',  ( 15.44008868035555260, 14.73035201082150536, 9.422509992056143702 ) ) ;
#36149 = CARTESIAN_POINT ( 'NONE',  ( 5.076628168052704559, 0.1755978176674514724, -8.527530157486179263 ) ) ;
#36150 = CARTESIAN_POINT ( 'NONE',  ( 10.00000000000000178, 28.05374883491396787, 14.16423886937410082 ) ) ;
#36151 = CARTESIAN_POINT ( 'NONE',  ( 0.1532563361054082862, 11.21726448433411605, 2.638427012816831674 ) ) ;
#36152 = CARTESIAN_POINT ( 'NONE',  ( 18.52753015748618282, 63.92559781766745886, -4.923371831947291888 ) ) ;
#36153 = CARTESIAN_POINT ( 'NONE',  ( 4.559911319644449179, 38.89701867748817676, 9.422509992056141925 ) ) ;
#36154 = DIRECTION ( 'NONE',  ( 0.5664062369248205053, 0.000000000000000000, 0.8241261886220241362 ) ) ;
#36155 = CARTESIAN_POINT ( 'NONE',  ( 20.88017736071110519, 25.56368534415483751, 2.639326808657452039E-16 ) ) ;
#36156 = B_SPLINE_CURVE_WITH_KNOTS ( 'NONE', 3,
 ( #52009, #7990, #6498, #68000, #518, #7510 ),
 .UNSPECIFIED., .F., .F.,
 ( 4, 2, 4 ),
 ( 3.409110551496140855E-05, 0.0004400426677367876016, 0.0008459942299586138692 ),
 .UNSPECIFIED. ) ;
#36158 = ORIENTED_EDGE ( 'NONE', *, *, #12093, .F. ) ;
#36157 = AXIS2_PLACEMENT_3D ( 'NONE', #15234, #37735, #30692 ) ;
#36159 = LINE ( 'NONE', #97186, #36959 ) ;
#36160 = CARTESIAN_POINT ( 'NONE',  ( 2.791683348922240793, 46.63393115100077324, 7.208316651077764092 ) ) ;
#36161 = TOROIDAL_SURFACE ( 'NONE', #39394, 14.49999999999999822, 0.5000000000000000000 ) ;
#36162 = ORIENTED_EDGE ( 'NONE', *, *, #60120, .F. ) ;
#36163 = ORIENTED_EDGE ( 'NONE', *, *, #30955, .F. ) ;
#36164 = CARTESIAN_POINT ( 'NONE',  ( 0.3998276802503074046, 15.00000000000000000, 15.99117050944548879 ) ) ;
#36165 = CARTESIAN_POINT ( 'NONE',  ( 13.79529636645030344, 28.26208216824729647, 14.16423886937410614 ) ) ;
#36167 = AXIS2_PLACEMENT_3D ( 'NONE', #51112, #97629, #81599 ) ;
#36166 = CARTESIAN_POINT ( 'NONE',  ( 2.917880565312950480, 15.97041550158063217, -12.26659068614894821 ) ) ;
#36168 = CARTESIAN_POINT ( 'NONE',  ( 17.96484262340118221, 61.18868534415482685, -7.964842623401177768 ) ) ;
#36169 = CARTESIAN_POINT ( 'NONE',  ( 22.26659068614895176, 49.72041550158063927, -7.082119434687042414 ) ) ;
#36170 = CARTESIAN_POINT ( 'NONE',  ( 0.1532563361054083140, 66.00893115100079456, 1.131784320476157264E-15 ) ) ;
#36171 = CARTESIAN_POINT ( 'NONE',  ( 17.20831665107776587, 52.88393115100078035, 7.208316651077764980 ) ) ;
#36172 = CARTESIAN_POINT ( 'NONE',  ( -11.20041124612599504, -94.46430075981348295, 3.750000000000000000 ) ) ;
#36174 = CARTESIAN_POINT ( 'NONE',  ( 22.81628187352647785, 1.415301336597087012, 3.434112377981063169 ) ) ;
#36173 = CARTESIAN_POINT ( 'NONE',  ( 15.44008868035555260, 49.73035201082150536, 9.422509992056143702 ) ) ;
#36175 = CARTESIAN_POINT ( 'NONE',  ( -4.164238869374099927, 12.01208216824730357, 3.795296366450308767 ) ) ;
#36176 = CARTESIAN_POINT ( 'NONE',  ( 2.917880565312948704, 52.63708216824730357, 12.26659068614894643 ) ) ;
#36177 = CARTESIAN_POINT ( 'NONE',  ( 7.084665262690076126, 19.10535201082150181, 10.88017736071109987 ) ) ;
#36178 = CARTESIAN_POINT ( 'NONE',  ( 0.000000000000000000, 0.5000000000000004441, 0.000000000000000000 ) ) ;
#36179 = CARTESIAN_POINT ( 'NONE',  ( 19.42250999205614193, 45.14701867748817676, 5.440088680355555262 ) ) ;
#36180 = CARTESIAN_POINT ( 'NONE',  ( 19.50000000000000711, 105.0000000000000000, 5.000000000000000000 ) ) ;
#36181 = VERTEX_POINT ( 'NONE', #79466 ) ;
#36182 = CARTESIAN_POINT ( 'NONE',  ( 13.21272562211570012, -2.664342135588400928E-15, 6.271554226548244237 ) ) ;
#36183 = ORIENTED_EDGE ( 'NONE', *, *, #23665, .F. ) ;
#36184 = EDGE_LOOP ( 'NONE', ( #60653, #3365, #26828, #33234 ) ) ;
#36185 = COLOUR_RGB ( '', 0.08235294, 0.09019608, 0.10196078) ;
#36186 = CARTESIAN_POINT ( 'NONE',  ( 22.26659068614894466, 43.88708216824729647, 7.082119434687054849 ) ) ;
#36187 = CARTESIAN_POINT ( 'NONE',  ( 10.00000000000000178, 47.25893115100078745, 9.846743663894594434 ) ) ;
#36188 = CARTESIAN_POINT ( 'NONE',  ( 19.42250999205614548, 65.98035201082151957, -5.440088680355545492 ) ) ;
#36189 = EDGE_CURVE ( 'NONE', #86614, #1529, #1878, .T. ) ;
#36190 = CARTESIAN_POINT ( 'NONE',  ( -8.900000000000002132, 80.99999999999994316, 3.000000000000000000 ) ) ;
#36191 = CARTESIAN_POINT ( 'NONE',  ( -0.8801773607111009756, 48.06368534415484817, 1.068504757029289695E-15 ) ) ;
#36192 = PRESENTATION_LAYER_ASSIGNMENT (  '', '', ( #95270 ) ) ;
#36193 = B_SPLINE_CURVE_WITH_KNOTS ( 'NONE', 3,
 ( #68183, #83171, #38180, #84174, #46639, #31141 ),
 .UNSPECIFIED., .F., .F.,
 ( 4, 2, 4 ),
 ( 0.0002800364959417991299, 0.0006862420824208958397, 0.001092447668899992549 ),
 .UNSPECIFIED. ) ;
#36194 = CARTESIAN_POINT ( 'NONE',  ( 0.6178305044545838731, 54.74863466993042493, 9.382169495545420901 ) ) ;
#36195 = CARTESIAN_POINT ( 'NONE',  ( -3.434112377981067610, 13.08196800326375175, -12.81628187352647252 ) ) ;
#36196 = VECTOR ( 'NONE', #68526, 1000.000000000000114 ) ;
#36197 = EDGE_LOOP ( 'NONE', ( #96366, #49492, #28185, #68502 ) ) ;
#36198 = CARTESIAN_POINT ( 'NONE',  ( 2.917880565312948704, 17.63708216824730357, 12.26659068614894643 ) ) ;
#36199 = CARTESIAN_POINT ( 'NONE',  ( 6.565887622018943937, 20.16530133659708213, 12.81628187352647430 ) ) ;
#36200 = ORIENTED_EDGE ( 'NONE', *, *, #49123, .F. ) ;
#36201 = CARTESIAN_POINT ( 'NONE',  ( 19.38216949554541557, 47.24863466993041783, -9.382169495545420901 ) ) ;
#36202 = CARTESIAN_POINT ( 'NONE',  ( 17.20831665107776587, 32.88393115100078745, 7.208316651077764980 ) ) ;
#36203 = CARTESIAN_POINT ( 'NONE',  ( 2.035157376598822676, 7.438685344154837509, -7.964842623401177768 ) ) ;
#36204 = CARTESIAN_POINT ( 'NONE',  ( 6.565887622018943937, 48.08196800326375353, -12.81628187352647608 ) ) ;
#36205 = DIRECTION ( 'NONE',  ( 0.000000000000000000, 0.000000000000000000, -1.000000000000000000 ) ) ;
#36206 = CARTESIAN_POINT ( 'NONE',  ( 5.076628168052703671, 36.84226448433412315, 8.527530157486179263 ) ) ;
#36207 = VECTOR ( 'NONE', #25803, 1000.000000000000114 ) ;
#36208 =( BOUNDED_CURVE ( )  B_SPLINE_CURVE ( 2, ( #28721, #81714, #13226, #59211, #89715, #45209, #98744, #98238, #236 ),
 .UNSPECIFIED., .F., .T. ) 
 B_SPLINE_CURVE_WITH_KNOTS ( ( 3, 2, 2, 2, 3 ),
 ( 0.2615695083688028277, 0.2619047619047619735, 0.2678571428571429047, 0.2738095238095238360, 0.2741447773454829817 ),
 .UNSPECIFIED. ) 
 CURVE ( )  GEOMETRIC_REPRESENTATION_ITEM ( )  RATIONAL_B_SPLINE_CURVE ( ( 0.9963778908391760503, 0.9980808541467920403, 1.000000000000000000, 0.9659258262890683122, 1.000000000000000000, 0.9659258262890683122, 1.000000000000000000, 0.9980808541467920403, 0.9963778908391759392 ) ) 
 REPRESENTATION_ITEM ( '' )  );
#36209 = CARTESIAN_POINT ( 'NONE',  ( 4.559911319644449179, 68.89701867748817676, 9.422509992056141925 ) ) ;
#36210 = CARTESIAN_POINT ( 'NONE',  ( 14.99999999999997868, 80.07179676972448590, -6.500000000000000888 ) ) ;
#36211 = CARTESIAN_POINT ( 'NONE',  ( 1.274849032794231007, 33.57228050351031357, 6.499999999999895195 ) ) ;
#36212 = DIRECTION ( 'NONE',  ( 0.000000000000000000, 0.000000000000000000, 1.000000000000000000 ) ) ;
#36213 = VECTOR ( 'NONE', #10533, 1000.000000000000114 ) ;
#36214 = CARTESIAN_POINT ( 'NONE',  ( 1.274849032794292736, 67.55509018479936856, -6.499999999999977796 ) ) ;
#36215 = CARTESIAN_POINT ( 'NONE',  ( 2.791683348922237240, 15.38393115100078212, -7.208316651077763204 ) ) ;
#36216 = CARTESIAN_POINT ( 'NONE',  ( 0.6178305044545838731, 24.74863466993042493, 9.382169495545420901 ) ) ;
#36217 = LINE ( 'NONE', #66717, #29217 ) ;
#36218 = ORIENTED_EDGE ( 'NONE', *, *, #61852, .F. ) ;
#36219 = CARTESIAN_POINT ( 'NONE',  ( 10.00000000000000178, 62.25893115100078745, 9.846743663894594434 ) ) ;
#36220 = CARTESIAN_POINT ( 'NONE',  ( -11.35178980618981370, 0.3640475087720883018, 9.804941009311852085 ) ) ;
#36221 = CARTESIAN_POINT ( 'NONE',  ( -4.164238869374098151, 16.59541550158063927, -3.795296366450310543 ) ) ;
#36222 = CARTESIAN_POINT ( 'NONE',  ( 7.361572987183170547, 47.05059781766745175, 9.846743663894590881 ) ) ;
#36223 = CARTESIAN_POINT ( 'NONE',  ( -1.099225684535947600, 49.54030133659708923, 6.408140936763237150 ) ) ;
#36225 = DIRECTION ( 'NONE',  ( -0.8949343616020228875, 0.000000000000000000, -0.4461978131098131573 ) ) ;
#36224 = CARTESIAN_POINT ( 'NONE',  ( -14.47650479471817597, 0.3640475087720992375, -3.928206833722206692 ) ) ;
#36226 = CARTESIAN_POINT ( 'NONE',  ( 5.076628168052704559, 10.17559781766745175, -8.527530157486179263 ) ) ;
#36227 = STYLED_ITEM ( 'NONE', ( #46724 ), #32199 ) ;
#36228 = CARTESIAN_POINT ( 'NONE',  ( 11.34661744925197624, 54.08985607419764818, 0.000000000000000000 ) ) ;
#36229 = CARTESIAN_POINT ( 'NONE',  ( 19.84674366389459266, 33.30059781766744464, 2.638427012816836559 ) ) ;
#36230 = CARTESIAN_POINT ( 'NONE',  ( 4.559911319644449179, 43.89701867748816966, 9.422509992056141925 ) ) ;
#36231 = ADVANCED_FACE ( 'NONE', ( #70497 ), #85001, .T. ) ;
#36232 = AXIS2_PLACEMENT_3D ( 'NONE', #15587, #7089, #22590 ) ;
#36233 = CIRCLE ( 'NONE', #1145, 14.49999999999999822 ) ;
#36234 = SHAPE_DEFINITION_REPRESENTATION ( #14719, #61309 ) ;
#36235 = PLANE ( 'NONE',  #74668 ) ;
#36236 = TOROIDAL_SURFACE ( 'NONE', #69792, 14.49999999999999822, 0.5000000000000000000 ) ;
#36237 = CARTESIAN_POINT ( 'NONE',  ( 2.035157376598822676, 52.43868534415483396, -7.964842623401177768 ) ) ;
#36238 = ORIENTED_EDGE ( 'NONE', *, *, #74721, .F. ) ;
#36239 = CARTESIAN_POINT ( 'NONE',  ( 0.5774900079438607392, 68.48035201082150536, 5.440088680355550821 ) ) ;
#36240 = CARTESIAN_POINT ( 'NONE',  ( 0.5774900079438607392, 18.48035201082150536, 5.440088680355550821 ) ) ;
#36242 = CARTESIAN_POINT ( 'NONE',  ( 19.42250999205614548, 40.98035201082150536, -5.440088680355545492 ) ) ;
#36241 = CARTESIAN_POINT ( 'NONE',  ( 2.791683348922237240, 50.38393115100078035, -7.208316651077763204 ) ) ;
#36243 = DIRECTION ( 'NONE',  ( 0.000000000000000000, 1.000000000000000000, 0.000000000000000000 ) ) ;
#36244 = CARTESIAN_POINT ( 'NONE',  ( 2.035157376598824452, 53.68868534415484817, 7.964842623401179544 ) ) ;
#36245 = CARTESIAN_POINT ( 'NONE',  ( 7.084665262690076126, 24.10535201082150181, 10.88017736071109987 ) ) ;
#36246 = SURFACE_STYLE_FILL_AREA ( #35247 ) ;
#36247 = CARTESIAN_POINT ( 'NONE',  ( 5.076628168052703671, 21.84226448433411960, 8.527530157486179263 ) ) ;
#36248 = CARTESIAN_POINT ( 'NONE',  ( 5.500000000000000000, 61.00000000000000711, 6.000000000000000000 ) ) ;
#36249 = CARTESIAN_POINT ( 'NONE',  ( -14.16423886937410082, 11.80374883491398030, 4.336808689942017736E-15 ) ) ;
#36250 = CARTESIAN_POINT ( 'NONE',  ( 1.472469842513823179, 55.59226448433412315, -4.923371831947296329 ) ) ;
#36251 = PRESENTATION_LAYER_ASSIGNMENT (  '', '', ( #95345 ) ) ;
#36252 = CARTESIAN_POINT ( 'NONE',  ( 6.204703633549690345, 67.84541550158060375, 14.16423886937410082 ) ) ;
#36253 = FILL_AREA_STYLE_COLOUR ( '', #83305 ) ;
#36254 = CARTESIAN_POINT ( 'NONE',  ( 22.26659068614895176, 9.720415501580633943, -7.082119434687042414 ) ) ;
#36255 = CARTESIAN_POINT ( 'NONE',  ( 6.204703633549690345, 42.84541550158063217, 14.16423886937410082 ) ) ;
#36256 = CARTESIAN_POINT ( 'NONE',  ( 6.565887622018943937, -1.918031996736246692, -12.81628187352647608 ) ) ;
#36257 = VERTEX_POINT ( 'NONE', #25007 ) ;
#36258 = EDGE_CURVE ( 'NONE', #42615, #42002, #8875, .T. ) ;
#36259 = CARTESIAN_POINT ( 'NONE',  ( 17.96484262340118221, 16.18868534415483396, -7.964842623401177768 ) ) ;
#36260 = CARTESIAN_POINT ( 'NONE',  ( 18.52753015748618282, 53.92559781766745175, -4.923371831947291888 ) ) ;
#36262 = FACE_OUTER_BOUND ( 'NONE', #59571, .T. ) ;
#36261 = CARTESIAN_POINT ( 'NONE',  ( 22.17874357816322117, 89.00000000000000000, 12.00000000000000000 ) ) ;
#36263 = CARTESIAN_POINT ( 'NONE',  ( -5.999999999999994671, 43.00000000000000000, 6.500000000000000888 ) ) ;
#36264 = CIRCLE ( 'NONE', #5946, 15.00000000000000000 ) ;
#36265 = CARTESIAN_POINT ( 'NONE',  ( 12.63842701281683922, 4.550597817667451750, -9.846743663894590881 ) ) ;
#36266 = CARTESIAN_POINT ( 'NONE',  ( -1.099225684535947600, 18.70696800326375353, -6.408140936763238038 ) ) ;
#36267 = CARTESIAN_POINT ( 'NONE',  ( 1.472469842513823179, 31.42559781766745530, 4.923371831947296329 ) ) ;
#36269 = VERTEX_POINT ( 'NONE', #55492 ) ;
#36268 = EDGE_CURVE ( 'NONE', #79084, #12193, #3000, .T. ) ;
#36270 = CARTESIAN_POINT ( 'NONE',  ( 14.92337183194729988, 4.342264484334117824, -8.527530157486177487 ) ) ;
#36271 = DIRECTION ( 'NONE',  ( 0.000000000000000000, -1.000000000000000000, 0.000000000000000000 ) ) ;
#36272 = CARTESIAN_POINT ( 'NONE',  ( 10.00000000000000178, 9.313685344154839285, 10.88017736071110342 ) ) ;
#36273 = CARTESIAN_POINT ( 'NONE',  ( -4.164238869374099927, 37.01208216824731068, 3.795296366450308767 ) ) ;
#36274 = CARTESIAN_POINT ( 'NONE',  ( -0.8801773607111008646, 63.27201867748817676, 2.915334737309923430 ) ) ;
#36275 = CARTESIAN_POINT ( 'NONE',  ( 38.04706783004212411, 44.99999999999999289, -7.000000000000000000 ) ) ;
#36276 = CARTESIAN_POINT ( 'NONE',  ( 14.92337183194729633, 22.67559781766745175, 8.527530157486181039 ) ) ;
#36277 = CARTESIAN_POINT ( 'NONE',  ( 6.880000000000009663, 40.74999999999999289, 4.250000000000000000 ) ) ;
#36278 = CARTESIAN_POINT ( 'NONE',  ( 18.52753015748617571, 3.092264484334118269, 4.923371831947298993 ) ) ;
#36279 = CARTESIAN_POINT ( 'NONE',  ( -0.5867979546742444485, 6.298283880980277759E-16, -3.244044026693988059 ) ) ;
#36280 = CARTESIAN_POINT ( 'NONE',  ( 12.63842701281683922, 39.55059781766744464, -9.846743663894590881 ) ) ;
#36281 = CARTESIAN_POINT ( 'NONE',  ( 19.84674366389459266, 58.30059781766745886, 2.638427012816836559 ) ) ;
#36282 = CARTESIAN_POINT ( 'NONE',  ( 20.88017736071110164, 40.35535201082150536, 2.915334737309930979 ) ) ;
#36283 = UNCERTAINTY_MEASURE_WITH_UNIT (LENGTH_MEASURE( 1.000000000000000082E-05 ), #16551, 'distance_accuracy_value', 'NONE');
#36284 = AXIS2_PLACEMENT_3D ( 'NONE', #1746, #46722, #31220 ) ;
#36285 = VERTEX_POINT ( 'NONE', #33450 ) ;
#36286 = CARTESIAN_POINT ( 'NONE',  ( 3.591859063236761518, 54.95696800326376064, 11.09922568453594849 ) ) ;
#36287 = CARTESIAN_POINT ( 'NONE',  ( -8.099999999999999645, 80.99999999999994316, -3.000000000000000000 ) ) ;
#36288 = CARTESIAN_POINT ( 'NONE',  ( 7.361572987183170547, 7.050597817667451750, 9.846743663894590881 ) ) ;
#36289 = CARTESIAN_POINT ( 'NONE',  ( 22.81628187352647785, 46.62363466993041783, 6.195893100308588602E-16 ) ) ;
#36291 = CARTESIAN_POINT ( 'NONE',  ( 0.1532563361054100626, 35.80059781766745175, -2.638427012816831230 ) ) ;
#36290 = CARTESIAN_POINT ( 'NONE',  ( 22.26659068614895176, 64.72041550158064638, -7.082119434687042414 ) ) ;
#36292 = PRESENTATION_LAYER_ASSIGNMENT (  '', '', ( #79397 ) ) ;
#36293 = CARTESIAN_POINT ( 'NONE',  ( 1.472469842513823179, 0.5922644843341181575, -4.923371831947296329 ) ) ;
#36294 = CARTESIAN_POINT ( 'NONE',  ( 2.917880565312950480, 45.97041550158063927, -12.26659068614894821 ) ) ;
#36295 = CARTESIAN_POINT ( 'NONE',  ( 19.84674366389459266, 38.71726448433412315, -2.638427012816827677 ) ) ;
#36296 = CARTESIAN_POINT ( 'NONE',  ( 6.655501998725182666, -69.44085999584420676, -2.499999999999999556 ) ) ;
#36297 = CARTESIAN_POINT ( 'NONE',  ( 17.96484262340118221, 34.93868534415482685, 7.964842623401181321 ) ) ;
#36298 = CARTESIAN_POINT ( 'NONE',  ( 0.1532563361054100626, 0.8005978176674514168, -2.638427012816831230 ) ) ;
#36299 = COLOUR_RGB ( '', 0.66274510, 0.83137255, 0.94901961) ;
#36300 =( LENGTH_UNIT ( ) NAMED_UNIT ( * ) SI_UNIT ( .MILLI., .METRE. ) );
#36301 = ORIENTED_EDGE ( 'NONE', *, *, #24867, .F. ) ;
#36302 = CARTESIAN_POINT ( 'NONE',  ( 3.591859063236763294, 58.29030133659708923, -11.09922568453595026 ) ) ;
#36303 = ORIENTED_EDGE ( 'NONE', *, *, #1167, .T. ) ;
#36304 = CARTESIAN_POINT ( 'NONE',  ( 10.00000000000000000, 61.81368534415484106, -10.88017736071110342 ) ) ;
#36305 = VERTEX_POINT ( 'NONE', #40497 ) ;
#36306 = CARTESIAN_POINT ( 'NONE',  ( 6.204703633549690345, 0.7620821682473009062, -14.16423886937410259 ) ) ;
#36307 = CARTESIAN_POINT ( 'NONE',  ( 19.84674366389459266, 3.717264484334118713, -2.638427012816827677 ) ) ;
#36308 = EDGE_CURVE ( 'NONE', #43937, #31231, #56762, .T. ) ;
#36309 = CARTESIAN_POINT ( 'NONE',  ( 10.84451454130507209, 15.00000000000000000, -9.625305416630832056 ) ) ;
#36310 = ORIENTED_EDGE ( 'NONE', *, *, #44603, .T. ) ;
#36311 = VECTOR ( 'NONE', #71833, 1000.000000000000000 ) ;
#36312 = CARTESIAN_POINT ( 'NONE',  ( 20.88017736071110519, 10.56368534415483751, 2.639326808657452039E-16 ) ) ;
#36313 = CARTESIAN_POINT ( 'NONE',  ( -9.957606878385396598, 13.12720750352077381, 6.606639848592291919 ) ) ;
#36314 = ORIENTED_EDGE ( 'NONE', *, *, #52943, .F. ) ;
#36315 = CARTESIAN_POINT ( 'NONE',  ( -0.8801773607111009756, 23.06368534415484106, 1.068504757029289695E-15 ) ) ;
#36316 = CARTESIAN_POINT ( 'NONE',  ( 12.63842701281683922, 59.55059781766744464, -9.846743663894590881 ) ) ;
#36317 = ORIENTED_EDGE ( 'NONE', *, *, #27217, .F. ) ;
#36318 = EDGE_CURVE ( 'NONE', #91549, #38899, #13654, .T. ) ;
#36319 = CARTESIAN_POINT ( 'NONE',  ( 0.1532563361054100626, 65.80059781766745175, -2.638427012816831230 ) ) ;
#36320 = ORIENTED_EDGE ( 'NONE', *, *, #74212, .F. ) ;
#36321 = CARTESIAN_POINT ( 'NONE',  ( 5.076628168052703671, 1.842264484334118047, 8.527530157486179263 ) ) ;
#36322 = CARTESIAN_POINT ( 'NONE',  ( 19.84674366389459266, 63.71726448433412315, -2.638427012816827677 ) ) ;
#36323 = CARTESIAN_POINT ( 'NONE',  ( 6.565887622018943937, 40.16530133659708923, 12.81628187352647430 ) ) ;
#36324 = CARTESIAN_POINT ( 'NONE',  ( -0.8801773607111008646, 3.272018677488171434, 2.915334737309923430 ) ) ;
#36325 = CARTESIAN_POINT ( 'NONE',  ( 19.84674366389459266, 3.717264484334118713, -2.638427012816827677 ) ) ;
#36326 = CARTESIAN_POINT ( 'NONE',  ( 2.035157376598822676, 17.43868534415483751, -7.964842623401177768 ) ) ;
#36327 = ORIENTED_EDGE ( 'NONE', *, *, #33793, .F. ) ;
#36328 = CARTESIAN_POINT ( 'NONE',  ( -1.099225684535947600, 54.54030133659708923, 6.408140936763237150 ) ) ;
#36329 = CARTESIAN_POINT ( 'NONE',  ( 0.5774900079438590739, 47.64701867748817676, -5.440088680355550821 ) ) ;
#36330 = CARTESIAN_POINT ( 'NONE',  ( -8.209432707284955555, 0.3640475087720992375, 12.55409154915480308 ) ) ;
#36331 = CARTESIAN_POINT ( 'NONE',  ( -1.099225684535947600, 48.70696800326375353, -6.408140936763238038 ) ) ;
#36332 = CARTESIAN_POINT ( 'NONE',  ( 20.88017736071110875, 50.77201867748817676, -2.915334737309920765 ) ) ;
#36333 = CIRCLE ( 'NONE', #87434, 14.49999999999999822 ) ;
#36334 = CARTESIAN_POINT ( 'NONE',  ( 0.1532563361054083140, 61.00893115100078745, 1.131784320476157264E-15 ) ) ;
#36335 = FACE_OUTER_BOUND ( 'NONE', #59219, .T. ) ;
#36336 = AXIS2_PLACEMENT_3D ( 'NONE', #14235, #98244, #29703 ) ;
#36337 = CARTESIAN_POINT ( 'NONE',  ( 12.63842701281683034, 22.46726448433411605, 9.846743663894596210 ) ) ;
#36338 = CARTESIAN_POINT ( 'NONE',  ( -2.816281873526471635, 3.915301336597087456, -3.434112377981056508 ) ) ;
#36340 = CARTESIAN_POINT ( 'NONE',  ( 0.1532563361054100626, 65.80059781766745175, -2.638427012816831230 ) ) ;
#36339 = CYLINDRICAL_SURFACE ( 'NONE', #27661, 0.5000000000000004441 ) ;
#36341 = CARTESIAN_POINT ( 'NONE',  ( 15.44008868035555793, 26.39701867748817321, -9.422509992056140149 ) ) ;
#36342 = CARTESIAN_POINT ( 'NONE',  ( 0.1532563361054082862, 56.21726448433411605, 2.638427012816831674 ) ) ;
#36343 = CARTESIAN_POINT ( 'NONE',  ( 10.00000000000000000, 4.758931151000784787, -9.846743663894594434 ) ) ;
#36344 = CARTESIAN_POINT ( 'NONE',  ( 1.274849032794116210, 8.572280503510292249, 6.499999999999738876 ) ) ;
#36345 = EDGE_CURVE ( 'NONE', #29582, #47699, #1027, .T. ) ;
#36347 = VERTEX_POINT ( 'NONE', #16514 ) ;
#36346 = CARTESIAN_POINT ( 'NONE',  ( 13.43411237798106583, 7.665301336597086568, -12.81628187352647252 ) ) ;
#36348 = AXIS2_PLACEMENT_3D ( 'NONE', #67550, #13552, #22549 ) ;
#36349 = CARTESIAN_POINT ( 'NONE',  ( -5.999999999999994671, 43.00000000000000000, -4.250000000000000000 ) ) ;
#36350 = CARTESIAN_POINT ( 'NONE',  ( -14.16722289976678617, 0.5000000000000004441, -4.928467845925704083 ) ) ;
#36351 = CARTESIAN_POINT ( 'NONE',  ( 3.591859063236761518, 34.95696800326375353, 11.09922568453594849 ) ) ;
#36352 = CARTESIAN_POINT ( 'NONE',  ( 19.84674366389459266, 33.30059781766744464, 2.638427012816836559 ) ) ;
#36353 = CARTESIAN_POINT ( 'NONE',  ( -4.289191146912808207E-15, 8.868033628982656680, -11.25000000000000178 ) ) ;
#36355 = EDGE_CURVE ( 'NONE', #55640, #10095, #61332, .T. ) ;
#36354 = CARTESIAN_POINT ( 'NONE',  ( -4.164238869374098151, 66.59541550158060375, -3.795296366450310543 ) ) ;
#36356 = CARTESIAN_POINT ( 'NONE',  ( 10.00000000000000000, 29.75893115100078745, -9.846743663894594434 ) ) ;
#36357 = DIRECTION ( 'NONE',  ( 0.6246950475544238435, 0.7808688094430307203, 0.000000000000000000 ) ) ;
#36358 = CARTESIAN_POINT ( 'NONE',  ( 20.36894250292379738, 64.92874883491397497, -10.36894250292379027 ) ) ;
#36359 = LINE ( 'NONE', #35369, #72709 ) ;
#36360 = CARTESIAN_POINT ( 'NONE',  ( 0.5774900079438607392, 23.48035201082150536, 5.440088680355550821 ) ) ;
#36362 = AXIS2_PLACEMENT_3D ( 'NONE', #50189, #35181, #87208 ) ;
#36361 = CARTESIAN_POINT ( 'NONE',  ( 6.204703633549690345, 52.84541550158062506, 14.16423886937410082 ) ) ;
#36363 = CARTESIAN_POINT ( 'NONE',  ( -0.3689425029237881626, 52.42874883491396076, 10.36894250292379027 ) ) ;
#36364 = DIRECTION ( 'NONE',  ( 0.000000000000000000, 0.000000000000000000, 1.000000000000000000 ) ) ;
#36365 = B_SPLINE_CURVE_WITH_KNOTS ( 'NONE', 3,
 ( #11058, #24601, #18073, #70583, #55067, #87052 ),
 .UNSPECIFIED., .F., .F.,
 ( 4, 2, 4 ),
 ( 0.0002800005319459032628, 0.0006862057665691756025, 0.001092411001192447996 ),
 .UNSPECIFIED. ) ;
#36366 = CARTESIAN_POINT ( 'NONE',  ( 17.20831665107776587, 14.13393115100078568, -7.208316651077762316 ) ) ;
#36367 = EDGE_CURVE ( 'NONE', #9889, #12702, #11454, .T. ) ;
#36368 = CARTESIAN_POINT ( 'NONE',  ( 5.076628168052704559, 65.17559781766745175, -8.527530157486179263 ) ) ;
#36369 = ORIENTED_EDGE ( 'NONE', *, *, #43686, .F. ) ;
#36370 = CARTESIAN_POINT ( 'NONE',  ( -0.8801773607110991993, 47.85535201082150536, -2.915334737309923874 ) ) ;
#36372 = CARTESIAN_POINT ( 'NONE',  ( -46.94000000000001194, 100.4376529975800025, -8.999999999986080468 ) ) ;
#36371 = VECTOR ( 'NONE', #51500, 1000.000000000000114 ) ;
#36373 = VECTOR ( 'NONE', #9126, 1000.000000000000000 ) ;
#36374 = CARTESIAN_POINT ( 'NONE',  ( 10.00000000000000178, 67.25893115100079456, 9.846743663894594434 ) ) ;
#36375 = CARTESIAN_POINT ( 'NONE',  ( 6.204703633549690345, 2.845415501580634388, 14.16423886937410082 ) ) ;
#36376 = B_SPLINE_CURVE_WITH_KNOTS ( 'NONE', 3,
 ( #35258, #18799, #80276, #96281, #18305, #10805 ),
 .UNSPECIFIED., .F., .F.,
 ( 4, 2, 4 ),
 ( 0.0002800338592528457487, 0.0006862394199277645993, 0.001092444980602683613 ),
 .UNSPECIFIED. ) ;
#36377 = CARTESIAN_POINT ( 'NONE',  ( 10.00000000000000178, 22.25893115100078745, 9.846743663894594434 ) ) ;
#36378 = FACE_BOUND ( 'NONE', #683, .T. ) ;
#36379 = CARTESIAN_POINT ( 'NONE',  ( 13.79529636645031943, 35.34541550158063927, -14.16423886937409904 ) ) ;
#36380 = CARTESIAN_POINT ( 'NONE',  ( 0.1532563361054083140, 11.00893115100078568, 1.131784320476157264E-15 ) ) ;
#36382 = CARTESIAN_POINT ( 'NONE',  ( 0.000000000000000000, 0.5000000000000004441, 0.000000000000000000 ) ) ;
#36381 = CARTESIAN_POINT ( 'NONE',  ( -0.1042174387088605353, 63.10736173766204615, 6.337391062633419558 ) ) ;
#36383 = CARTESIAN_POINT ( 'NONE',  ( 10.00000000000000000, 36.81368534415484106, -10.88017736071110342 ) ) ;
#36384 = CARTESIAN_POINT ( 'NONE',  ( -1.099225684535947600, 38.70696800326375353, -6.408140936763238038 ) ) ;
#36385 = CARTESIAN_POINT ( 'NONE',  ( 17.96484262340118221, 4.938685344154837509, 7.964842623401181321 ) ) ;
#36386 = CARTESIAN_POINT ( 'NONE',  ( 21.09922568453595559, 37.04030133659708923, -6.408140936763230044 ) ) ;
#36387 = CARTESIAN_POINT ( 'NONE',  ( 19.38216949554541202, 55.99863466993041072, 9.382169495545424454 ) ) ;
#36389 = EDGE_CURVE ( 'NONE', #27786, #79719, #73192, .T. ) ;
#36388 = ORIENTED_EDGE ( 'NONE', *, *, #94607, .T. ) ;
#36390 = LINE ( 'NONE', #5416, #62840 ) ;
#36391 = CARTESIAN_POINT ( 'NONE',  ( -11.33436264772833724, -69.53389133802667743, -3.999999999999999112 ) ) ;
#36392 = CARTESIAN_POINT ( 'NONE',  ( 2.917880565312948704, 37.63708216824731068, 12.26659068614894643 ) ) ;
#36393 = CARTESIAN_POINT ( 'NONE',  ( -2.266590686148945544, 2.220415501580634388, 7.082119434687048631 ) ) ;
#36394 = CARTESIAN_POINT ( 'NONE',  ( -0.8801773607110991993, 12.85535201082150358, -2.915334737309923874 ) ) ;
#36395 = CARTESIAN_POINT ( 'NONE',  ( 4.559911319644449179, 18.89701867748817321, 9.422509992056141925 ) ) ;
#36396 = LINE ( 'NONE', #35892, #82996 ) ;
#36397 = FACE_OUTER_BOUND ( 'NONE', #65577, .T. ) ;
#36398 = CARTESIAN_POINT ( 'NONE',  ( 2.035157376598822676, 47.43868534415484817, -7.964842623401177768 ) ) ;
#36399 = CARTESIAN_POINT ( 'NONE',  ( 15.44008868035555260, 54.73035201082150536, 9.422509992056143702 ) ) ;
#36400 = CARTESIAN_POINT ( 'NONE',  ( 10.00000000000000000, 17.87363466993041783, -12.81628187352647608 ) ) ;
#36401 = CARTESIAN_POINT ( 'NONE',  ( -5.817157072110894056, 0.3639308157993875747, 13.82608706751086913 ) ) ;
#36402 = CARTESIAN_POINT ( 'NONE',  ( 0.000000000000000000, 70.80332830338373640, -5.000000000000000000 ) ) ;
#36403 = CARTESIAN_POINT ( 'NONE',  ( 2.791683348922237240, 25.38393115100078390, -7.208316651077763204 ) ) ;
#36404 = CARTESIAN_POINT ( 'NONE',  ( -0.8801773607111008646, 58.27201867748816966, 2.915334737309923430 ) ) ;
#36405 = CARTESIAN_POINT ( 'NONE',  ( -1.099225684535947600, 13.70696800326375353, -6.408140936763238038 ) ) ;
#36406 =( LENGTH_UNIT ( ) NAMED_UNIT ( * ) SI_UNIT ( .MILLI., .METRE. ) );
#36407 = CARTESIAN_POINT ( 'NONE',  ( 4.559911319644449179, 13.89701867748817143, 9.422509992056141925 ) ) ;
#36408 = CARTESIAN_POINT ( 'NONE',  ( 10.00000000000000000, 39.75893115100078745, -9.846743663894594434 ) ) ;
#36409 = CARTESIAN_POINT ( 'NONE',  ( 16.40814093676324603, 47.45696800326375353, -11.09922568453594671 ) ) ;
#36411 =( LENGTH_UNIT ( ) NAMED_UNIT ( * ) SI_UNIT ( .MILLI., .METRE. ) );
#36410 = CARTESIAN_POINT ( 'NONE',  ( 1.472469842513823179, 21.42559781766745175, 4.923371831947296329 ) ) ;
#36412 = CARTESIAN_POINT ( 'NONE',  ( 13.79529636645031943, 10.34541550158063394, -14.16423886937409904 ) ) ;
#36413 = FACE_OUTER_BOUND ( 'NONE', #80341, .T. ) ;
#36414 = CARTESIAN_POINT ( 'NONE',  ( 15.44008868035555260, 24.73035201082150891, 9.422509992056143702 ) ) ;
#36416 = CARTESIAN_POINT ( 'NONE',  ( 13.79529636645030344, 28.26208216824729647, 14.16423886937410614 ) ) ;
#36415 = DIRECTION ( 'NONE',  ( -0.9961946980917461003, 0.08715574274765068574, 0.000000000000000000 ) ) ;
#36417 = CARTESIAN_POINT ( 'NONE',  ( 18.52753015748617571, 28.09226448433411960, 4.923371831947298993 ) ) ;
#36418 = CARTESIAN_POINT ( 'NONE',  ( 0.5774900079438607392, 23.48035201082150536, 5.440088680355550821 ) ) ;
#36419 = CARTESIAN_POINT ( 'NONE',  ( 0.5774900079438607392, 23.48035201082150536, 5.440088680355550821 ) ) ;
#36420 = EDGE_LOOP ( 'NONE', ( #43954, #77723, #47168, #50962 ) ) ;
#36421 = CARTESIAN_POINT ( 'NONE',  ( 10.00000000000000000, 26.81368534415484106, -10.88017736071110342 ) ) ;
#36422 = CARTESIAN_POINT ( 'NONE',  ( -2.816281873526473856, 44.33196800326375353, 3.434112377981055619 ) ) ;
#36423 = ADVANCED_FACE ( 'NONE', ( #64440 ), #73923, .T. ) ;
#36424 = CARTESIAN_POINT ( 'NONE',  ( 19.42250999205614193, 40.14701867748817676, 5.440088680355555262 ) ) ;
#36426 = CARTESIAN_POINT ( 'NONE',  ( 15.44008868035555260, 39.73035201082150536, 9.422509992056143702 ) ) ;
#36425 = DIRECTION ( 'NONE',  ( -1.000000000000000000, 0.000000000000000000, 0.000000000000000000 ) ) ;
#36427 = TOROIDAL_SURFACE ( 'NONE', #74743, 14.49999999999999822, 0.5000000000000000000 ) ;
#36428 = ORIENTED_EDGE ( 'NONE', *, *, #79964, .T. ) ;
#36429 = CARTESIAN_POINT ( 'NONE',  ( 5.076628168052703671, 51.84226448433412315, 8.527530157486179263 ) ) ;
#36430 = CARTESIAN_POINT ( 'NONE',  ( 0.5774900079438607392, 38.48035201082150536, 5.440088680355550821 ) ) ;
#36431 = SURFACE_STYLE_FILL_AREA ( #43427 ) ;
#36432 = FILL_AREA_STYLE_COLOUR ( '', #56884 ) ;
#36433 = CARTESIAN_POINT ( 'NONE',  ( -0.1038446121089122015, 9.243024370107935539, -6.337995344473772441 ) ) ;
#36434 = CARTESIAN_POINT ( 'NONE',  ( 6.204703633549690345, 52.84541550158062506, 14.16423886937410082 ) ) ;
#36435 = CARTESIAN_POINT ( 'NONE',  ( 15.44008868035555260, 54.73035201082150536, 9.422509992056143702 ) ) ;
#36436 = DIRECTION ( 'NONE',  ( 0.000000000000000000, 1.000000000000000000, 0.000000000000000000 ) ) ;
#36437 = CARTESIAN_POINT ( 'NONE',  ( -10.85532661662059972, -98.11526154878892214, -3.749999999999999556 ) ) ;
#36438 = CARTESIAN_POINT ( 'NONE',  ( 19.84674366389459266, 63.30059781766745886, 2.638427012816836559 ) ) ;
#36439 = CARTESIAN_POINT ( 'NONE',  ( 10.00000000000000178, 2.258931151000784787, 9.846743663894594434 ) ) ;
#36440 = CARTESIAN_POINT ( 'NONE',  ( 17.20831665107776587, 24.13393115100078035, -7.208316651077762316 ) ) ;
#36441 = ORIENTED_EDGE ( 'NONE', *, *, #31312, .T. ) ;
#36442 = CARTESIAN_POINT ( 'NONE',  ( 1.472469842513823179, 16.42559781766745175, 4.923371831947296329 ) ) ;
#36443 = CARTESIAN_POINT ( 'NONE',  ( -9.382169495545422677, -16.50136533006957862, -9.382169495545417348 ) ) ;
#36444 = VECTOR ( 'NONE', #61185, 1000.000000000000000 ) ;
#36445 = CARTESIAN_POINT ( 'NONE',  ( 4.559911319644449179, 28.89701867748817321, 9.422509992056141925 ) ) ;
#36446 = CARTESIAN_POINT ( 'NONE',  ( 14.92337183194729988, 19.34226448433411960, -8.527530157486177487 ) ) ;
#36447 = CARTESIAN_POINT ( 'NONE',  ( 22.81628187352647785, 6.415301336597088344, 3.434112377981063169 ) ) ;
#36449 = CARTESIAN_POINT ( 'NONE',  ( -0.8801773607111009756, 58.06368534415484106, 1.068504757029289695E-15 ) ) ;
#36448 = CARTESIAN_POINT ( 'NONE',  ( 7.084665262690076126, 59.10535201082150536, 10.88017736071109987 ) ) ;
#36451 = CARTESIAN_POINT ( 'NONE',  ( 19.38216949554541202, 60.99863466993042493, 9.382169495545424454 ) ) ;
#36450 = CARTESIAN_POINT ( 'NONE',  ( 2.035157376598824452, 38.68868534415483396, 7.964842623401179544 ) ) ;
#36452 = CARTESIAN_POINT ( 'NONE',  ( 20.36894250292379738, 49.92874883491396787, -10.36894250292379027 ) ) ;
#36453 = CIRCLE ( 'NONE', #9316, 14.49999999999999822 ) ;
#36454 = VECTOR ( 'NONE', #76030, 999.9999999999998863 ) ;
#36455 = DIRECTION ( 'NONE',  ( -0.8526401643540884034, 0.000000000000000000, -0.5224985647159551272 ) ) ;
#36456 = ORIENTED_EDGE ( 'NONE', *, *, #35991, .T. ) ;
#36457 = CARTESIAN_POINT ( 'NONE',  ( 13.43411237798105340, 0.5819680032637533085, 12.81628187352647963 ) ) ;
#36458 = CARTESIAN_POINT ( 'NONE',  ( 4.559911319644449179, 52.23035201082151247, -9.422509992056141925 ) ) ;
#36459 = CARTESIAN_POINT ( 'NONE',  ( 6.204703633549690345, 0.7620821682473009062, -14.16423886937410259 ) ) ;
#36460 = VERTEX_POINT ( 'NONE', #79949 ) ;
#36461 = CARTESIAN_POINT ( 'NONE',  ( 12.63842701281683922, 14.55059781766744997, -9.846743663894590881 ) ) ;
#36462 = PRODUCT ( '1.0 Fixed Jaw', '1.0 Fixed Jaw', '', ( #60699 ) ) ;
#36463 = CARTESIAN_POINT ( 'NONE',  ( 12.91533473730992121, 59.52201867748816966, 10.88017736071110164 ) ) ;
#36464 = CARTESIAN_POINT ( 'NONE',  ( 19.84674366389459621, 33.50893115100078745, 7.409399052514197653E-17 ) ) ;
#36465 = CARTESIAN_POINT ( 'NONE',  ( 19.84674366389459266, 28.71726448433411960, -2.638427012816827677 ) ) ;
#36466 = CARTESIAN_POINT ( 'NONE',  ( 2.791683348922240793, 16.63393115100078745, 7.208316651077764092 ) ) ;
#36468 = CARTESIAN_POINT ( 'NONE',  ( 0.6178305044545818747, 38.49863466993042493, -9.382169495545419124 ) ) ;
#36467 = CARTESIAN_POINT ( 'NONE',  ( -6.871342362925322078, -73.24551516664604378, 2.500000000000000000 ) ) ;
#36470 = FACE_OUTER_BOUND ( 'NONE', #53381, .T. ) ;
#36469 = CARTESIAN_POINT ( 'NONE',  ( 19.84674366389459266, 3.717264484334118713, -2.638427012816827677 ) ) ;
#36471 = CARTESIAN_POINT ( 'NONE',  ( 9.729341964144056831, -19.62354698955503451, 4.000000000000000000 ) ) ;
#36473 = ORIENTED_EDGE ( 'NONE', *, *, #93228, .F. ) ;
#36472 = CARTESIAN_POINT ( 'NONE',  ( 0.1532563361054082862, 26.21726448433411605, 2.638427012816831674 ) ) ;
#36474 = EDGE_CURVE ( 'NONE', #81080, #23413, #66107, .T. ) ;
#36475 = CARTESIAN_POINT ( 'NONE',  ( 6.565887622018943937, 53.08196800326374643, -12.81628187352647608 ) ) ;
#36476 = CARTESIAN_POINT ( 'NONE',  ( -7.199999999999996625, 99.99999999999998579, -8.525133428036873795 ) ) ;
#36477 = CARTESIAN_POINT ( 'NONE',  ( -1.099225684535947600, -1.293031996736246469, -6.408140936763238038 ) ) ;
#36478 = CARTESIAN_POINT ( 'NONE',  ( 2.035157376598824452, 3.688685344154837953, 7.964842623401179544 ) ) ;
#36479 = ADVANCED_FACE ( 'NONE', ( #50928 ), #89422, .F. ) ;
#36481 = EDGE_CURVE ( 'NONE', #56358, #60281, #50478, .T. ) ;
#36480 = CARTESIAN_POINT ( 'NONE',  ( 13.79529636645031943, 15.34541550158063750, -14.16423886937409904 ) ) ;
#36482 = PRODUCT_DEFINITION_CONTEXT ( 'detailed design', #98582, 'design' ) ;
#36483 = CARTESIAN_POINT ( 'NONE',  ( 34.56412365047464874, 28.99999999999999645, 9.500000000000000000 ) ) ;
#36484 = CARTESIAN_POINT ( 'NONE',  ( 2.917880565312950480, 35.97041550158063217, -12.26659068614894821 ) ) ;
#36485 = CARTESIAN_POINT ( 'NONE',  ( 10.00000000000000000, 45.55374883491397497, -14.16423886937410082 ) ) ;
#36486 = CARTESIAN_POINT ( 'NONE',  ( 24.16423886937410614, 9.303748834913967869, 8.672049930838204340E-16 ) ) ;
#36488 = DIRECTION ( 'NONE',  ( -0.000000000000000000, 0.000000000000000000, 1.000000000000000000 ) ) ;
#36487 = CARTESIAN_POINT ( 'NONE',  ( -4.164238869374099927, 17.01208216824730357, 3.795296366450308767 ) ) ;
#36489 = CARTESIAN_POINT ( 'NONE',  ( 17.96484262340118221, 44.93868534415483396, 7.964842623401181321 ) ) ;
#36490 = CARTESIAN_POINT ( 'NONE',  ( 10.70613742633251420, 4.218616272510096815E-16, 9.778988772285311271 ) ) ;
#36491 = CARTESIAN_POINT ( 'NONE',  ( 18.52753015748618282, 28.92559781766745175, -4.923371831947291888 ) ) ;
#36493 = CARTESIAN_POINT ( 'NONE',  ( 14.92337183194729633, 32.67559781766745175, 8.527530157486181039 ) ) ;
#36492 = CARTESIAN_POINT ( 'NONE',  ( 2.035157376598824452, 68.68868534415484817, 7.964842623401179544 ) ) ;
#36494 = CARTESIAN_POINT ( 'NONE',  ( 17.96484262340118221, 14.93868534415484106, 7.964842623401181321 ) ) ;
#36495 = CARTESIAN_POINT ( 'NONE',  ( 3.591859063236761518, 64.95696800326376774, 11.09922568453594849 ) ) ;
#36496 = CARTESIAN_POINT ( 'NONE',  ( 19.84674366389459266, 48.71726448433413026, -2.638427012816827677 ) ) ;
#36497 = CARTESIAN_POINT ( 'NONE',  ( 0.000000000000000000, 14.49999999999999822, 0.000000000000000000 ) ) ;
#36498 = CARTESIAN_POINT ( 'NONE',  ( 18.52753015748617571, 23.09226448433411960, 4.923371831947298993 ) ) ;
#36499 = CARTESIAN_POINT ( 'NONE',  ( 0.6178305044545838731, 44.74863466993042493, 9.382169495545420901 ) ) ;
#36500 = CARTESIAN_POINT ( 'NONE',  ( -10.36894250292379205, -18.82125116508602858, -10.36894250292378672 ) ) ;
#36501 = CARTESIAN_POINT ( 'NONE',  ( 4.559911319644449179, 42.23035201082151247, -9.422509992056141925 ) ) ;
#36502 = CARTESIAN_POINT ( 'NONE',  ( 14.92337183194729633, 42.67559781766745886, 8.527530157486181039 ) ) ;
#36503 = CARTESIAN_POINT ( 'NONE',  ( 22.26659068614894466, 28.88708216824730357, 7.082119434687054849 ) ) ;
#36504 = ORIENTED_EDGE ( 'NONE', *, *, #46255, .F. ) ;
#36505 = CARTESIAN_POINT ( 'NONE',  ( -0.3689425029237881626, 2.428748834913967869, 10.36894250292379027 ) ) ;
#36506 = CARTESIAN_POINT ( 'NONE',  ( 10.00000000000000000, 51.81368534415484106, -10.88017736071110342 ) ) ;
#36507 = CARTESIAN_POINT ( 'NONE',  ( -0.1491070598754174470, 61.94583914210339515, 4.500000000000000888 ) ) ;
#36508 = CARTESIAN_POINT ( 'NONE',  ( 10.00000000000000000, 55.55374883491396787, -14.16423886937410082 ) ) ;
#36509 = CARTESIAN_POINT ( 'NONE',  ( 14.92337183194729633, 62.67559781766745886, 8.527530157486181039 ) ) ;
#36510 = CARTESIAN_POINT ( 'NONE',  ( 0.000000000000000000, 0.000000000000000000, -14.25000000000000000 ) ) ;
#36511 = CARTESIAN_POINT ( 'NONE',  ( 0.5774900079438607392, 48.48035201082150536, 5.440088680355550821 ) ) ;
#36512 = EDGE_CURVE ( 'NONE', #29252, #84180, #28138, .T. ) ;
#36513 = CARTESIAN_POINT ( 'NONE',  ( 0.2751277870542911952, 38.21833443783937412, 6.499999999999992006 ) ) ;
#36514 = MECHANICAL_DESIGN_GEOMETRIC_PRESENTATION_REPRESENTATION (  '', ( #20524 ), #6178 ) ;
#36515 = CARTESIAN_POINT ( 'NONE',  ( 3.591859063236761518, 29.95696800326375708, 11.09922568453594849 ) ) ;
#36516 = CARTESIAN_POINT ( 'NONE',  ( 19.38216949554541557, 2.248634669930420049, -9.382169495545420901 ) ) ;
#36517 = CARTESIAN_POINT ( 'NONE',  ( -5.440088680355558814, 22.23035201082151957, -9.422509992056136596 ) ) ;
#36518 = CARTESIAN_POINT ( 'NONE',  ( 19.42250999205614193, 15.14701867748817143, 5.440088680355555262 ) ) ;
#36519 = CARTESIAN_POINT ( 'NONE',  ( -0.8801773607111008646, 8.272018677488171434, 2.915334737309923430 ) ) ;
#36520 = CARTESIAN_POINT ( 'NONE',  ( 19.84674366389459266, 48.71726448433413026, -2.638427012816827677 ) ) ;
#36521 = ORIENTED_EDGE ( 'NONE', *, *, #59631, .F. ) ;
#36522 = B_SPLINE_CURVE_WITH_KNOTS ( 'NONE', 3,
 ( #13183, #97208, #44162, #74672, #6182, #67174 ),
 .UNSPECIFIED., .F., .F.,
 ( 4, 2, 4 ),
 ( 0.000000000000000000, 0.0002565770811490990168, 0.0005131541622981980336 ),
 .UNSPECIFIED. ) ;
#36523 = MECHANICAL_DESIGN_GEOMETRIC_PRESENTATION_REPRESENTATION (  '', ( #2998 ), #41318 ) ;
#36524 = CARTESIAN_POINT ( 'NONE',  ( -0.8801773607110991993, 7.855352010821504471, -2.915334737309923874 ) ) ;
#36525 = CARTESIAN_POINT ( 'NONE',  ( 13.43411237798105340, 0.5819680032637533085, 12.81628187352647963 ) ) ;
#36527 = ADVANCED_FACE ( 'NONE', ( #26448 ), #18513, .T. ) ;
#36526 = FACE_OUTER_BOUND ( 'NONE', #4021, .T. ) ;
#36528 = TOROIDAL_SURFACE ( 'NONE', #92399, 14.49999999999999822, 0.5000000000000000000 ) ;
#36529 = CARTESIAN_POINT ( 'NONE',  ( 0.1532563361054083140, 6.008931151000784787, 1.131784320476157264E-15 ) ) ;
#36530 = B_SPLINE_CURVE_WITH_KNOTS ( 'NONE', 3,
 ( #58370, #59861, #44369, #29358, #90348, #88398 ),
 .UNSPECIFIED., .F., .F.,
 ( 4, 2, 4 ),
 ( 0.0002800364959418003225, 0.0006862420824208872745, 0.001092447668899974335 ),
 .UNSPECIFIED. ) ;
#36531 = CARTESIAN_POINT ( 'NONE',  ( 12.63842701281683922, 49.55059781766744464, -9.846743663894590881 ) ) ;
#36532 = CARTESIAN_POINT ( 'NONE',  ( 2.035157376598822676, 42.43868534415483396, -7.964842623401177768 ) ) ;
#36533 = CARTESIAN_POINT ( 'NONE',  ( 10.00000000000000178, 10.37363466993041961, 12.81628187352647608 ) ) ;
#36535 = CARTESIAN_POINT ( 'NONE',  ( 11.92686044187656869, 10.37045670184114599, -3.195792623639533758 ) ) ;
#36534 = CARTESIAN_POINT ( 'NONE',  ( 17.96484262340118221, 51.18868534415483396, -7.964842623401177768 ) ) ;
#36536 = CARTESIAN_POINT ( 'NONE',  ( 2.831191079880678085, 79.91181047996344944, -9.500000000000000000 ) ) ;
#36537 = CARTESIAN_POINT ( 'NONE',  ( 16.40814093676323893, 50.79030133659708923, 11.09922568453595026 ) ) ;
#36538 = ORIENTED_EDGE ( 'NONE', *, *, #61077, .T. ) ;
#36539 = CARTESIAN_POINT ( 'NONE',  ( 7.084665262690076126, 62.02201867748816966, -10.88017736071110164 ) ) ;
#36541 = CARTESIAN_POINT ( 'NONE',  ( -4.164238869374099927, 2.012082168247300906, 3.795296366450308767 ) ) ;
#36540 = CARTESIAN_POINT ( 'NONE',  ( 21.09922568453594849, 31.20696800326375353, 6.408140936763242479 ) ) ;
#36542 = CARTESIAN_POINT ( 'NONE',  ( -16.94000000000001549, 92.00000000000000000, 9.500000000000000000 ) ) ;
#36543 = CARTESIAN_POINT ( 'NONE',  ( 15.44008868035555260, 39.73035201082150536, 9.422509992056143702 ) ) ;
#36544 = CARTESIAN_POINT ( 'NONE',  ( -0.1503990784575328643, 15.12777174578612538, 6.262539305110068177 ) ) ;
#36545 = CARTESIAN_POINT ( 'NONE',  ( 7.361572987183170547, 57.05059781766744464, 9.846743663894590881 ) ) ;
#36546 = CARTESIAN_POINT ( 'NONE',  ( 14.92337183194729633, 12.67559781766745353, 8.527530157486181039 ) ) ;
#36547 = CARTESIAN_POINT ( 'NONE',  ( 7.361572987183169658, 9.967264484334119601, -9.846743663894592657 ) ) ;
#36548 = CARTESIAN_POINT ( 'NONE',  ( 2.917880565312948704, 42.63708216824729647, 12.26659068614894643 ) ) ;
#36549 = CARTESIAN_POINT ( 'NONE',  ( 6.090257717040610252, 15.00000000000000533, -13.29726560978568806 ) ) ;
#36550 = CARTESIAN_POINT ( 'NONE',  ( 9.730224124549700093, -19.64066503251600793, -3.750000000000000444 ) ) ;
#36551 = CARTESIAN_POINT ( 'NONE',  ( 19.67858290521088449, 88.19818180006032549, -5.461713021790604472 ) ) ;
#36552 = EDGE_LOOP ( 'NONE', ( #62152, #63128, #28101, #65531 ) ) ;
#36553 = CARTESIAN_POINT ( 'NONE',  ( 24.16423886937410614, 64.51208216824728936, -3.795296366450302550 ) ) ;
#36554 = CARTESIAN_POINT ( 'NONE',  ( 2.917880565312948704, 57.63708216824731068, 12.26659068614894643 ) ) ;
#36555 = CARTESIAN_POINT ( 'NONE',  ( 17.20831665107776587, 32.88393115100078745, 7.208316651077764980 ) ) ;
#36556 = CARTESIAN_POINT ( 'NONE',  ( 19.38216949554541202, 25.99863466993042138, 9.382169495545424454 ) ) ;
#36557 = FACE_OUTER_BOUND ( 'NONE', #53134, .T. ) ;
#36559 = CARTESIAN_POINT ( 'NONE',  ( 2.917880565312948704, 2.637082168247300906, 12.26659068614894643 ) ) ;
#36558 = CARTESIAN_POINT ( 'NONE',  ( -5.149999999999996803, 98.49999999999998579, 8.000000000000000000 ) ) ;
#36560 = CARTESIAN_POINT ( 'NONE',  ( -0.8801773607111008646, 8.272018677488171434, 2.915334737309923430 ) ) ;
#36561 = CARTESIAN_POINT ( 'NONE',  ( -2.266590686148945544, 56.38708216824731068, -7.082119434687050408 ) ) ;
#36562 = CARTESIAN_POINT ( 'NONE',  ( 17.20831665107776587, 24.13393115100078035, -7.208316651077762316 ) ) ;
#36563 =( BOUNDED_SURFACE ( )  B_SPLINE_SURFACE ( 1, 2, ( 
 ( #62678, #85690, #71185, #47180, #63167, #3180, #46698, #86675, #25691, #41190, #39219, #77196, #10675, #17210, #70695, #47687, #2214, #8702, #93178, #1719, #71670, #69705, #70200, #32673, #78180, #1235, #31690, #32175, #18180, #62180, #24704, #86187, #48168, #92690, #2710, #33161, #48660, #24215, #43624, #88627, #57145, #73123, #36120, #79662, #97157, #19647, #28129, #4665, #87642, #35127, #3675, #19156, #20136, #95138, #65626, #96151, #50139, #80648, #49635, #73622, #12142, #74110, #96650, #66628, #66121, #28625, #50640, #5145, #11158, #81129, #26649, #42647, #95651, #27634, #80143, #72631, #51128, #11653, #42168, #58629, #35635, #27135, #58119, #4163, #59112, #12631, #43130, #18673, #89127, #41678, #20639, #65130, #5644, #49159, #81618, #34631, #13127, #57639, #88134, #72147, #34137, #64629, #52120, #98135, #22126, #14637, #7630, #68118, #75111, #53101, #8107, #29596, #61092, #45100, #60098, #22622, #75607, #83611, #37622, #69101, #82114, #37131, #76099, #52607, #44106, #51635, #59612, #21634, #14130, #74617, #90109, #82614, #46105, #6131, #13624, #91602, #76589, #97645, #67120, #83108, #7118, #38121, #29109, #98644, #30093, #15126, #6617, #44615, #23118, #45601, #53590, #38602, #635, #60600, #68609, #31083, #30587, #67626, #91095, #90599, #36637, #138, #84104, #15620, #89622, #21134, #40075, #2103, #33051, #55060, #69590, #48547, #54567, #92574, #1608, #62067, #93064, #41071, #31572, #85578, #32057, #24098, #32562, #54082, #16096, #1110, #70576, #92089, #55575, #10074, #56070, #85083, #39596, #18068, #63547, #16591, #63060, #17092, #47068, #70084, #79047, #71566, #9082, #62560, #94056, #25578, #77566, #71072, #84598, #46583, #24595, #40575, #47574, #10560, #86565, #78070, #9575, #93558, #25092, #2597, #86073, #17585, #48050, #3078, #78564, #61578, #23617, #77081, #8592, #39099, #34027, #89017, #87046, #94543, #35518, #20526, #41572, #11052, #95538, #57527, #50523, #72039, #88022, #27028, #65513, #19049, #3569, #66009, #27519, #96537, #51011, #81505, #65010, #20023, #13010, #73507, #64524, #12033, #95029, #18557, #79553, #26538, #81020, #49049, #19535, #42531, #73015, #5031, #50031, #57034, #43507, #87536, #49526, #72522, #80033, #80534, #74005, #11538, #4548, #4056, #42059, #35012, #26061, #34517, #96035, #58010, #64031, #88520, #12522, #28012, #43024, #58508, #33536, #56551, #67008, #76839, #30847, #13514, #15382, #24356, #85330, #53350, #45867, #77326, #8839, #97529, #16351, #97039, #28514, #43995, #84844, #76357, #54819, #31823, #83858, #7872, #397, #84367, #54329, #31333, #38367, #61833, #92827, #23866, #16844 ),
 ( #39353, #46833, #53857, #47318, #92341, #8353, #15866, #69847, #74497, #1371, #68866, #61345, #69350, #22879, #91856, #62320, #6020, #23371, #5530, #36010, #66512, #36516, #46351, #59008, #89511, #21021, #38861, #51510, #874, #30346, #82002, #60853, #91352, #48797, #55323, #25820, #63788, #10322, #40824, #47814, #33773, #71324, #34268, #56794, #26785, #26294, #57283, #10814, #64280, #39835, #41333, #85829, #2842, #55826, #33297, #17344, #32807, #11295, #78314, #9834, #18809, #94792, #86320, #94297, #40335, #87777, #56317, #71805, #19293, #86813, #70341, #79306, #25342, #64770, #77818, #18317, #70838, #87289, #2351, #63303, #93812, #9333, #17825, #48306, #49292, #3310, #78814, #1859, #79793, #41815, #62820, #72282, #3812, #95284, #32315, #93318, #24840, #59250, #96789, #90243, #36266, #20775, #58760, #66761, #88276, #51764, #12768, #73759, #13264, #65764, #88768, #74245, #50265, #66255, #6263, #49780, #89750, #28758, #44251, #42294, #97787, #13763, #58252, #5290, #50776, #43264, #67260, #96291, #4791, #82248, #74754, #80781, #35767, #20279, #80286, #11786, #19777, #21267, #34776, #42785, #12278, #73270, #36768, #28265, #89264, #81268, #51266, #29250, #81750, #43756, #97284, #35268, #59746, #5777, #72766, #4302, #27768, #65262, #95791, #27272, #57771, #77216, #21774, #61711, #763, #16236, #14270, #69727, #84730, #30228, #45748, #22757, #15267, #39239, #68260, #75740, #54213, #46716, #22267, #76244, #91233, #62204, #52253, #60246, #31216, #6759, #14771, #52740, #90739, #8721, #7760, #61231, #53239, #60732, #1254, #91737, #83249, #38253, #31709, #82749, #44744, #83743, #92227, #68745, #45244, #277, #37273, #7261, #23258, #98281, #30724, #53733, #84252, #15754, #37763, #76725, #46239, #75246, #23753, #67762, #69241, #29736, #8244, #38741, #98780, #25711, #70223, #86206, #70719, #55709, #1742, #47706, #26189, #62697, #32196, #33666, #10699, #2235, #17717, #55200, #72169, #48190, #56204, #34157, #78703, #85224, #94182, #40212, #49179, #41698, #71208, #93198, #3203, #17229, #24724, #85714, #3696, #78200, #9712, #64163, #2730, #32693, #92710, #94681, #86697, #77705, #10212, #18203, #48682, #33185, #24236, #56681, #87172, #40704, #54703, #79185, #63677, #63190, #93695, #79680, #47204, #16727, #18695, #11178, #25230, #41213, #71691, #9217, #39729, #4184, #20154, #27650, #96668, #50156, #34655, #66647, #58645, #97171, #82129, #13638, #96167, #51148, #44123, #5661, #95669, #43147, #27155, #19174, #11675, #57656, #81634, #49654, #58137, #73636, #5164, #36143, #88646, #72649, #51649, #88153, #19667, #4681, #65150, #50657, #74633 ) ),
 .UNSPECIFIED., .F., .F., .F. ) 
 B_SPLINE_SURFACE_WITH_KNOTS ( ( 2, 2 ),
 ( 3, 2, 2, 2, 2, 2, 2, 2, 2, 2, 2, 2, 2, 2, 2, 2, 2, 2, 2, 2, 2, 2, 2, 2, 2, 2, 2, 2, 2, 2, 2, 2, 2, 2, 2, 2, 2, 2, 2, 2, 2, 2, 2, 2, 2, 2, 2, 2, 2, 2, 2, 2, 2, 2, 2, 2, 2, 2, 2, 2, 2, 2, 2, 2, 2, 2, 2, 2, 2, 2, 2, 2, 2, 2, 2, 2, 2, 2, 2, 2, 2, 2, 2, 2, 2, 2, 2, 2, 2, 2, 2, 2, 2, 2, 2, 2, 2, 2, 2, 2, 2, 2, 2, 2, 2, 2, 2, 2, 2, 2, 2, 2, 2, 2, 2, 2, 2, 2, 2, 2, 2, 2, 2, 2, 2, 2, 2, 2, 2, 2, 2, 2, 2, 2, 2, 2, 2, 2, 2, 2, 2, 2, 2, 2, 2, 2, 2, 2, 2, 2, 2, 2, 2, 2, 2, 2, 2, 2, 2, 2, 2, 2, 3 ),
 ( 0.000000000000000000, 1.000000000000000000 ),
 ( 0.000000000000000000, 0.005952380952380952051, 0.01190476190476190410, 0.01785714285714285615, 0.02380952380952380820, 0.02976190476190476025, 0.03571428571428571230, 0.04166666666666666435, 0.04761904761904761640, 0.05357142857142856845, 0.05952380952380952051, 0.06547619047619047949, 0.07142857142857142461, 0.07738095238095238360, 0.08333333333333332871, 0.08928571428571428770, 0.09523809523809523281, 0.1011904761904761918, 0.1071428571428571369, 0.1130952380952380959, 0.1190476190476190410, 0.1250000000000000000, 0.1309523809523809590, 0.1369047619047619180, 0.1428571428571428492, 0.1488095238095238082, 0.1547619047619047672, 0.1607142857142857262, 0.1666666666666666574, 0.1726190476190476164, 0.1785714285714285754, 0.1845238095238095344, 0.1904761904761904656, 0.1964285714285714246, 0.2023809523809523836, 0.2083333333333333426, 0.2142857142857142738, 0.2202380952380952328, 0.2261904761904761918, 0.2321428571428571508, 0.2380952380952380820, 0.2440476190476190410, 0.2500000000000000000, 0.2559523809523809312, 0.2619047619047619180, 0.2678571428571428492, 0.2738095238095238360, 0.2797619047619047672, 0.2857142857142856984, 0.2916666666666666852, 0.2976190476190476164, 0.3035714285714285476, 0.3095238095238095344, 0.3154761904761904656, 0.3214285714285714524, 0.3273809523809523836, 0.3333333333333333148, 0.3392857142857143016, 0.3452380952380952328, 0.3511904761904761640, 0.3571428571428571508, 0.3630952380952380820, 0.3690476190476190688, 0.3750000000000000000, 0.3809523809523809312, 0.3869047619047619180, 0.3928571428571428492, 0.3988095238095238360, 0.4047619047619047672, 0.4107142857142856984, 0.4166666666666666852, 0.4226190476190476164, 0.4285714285714285476, 0.4345238095238095344, 0.4404761904761904656, 0.4464285714285714524, 0.4523809523809523836, 0.4583333333333333148, 0.4642857142857143016, 0.4702380952380952328, 0.4761904761904761640, 0.4821428571428571508, 0.4880952380952380820, 0.4940476190476190688, 0.5000000000000000000, 0.5059523809523809312, 0.5119047619047618625, 0.5178571428571429047, 0.5238095238095238360, 0.5297619047619047672, 0.5357142857142856984, 0.5416666666666666297, 0.5476190476190476719, 0.5535714285714286031, 0.5595238095238095344, 0.5654761904761904656, 0.5714285714285713969, 0.5773809523809523281, 0.5833333333333333703, 0.5892857142857143016, 0.5952380952380952328, 0.6011904761904761640, 0.6071428571428570953, 0.6130952380952381375, 0.6190476190476190688, 0.6250000000000000000, 0.6309523809523809312, 0.6369047619047618625, 0.6428571428571429047, 0.6488095238095238360, 0.6547619047619047672, 0.6607142857142856984, 0.6666666666666666297, 0.6726190476190476719, 0.6785714285714286031, 0.6845238095238095344, 0.6904761904761904656, 0.6964285714285713969, 0.7023809523809523281, 0.7083333333333333703, 0.7142857142857143016, 0.7202380952380952328, 0.7261904761904761640, 0.7321428571428570953, 0.7380952380952381375, 0.7440476190476190688, 0.7500000000000000000, 0.7559523809523809312, 0.7619047619047618625, 0.7678571428571429047, 0.7738095238095238360, 0.7797619047619047672, 0.7857142857142856984, 0.7916666666666666297, 0.7976190476190476719, 0.8035714285714286031, 0.8095238095238095344, 0.8154761904761904656, 0.8214285714285713969, 0.8273809523809523281, 0.8333333333333333703, 0.8392857142857143016, 0.8452380952380952328, 0.8511904761904761640, 0.8571428571428570953, 0.8630952380952381375, 0.8690476190476190688, 0.8750000000000000000, 0.8809523809523809312, 0.8869047619047618625, 0.8928571428571429047, 0.8988095238095238360, 0.9047619047619047672, 0.9107142857142856984, 0.9166666666666666297, 0.9226190476190476719, 0.9285714285714286031, 0.9345238095238095344, 0.9404761904761904656, 0.9464285714285713969, 0.9523809523809523281, 0.9583333333333333703, 0.9642857142857143016 ),
 .UNSPECIFIED. ) 
 GEOMETRIC_REPRESENTATION_ITEM ( )  RATIONAL_B_SPLINE_SURFACE ( (
 ( 1.000000000000000000, 0.9659258262890683122, 1.000000000000000000, 0.9659258262890683122, 1.000000000000000000, 0.9659258262890683122, 1.000000000000000000, 0.9659258262890683122, 1.000000000000000000, 0.9659258262890683122, 1.000000000000000000, 0.9659258262890683122, 1.000000000000000000, 0.9659258262890683122, 1.000000000000000000, 0.9659258262890683122, 1.000000000000000000, 0.9659258262890683122, 1.000000000000000000, 0.9659258262890683122, 1.000000000000000000, 0.9659258262890683122, 1.000000000000000000, 0.9659258262890683122, 1.000000000000000000, 0.9659258262890683122, 1.000000000000000000, 0.9659258262890683122, 1.000000000000000000, 0.9659258262890683122, 1.000000000000000000, 0.9659258262890683122, 1.000000000000000000, 0.9659258262890683122, 1.000000000000000000, 0.9659258262890683122, 1.000000000000000000, 0.9659258262890683122, 1.000000000000000000, 0.9659258262890683122, 1.000000000000000000, 0.9659258262890683122, 1.000000000000000000, 0.9659258262890683122, 1.000000000000000000, 0.9659258262890683122, 1.000000000000000000, 0.9659258262890683122, 1.000000000000000000, 0.9659258262890683122, 1.000000000000000000, 0.9659258262890683122, 1.000000000000000000, 0.9659258262890683122, 1.000000000000000000, 0.9659258262890683122, 1.000000000000000000, 0.9659258262890683122, 1.000000000000000000, 0.9659258262890683122, 1.000000000000000000, 0.9659258262890683122, 1.000000000000000000, 0.9659258262890683122, 1.000000000000000000, 0.9659258262890683122, 1.000000000000000000, 0.9659258262890683122, 1.000000000000000000, 0.9659258262890683122, 1.000000000000000000, 0.9659258262890683122, 1.000000000000000000, 0.9659258262890683122, 1.000000000000000000, 0.9659258262890683122, 1.000000000000000000, 0.9659258262890683122, 1.000000000000000000, 0.9659258262890683122, 1.000000000000000000, 0.9659258262890683122, 1.000000000000000000, 0.9659258262890683122, 1.000000000000000000, 0.9659258262890683122, 1.000000000000000000, 0.9659258262890683122, 1.000000000000000000, 0.9659258262890683122, 1.000000000000000000, 0.9659258262890683122, 1.000000000000000000, 0.9659258262890683122, 1.000000000000000000, 0.9659258262890683122, 1.000000000000000000, 0.9659258262890683122, 1.000000000000000000, 0.9659258262890683122, 1.000000000000000000, 0.9659258262890683122, 1.000000000000000000, 0.9659258262890683122, 1.000000000000000000, 0.9659258262890683122, 1.000000000000000000, 0.9659258262890683122, 1.000000000000000000, 0.9659258262890683122, 1.000000000000000000, 0.9659258262890683122, 1.000000000000000000, 0.9659258262890683122, 1.000000000000000000, 0.9659258262890683122, 1.000000000000000000, 0.9659258262890683122, 1.000000000000000000, 0.9659258262890683122, 1.000000000000000000, 0.9659258262890683122, 1.000000000000000000, 0.9659258262890683122, 1.000000000000000000, 0.9659258262890683122, 1.000000000000000000, 0.9659258262890683122, 1.000000000000000000, 0.9659258262890683122, 1.000000000000000000, 0.9659258262890683122, 1.000000000000000000, 0.9659258262890683122, 1.000000000000000000, 0.9659258262890683122, 1.000000000000000000, 0.9659258262890683122, 1.000000000000000000, 0.9659258262890683122, 1.000000000000000000, 0.9659258262890683122, 1.000000000000000000, 0.9659258262890683122, 1.000000000000000000, 0.9659258262890683122, 1.000000000000000000, 0.9659258262890683122, 1.000000000000000000, 0.9659258262890683122, 1.000000000000000000, 0.9659258262890683122, 1.000000000000000000, 0.9659258262890683122, 1.000000000000000000, 0.9659258262890683122, 1.000000000000000000, 0.9659258262890683122, 1.000000000000000000, 0.9659258262890683122, 1.000000000000000000, 0.9659258262890683122, 1.000000000000000000, 0.9659258262890683122, 1.000000000000000000, 0.9659258262890683122, 1.000000000000000000, 0.9659258262890683122, 1.000000000000000000, 0.9659258262890683122, 1.000000000000000000, 0.9659258262890683122, 1.000000000000000000, 0.9659258262890683122, 1.000000000000000000, 0.9659258262890683122, 1.000000000000000000, 0.9659258262890683122, 1.000000000000000000, 0.9659258262890683122, 1.000000000000000000, 0.9659258262890683122, 1.000000000000000000, 0.9659258262890683122, 1.000000000000000000, 0.9659258262890683122, 1.000000000000000000, 0.9659258262890683122, 1.000000000000000000, 0.9659258262890683122, 1.000000000000000000, 0.9659258262890683122, 1.000000000000000000, 0.9659258262890683122, 1.000000000000000000, 0.9659258262890683122, 1.000000000000000000, 0.9659258262890683122, 1.000000000000000000, 0.9659258262890683122, 1.000000000000000000, 0.9659258262890683122, 1.000000000000000000, 0.9659258262890683122, 1.000000000000000000, 0.9659258262890683122, 1.000000000000000000, 0.9659258262890683122, 1.000000000000000000, 0.9659258262890683122, 1.000000000000000000, 0.9659258262890683122, 1.000000000000000000, 0.9659258262890683122, 1.000000000000000000, 0.9659258262890683122, 1.000000000000000000, 0.9659258262890683122, 1.000000000000000000, 0.9659258262890683122, 1.000000000000000000, 0.9659258262890683122, 1.000000000000000000, 0.9659258262890683122, 1.000000000000000000, 0.9659258262890683122, 1.000000000000000000, 0.9659258262890683122, 1.000000000000000000, 0.9659258262890683122, 1.000000000000000000, 0.9659258262890683122, 1.000000000000000000, 0.9659258262890683122, 1.000000000000000000, 0.9659258262890683122, 1.000000000000000000, 0.9659258262890683122, 1.000000000000000000, 0.9659258262890683122, 1.000000000000000000, 0.9659258262890683122, 1.000000000000000000, 0.9659258262890683122, 1.000000000000000000, 0.9659258262890683122, 1.000000000000000000, 0.9659258262890683122, 1.000000000000000000, 0.9659258262890683122, 1.000000000000000000, 0.9659258262890683122, 1.000000000000000000, 0.9659258262890683122, 1.000000000000000000, 0.9659258262890683122, 1.000000000000000000, 0.9659258262890683122, 1.000000000000000000, 0.9659258262890683122, 1.000000000000000000, 0.9659258262890683122, 1.000000000000000000, 0.9659258262890683122, 1.000000000000000000, 0.9659258262890683122, 1.000000000000000000, 0.9659258262890683122, 1.000000000000000000, 0.9659258262890683122, 1.000000000000000000, 0.9659258262890683122, 1.000000000000000000, 0.9659258262890683122, 1.000000000000000000, 0.9659258262890683122, 1.000000000000000000, 0.9659258262890683122, 1.000000000000000000, 0.9659258262890683122, 1.000000000000000000, 0.9659258262890683122, 1.000000000000000000, 0.9659258262890683122, 1.000000000000000000, 0.9659258262890683122, 1.000000000000000000, 0.9659258262890683122, 1.000000000000000000, 0.9659258262890683122, 1.000000000000000000, 0.9659258262890683122, 1.000000000000000000, 0.9659258262890683122, 1.000000000000000000, 0.9659258262890683122, 1.000000000000000000, 0.9659258262890683122, 1.000000000000000000, 0.9659258262890683122, 1.000000000000000000, 0.9659258262890683122, 1.000000000000000000, 0.9659258262890683122, 1.000000000000000000, 0.9659258262890683122, 1.000000000000000000, 0.9659258262890683122, 1.000000000000000000, 0.9659258262890683122, 1.000000000000000000, 0.9659258262890683122, 1.000000000000000000, 0.9659258262890683122, 1.000000000000000000, 0.9659258262890683122, 1.000000000000000000, 0.9659258262890683122, 1.000000000000000000, 0.9659258262890683122, 1.000000000000000000, 0.9659258262890683122, 1.000000000000000000, 0.9659258262890683122, 1.000000000000000000),
 ( 1.000000000000000000, 0.9659258262890683122, 1.000000000000000000, 0.9659258262890683122, 1.000000000000000000, 0.9659258262890683122, 1.000000000000000000, 0.9659258262890683122, 1.000000000000000000, 0.9659258262890683122, 1.000000000000000000, 0.9659258262890683122, 1.000000000000000000, 0.9659258262890683122, 1.000000000000000000, 0.9659258262890683122, 1.000000000000000000, 0.9659258262890683122, 1.000000000000000000, 0.9659258262890683122, 1.000000000000000000, 0.9659258262890683122, 1.000000000000000000, 0.9659258262890683122, 1.000000000000000000, 0.9659258262890683122, 1.000000000000000000, 0.9659258262890683122, 1.000000000000000000, 0.9659258262890683122, 1.000000000000000000, 0.9659258262890683122, 1.000000000000000000, 0.9659258262890683122, 1.000000000000000000, 0.9659258262890683122, 1.000000000000000000, 0.9659258262890683122, 1.000000000000000000, 0.9659258262890683122, 1.000000000000000000, 0.9659258262890683122, 1.000000000000000000, 0.9659258262890683122, 1.000000000000000000, 0.9659258262890683122, 1.000000000000000000, 0.9659258262890683122, 1.000000000000000000, 0.9659258262890683122, 1.000000000000000000, 0.9659258262890683122, 1.000000000000000000, 0.9659258262890683122, 1.000000000000000000, 0.9659258262890683122, 1.000000000000000000, 0.9659258262890683122, 1.000000000000000000, 0.9659258262890683122, 1.000000000000000000, 0.9659258262890683122, 1.000000000000000000, 0.9659258262890683122, 1.000000000000000000, 0.9659258262890683122, 1.000000000000000000, 0.9659258262890683122, 1.000000000000000000, 0.9659258262890683122, 1.000000000000000000, 0.9659258262890683122, 1.000000000000000000, 0.9659258262890683122, 1.000000000000000000, 0.9659258262890683122, 1.000000000000000000, 0.9659258262890683122, 1.000000000000000000, 0.9659258262890683122, 1.000000000000000000, 0.9659258262890683122, 1.000000000000000000, 0.9659258262890683122, 1.000000000000000000, 0.9659258262890683122, 1.000000000000000000, 0.9659258262890683122, 1.000000000000000000, 0.9659258262890683122, 1.000000000000000000, 0.9659258262890683122, 1.000000000000000000, 0.9659258262890683122, 1.000000000000000000, 0.9659258262890683122, 1.000000000000000000, 0.9659258262890683122, 1.000000000000000000, 0.9659258262890683122, 1.000000000000000000, 0.9659258262890683122, 1.000000000000000000, 0.9659258262890683122, 1.000000000000000000, 0.9659258262890683122, 1.000000000000000000, 0.9659258262890683122, 1.000000000000000000, 0.9659258262890683122, 1.000000000000000000, 0.9659258262890683122, 1.000000000000000000, 0.9659258262890683122, 1.000000000000000000, 0.9659258262890683122, 1.000000000000000000, 0.9659258262890683122, 1.000000000000000000, 0.9659258262890683122, 1.000000000000000000, 0.9659258262890683122, 1.000000000000000000, 0.9659258262890683122, 1.000000000000000000, 0.9659258262890683122, 1.000000000000000000, 0.9659258262890683122, 1.000000000000000000, 0.9659258262890683122, 1.000000000000000000, 0.9659258262890683122, 1.000000000000000000, 0.9659258262890683122, 1.000000000000000000, 0.9659258262890683122, 1.000000000000000000, 0.9659258262890683122, 1.000000000000000000, 0.9659258262890683122, 1.000000000000000000, 0.9659258262890683122, 1.000000000000000000, 0.9659258262890683122, 1.000000000000000000, 0.9659258262890683122, 1.000000000000000000, 0.9659258262890683122, 1.000000000000000000, 0.9659258262890683122, 1.000000000000000000, 0.9659258262890683122, 1.000000000000000000, 0.9659258262890683122, 1.000000000000000000, 0.9659258262890683122, 1.000000000000000000, 0.9659258262890683122, 1.000000000000000000, 0.9659258262890683122, 1.000000000000000000, 0.9659258262890683122, 1.000000000000000000, 0.9659258262890683122, 1.000000000000000000, 0.9659258262890683122, 1.000000000000000000, 0.9659258262890683122, 1.000000000000000000, 0.9659258262890683122, 1.000000000000000000, 0.9659258262890683122, 1.000000000000000000, 0.9659258262890683122, 1.000000000000000000, 0.9659258262890683122, 1.000000000000000000, 0.9659258262890683122, 1.000000000000000000, 0.9659258262890683122, 1.000000000000000000, 0.9659258262890683122, 1.000000000000000000, 0.9659258262890683122, 1.000000000000000000, 0.9659258262890683122, 1.000000000000000000, 0.9659258262890683122, 1.000000000000000000, 0.9659258262890683122, 1.000000000000000000, 0.9659258262890683122, 1.000000000000000000, 0.9659258262890683122, 1.000000000000000000, 0.9659258262890683122, 1.000000000000000000, 0.9659258262890683122, 1.000000000000000000, 0.9659258262890683122, 1.000000000000000000, 0.9659258262890683122, 1.000000000000000000, 0.9659258262890683122, 1.000000000000000000, 0.9659258262890683122, 1.000000000000000000, 0.9659258262890683122, 1.000000000000000000, 0.9659258262890683122, 1.000000000000000000, 0.9659258262890683122, 1.000000000000000000, 0.9659258262890683122, 1.000000000000000000, 0.9659258262890683122, 1.000000000000000000, 0.9659258262890683122, 1.000000000000000000, 0.9659258262890683122, 1.000000000000000000, 0.9659258262890683122, 1.000000000000000000, 0.9659258262890683122, 1.000000000000000000, 0.9659258262890683122, 1.000000000000000000, 0.9659258262890683122, 1.000000000000000000, 0.9659258262890683122, 1.000000000000000000, 0.9659258262890683122, 1.000000000000000000, 0.9659258262890683122, 1.000000000000000000, 0.9659258262890683122, 1.000000000000000000, 0.9659258262890683122, 1.000000000000000000, 0.9659258262890683122, 1.000000000000000000, 0.9659258262890683122, 1.000000000000000000, 0.9659258262890683122, 1.000000000000000000, 0.9659258262890683122, 1.000000000000000000, 0.9659258262890683122, 1.000000000000000000, 0.9659258262890683122, 1.000000000000000000, 0.9659258262890683122, 1.000000000000000000, 0.9659258262890683122, 1.000000000000000000, 0.9659258262890683122, 1.000000000000000000, 0.9659258262890683122, 1.000000000000000000, 0.9659258262890683122, 1.000000000000000000, 0.9659258262890683122, 1.000000000000000000, 0.9659258262890683122, 1.000000000000000000, 0.9659258262890683122, 1.000000000000000000, 0.9659258262890683122, 1.000000000000000000, 0.9659258262890683122, 1.000000000000000000, 0.9659258262890683122, 1.000000000000000000, 0.9659258262890683122, 1.000000000000000000, 0.9659258262890683122, 1.000000000000000000, 0.9659258262890683122, 1.000000000000000000, 0.9659258262890683122, 1.000000000000000000, 0.9659258262890683122, 1.000000000000000000, 0.9659258262890683122, 1.000000000000000000, 0.9659258262890683122, 1.000000000000000000, 0.9659258262890683122, 1.000000000000000000, 0.9659258262890683122, 1.000000000000000000, 0.9659258262890683122, 1.000000000000000000, 0.9659258262890683122, 1.000000000000000000, 0.9659258262890683122, 1.000000000000000000, 0.9659258262890683122, 1.000000000000000000, 0.9659258262890683122, 1.000000000000000000, 0.9659258262890683122, 1.000000000000000000, 0.9659258262890683122, 1.000000000000000000, 0.9659258262890683122, 1.000000000000000000, 0.9659258262890683122, 1.000000000000000000, 0.9659258262890683122, 1.000000000000000000, 0.9659258262890683122, 1.000000000000000000, 0.9659258262890683122, 1.000000000000000000, 0.9659258262890683122, 1.000000000000000000, 0.9659258262890683122, 1.000000000000000000, 0.9659258262890683122, 1.000000000000000000, 0.9659258262890683122, 1.000000000000000000, 0.9659258262890683122, 1.000000000000000000) ) ) 
 REPRESENTATION_ITEM ( '' )  SURFACE ( )  );
#36564 = CARTESIAN_POINT ( 'NONE',  ( 12.80781515976314822, -0.03417435944610275333, -6.246788841744324472 ) ) ;
#36565 = CARTESIAN_POINT ( 'NONE',  ( 0.1532563361054082862, 11.21726448433411605, 2.638427012816831674 ) ) ;
#36566 = CARTESIAN_POINT ( 'NONE',  ( 18.17829156368505750, 59.16792564121895026, 6.500000000000043521 ) ) ;
#36567 = CARTESIAN_POINT ( 'NONE',  ( 2.638427012816829897, 19.55059781766745175, -9.846743663894592657 ) ) ;
#36568 = ORIENTED_EDGE ( 'NONE', *, *, #57583, .F. ) ;
#36569 = ORIENTED_EDGE ( 'NONE', *, *, #2134, .T. ) ;
#36570 = CARTESIAN_POINT ( 'NONE',  ( 1.354709868695649577, 14.49999999999999112, -14.93870011653157448 ) ) ;
#36571 = ORIENTED_EDGE ( 'NONE', *, *, #93681, .F. ) ;
#36572 = CARTESIAN_POINT ( 'NONE',  ( 1.472469842513823179, 45.59226448433412315, -4.923371831947296329 ) ) ;
#36573 = CARTESIAN_POINT ( 'NONE',  ( 10.00000000000000000, 20.55374883491396787, -14.16423886937410082 ) ) ;
#36575 = CARTESIAN_POINT ( 'NONE',  ( 20.88017736071110164, 30.35535201082151247, 2.915334737309930979 ) ) ;
#36574 = CARTESIAN_POINT ( 'NONE',  ( 17.96484262340118221, 24.93868534415484461, 7.964842623401181321 ) ) ;
#36577 = CARTESIAN_POINT ( 'NONE',  ( 13.43411237798105340, 15.58196800326374998, 12.81628187352647963 ) ) ;
#36576 = CARTESIAN_POINT ( 'NONE',  ( 0.1532563361054083140, 61.00893115100078745, 1.131784320476157264E-15 ) ) ;
#36578 = EDGE_CURVE ( 'NONE', #68087, #8055, #81913, .T. ) ;
#36579 = CARTESIAN_POINT ( 'NONE',  ( 20.88017736071110519, 65.56368534415483396, 2.639326808657452039E-16 ) ) ;
#36580 = CARTESIAN_POINT ( 'NONE',  ( 13.43411237798106583, 32.66530133659708213, -12.81628187352647252 ) ) ;
#36581 = ORIENTED_EDGE ( 'NONE', *, *, #57670, .T. ) ;
#36582 = CARTESIAN_POINT ( 'NONE',  ( 18.52753015748617571, 28.09226448433411960, 4.923371831947298993 ) ) ;
#36583 = CARTESIAN_POINT ( 'NONE',  ( -0.8801773607111008646, 8.272018677488171434, 2.915334737309923430 ) ) ;
#36584 = VERTEX_POINT ( 'NONE', #41487 ) ;
#36585 = CARTESIAN_POINT ( 'NONE',  ( 7.771322705631503069, 4.156677014937179135E-16, -12.24159072199917375 ) ) ;
#36586 = CARTESIAN_POINT ( 'NONE',  ( 19.42250999205614548, 5.980352010821504471, -5.440088680355545492 ) ) ;
#36587 = VERTEX_POINT ( 'NONE', #26944 ) ;
#36588 = CARTESIAN_POINT ( 'NONE',  ( 7.084665262690076126, 54.10535201082151247, 10.88017736071109987 ) ) ;
#36589 = CARTESIAN_POINT ( 'NONE',  ( 0.5774900079438607392, 63.48035201082149825, 5.440088680355550821 ) ) ;
#36590 = PRESENTATION_LAYER_ASSIGNMENT (  '', '', ( #94029 ) ) ;
#36591 = CARTESIAN_POINT ( 'NONE',  ( 20.88017736071110164, 55.35535201082149825, 2.915334737309930979 ) ) ;
#36592 = DIRECTION ( 'NONE',  ( 1.000000000000000000, -1.244644646440729013E-15, 0.000000000000000000 ) ) ;
#36593 = ADVANCED_FACE ( 'NONE', ( #71956 ), #57445, .F. ) ;
#36594 = CARTESIAN_POINT ( 'NONE',  ( 7.084665262690076126, 59.10535201082150536, 10.88017736071109987 ) ) ;
#36595 = CARTESIAN_POINT ( 'NONE',  ( -46.94000000000001904, 100.7935499705848486, 8.437539667958747103 ) ) ;
#36596 = AXIS2_PLACEMENT_3D ( 'NONE', #23055, #59058, #97584 ) ;
#36597 = AXIS2_PLACEMENT_3D ( 'NONE', #45194, #66714, #5727 ) ;
#36598 = EDGE_CURVE ( 'NONE', #94453, #36109, #1683, .T. ) ;
#36599 = CARTESIAN_POINT ( 'NONE',  ( 18.52753015748618282, 23.92559781766745530, -4.923371831947291888 ) ) ;
#36600 = ORIENTED_EDGE ( 'NONE', *, *, #30041, .F. ) ;
#36601 = CARTESIAN_POINT ( 'NONE',  ( 19.84674366389459266, 53.30059781766744464, 2.638427012816836559 ) ) ;
#36603 = EDGE_CURVE ( 'NONE', #26702, #91250, #18303, .T. ) ;
#36602 = CARTESIAN_POINT ( 'NONE',  ( 0.000000000000000000, 14.49999999999999822, 0.000000000000000000 ) ) ;
#36604 = CARTESIAN_POINT ( 'NONE',  ( 17.08211943468705130, 8.470415501580635720, 12.26659068614894998 ) ) ;
#36605 = ORIENTED_EDGE ( 'NONE', *, *, #75923, .F. ) ;
#36606 = CARTESIAN_POINT ( 'NONE',  ( -10.65450226470440676, 12.60126542628704627, -3.926157240590227193 ) ) ;
#36607 = CARTESIAN_POINT ( 'NONE',  ( 14.43100913236850502, 4.664102659404345836E-16, -1.412789942453164693 ) ) ;
#36609 = CARTESIAN_POINT ( 'NONE',  ( 19.84674366389459266, 38.30059781766745175, 2.638427012816836559 ) ) ;
#36608 = CARTESIAN_POINT ( 'NONE',  ( 4.469999999999999751, 10.00000000000000000, 4.000000000000000000 ) ) ;
#36610 = CARTESIAN_POINT ( 'NONE',  ( 12.91533473730993009, 11.60535201082150714, -10.88017736071109987 ) ) ;
#36611 = DIRECTION ( 'NONE',  ( 0.000000000000000000, 1.000000000000000000, 0.000000000000000000 ) ) ;
#36612 = EDGE_LOOP ( 'NONE', ( #72801, #83848, #9252, #46614 ) ) ;
#36613 = CARTESIAN_POINT ( 'NONE',  ( 2.831191079880678085, 79.91181047996344944, 9.500000000000000000 ) ) ;
#36614 = CARTESIAN_POINT ( 'NONE',  ( 10.00000000000000178, 52.25893115100078745, 9.846743663894594434 ) ) ;
#36615 = FACE_OUTER_BOUND ( 'NONE', #460, .T. ) ;
#36616 = CARTESIAN_POINT ( 'NONE',  ( 10.00000000000000000, 17.87363466993041783, -12.81628187352647608 ) ) ;
#36617 = CARTESIAN_POINT ( 'NONE',  ( 19.84674366389459266, 8.300597817667451750, 2.638427012816836559 ) ) ;
#36618 = COLOUR_RGB ( '', 0.31764706, 0.68627451, 0.89019608) ;
#36619 = CARTESIAN_POINT ( 'NONE',  ( 0.5069705099446313312, 0.4330826616539849572, 6.500000000000002665 ) ) ;
#36620 = CARTESIAN_POINT ( 'NONE',  ( 0.6178305044545838731, 4.748634669930420493, 9.382169495545420901 ) ) ;
#36621 = CARTESIAN_POINT ( 'NONE',  ( -9.000000000000001776, 80.99999999999994316, 0.000000000000000000 ) ) ;
#36622 = EDGE_CURVE ( 'NONE', #18004, #91280, #82768, .T. ) ;
#36623 = ADVANCED_FACE ( 'NONE', ( #21929 ), #5742, .T. ) ;
#36624 = ORIENTED_EDGE ( 'NONE', *, *, #3671, .F. ) ;
#36625 = CARTESIAN_POINT ( 'NONE',  ( 4.559911319644449179, 13.89701867748817321, 9.422509992056141925 ) ) ;
#36626 = CARTESIAN_POINT ( 'NONE',  ( 13.79529636645030344, 8.262082168247300018, 14.16423886937410614 ) ) ;
#36627 = CARTESIAN_POINT ( 'NONE',  ( 19.84674366389459621, 28.50893115100078745, 7.409399052514197653E-17 ) ) ;
#36628 = CARTESIAN_POINT ( 'NONE',  ( 4.559911319644449179, 57.23035201082150536, -9.422509992056141925 ) ) ;
#36629 = CARTESIAN_POINT ( 'NONE',  ( 0.6178305044545838731, 44.74863466993042493, 9.382169495545420901 ) ) ;
#36630 = CARTESIAN_POINT ( 'NONE',  ( 20.88017736071110875, 20.77201867748816611, -2.915334737309920765 ) ) ;
#36631 = EDGE_CURVE ( 'NONE', #35160, #57591, #53694, .T. ) ;
#36632 = CARTESIAN_POINT ( 'NONE',  ( -9.065164099344372062, 14.49999999999999822, -11.95084933600779742 ) ) ;
#36633 = LINE ( 'NONE', #47443, #95103 ) ;
#36634 = AXIS2_PLACEMENT_3D ( 'NONE', #4074, #27541, #43048 ) ;
#36635 = CARTESIAN_POINT ( 'NONE',  ( 22.81628187352648496, 1.831968003263753753, -3.434112377981050290 ) ) ;
#36636 = CARTESIAN_POINT ( 'NONE',  ( 12.63842701281683034, 62.46726448433410894, 9.846743663894596210 ) ) ;
#36637 = CARTESIAN_POINT ( 'NONE',  ( 18.52753015748617571, 33.09226448433411605, 4.923371831947298993 ) ) ;
#36638 = CARTESIAN_POINT ( 'NONE',  ( 7.964842623401181321, -5.061314655845157162, 7.964842623401174215 ) ) ;
#36639 = CARTESIAN_POINT ( 'NONE',  ( 16.40814093676324603, 37.45696800326376064, -11.09922568453594671 ) ) ;
#36641 = CARTESIAN_POINT ( 'NONE',  ( 14.91937968691864747, 0.2306972965111891982, 0.8063277559919165283 ) ) ;
#36640 = CARTESIAN_POINT ( 'NONE',  ( 19.42250999205614548, 45.98035201082150536, -5.440088680355545492 ) ) ;
#36642 = CARTESIAN_POINT ( 'NONE',  ( 12.91533473730993009, 36.60535201082151247, -10.88017736071109987 ) ) ;
#36643 = CARTESIAN_POINT ( 'NONE',  ( 4.559911319644449179, 27.23035201082150536, -9.422509992056141925 ) ) ;
#36644 = CARTESIAN_POINT ( 'NONE',  ( 0.1532563361054083140, 66.00893115100079456, 1.131784320476157264E-15 ) ) ;
#36645 = CARTESIAN_POINT ( 'NONE',  ( 19.42250999205614193, 60.14701867748817676, 5.440088680355555262 ) ) ;
#36646 = CARTESIAN_POINT ( 'NONE',  ( 2.791683348922240793, 41.63393115100078745, 7.208316651077764092 ) ) ;
#36647 = CARTESIAN_POINT ( 'NONE',  ( 17.96484262340118221, 14.93868534415483751, 7.964842623401181321 ) ) ;
#36648 = CARTESIAN_POINT ( 'NONE',  ( 22.81628187352647785, 16.62363466993042138, 6.195893100308588602E-16 ) ) ;
#36649 = ORIENTED_EDGE ( 'NONE', *, *, #77270, .T. ) ;
#36650 = CARTESIAN_POINT ( 'NONE',  ( -0.8801773607111008646, 23.27201867748817676, 2.915334737309923430 ) ) ;
#36651 = B_SPLINE_CURVE_WITH_KNOTS ( 'NONE', 3,
 ( #14267, #38737, #275, #54211, #83246, #52251 ),
 .UNSPECIFIED., .F., .F.,
 ( 4, 2, 4 ),
 ( 0.0002800338592536502809, 0.0006862394199285692942, 0.001092444980603488307 ),
 .UNSPECIFIED. ) ;
#36652 = CARTESIAN_POINT ( 'NONE',  ( 18.18329248733322245, 7.602906685120198738, 6.499999999999993783 ) ) ;
#36653 = CARTESIAN_POINT ( 'NONE',  ( 10.00000000000000000, 1.813685344154837731, -10.88017736071110342 ) ) ;
#36654 = CARTESIAN_POINT ( 'NONE',  ( 20.88017736071110519, 15.56368534415483751, 2.639326808657452039E-16 ) ) ;
#36655 = CARTESIAN_POINT ( 'NONE',  ( 20.88017736071110164, 65.35535201082150536, 2.915334737309930979 ) ) ;
#36656 = CARTESIAN_POINT ( 'NONE',  ( 17.08211943468705130, 28.47041550158063572, 12.26659068614894998 ) ) ;
#36657 = CARTESIAN_POINT ( 'NONE',  ( 0.1532563361054083140, 16.00893115100078390, 1.131784320476157264E-15 ) ) ;
#36658 = CARTESIAN_POINT ( 'NONE',  ( 2.791683348922237240, 65.38393115100078035, -7.208316651077763204 ) ) ;
#36659 = CARTESIAN_POINT ( 'NONE',  ( -0.8801773607111009756, 48.06368534415484817, 1.068504757029289695E-15 ) ) ;
#36660 = LINE ( 'NONE', #89155, #54351 ) ;
#36661 = CARTESIAN_POINT ( 'NONE',  ( 20.88017736071110875, 25.77201867748816966, -2.915334737309920321 ) ) ;
#36662 = ORIENTED_EDGE ( 'NONE', *, *, #23665, .T. ) ;
#36663 = DIRECTION ( 'NONE',  ( 0.000000000000000000, 1.000000000000000000, 0.000000000000000000 ) ) ;
#36664 = CARTESIAN_POINT ( 'NONE',  ( 19.84674366389459266, 48.71726448433413026, -2.638427012816827677 ) ) ;
#36665 = ORIENTED_EDGE ( 'NONE', *, *, #72974, .T. ) ;
#36666 = ORIENTED_EDGE ( 'NONE', *, *, #62916, .F. ) ;
#36667 = CARTESIAN_POINT ( 'NONE',  ( -14.64885433385998326, 0.04922511925147129291, -1.748475581354406616 ) ) ;
#36668 = CARTESIAN_POINT ( 'NONE',  ( -0.3689425029237881626, 22.42874883491397142, 10.36894250292379027 ) ) ;
#36669 = CARTESIAN_POINT ( 'NONE',  ( -0.3689425029237898834, 26.17874883491396432, -10.36894250292378850 ) ) ;
#36670 = CARTESIAN_POINT ( 'NONE',  ( 15.44008868035555793, 56.39701867748817676, -9.422509992056140149 ) ) ;
#36671 = CARTESIAN_POINT ( 'NONE',  ( -0.8801773607111008646, 3.272018677488171434, 2.915334737309923430 ) ) ;
#36672 = CARTESIAN_POINT ( 'NONE',  ( -1.099225684535947600, 4.540301336597087456, 6.408140936763237150 ) ) ;
#36673 = CARTESIAN_POINT ( 'NONE',  ( 17.20831665107776587, 54.13393115100079456, -7.208316651077762316 ) ) ;
#36674 = CARTESIAN_POINT ( 'NONE',  ( -11.02874191901561041, -96.54482102870888127, 4.000000000000000000 ) ) ;
#36676 = CARTESIAN_POINT ( 'NONE',  ( 6.565887622018943937, 3.081968003263753531, -12.81628187352647608 ) ) ;
#36675 = CARTESIAN_POINT ( 'NONE',  ( -0.8801773607111008646, 43.27201867748817676, 2.915334737309923430 ) ) ;
#36677 = CARTESIAN_POINT ( 'NONE',  ( 6.204703633549690345, 20.76208216824730357, -14.16423886937410259 ) ) ;
#36678 = CARTESIAN_POINT ( 'NONE',  ( 19.42250999205614193, 20.14701867748817321, 5.440088680355555262 ) ) ;
#36679 = CARTESIAN_POINT ( 'NONE',  ( 0.5774900079438590739, 12.64701867748817321, -5.440088680355550821 ) ) ;
#36680 = CARTESIAN_POINT ( 'NONE',  ( 18.52753015748618282, 53.92559781766745175, -4.923371831947291888 ) ) ;
#36681 = CARTESIAN_POINT ( 'NONE',  ( 2.035157376598822676, 42.43868534415483396, -7.964842623401177768 ) ) ;
#36682 = VECTOR ( 'NONE', #44382, 1000.000000000000000 ) ;
#36683 = CARTESIAN_POINT ( 'NONE',  ( -2.638427012816840111, -30.03273551566588040, -9.846743663894590881 ) ) ;
#36684 = ORIENTED_EDGE ( 'NONE', *, *, #40889, .T. ) ;
#36685 = CARTESIAN_POINT ( 'NONE',  ( 0.3093388210927642268, 14.49999999999999822, -14.99680997725065978 ) ) ;
#36686 = ORIENTED_EDGE ( 'NONE', *, *, #70683, .T. ) ;
#36687 = CARTESIAN_POINT ( 'NONE',  ( 0.1532563361054100626, 30.80059781766744820, -2.638427012816831230 ) ) ;
#36688 = AXIS2_PLACEMENT_3D ( 'NONE', #96851, #79366, #10873 ) ;
#36689 = ORIENTED_EDGE ( 'NONE', *, *, #98608, .F. ) ;
#36690 = DIRECTION ( 'NONE',  ( 0.000000000000000000, 0.7071067811865465735, 0.7071067811865485719 ) ) ;
#36692 = CARTESIAN_POINT ( 'NONE',  ( -0.8801773607110991993, 2.855352010821504471, -2.915334737309923874 ) ) ;
#36691 = CARTESIAN_POINT ( 'NONE',  ( 13.79529636645030344, 43.26208216824730357, 14.16423886937410614 ) ) ;
#36694 = CARTESIAN_POINT ( 'NONE',  ( 2.791683348922237240, 50.38393115100078035, -7.208316651077763204 ) ) ;
#36693 = CARTESIAN_POINT ( 'NONE',  ( 19.84674366389459266, 28.71726448433411960, -2.638427012816827677 ) ) ;
#36695 = DIRECTION ( 'NONE',  ( 0.000000000000000000, 1.000000000000000000, 0.000000000000000000 ) ) ;
#36696 = ADVANCED_FACE ( 'NONE', ( #82406 ), #60396, .T. ) ;
#36697 = AXIS2_PLACEMENT_3D ( 'NONE', #68516, #46978, #91505 ) ;
#36698 = DIRECTION ( 'NONE',  ( -1.000000000000000000, 0.000000000000000000, 0.000000000000000000 ) ) ;
#36699 = CARTESIAN_POINT ( 'NONE',  ( 19.84674366389459621, 3.508931151000785231, 7.409399052514197653E-17 ) ) ;
#36700 = CARTESIAN_POINT ( 'NONE',  ( -5.204170427930421283E-15, 27.87363466993042493, -12.81628187352647608 ) ) ;
#36701 = ORIENTED_EDGE ( 'NONE', *, *, #21603, .F. ) ;
#36702 = CARTESIAN_POINT ( 'NONE',  ( 17.08211943468705840, 35.13708216824730357, -12.26659068614894466 ) ) ;
#36703 = CARTESIAN_POINT ( 'NONE',  ( 13.43411237798106583, 27.66530133659708568, -12.81628187352647252 ) ) ;
#36704 = ORIENTED_EDGE ( 'NONE', *, *, #8830, .T. ) ;
#36705 = CARTESIAN_POINT ( 'NONE',  ( 21.09922568453595559, 42.04030133659708213, -6.408140936763230044 ) ) ;
#36706 = CARTESIAN_POINT ( 'NONE',  ( 12.63842701281683922, 39.55059781766744464, -9.846743663894590881 ) ) ;
#36707 = CARTESIAN_POINT ( 'NONE',  ( 20.88017736071110164, 10.35535201082150714, 2.915334737309930979 ) ) ;
#36708 = CARTESIAN_POINT ( 'NONE',  ( 14.48718990079892066, 15.00000000000000000, 0.6093675230841449908 ) ) ;
#36709 = CARTESIAN_POINT ( 'NONE',  ( 7.361572987183170547, 47.05059781766745175, 9.846743663894590881 ) ) ;
#36710 = CARTESIAN_POINT ( 'NONE',  ( 12.63842701281683034, 52.46726448433413026, 9.846743663894596210 ) ) ;
#36712 = EDGE_LOOP ( 'NONE', ( #64899, #1758, #48040, #14703 ) ) ;
#36711 = CARTESIAN_POINT ( 'NONE',  ( 6.898461952320432466, 4.226027835726576547E-16, -12.75387089053309175 ) ) ;
#36713 = ADVANCED_FACE ( 'NONE', ( #44408 ), #61605, .F. ) ;
#36714 = CIRCLE ( 'NONE', #92586, 3.250000000000002665 ) ;
#36715 = B_SPLINE_CURVE_WITH_KNOTS ( 'NONE', 3,
 ( #38939, #69428, #54410, #474, #53429, #67958 ),
 .UNSPECIFIED., .F., .F.,
 ( 4, 2, 4 ),
 ( 4.906538933386797396E-18, 0.0002605067024380951332, 0.0005210134048761852791 ),
 .UNSPECIFIED. ) ;
#36716 = CARTESIAN_POINT ( 'NONE',  ( -0.3093388210927753845, 0.3625444014373740975, -14.99680997725068821 ) ) ;
#36717 = DIRECTION ( 'NONE',  ( -0.000000000000000000, -0.000000000000000000, -1.000000000000000000 ) ) ;
#36718 = DIRECTION ( 'NONE',  ( -0.000000000000000000, 1.000000000000000000, -0.000000000000000000 ) ) ;
#36719 = SURFACE_STYLE_USAGE ( .BOTH. , #6215 ) ;
#36720 = CARTESIAN_POINT ( 'NONE',  ( 10.00000000000000000, 14.75893115100078568, -9.846743663894594434 ) ) ;
#36721 = EDGE_CURVE ( 'NONE', #87224, #54365, #37146, .T. ) ;
#36722 = CARTESIAN_POINT ( 'NONE',  ( 22.81628187352648496, 41.83196800326375353, -3.434112377981050290 ) ) ;
#36723 = CARTESIAN_POINT ( 'NONE',  ( -3.750000000000000000, 10.25000000000000000, -2.750000000000000000 ) ) ;
#36724 = ORIENTED_EDGE ( 'NONE', *, *, #4446, .F. ) ;
#36725 = CARTESIAN_POINT ( 'NONE',  ( 17.20831665107776587, 54.13393115100079456, -7.208316651077762316 ) ) ;
#36726 = CARTESIAN_POINT ( 'NONE',  ( -14.49440716394874151, 3.911302179139366829E-16, 0.4026921475165256004 ) ) ;
#36727 = CARTESIAN_POINT ( 'NONE',  ( 20.36894250292379382, 33.67874883491396076, 10.36894250292379205 ) ) ;
#36728 = CARTESIAN_POINT ( 'NONE',  ( 19.84674366389459621, 43.50893115100078745, 7.409399052514197653E-17 ) ) ;
#36729 = CARTESIAN_POINT ( 'NONE',  ( 19.38216949554541202, 50.99863466993042493, 9.382169495545424454 ) ) ;
#36731 = CARTESIAN_POINT ( 'NONE',  ( 0.2751277870542980231, 9.366073187301308778, -6.500000000000002665 ) ) ;
#36730 = DIRECTION ( 'NONE',  ( 0.000000000000000000, -0.000000000000000000, -1.000000000000000000 ) ) ;
#36732 = CARTESIAN_POINT ( 'NONE',  ( 14.92337183194729988, 4.342264484334117824, -8.527530157486177487 ) ) ;
#36733 = CARTESIAN_POINT ( 'NONE',  ( -0.1503990784575247319, 67.22266099184919597, -6.262539305110083276 ) ) ;
#36734 = CARTESIAN_POINT ( 'NONE',  ( 12.63842701281683922, 49.55059781766744464, -9.846743663894590881 ) ) ;
#36735 = CARTESIAN_POINT ( 'NONE',  ( 19.42250999205614548, 40.98035201082150536, -5.440088680355545492 ) ) ;
#36736 = CARTESIAN_POINT ( 'NONE',  ( 14.92337183194729988, 29.34226448433411960, -8.527530157486177487 ) ) ;
#36737 = CARTESIAN_POINT ( 'NONE',  ( 20.88017736071110519, 45.56368534415484106, 2.639326808657452039E-16 ) ) ;
#36738 = ADVANCED_FACE ( 'NONE', ( #30387 ), #15427, .F. ) ;
#36739 = ORIENTED_EDGE ( 'NONE', *, *, #55802, .F. ) ;
#36740 = CARTESIAN_POINT ( 'NONE',  ( -5.625000000000007994, 4.284700295649321866, -9.742785792574931492 ) ) ;
#36741 = CARTESIAN_POINT ( 'NONE',  ( 2.035157376598822676, 17.43868534415483751, -7.964842623401177768 ) ) ;
#36743 = CARTESIAN_POINT ( 'NONE',  ( 0.5774900079438607392, 43.48035201082151247, 5.440088680355550821 ) ) ;
#36742 = CARTESIAN_POINT ( 'NONE',  ( 10.00000000000000178, 52.25893115100078745, 9.846743663894594434 ) ) ;
#36744 = FILL_AREA_STYLE ('',( #52231 ) ) ;
#36745 = CARTESIAN_POINT ( 'NONE',  ( 12.91533473730992121, 64.52201867748817676, 10.88017736071110164 ) ) ;
#36747 = AXIS2_PLACEMENT_3D ( 'NONE', #87299, #86329, #25829 ) ;
#36746 = FACE_OUTER_BOUND ( 'NONE', #74800, .T. ) ;
#36749 = CARTESIAN_POINT ( 'NONE',  ( 64.56412365047462742, 26.99999999999999645, 9.500000000000000000 ) ) ;
#36748 = CARTESIAN_POINT ( 'NONE',  ( 2.035157376598824452, 28.68868534415484106, 7.964842623401179544 ) ) ;
#36750 = CARTESIAN_POINT ( 'NONE',  ( 7.361572987183170547, 7.050597817667451750, 9.846743663894590881 ) ) ;
#36751 = CARTESIAN_POINT ( 'NONE',  ( 5.076628168052704559, 20.17559781766745175, -8.527530157486179263 ) ) ;
#36752 = CARTESIAN_POINT ( 'NONE',  ( 1.847340224724751456, 0.04922511925147066841, 14.63671528203493288 ) ) ;
#36753 = CARTESIAN_POINT ( 'NONE',  ( -7.082119434687058401, 15.97041550158064638, -12.26659068614894110 ) ) ;
#36754 = CARTESIAN_POINT ( 'NONE',  ( 1.472469842513823179, 65.59226448433412315, -4.923371831947296329 ) ) ;
#36755 = CARTESIAN_POINT ( 'NONE',  ( 10.00000000000000178, 4.313685344154837509, 10.88017736071110342 ) ) ;
#36756 = CARTESIAN_POINT ( 'NONE',  ( -10.19513985507841980, 0.3639309290920410001, 11.00268709613213503 ) ) ;
#36757 = CARTESIAN_POINT ( 'NONE',  ( 22.26659068614895176, 4.720415501580633943, -7.082119434687042414 ) ) ;
#36758 = CARTESIAN_POINT ( 'NONE',  ( 17.08211943468705840, 45.13708216824730357, -12.26659068614894466 ) ) ;
#36759 = CARTESIAN_POINT ( 'NONE',  ( 0.6178305044545818747, 8.498634669930421381, -9.382169495545419124 ) ) ;
#36760 = ORIENTED_EDGE ( 'NONE', *, *, #33525, .T. ) ;
#36761 = CARTESIAN_POINT ( 'NONE',  ( 5.076628168052704559, 15.17559781766745175, -8.527530157486179263 ) ) ;
#36762 = CARTESIAN_POINT ( 'NONE',  ( -0.8801773607111008646, 13.27201867748817321, 2.915334737309923430 ) ) ;
#36763 = CARTESIAN_POINT ( 'NONE',  ( 0.1532563361054083140, 46.00893115100079456, 1.131784320476157264E-15 ) ) ;
#36765 = DIRECTION ( 'NONE',  ( 0.000000000000000000, 0.000000000000000000, 1.000000000000000000 ) ) ;
#36764 = CARTESIAN_POINT ( 'NONE',  ( 2.120353041430538266, 15.00000000000000000, 14.34413130794944635 ) ) ;
#36766 = LINE ( 'NONE', #81266, #24472 ) ;
#36767 = CARTESIAN_POINT ( 'NONE',  ( 7.361572987183169658, -0.03273551566588185635, -9.846743663894592657 ) ) ;
#36768 = CARTESIAN_POINT ( 'NONE',  ( 16.40814093676324603, 27.45696800326375708, -11.09922568453594671 ) ) ;
#36769 = CARTESIAN_POINT ( 'NONE',  ( 5.076628168052703671, 21.84226448433411960, 8.527530157486179263 ) ) ;
#36770 = ORIENTED_EDGE ( 'NONE', *, *, #35332, .T. ) ;
#36771 = CARTESIAN_POINT ( 'NONE',  ( 7.361572987183170547, 12.05059781766744997, 9.846743663894590881 ) ) ;
#36772 = CARTESIAN_POINT ( 'NONE',  ( 9.729335482426746395, -19.62342160288699588, -3.750000000000000000 ) ) ;
#36773 = CARTESIAN_POINT ( 'NONE',  ( -14.56372689393802311, 14.95037103587093874, 2.356940382831874015 ) ) ;
#36774 = CARTESIAN_POINT ( 'NONE',  ( 19.42250999205614548, 10.98035201082150358, -5.440088680355545492 ) ) ;
#36775 = CARTESIAN_POINT ( 'NONE',  ( 6.204703633549690345, 35.76208216824729647, -14.16423886937410259 ) ) ;
#36776 = CARTESIAN_POINT ( 'NONE',  ( 15.44008868035555793, 41.39701867748817676, -9.422509992056140149 ) ) ;
#36777 = CARTESIAN_POINT ( 'NONE',  ( 12.91533473730992121, 59.52201867748816966, 10.88017736071110164 ) ) ;
#36778 = AXIS2_PLACEMENT_3D ( 'NONE', #4773, #5270, #27252 ) ;
#36779 = PRESENTATION_STYLE_ASSIGNMENT (( #74255 ) ) ;
#36780 = CARTESIAN_POINT ( 'NONE',  ( 2.791683348922237240, 25.38393115100078390, -7.208316651077763204 ) ) ;
#36781 = CARTESIAN_POINT ( 'NONE',  ( 7.084665262690076126, 9.105352010821503583, 10.88017736071109987 ) ) ;
#36782 = CARTESIAN_POINT ( 'NONE',  ( 5.076628168052704559, 10.17559781766745175, -8.527530157486179263 ) ) ;
#36783 = CARTESIAN_POINT ( 'NONE',  ( 0.5636945946910000282, 8.154255672638645939E-15, -5.268011858241770540 ) ) ;
#36784 = CARTESIAN_POINT ( 'NONE',  ( 14.92337183194729633, 42.67559781766745886, 8.527530157486181039 ) ) ;
#36785 = CARTESIAN_POINT ( 'NONE',  ( -0.8801773607111009756, 38.06368534415484106, 1.068504757029289695E-15 ) ) ;
#36786 = ORIENTED_EDGE ( 'NONE', *, *, #66771, .T. ) ;
#36787 = CARTESIAN_POINT ( 'NONE',  ( -2.816281873526471635, 53.91530133659709634, -3.434112377981056508 ) ) ;
#36788 = DIRECTION ( 'NONE',  ( 0.3826834323650877279, 0.000000000000000000, 0.9238795325112876267 ) ) ;
#36789 = CARTESIAN_POINT ( 'NONE',  ( 0.1532563361054082862, 6.217264484334118713, 2.638427012816831674 ) ) ;
#36790 = CARTESIAN_POINT ( 'NONE',  ( 21.09922568453595559, 47.04030133659708923, -6.408140936763230044 ) ) ;
#36792 = CARTESIAN_POINT ( 'NONE',  ( 14.92337183194729633, 37.67559781766745175, 8.527530157486181039 ) ) ;
#36791 = CARTESIAN_POINT ( 'NONE',  ( 15.44008868035555260, 9.730352010821505360, 9.422509992056143702 ) ) ;
#36793 = DIRECTION ( 'NONE',  ( -0.000000000000000000, -1.000000000000000000, -0.000000000000000000 ) ) ;
#36794 = CARTESIAN_POINT ( 'NONE',  ( -2.266590686148945544, 17.22041550158063572, 7.082119434687048631 ) ) ;
#36795 = CARTESIAN_POINT ( 'NONE',  ( 24.16423886937410614, 39.51208216824731068, -3.795296366450302550 ) ) ;
#36796 = CARTESIAN_POINT ( 'NONE',  ( 19.84674366389459621, 38.50893115100078745, 7.409399052514197653E-17 ) ) ;
#36797 = DIRECTION ( 'NONE',  ( -0.9961946980917459893, 0.08715574274765408580, -0.000000000000000000 ) ) ;
#36798 = CARTESIAN_POINT ( 'NONE',  ( 12.91533473730992121, 34.52201867748817676, 10.88017736071110164 ) ) ;
#36799 = CARTESIAN_POINT ( 'NONE',  ( 4.559911319644449179, 68.89701867748817676, 9.422509992056141925 ) ) ;
#36800 = CARTESIAN_POINT ( 'NONE',  ( -3.628626191893843167, -3.642031182898128439, 3.749999999999596323 ) ) ;
#36801 = VERTEX_POINT ( 'NONE', #54908 ) ;
#36802 = CARTESIAN_POINT ( 'NONE',  ( -2.816281873526473856, 54.12363466993041783, 9.499525473075851096E-16 ) ) ;
#36803 = CARTESIAN_POINT ( 'NONE',  ( 4.559911319644449179, 63.89701867748817676, 9.422509992056141925 ) ) ;
#36804 = ORIENTED_EDGE ( 'NONE', *, *, #14144, .T. ) ;
#36805 = CARTESIAN_POINT ( 'NONE',  ( 6.204703633549690345, 10.76208216824729824, -14.16423886937410259 ) ) ;
#36806 = CARTESIAN_POINT ( 'NONE',  ( 1.472469842513823179, 10.59226448433411782, -4.923371831947296329 ) ) ;
#36807 = EDGE_CURVE ( 'NONE', #46091, #25626, #49379, .T. ) ;
#36808 = CARTESIAN_POINT ( 'NONE',  ( 1.197528957823066786, 8.576208590949788468E-17, -6.052460312987175683 ) ) ;
#36809 = ORIENTED_EDGE ( 'NONE', *, *, #60105, .T. ) ;
#36810 =( BOUNDED_CURVE ( )  B_SPLINE_CURVE ( 2, ( #2943, #49390, #40930, #79890, #63889, #10423, #34877, #65371, #86904 ),
 .UNSPECIFIED., .F., .T. ) 
 B_SPLINE_CURVE_WITH_KNOTS ( ( 3, 2, 2, 2, 3 ),
 ( 0.3677146600783225971, 0.3690476190476190688, 0.3750000000000000000, 0.3809523809523809312, 0.3822853399216774029 ),
 .UNSPECIFIED. ) 
 CURVE ( )  GEOMETRIC_REPRESENTATION_ITEM ( )  RATIONAL_B_SPLINE_CURVE ( ( 0.9881565478350731180, 0.9923695281211488695, 1.000000000000000000, 0.9659258262890683122, 1.000000000000000000, 0.9659258262890683122, 1.000000000000000000, 0.9923695281211488695, 0.9881565478350731180 ) ) 
 REPRESENTATION_ITEM ( '' )  );
#36811 = MECHANICAL_DESIGN_GEOMETRIC_PRESENTATION_REPRESENTATION (  '', ( #33568 ), #88 ) ;
#36812 = CARTESIAN_POINT ( 'NONE',  ( 10.00000000000000000, 11.81368534415483751, -10.88017736071110342 ) ) ;
#36813 = ORIENTED_EDGE ( 'NONE', *, *, #58991, .F. ) ;
#36814 = CARTESIAN_POINT ( 'NONE',  ( 19.42250999205614548, 40.98035201082150536, -5.440088680355545492 ) ) ;
#36815 = VECTOR ( 'NONE', #69969, 1000.000000000000000 ) ;
#36816 = EDGE_LOOP ( 'NONE', ( #97843, #73101, #86473, #30460 ) ) ;
#36817 = VECTOR ( 'NONE', #82517, 1000.000000000000000 ) ;
#36818 = CARTESIAN_POINT ( 'NONE',  ( 16.40814093676323893, 10.79030133659708923, 11.09922568453595026 ) ) ;
#36819 = ORIENTED_EDGE ( 'NONE', *, *, #67334, .T. ) ;
#36820 = CARTESIAN_POINT ( 'NONE',  ( 17.96484262340118221, 61.18868534415482685, -7.964842623401177768 ) ) ;
#36821 = CARTESIAN_POINT ( 'NONE',  ( 10.00000000000000178, 67.25893115100079456, 9.846743663894594434 ) ) ;
#36823 = DIRECTION ( 'NONE',  ( -0.9099612708765455471, 0.000000000000000000, 0.4146932426562339180 ) ) ;
#36822 = CARTESIAN_POINT ( 'NONE',  ( 15.44008868035555793, 16.39701867748817321, -9.422509992056140149 ) ) ;
#36824 = CARTESIAN_POINT ( 'NONE',  ( 0.5774900079438607392, 68.48035201082150536, 5.440088680355550821 ) ) ;
#36825 = AXIS2_PLACEMENT_3D ( 'NONE', #28205, #58701, #81693 ) ;
#36826 = CARTESIAN_POINT ( 'NONE',  ( 10.00000000000000178, 14.31368534415483929, 10.88017736071110342 ) ) ;
#36827 = ORIENTED_EDGE ( 'NONE', *, *, #57066, .T. ) ;
#36828 = EDGE_CURVE ( 'NONE', #96626, #67947, #67184, .T. ) ;
#36829 = CARTESIAN_POINT ( 'NONE',  ( -1.099225684535947600, 59.54030133659708923, 6.408140936763237150 ) ) ;
#36830 = CARTESIAN_POINT ( 'NONE',  ( 17.96484262340118221, 49.93868534415484106, 7.964842623401181321 ) ) ;
#36831 = CARTESIAN_POINT ( 'NONE',  ( 14.71525861348291464, 14.63606890215477918, 2.908807992686703425 ) ) ;
#36832 = B_SPLINE_CURVE_WITH_KNOTS ( 'NONE', 3,
 ( #22550, #6542, #76518, #53020, #83535, #15054 ),
 .UNSPECIFIED., .F., .F.,
 ( 4, 2, 4 ),
 ( 0.0002800015744541034719, 0.0006862068192693090464, 0.001092412064084514675 ),
 .UNSPECIFIED. ) ;
#36833 = CARTESIAN_POINT ( 'NONE',  ( 22.81628187352648496, 51.83196800326376064, -3.434112377981050290 ) ) ;
#36834 = CARTESIAN_POINT ( 'NONE',  ( 4.559911319644449179, 43.89701867748816966, 9.422509992056141925 ) ) ;
#36835 = CARTESIAN_POINT ( 'NONE',  ( -1.099225684535947600, -1.293031996736246469, -6.408140936763238038 ) ) ;
#36836 = DIRECTION ( 'NONE',  ( 0.000000000000000000, 0.000000000000000000, -1.000000000000000000 ) ) ;
#36837 = B_SPLINE_CURVE_WITH_KNOTS ( 'NONE', 3,
 ( #70159, #4980, #11980, #80480 ),
 .UNSPECIFIED., .F., .F.,
 ( 4, 4 ),
 ( 3.291406376790657244E-17, 0.001060528352562001547 ),
 .UNSPECIFIED. ) ;
#36838 = CIRCLE ( 'NONE', #71950, 15.00000000000000000 ) ;
#36839 = CARTESIAN_POINT ( 'NONE',  ( 7.361572987183169658, 19.96726448433411960, -9.846743663894592657 ) ) ;
#36840 = CARTESIAN_POINT ( 'NONE',  ( -1.099225684535947600, 8.706968003263753531, -6.408140936763238038 ) ) ;
#36842 = CARTESIAN_POINT ( 'NONE',  ( 5.076628168052703671, 66.84226448433412315, 8.527530157486179263 ) ) ;
#36841 = DIRECTION ( 'NONE',  ( 0.000000000000000000, 1.000000000000000000, -0.000000000000000000 ) ) ;
#36843 = CARTESIAN_POINT ( 'NONE',  ( 19.42250999205614548, 40.98035201082150536, -5.440088680355545492 ) ) ;
#36844 = CIRCLE ( 'NONE', #30479, 2.000000000000000888 ) ;
#36845 = DIRECTION ( 'NONE',  ( 1.000000000000000000, 0.000000000000000000, 0.000000000000000000 ) ) ;
#36846 = CARTESIAN_POINT ( 'NONE',  ( 10.00000000000000178, 7.258931151000785675, 9.846743663894594434 ) ) ;
#36848 = ORIENTED_EDGE ( 'NONE', *, *, #90779, .T. ) ;
#36847 = CARTESIAN_POINT ( 'NONE',  ( -2.816281873526471635, 3.915301336597087456, -3.434112377981056508 ) ) ;
#36849 = CARTESIAN_POINT ( 'NONE',  ( -10.93781366033354274, 14.49999999999999822, 10.26470809774057891 ) ) ;
#36850 = CARTESIAN_POINT ( 'NONE',  ( 7.313705784284555200, 14.49999999999999112, 13.09617149020753146 ) ) ;
#36851 = CARTESIAN_POINT ( 'NONE',  ( 0.1532563361054083140, 61.00893115100078745, 1.131784320476157264E-15 ) ) ;
#36852 = CARTESIAN_POINT ( 'NONE',  ( 3.591859063236763294, 53.29030133659708923, -11.09922568453595026 ) ) ;
#36853 = CARTESIAN_POINT ( 'NONE',  ( 5.076628168052703671, 36.84226448433412315, 8.527530157486179263 ) ) ;
#36854 = CARTESIAN_POINT ( 'NONE',  ( 6.935134328218562239, -80.57830137102044432, -2.750000000000000444 ) ) ;
#36855 = CARTESIAN_POINT ( 'NONE',  ( 4.559911319644449179, 7.230352010821505360, -9.422509992056141925 ) ) ;
#36856 = CARTESIAN_POINT ( 'NONE',  ( 0.1532563361054083140, 36.00893115100078745, 1.131784320476157264E-15 ) ) ;
#36857 = DIRECTION ( 'NONE',  ( 0.5150380749100554878, 1.049727191138617710E-16, 0.8571673007021115565 ) ) ;
#36858 = CARTESIAN_POINT ( 'NONE',  ( 7.084665262690076126, 2.022018677488171434, -10.88017736071110164 ) ) ;
#36859 = CARTESIAN_POINT ( 'NONE',  ( 2.603489959281584998, 6.582109641433292246, 6.499999999999998224 ) ) ;
#36860 = CARTESIAN_POINT ( 'NONE',  ( 10.00000000000000178, 24.31368534415484106, 10.88017736071110342 ) ) ;
#36861 = CARTESIAN_POINT ( 'NONE',  ( -4.164238869374099039, 51.80374883491396787, 8.674139862899312516E-16 ) ) ;
#36863 = DIRECTION ( 'NONE',  ( 1.000000000000000000, 0.000000000000000000, 0.000000000000000000 ) ) ;
#36862 = CARTESIAN_POINT ( 'NONE',  ( -2.266590686148945544, 47.22041550158063927, 7.082119434687048631 ) ) ;
#36864 = CARTESIAN_POINT ( 'NONE',  ( -9.898881779040801021, 15.00000000000000000, 10.25059215482569641 ) ) ;
#36865 = EDGE_CURVE ( 'NONE', #24048, #1911, #48398, .T. ) ;
#36866 = CARTESIAN_POINT ( 'NONE',  ( 5.076628168052704559, 30.17559781766745175, -8.527530157486179263 ) ) ;
#36867 = CARTESIAN_POINT ( 'NONE',  ( 22.81628187352648496, 1.831968003263753753, -3.434112377981050290 ) ) ;
#36868 = ORIENTED_EDGE ( 'NONE', *, *, #38207, .F. ) ;
#36869 = FILL_AREA_STYLE_COLOUR ( '', #46478 ) ;
#36870 = EDGE_CURVE ( 'NONE', #10425, #94783, #23315, .T. ) ;
#36871 = CARTESIAN_POINT ( 'NONE',  ( 11.92686044187656513, 2.007122731651787007, 2.779367613825428407 ) ) ;
#36872 = DIRECTION ( 'NONE',  ( -0.000000000000000000, -0.000000000000000000, 1.000000000000000000 ) ) ;
#36873 = CARTESIAN_POINT ( 'NONE',  ( 2.917880565312948704, 12.63708216824730179, 12.26659068614894643 ) ) ;
#36874 = MECHANICAL_DESIGN_GEOMETRIC_PRESENTATION_REPRESENTATION (  '', ( #27290 ), #14550 ) ;
#36875 = CARTESIAN_POINT ( 'NONE',  ( 14.92337183194729633, 27.67559781766745530, 8.527530157486181039 ) ) ;
#36876 = SURFACE_SIDE_STYLE ('',( #6868 ) ) ;
#36877 = ORIENTED_EDGE ( 'NONE', *, *, #20069, .F. ) ;
#36878 = CARTESIAN_POINT ( 'NONE',  ( 22.26659068614895176, 39.72041550158063217, -7.082119434687042414 ) ) ;
#36879 = CARTESIAN_POINT ( 'NONE',  ( 2.791683348922240793, 11.63393115100078568, 7.208316651077764092 ) ) ;
#36880 = CARTESIAN_POINT ( 'NONE',  ( -7.037799270021981357, -86.25965645051654462, -2.749999999998791189 ) ) ;
#36881 = CARTESIAN_POINT ( 'NONE',  ( 7.084665262690076126, 27.02201867748817676, -10.88017736071110164 ) ) ;
#36882 = CARTESIAN_POINT ( 'NONE',  ( 3.591859063236763294, 38.29030133659708923, -11.09922568453595026 ) ) ;
#36883 = SURFACE_STYLE_USAGE ( .BOTH. , #89873 ) ;
#36884 = AXIS2_PLACEMENT_3D ( 'NONE', #65274, #64778, #56328 ) ;
#36885 = CARTESIAN_POINT ( 'NONE',  ( 13.43411237798105340, 30.58196800326374998, 12.81628187352647963 ) ) ;
#36886 = CARTESIAN_POINT ( 'NONE',  ( 10.00000000000000178, 65.37363466993042493, 12.81628187352647608 ) ) ;
#36887 = ORIENTED_EDGE ( 'NONE', *, *, #88268, .F. ) ;
#36888 = DIRECTION ( 'NONE',  ( -0.8870108331782244893, 0.000000000000000000, 0.4617486132350284156 ) ) ;
#36889 = EDGE_CURVE ( 'NONE', #1776, #45067, #33862, .T. ) ;
#36890 = CARTESIAN_POINT ( 'NONE',  ( 20.15039907845753575, 35.60158574516643171, -6.262539305110076171 ) ) ;
#36891 = CARTESIAN_POINT ( 'NONE',  ( 6.204703633549690345, 40.76208216824731778, -14.16423886937410259 ) ) ;
#36892 = CARTESIAN_POINT ( 'NONE',  ( -4.164238869374099927, 2.012082168247300906, 3.795296366450308767 ) ) ;
#36893 = CARTESIAN_POINT ( 'NONE',  ( 19.42250999205614548, 10.98035201082150358, -5.440088680355545492 ) ) ;
#36894 = CARTESIAN_POINT ( 'NONE',  ( 10.00000000000000000, 26.81368534415484106, -10.88017736071110342 ) ) ;
#36895 = CYLINDRICAL_SURFACE ( 'NONE', #49437, 15.00000000000000000 ) ;
#36896 = DIRECTION ( 'NONE',  ( -0.9426414910921759871, 0.000000000000000000, -0.3338068592337775642 ) ) ;
#36897 = CARTESIAN_POINT ( 'NONE',  ( 10.00000000000000178, 54.31368534415484106, 10.88017736071110342 ) ) ;
#36898 = CARTESIAN_POINT ( 'NONE',  ( 7.084665262690076126, 47.02201867748818387, -10.88017736071110164 ) ) ;
#36899 = CARTESIAN_POINT ( 'NONE',  ( 13.43411237798106583, 32.66530133659708213, -12.81628187352647252 ) ) ;
#36900 = CARTESIAN_POINT ( 'NONE',  ( 19.88701968852511826, 26.79427333184090898, 6.480634945678690251 ) ) ;
#36901 = CARTESIAN_POINT ( 'NONE',  ( 7.361572987183170547, 27.05059781766745175, 9.846743663894590881 ) ) ;
#36902 = CARTESIAN_POINT ( 'NONE',  ( 4.559911319644449179, 52.23035201082151247, -9.422509992056141925 ) ) ;
#36903 = CARTESIAN_POINT ( 'NONE',  ( 10.00000000000000000, 17.87363466993041783, -12.81628187352647608 ) ) ;
#36904 = DIRECTION ( 'NONE',  ( 0.04361938736533305799, -0.000000000000000000, 0.9990482215818579093 ) ) ;
#36905 = CARTESIAN_POINT ( 'NONE',  ( 0.5774900079438590739, 7.647018677488171434, -5.440088680355550821 ) ) ;
#36906 = CARTESIAN_POINT ( 'NONE',  ( 10.00000000000000178, 37.25893115100078745, 9.846743663894594434 ) ) ;
#36907 = CARTESIAN_POINT ( 'NONE',  ( 13.43411237798106583, 62.66530133659708923, -12.81628187352647252 ) ) ;
#36908 = CARTESIAN_POINT ( 'NONE',  ( 19.84674366389459621, 13.50893115100078568, 7.409399052514197653E-17 ) ) ;
#36909 = CARTESIAN_POINT ( 'NONE',  ( 24.16423886937410614, 9.303748834913967869, 8.672049930838204340E-16 ) ) ;
#36910 = CARTESIAN_POINT ( 'NONE',  ( 19.10478245763057714, 30.10160829253887371, 5.990408912944228170 ) ) ;
#36911 = CARTESIAN_POINT ( 'NONE',  ( 0.5774900079438607392, 38.48035201082150536, 5.440088680355550821 ) ) ;
#36912 = CARTESIAN_POINT ( 'NONE',  ( -0.8801773607110991993, 2.855352010821504471, -2.915334737309923874 ) ) ;
#36913 = CARTESIAN_POINT ( 'NONE',  ( 19.84674366389459266, 43.30059781766744464, 2.638427012816836559 ) ) ;
#36914 = CARTESIAN_POINT ( 'NONE',  ( -0.8801773607111008646, 38.27201867748816255, 2.915334737309923430 ) ) ;
#36915 = CARTESIAN_POINT ( 'NONE',  ( 10.00000000000000178, 19.31368534415484106, 10.88017736071110342 ) ) ;
#36916 = ORIENTED_EDGE ( 'NONE', *, *, #19708, .T. ) ;
#36917 = TOROIDAL_SURFACE ( 'NONE', #75232, 14.49999999999999822, 0.5000000000000000000 ) ;
#36918 = CARTESIAN_POINT ( 'NONE',  ( 15.44008868035555260, 29.73035201082150891, 9.422509992056143702 ) ) ;
#36919 = CIRCLE ( 'NONE', #68903, 14.49999999999999822 ) ;
#36920 = CARTESIAN_POINT ( 'NONE',  ( 13.43411237798105340, 40.58196800326375353, 12.81628187352647963 ) ) ;
#36921 = ADVANCED_FACE ( 'NONE', ( #31905 ), #10410, .F. ) ;
#36922 = CARTESIAN_POINT ( 'NONE',  ( 0.5774900079438607392, 33.48035201082150536, 5.440088680355550821 ) ) ;
#36924 = CARTESIAN_POINT ( 'NONE',  ( 20.88017736071110875, 35.77201867748816966, -2.915334737309920765 ) ) ;
#36923 = CARTESIAN_POINT ( 'NONE',  ( 1.959929470562273179, 46.50257860105348584, 5.767676674365838529 ) ) ;
#36925 = ORIENTED_EDGE ( 'NONE', *, *, #68556, .F. ) ;
#36926 = CARTESIAN_POINT ( 'NONE',  ( 14.92337183194729633, 52.67559781766745175, 8.527530157486181039 ) ) ;
#36927 = CARTESIAN_POINT ( 'NONE',  ( 20.88017736071110164, 40.35535201082150536, 2.915334737309930979 ) ) ;
#36928 = CARTESIAN_POINT ( 'NONE',  ( 2.791683348922240793, 66.63393115100079456, 7.208316651077764092 ) ) ;
#36929 = AXIS2_PLACEMENT_3D ( 'NONE', #6496, #59004, #82993 ) ;
#36930 = DIRECTION ( 'NONE',  ( 3.552713678800500929E-14, 0.000000000000000000, 1.000000000000000000 ) ) ;
#36931 = CARTESIAN_POINT ( 'NONE',  ( 24.16423886937410614, 49.51208216824730357, -3.795296366450302550 ) ) ;
#36932 = CARTESIAN_POINT ( 'NONE',  ( 2.035157376598824452, 58.68868534415482685, 7.964842623401179544 ) ) ;
#36933 = EDGE_CURVE ( 'NONE', #5021, #89406, #24933, .T. ) ;
#36934 = CARTESIAN_POINT ( 'NONE',  ( 0.000000000000000000, 91.25000000000000000, 7.750000000000000000 ) ) ;
#36935 = CARTESIAN_POINT ( 'NONE',  ( -3.927832320392339316, 15.00000000000000000, 13.69797916712101404 ) ) ;
#36936 = CARTESIAN_POINT ( 'NONE',  ( 19.84674366389459266, 63.71726448433412315, -2.638427012816827677 ) ) ;
#36937 = CARTESIAN_POINT ( 'NONE',  ( 0.1532563361054082862, 26.21726448433411605, 2.638427012816831674 ) ) ;
#36938 = VERTEX_POINT ( 'NONE', #78901 ) ;
#36939 = CARTESIAN_POINT ( 'NONE',  ( 14.92337183194729633, 27.67559781766745530, 8.527530157486181039 ) ) ;
#36940 = CARTESIAN_POINT ( 'NONE',  ( -11.09922568453594316, -20.45969866340291077, 6.408140936763246920 ) ) ;
#36941 = CARTESIAN_POINT ( 'NONE',  ( 7.084665262690076126, 24.10535201082150181, 10.88017736071109987 ) ) ;
#36942 = CARTESIAN_POINT ( 'NONE',  ( 0.1532563361054082862, 26.21726448433411605, 2.638427012816831674 ) ) ;
#36943 = CARTESIAN_POINT ( 'NONE',  ( -7.750000000000000000, 40.74999999999999289, -4.250000000000000000 ) ) ;
#36944 =( GEOMETRIC_REPRESENTATION_CONTEXT ( 3 ) GLOBAL_UNCERTAINTY_ASSIGNED_CONTEXT ( ( #64421 ) ) GLOBAL_UNIT_ASSIGNED_CONTEXT ( ( #90700, #44207, #5251 ) ) REPRESENTATION_CONTEXT ( 'NONE', 'WORKASPACE' ) );
#36945 = CARTESIAN_POINT ( 'NONE',  ( 19.05866839779139355, 25.95508385108958649, -6.499999999999974243 ) ) ;
#36946 = CARTESIAN_POINT ( 'NONE',  ( 4.559911319644449179, 37.23035201082150536, -9.422509992056141925 ) ) ;
#36947 = CARTESIAN_POINT ( 'NONE',  ( -0.3689425029237881626, 47.42874883491396787, 10.36894250292379027 ) ) ;
#36948 = CIRCLE ( 'NONE', #6603, 0.5000000000000004441 ) ;
#36949 = EDGE_CURVE ( 'NONE', #71629, #35522, #31272, .T. ) ;
#36950 = CARTESIAN_POINT ( 'NONE',  ( 20.15039907845753575, 35.60158574516643171, -6.262539305110076171 ) ) ;
#36951 = ORIENTED_EDGE ( 'NONE', *, *, #93389, .F. ) ;
#36952 = CARTESIAN_POINT ( 'NONE',  ( -2.816281873526471635, 18.91530133659708213, -3.434112377981056508 ) ) ;
#36953 = CARTESIAN_POINT ( 'NONE',  ( 19.42250999205614548, 5.980352010821504471, -5.440088680355545492 ) ) ;
#36954 = CARTESIAN_POINT ( 'NONE',  ( 20.88017736071110164, 50.35535201082151247, 2.915334737309930979 ) ) ;
#36955 = AXIS2_PLACEMENT_3D ( 'NONE', #66528, #65529, #50540 ) ;
#36956 = ADVANCED_FACE ( 'NONE', ( #39924 ), #92912, .T. ) ;
#36957 = ORIENTED_EDGE ( 'NONE', *, *, #98268, .T. ) ;
#36958 = CARTESIAN_POINT ( 'NONE',  ( 20.88017736071110875, 55.77201867748816966, -2.915334737309920765 ) ) ;
#36959 = VECTOR ( 'NONE', #98168, 1000.000000000000000 ) ;
#36960 = CARTESIAN_POINT ( 'NONE',  ( 10.00000000000000000, 39.75893115100078745, -9.846743663894594434 ) ) ;
#36961 = CARTESIAN_POINT ( 'NONE',  ( 10.00000000000000178, 22.25893115100078745, 9.846743663894594434 ) ) ;
#36962 = CARTESIAN_POINT ( 'NONE',  ( 2.791683348922237240, 10.38393115100078390, -7.208316651077763204 ) ) ;
#36963 = CARTESIAN_POINT ( 'NONE',  ( -6.030006457173053391, -39.79017371240020395, 2.499999999999193534 ) ) ;
#36965 = CARTESIAN_POINT ( 'NONE',  ( -6.382347221874564269, 14.49999999999999112, 13.57444820018227993 ) ) ;
#36964 = CARTESIAN_POINT ( 'NONE',  ( 1.472469842513823179, 0.5922644843341181575, -4.923371831947296329 ) ) ;
#36966 = CARTESIAN_POINT ( 'NONE',  ( -3.999999999999994671, 43.00000000000000711, 6.250000000000000000 ) ) ;
#36968 = ORIENTED_EDGE ( 'NONE', *, *, #20881, .F. ) ;
#36967 = CARTESIAN_POINT ( 'NONE',  ( 14.92337183194729633, 37.67559781766745175, 8.527530157486181039 ) ) ;
#36969 = CARTESIAN_POINT ( 'NONE',  ( -2.816281873526473856, 59.12363466993042493, 9.499525473075851096E-16 ) ) ;
#36970 = CARTESIAN_POINT ( 'NONE',  ( 4.630000000000001670, 0.09071050906739680508, 4.000000000000000000 ) ) ;
#36971 = CARTESIAN_POINT ( 'NONE',  ( 10.00000000000000000, 64.75893115100078035, -9.846743663894594434 ) ) ;
#36972 = CARTESIAN_POINT ( 'NONE',  ( 22.26659068614894466, 33.88708216824730357, 7.082119434687054849 ) ) ;
#36973 = CARTESIAN_POINT ( 'NONE',  ( -14.88232117145532385, 0.5000000000000004441, 1.875237731503040628 ) ) ;
#36974 = CARTESIAN_POINT ( 'NONE',  ( -0.3689425029237898834, 31.17874883491396787, -10.36894250292378850 ) ) ;
#36975 = CARTESIAN_POINT ( 'NONE',  ( 24.16423886937410614, 44.30374883491397497, 8.672049930838204340E-16 ) ) ;
#36976 = CARTESIAN_POINT ( 'NONE',  ( 17.08211943468705130, 3.470415501580634388, 12.26659068614894998 ) ) ;
#36978 = CARTESIAN_POINT ( 'NONE',  ( 17.96484262340118221, 64.93868534415483396, 7.964842623401181321 ) ) ;
#36977 = CARTESIAN_POINT ( 'NONE',  ( 24.16423886937410614, 9.303748834913967869, 8.672049930838204340E-16 ) ) ;
#36979 = CARTESIAN_POINT ( 'NONE',  ( 20.88017736071110519, 45.56368534415484106, 2.639326808657452039E-16 ) ) ;
#36980 = CARTESIAN_POINT ( 'NONE',  ( 0.000000000000000000, 0.5000000000000004441, 0.000000000000000000 ) ) ;
#36981 = CARTESIAN_POINT ( 'NONE',  ( 14.92337183194729988, 29.34226448433411960, -8.527530157486177487 ) ) ;
#36983 = CARTESIAN_POINT ( 'NONE',  ( 10.00000000000000178, 32.25893115100078745, 9.846743663894594434 ) ) ;
#36982 = CARTESIAN_POINT ( 'NONE',  ( 2.603489959281588106, 1.582109641433292690, 6.500000000000000888 ) ) ;
#36984 = VECTOR ( 'NONE', #57757, 1000.000000000000000 ) ;
#36985 = ORIENTED_EDGE ( 'NONE', *, *, #77348, .T. ) ;
#36986 = CARTESIAN_POINT ( 'NONE',  ( 4.559911319644449179, 27.23035201082150536, -9.422509992056141925 ) ) ;
#36987 = CARTESIAN_POINT ( 'NONE',  ( -1.099225684535947600, 53.70696800326376064, -6.408140936763238038 ) ) ;
#36988 = CARTESIAN_POINT ( 'NONE',  ( 18.52753015748618282, 63.92559781766745886, -4.923371831947291888 ) ) ;
#36989 = CARTESIAN_POINT ( 'NONE',  ( 18.00000000000000000, 78.06026161867410451, 3.869897282520398551 ) ) ;
#36990 = EDGE_CURVE ( 'NONE', #73831, #85496, #92329, .T. ) ;
#36991 = CARTESIAN_POINT ( 'NONE',  ( 0.1532563361054100626, 30.80059781766744820, -2.638427012816831230 ) ) ;
#36992 = CARTESIAN_POINT ( 'NONE',  ( 22.81628187352647785, 41.41530133659708923, 3.434112377981063169 ) ) ;
#36993 = CARTESIAN_POINT ( 'NONE',  ( 7.082119434687047743, -14.86291783175269465, -12.26659068614894821 ) ) ;
#36994 = CARTESIAN_POINT ( 'NONE',  ( 7.084665262690076126, 39.10535201082150536, 10.88017736071109987 ) ) ;
#36995 = CARTESIAN_POINT ( 'NONE',  ( 1.472469842513823179, 55.59226448433412315, -4.923371831947296329 ) ) ;
#36996 = CIRCLE ( 'NONE', #43328, 0.2500000000000002220 ) ;
#36997 = CARTESIAN_POINT ( 'NONE',  ( -4.164238869374098151, 31.59541550158063927, -3.795296366450310543 ) ) ;
#36998 = VERTEX_POINT ( 'NONE', #77912 ) ;
#36999 = PRESENTATION_STYLE_ASSIGNMENT (( #6491 ) ) ;
#37000 = CARTESIAN_POINT ( 'NONE',  ( 20.88017736071110164, 60.35535201082151957, 2.915334737309930979 ) ) ;
#37001 = CARTESIAN_POINT ( 'NONE',  ( 7.084665262690076126, 69.10535201082151957, 10.88017736071109987 ) ) ;
#37002 = CARTESIAN_POINT ( 'NONE',  ( 6.204703633549690345, 62.84541550158063927, 14.16423886937410082 ) ) ;
#37003 = CARTESIAN_POINT ( 'NONE',  ( 19.84674366389459621, 63.50893115100078745, 7.409399052514197653E-17 ) ) ;
#37004 = CARTESIAN_POINT ( 'NONE',  ( 0.1089645850229084695, 53.16234555792572536, 6.479102184480833415 ) ) ;
#37005 = CARTESIAN_POINT ( 'NONE',  ( 12.91533473730992121, 49.52201867748817676, 10.88017736071110164 ) ) ;
#37006 = CARTESIAN_POINT ( 'NONE',  ( 1.175527996597014457, 15.00000000000000888, 14.57931687975696811 ) ) ;
#37007 = CARTESIAN_POINT ( 'NONE',  ( 19.38216949554541202, 30.99863466993042138, 9.382169495545424454 ) ) ;
#37008 = CARTESIAN_POINT ( 'NONE',  ( 2.915334737309921209, 26.60535201082150891, -10.88017736071110164 ) ) ;
#37009 = CARTESIAN_POINT ( 'NONE',  ( 4.559911319644449179, 8.897018677488171434, 9.422509992056141925 ) ) ;
#37010 = CARTESIAN_POINT ( 'NONE',  ( 15.44008868035555260, 4.730352010821505360, 9.422509992056143702 ) ) ;
#37011 = CARTESIAN_POINT ( 'NONE',  ( 14.92337183194729988, 54.34226448433412315, -8.527530157486177487 ) ) ;
#37012 = CARTESIAN_POINT ( 'NONE',  ( 21.09922568453595559, 47.04030133659708923, -6.408140936763230044 ) ) ;
#37013 = SURFACE_STYLE_FILL_AREA ( #81509 ) ;
#37014 = VERTEX_POINT ( 'NONE', #2933 ) ;
#37015 = CARTESIAN_POINT ( 'NONE',  ( 7.084665262690076126, 12.02201867748817143, -10.88017736071110164 ) ) ;
#37016 = CARTESIAN_POINT ( 'NONE',  ( 13.43411237798106583, 22.66530133659708923, -12.81628187352647252 ) ) ;
#37017 = CARTESIAN_POINT ( 'NONE',  ( 20.04068437667223890, 39.71974360917720048, 6.396802510829769695 ) ) ;
#37018 = CARTESIAN_POINT ( 'NONE',  ( 7.361572987183170547, 17.05059781766745530, 9.846743663894590881 ) ) ;
#37019 = AXIS2_PLACEMENT_3D ( 'NONE', #91608, #53597, #46111 ) ;
#37020 = CIRCLE ( 'NONE', #19308, 14.49999999999999822 ) ;
#37021 = CARTESIAN_POINT ( 'NONE',  ( 19.84674366389459621, 48.50893115100078745, 7.409399052514197653E-17 ) ) ;
#37022 = CARTESIAN_POINT ( 'NONE',  ( 15.44008868035555793, 36.39701867748816966, -9.422509992056140149 ) ) ;
#37023 = B_SPLINE_CURVE_WITH_KNOTS ( 'NONE', 3,
 ( #70951, #2470, #32928, #54444, #16464, #93933 ),
 .UNSPECIFIED., .F., .F.,
 ( 4, 2, 4 ),
 ( 0.0002800858945027832718, 0.0006862919646584851509, 0.001092498034814187030 ),
 .UNSPECIFIED. ) ;
#37024 = CARTESIAN_POINT ( 'NONE',  ( 6.565887622018943937, 10.16530133659708746, 12.81628187352647430 ) ) ;
#37026 = DIRECTION ( 'NONE',  ( 1.000000000000000000, -0.000000000000000000, 0.000000000000000000 ) ) ;
#37025 = CARTESIAN_POINT ( 'NONE',  ( 10.00000000000000000, 46.81368534415484106, -10.88017736071110342 ) ) ;
#37027 = EDGE_CURVE ( 'NONE', #77111, #70022, #85922, .T. ) ;
#37028 = STYLED_ITEM ( 'NONE', ( #7811 ), #47403 ) ;
#37029 = CARTESIAN_POINT ( 'NONE',  ( 6.565887622018943937, 53.08196800326374643, -12.81628187352647608 ) ) ;
#37030 = VERTEX_POINT ( 'NONE', #32407 ) ;
#37031 = DIRECTION ( 'NONE',  ( -0.9762960071199316969, 0.000000000000000000, -0.2164396139381103701 ) ) ;
#37033 = CARTESIAN_POINT ( 'NONE',  ( 24.16423886937410614, 4.303748834913967869, 8.672049930838204340E-16 ) ) ;
#37032 = CARTESIAN_POINT ( 'NONE',  ( 3.591859063236763294, 33.29030133659708213, -11.09922568453595026 ) ) ;
#37034 = CARTESIAN_POINT ( 'NONE',  ( 4.559911319644449179, 33.89701867748817676, 9.422509992056141925 ) ) ;
#37035 = CARTESIAN_POINT ( 'NONE',  ( 5.076628168052703671, 61.84226448433412315, 8.527530157486179263 ) ) ;
#37036 = CARTESIAN_POINT ( 'NONE',  ( 0.000000000000000000, 15.00000000000000000, 0.000000000000000000 ) ) ;
#37037 = CARTESIAN_POINT ( 'NONE',  ( 0.1532563361054100626, 15.80059781766745353, -2.638427012816831230 ) ) ;
#37038 = CARTESIAN_POINT ( 'NONE',  ( 18.52753015748617571, 3.092264484334118269, 4.923371831947298993 ) ) ;
#37039 = CARTESIAN_POINT ( 'NONE',  ( -4.164238869374099927, 37.01208216824731068, 3.795296366450308767 ) ) ;
#37040 = AXIS2_PLACEMENT_3D ( 'NONE', #82089, #75084, #52094 ) ;
#37041 = CARTESIAN_POINT ( 'NONE',  ( 5.991992585808628036, 15.00000000000000000, -13.20401548210295140 ) ) ;
#37042 = EDGE_CURVE ( 'NONE', #97109, #93052, #91081, .T. ) ;
#37043 = CARTESIAN_POINT ( 'NONE',  ( 8.880000000000000782, 1.019547802438458550, -3.750000000000000000 ) ) ;
#37044 = CARTESIAN_POINT ( 'NONE',  ( -5.070949216187652375, -24.98410106517849982, -3.750000000001612044 ) ) ;
#37045 = VERTEX_POINT ( 'NONE', #9923 ) ;
#37046 = ORIENTED_EDGE ( 'NONE', *, *, #83578, .F. ) ;
#37047 = CARTESIAN_POINT ( 'NONE',  ( 6.204703633549690345, 60.76208216824730357, -14.16423886937410259 ) ) ;
#37048 = CARTESIAN_POINT ( 'NONE',  ( 20.36894250292379382, 58.67874883491396076, 10.36894250292379205 ) ) ;
#37049 = CARTESIAN_POINT ( 'NONE',  ( 12.63842701281683034, 27.46726448433411250, 9.846743663894596210 ) ) ;
#37050 = CARTESIAN_POINT ( 'NONE',  ( -1.099225684535947600, 28.70696800326375353, -6.408140936763238038 ) ) ;
#37051 = CARTESIAN_POINT ( 'NONE',  ( 4.265913727722193904, 14.95037113646324478, -14.12300574719579416 ) ) ;
#37053 = CARTESIAN_POINT ( 'NONE',  ( 6.204703633549690345, 5.762082168247301794, -14.16423886937410259 ) ) ;
#37052 = CARTESIAN_POINT ( 'NONE',  ( -13.59072821819446020, 90.85999462608982924, -7.686992381060815838 ) ) ;
#37054 = CARTESIAN_POINT ( 'NONE',  ( 4.559911319644449179, 8.897018677488171434, 9.422509992056141925 ) ) ;
#37055 = CARTESIAN_POINT ( 'NONE',  ( -4.164238869374099927, 52.01208216824729647, 3.795296366450308767 ) ) ;
#37056 = EDGE_CURVE ( 'NONE', #16083, #32902, #64374, .T. ) ;
#37057 = EDGE_CURVE ( 'NONE', #3541, #2122, #60779, .T. ) ;
#37058 = CARTESIAN_POINT ( 'NONE',  ( 19.84674366389459621, 28.50893115100078745, 7.409399052514197653E-17 ) ) ;
#37059 = CARTESIAN_POINT ( 'NONE',  ( 0.000000000000000000, 15.00000000000000000, 0.000000000000000000 ) ) ;
#37060 = CARTESIAN_POINT ( 'NONE',  ( 7.361572987183169658, 24.96726448433412315, -9.846743663894592657 ) ) ;
#37061 = DIRECTION ( 'NONE',  ( 0.000000000000000000, 0.000000000000000000, 1.000000000000000000 ) ) ;
#37062 = CARTESIAN_POINT ( 'NONE',  ( 9.846743663894590881, 13.30059781766745708, 2.638427012816828565 ) ) ;
#37063 = ORIENTED_EDGE ( 'NONE', *, *, #39541, .T. ) ;
#37064 = ORIENTED_EDGE ( 'NONE', *, *, #31158, .F. ) ;
#37065 = CARTESIAN_POINT ( 'NONE',  ( -14.19749592853509768, 15.00000000000000000, 7.369430493279844008 ) ) ;
#37066 = VERTEX_POINT ( 'NONE', #4396 ) ;
#37067 = CARTESIAN_POINT ( 'NONE',  ( 10.00000000000000000, 49.75893115100078745, -9.846743663894594434 ) ) ;
#37068 = CARTESIAN_POINT ( 'NONE',  ( 2.917880565312948704, 17.63708216824730357, 12.26659068614894643 ) ) ;
#37070 = CARTESIAN_POINT ( 'NONE',  ( 15.44008868035555260, 44.73035201082151247, 9.422509992056143702 ) ) ;
#37069 = CARTESIAN_POINT ( 'NONE',  ( 7.084665262690076126, 32.02201867748816966, -10.88017736071110164 ) ) ;
#37072 = CARTESIAN_POINT ( 'NONE',  ( 6.565887622018943937, 15.16530133659708568, 12.81628187352647430 ) ) ;
#37071 = CARTESIAN_POINT ( 'NONE',  ( 17.20831665107776587, 57.88393115100078745, 7.208316651077764980 ) ) ;
#37073 = CARTESIAN_POINT ( 'NONE',  ( -4.164238869374098151, 1.595415501580634388, -3.795296366450310543 ) ) ;
#37074 = CARTESIAN_POINT ( 'NONE',  ( 0.5774900079438590739, 62.64701867748817676, -5.440088680355550821 ) ) ;
#37075 = AXIS2_PLACEMENT_3D ( 'NONE', #20789, #88290, #88782 ) ;
#37076 = CARTESIAN_POINT ( 'NONE',  ( 0.6178305044545818747, 38.49863466993042493, -9.382169495545419124 ) ) ;
#37077 = VERTEX_POINT ( 'NONE', #42874 ) ;
#37078 = CARTESIAN_POINT ( 'NONE',  ( 5.076628168052704559, 45.17559781766745175, -8.527530157486179263 ) ) ;
#37079 = CARTESIAN_POINT ( 'NONE',  ( 2.035157376598822676, 2.438685344154838397, -7.964842623401177768 ) ) ;
#37080 = ORIENTED_EDGE ( 'NONE', *, *, #79343, .T. ) ;
#37081 = EDGE_CURVE ( 'NONE', #71137, #11622, #34865, .T. ) ;
#37082 = CARTESIAN_POINT ( 'NONE',  ( 12.91533473730992121, 9.522018677488171434, 10.88017736071110164 ) ) ;
#37083 = EDGE_LOOP ( 'NONE', ( #16176, #73656, #16405, #89677, #25382, #85373 ) ) ;
#37084 = CARTESIAN_POINT ( 'NONE',  ( 20.88017736071110519, 50.56368534415484106, 2.639326808657452039E-16 ) ) ;
#37085 = CARTESIAN_POINT ( 'NONE',  ( 4.559911319644449179, 57.23035201082150536, -9.422509992056141925 ) ) ;
#37086 = CARTESIAN_POINT ( 'NONE',  ( 2.035157376598824452, 58.68868534415482685, 7.964842623401179544 ) ) ;
#37087 = FACE_OUTER_BOUND ( 'NONE', #52149, .T. ) ;
#37088 = CARTESIAN_POINT ( 'NONE',  ( 20.88017736071110875, 60.77201867748817676, -2.915334737309920765 ) ) ;
#37089 = DIRECTION ( 'NONE',  ( 0.000000000000000000, 0.000000000000000000, 1.000000000000000000 ) ) ;
#37091 = VECTOR ( 'NONE', #80229, 1000.000000000000000 ) ;
#37090 = FILL_AREA_STYLE_COLOUR ( '', #79252 ) ;
#37092 = CARTESIAN_POINT ( 'NONE',  ( 5.076628168052704559, 30.17559781766745175, -8.527530157486179263 ) ) ;
#37093 = VERTEX_POINT ( 'NONE', #65358 ) ;
#37094 = DIRECTION ( 'NONE',  ( 0.9970872288863210642, 0.07626964003977955431, 0.000000000000000000 ) ) ;
#37095 = AXIS2_PLACEMENT_3D ( 'NONE', #74821, #59811, #45820 ) ;
#37096 = COLOUR_RGB ( '', 0.72549020, 0.75294118, 0.79215686) ;
#37097 = AXIS2_PLACEMENT_3D ( 'NONE', #85010, #19333, #55993 ) ;
#37098 = VERTEX_POINT ( 'NONE', #50865 ) ;
#37099 = PRESENTATION_STYLE_ASSIGNMENT (( #6102 ) ) ;
#37100 = LINE ( 'NONE', #30065, #50626 ) ;
#37102 = CARTESIAN_POINT ( 'NONE',  ( 1.472469842513823179, 36.42559781766745175, 4.923371831947296329 ) ) ;
#37101 = LINE ( 'NONE', #82588, #38605 ) ;
#37103 = CARTESIAN_POINT ( 'NONE',  ( 17.96484262340118221, 6.188685344154837509, -7.964842623401177768 ) ) ;
#37104 = DIRECTION ( 'NONE',  ( -1.000000000000000000, 0.000000000000000000, 0.000000000000000000 ) ) ;
#37105 = ORIENTED_EDGE ( 'NONE', *, *, #86035, .T. ) ;
#37107 = AXIS2_PLACEMENT_3D ( 'NONE', #65878, #43865, #96406 ) ;
#37106 = CARTESIAN_POINT ( 'NONE',  ( 20.03447792253739834, 62.65514106990689669, -6.401564815979719825 ) ) ;
#37108 = CARTESIAN_POINT ( 'NONE',  ( 14.92337183194729988, 49.34226448433411605, -8.527530157486177487 ) ) ;
#37109 = CARTESIAN_POINT ( 'NONE',  ( 0.000000000000000000, 0.000000000000000000, 0.000000000000000000 ) ) ;
#37110 = CARTESIAN_POINT ( 'NONE',  ( 6.565887622018943937, 13.08196800326374998, -12.81628187352647608 ) ) ;
#37111 = CARTESIAN_POINT ( 'NONE',  ( 5.076628168052703671, 11.84226448433411960, 8.527530157486179263 ) ) ;
#37112 = DIRECTION ( 'NONE',  ( 1.257568779154408793E-17, 1.000000000000000000, -0.000000000000000000 ) ) ;
#37113 = CARTESIAN_POINT ( 'NONE',  ( 1.472469842513823179, 16.42559781766745175, 4.923371831947296329 ) ) ;
#37114 = CARTESIAN_POINT ( 'NONE',  ( 3.591859063236763294, 8.290301336597087456, -11.09922568453595026 ) ) ;
#37115 = AXIS2_PLACEMENT_3D ( 'NONE', #49671, #94699, #4698 ) ;
#37116 = B_SPLINE_CURVE_WITH_KNOTS ( 'NONE', 3,
 ( #47140, #86998, #76663, #77637, #33483, #63980 ),
 .UNSPECIFIED., .F., .F.,
 ( 4, 2, 4 ),
 ( 3.409110551494641268E-05, 0.0004400426677367931852, 0.0008459942299586398901 ),
 .UNSPECIFIED. ) ;
#37117 = ORIENTED_EDGE ( 'NONE', *, *, #6400, .T. ) ;
#37118 = ORIENTED_EDGE ( 'NONE', *, *, #67558, .F. ) ;
#37119 = CARTESIAN_POINT ( 'NONE',  ( 20.88017736071110875, 25.77201867748816966, -2.915334737309920765 ) ) ;
#37120 = CARTESIAN_POINT ( 'NONE',  ( -4.164238869374098151, 21.59541550158063217, -3.795296366450310543 ) ) ;
#37121 = CARTESIAN_POINT ( 'NONE',  ( 19.84674366389459266, 33.71726448433410894, -2.638427012816827677 ) ) ;
#37122 = CARTESIAN_POINT ( 'NONE',  ( 10.00000000000000000, 61.81368534415484106, -10.88017736071110342 ) ) ;
#37124 = FACE_BOUND ( 'NONE', #34324, .T. ) ;
#37123 = CARTESIAN_POINT ( 'NONE',  ( 13.43411237798106583, 37.66530133659708923, -12.81628187352647252 ) ) ;
#37125 = CARTESIAN_POINT ( 'NONE',  ( 20.88017736071110164, 10.35535201082150714, 2.915334737309930979 ) ) ;
#37126 = CARTESIAN_POINT ( 'NONE',  ( 17.35999999999999943, 37.99999999999997868, 10.00000000000000000 ) ) ;
#37127 = CARTESIAN_POINT ( 'NONE',  ( -4.267749253172081758, 0.000000000000000000, 3.394721039305316879 ) ) ;
#37128 = AXIS2_PLACEMENT_3D ( 'NONE', #87980, #66463, #73464 ) ;
#37129 = CARTESIAN_POINT ( 'NONE',  ( 13.43411237798105340, 10.58196800326375353, 12.81628187352647963 ) ) ;
#37130 = CARTESIAN_POINT ( 'NONE',  ( 5.076628168052703671, 61.84226448433412315, 8.527530157486179263 ) ) ;
#37131 = CARTESIAN_POINT ( 'NONE',  ( 7.361572987183169658, 24.96726448433412315, -9.846743663894592657 ) ) ;
#37132 = CARTESIAN_POINT ( 'NONE',  ( -10.88017736071110342, -16.93631465584515539, 3.903127820947815962E-15 ) ) ;
#37133 = CARTESIAN_POINT ( 'NONE',  ( 19.38216949554541557, 32.24863466993041783, -9.382169495545420901 ) ) ;
#37134 = DIRECTION ( 'NONE',  ( -0.000000000000000000, -0.000000000000000000, -1.000000000000000000 ) ) ;
#37136 = CARTESIAN_POINT ( 'NONE',  ( 14.94699059465101598, 14.63595249122788999, 1.259949270174913316 ) ) ;
#37135 = CARTESIAN_POINT ( 'NONE',  ( 2.035157376598822676, 37.43868534415484106, -7.964842623401177768 ) ) ;
#37137 = EDGE_CURVE ( 'NONE', #74265, #59795, #51849, .T. ) ;
#37138 = CARTESIAN_POINT ( 'NONE',  ( 0.000000000000000000, 0.000000000000000000, 9.500000000000000000 ) ) ;
#37139 = CARTESIAN_POINT ( 'NONE',  ( 18.50749283717776805, 29.69955587570480660, 6.499999999999997335 ) ) ;
#37140 = CARTESIAN_POINT ( 'NONE',  ( 10.00000000000000000, 46.81368534415484106, -10.88017736071110342 ) ) ;
#37142 = CARTESIAN_POINT ( 'NONE',  ( -0.8801773607110991993, 37.85535201082151247, -2.915334737309923874 ) ) ;
#37141 = CIRCLE ( 'NONE', #94579, 15.00000000000000000 ) ;
#37143 = CARTESIAN_POINT ( 'NONE',  ( 18.52753015748617571, 63.09226448433412315, 4.923371831947298993 ) ) ;
#37144 = DIRECTION ( 'NONE',  ( -0.9426414910921805390, 0.000000000000000000, 0.3338068592337649076 ) ) ;
#37145 = UNCERTAINTY_MEASURE_WITH_UNIT (LENGTH_MEASURE( 1.000000000000000082E-05 ), #97413, 'distance_accuracy_value', 'NONE');
#37146 =( BOUNDED_CURVE ( )  B_SPLINE_CURVE ( 2, ( #75899, #51922, #68410, #74911, #13932, #6411, #22918, #36923, #98932 ),
 .UNSPECIFIED., .F., .T. ) 
 B_SPLINE_CURVE_WITH_KNOTS ( ( 3, 2, 2, 2, 3 ),
 ( 0.6525141644748393421, 0.6547619047619047672, 0.6607142857142856984, 0.6666666666666666297, 0.6689144069537320547 ),
 .UNSPECIFIED. ) 
 CURVE ( )  GEOMETRIC_REPRESENTATION_ITEM ( )  RATIONAL_B_SPLINE_CURVE ( ( 0.9839835555609424134, 0.9871328979762474809, 1.000000000000000000, 0.9659258262890683122, 1.000000000000000000, 0.9659258262890683122, 1.000000000000000000, 0.9871328979762477029, 0.9839835555609425244 ) ) 
 REPRESENTATION_ITEM ( '' )  );
#37147 = CARTESIAN_POINT ( 'NONE',  ( 0.1532563361054083140, 41.00893115100078745, 1.131784320476157264E-15 ) ) ;
#37148 = CARTESIAN_POINT ( 'NONE',  ( 17.96484262340118221, 9.938685344154837509, 7.964842623401181321 ) ) ;
#37149 = CARTESIAN_POINT ( 'NONE',  ( 0.6178305044545838731, 14.74863466993041783, 9.382169495545420901 ) ) ;
#37150 = EDGE_LOOP ( 'NONE', ( #4628, #85417, #45918, #72620 ) ) ;
#37151 = CARTESIAN_POINT ( 'NONE',  ( -0.8801773607110991993, 22.85535201082150181, -2.915334737309923874 ) ) ;
#37152 = CARTESIAN_POINT ( 'NONE',  ( 0.000000000000000000, 40.74999999999999289, -4.250000000000000000 ) ) ;
#37153 = CARTESIAN_POINT ( 'NONE',  ( 7.084665262690076126, 4.105352010821503583, 10.88017736071109987 ) ) ;
#37154 = CARTESIAN_POINT ( 'NONE',  ( 7.084665262690076126, 27.02201867748817676, -10.88017736071110164 ) ) ;
#37155 = CARTESIAN_POINT ( 'NONE',  ( 17.20831665107776587, 2.883931151000785231, 7.208316651077764980 ) ) ;
#37156 = CARTESIAN_POINT ( 'NONE',  ( 17.08211943468705130, 43.47041550158063927, 12.26659068614894998 ) ) ;
#37157 = CARTESIAN_POINT ( 'NONE',  ( 12.63842701281683922, 9.550597817667449974, -9.846743663894590881 ) ) ;
#37158 = CARTESIAN_POINT ( 'NONE',  ( 7.084665262690076126, 42.02201867748816966, -10.88017736071110164 ) ) ;
#37159 = CARTESIAN_POINT ( 'NONE',  ( 19.72487221294571569, 45.71833443783938122, -6.499999999999989342 ) ) ;
#37160 = EDGE_CURVE ( 'NONE', #89788, #44051, #12368, .T. ) ;
#37161 = VERTEX_POINT ( 'NONE', #73357 ) ;
#37162 = UNCERTAINTY_MEASURE_WITH_UNIT (LENGTH_MEASURE( 1.000000000000000082E-05 ), #27747, 'distance_accuracy_value', 'NONE');
#37163 = STYLED_ITEM ( 'NONE', ( #49614 ), #65095 ) ;
#37164 = FACE_BOUND ( 'NONE', #49477, .T. ) ;
#37165 = CARTESIAN_POINT ( 'NONE',  ( 2.791683348922237240, 65.38393115100078035, -7.208316651077763204 ) ) ;
#37167 = EDGE_LOOP ( 'NONE', ( #37063, #1496, #2297, #92492 ) ) ;
#37166 = EDGE_CURVE ( 'NONE', #47944, #39498, #265, .T. ) ;
#37168 = ORIENTED_EDGE ( 'NONE', *, *, #6952, .F. ) ;
#37169 =( LENGTH_UNIT ( ) NAMED_UNIT ( * ) SI_UNIT ( .MILLI., .METRE. ) );
#37170 = CARTESIAN_POINT ( 'NONE',  ( 17.08211943468705130, 18.47041550158063572, 12.26659068614894998 ) ) ;
#37171 = CARTESIAN_POINT ( 'NONE',  ( 13.79529636645031943, 20.34541550158063572, -14.16423886937409904 ) ) ;
#37172 = CARTESIAN_POINT ( 'NONE',  ( 12.91533473730993009, 61.60535201082150536, -10.88017736071109987 ) ) ;
#37173 = CARTESIAN_POINT ( 'NONE',  ( -4.164238869374099927, 62.01208216824728936, 3.795296366450308767 ) ) ;
#37174 = CARTESIAN_POINT ( 'NONE',  ( 21.09922568453595559, 2.040301336597086568, -6.408140936763230044 ) ) ;
#37175 = CARTESIAN_POINT ( 'NONE',  ( 17.20831665107776587, 44.13393115100078745, -7.208316651077762316 ) ) ;
#37176 = CARTESIAN_POINT ( 'NONE',  ( -8.330954873910256353, -7.272562134485029084, 4.000000000000000000 ) ) ;
#37178 = CARTESIAN_POINT ( 'NONE',  ( 16.40814093676323893, 5.790301336597087456, 11.09922568453595026 ) ) ;
#37177 = CARTESIAN_POINT ( 'NONE',  ( 17.96484262340118221, 44.93868534415483396, 7.964842623401181321 ) ) ;
#37179 = CARTESIAN_POINT ( 'NONE',  ( 20.36894250292379738, 14.92874883491396432, -10.36894250292379027 ) ) ;
#37180 = CARTESIAN_POINT ( 'NONE',  ( 0.5774900079438607392, 13.48035201082150358, 5.440088680355550821 ) ) ;
#37181 = ADVANCED_FACE ( 'NONE', ( #57860 ), #4884, .F. ) ;
#37182 = CARTESIAN_POINT ( 'NONE',  ( 4.559911319644449179, 13.89701867748817321, 9.422509992056141925 ) ) ;
#37183 = VECTOR ( 'NONE', #40550, 1000.000000000000000 ) ;
#37184 = FILL_AREA_STYLE ('',( #74159 ) ) ;
#37185 = CARTESIAN_POINT ( 'NONE',  ( 20.88017736071110875, 55.77201867748816966, -2.915334737309920765 ) ) ;
#37186 = CIRCLE ( 'NONE', #59497, 14.49999999999999822 ) ;
#37187 = CARTESIAN_POINT ( 'NONE',  ( 13.43411237798106583, 47.66530133659709634, -12.81628187352647252 ) ) ;
#37188 = CARTESIAN_POINT ( 'NONE',  ( -8.527530157486182816, -24.40773551566587685, -4.923371831947288335 ) ) ;
#37189 = VERTEX_POINT ( 'NONE', #58848 ) ;
#37190 = FACE_OUTER_BOUND ( 'NONE', #93026, .T. ) ;
#37191 = VECTOR ( 'NONE', #79786, 1000.000000000000000 ) ;
#37192 = VERTEX_POINT ( 'NONE', #89354 ) ;
#37193 = ORIENTED_EDGE ( 'NONE', *, *, #29891, .F. ) ;
#37194 = CARTESIAN_POINT ( 'NONE',  ( 0.2751277870542911952, 19.36607318730131055, -6.499999999999992006 ) ) ;
#37196 = CARTESIAN_POINT ( 'NONE',  ( 7.084665262690076126, 2.022018677488171434, -10.88017736071110164 ) ) ;
#37195 = CARTESIAN_POINT ( 'NONE',  ( -2.266590686148945544, 41.38708216824729647, -7.082119434687050408 ) ) ;
#37198 = CARTESIAN_POINT ( 'NONE',  ( 14.92337183194729988, 49.34226448433411605, -8.527530157486177487 ) ) ;
#37197 = CARTESIAN_POINT ( 'NONE',  ( 14.92337183194729988, 19.34226448433411960, -8.527530157486177487 ) ) ;
#37199 = CARTESIAN_POINT ( 'NONE',  ( 4.559911319644449179, 68.89701867748817676, 9.422509992056141925 ) ) ;
#37200 = CARTESIAN_POINT ( 'NONE',  ( 18.52753015748618282, 3.925597817667451306, -4.923371831947291888 ) ) ;
#37201 = CARTESIAN_POINT ( 'NONE',  ( 6.408140936763236262, 22.45696800326375708, -11.09922568453595026 ) ) ;
#37202 = ORIENTED_EDGE ( 'NONE', *, *, #92786, .T. ) ;
#37203 = CARTESIAN_POINT ( 'NONE',  ( 20.36894250292379738, 34.92874883491396076, -10.36894250292379027 ) ) ;
#37204 = B_SPLINE_CURVE_WITH_KNOTS ( 'NONE', 3,
 ( #61388, #7917, #38413, #15908, #67925, #84891 ),
 .UNSPECIFIED., .F., .F.,
 ( 4, 2, 4 ),
 ( 0.0002800008091676931660, 0.0006862060465022924369, 0.001092411283836891654 ),
 .UNSPECIFIED. ) ;
#37205 = EDGE_CURVE ( 'NONE', #80817, #87107, #16950, .T. ) ;
#37206 = CARTESIAN_POINT ( 'NONE',  ( 0.6178305044545838731, 29.74863466993042138, 9.382169495545420901 ) ) ;
#37207 = ORIENTED_EDGE ( 'NONE', *, *, #45495, .T. ) ;
#37208 = CIRCLE ( 'NONE', #49959, 14.49999999999999822 ) ;
#37209 = CARTESIAN_POINT ( 'NONE',  ( 6.565887622018943937, 55.16530133659709634, 12.81628187352647430 ) ) ;
#37210 = CARTESIAN_POINT ( 'NONE',  ( 15.44008868035555260, 29.73035201082150891, 9.422509992056143702 ) ) ;
#37211 = CARTESIAN_POINT ( 'NONE',  ( 0.1532563361054083140, 41.00893115100078745, 1.131784320476157264E-15 ) ) ;
#37212 = CARTESIAN_POINT ( 'NONE',  ( 0.5774900079438590739, 32.64701867748816966, -5.440088680355550821 ) ) ;
#37213 = CARTESIAN_POINT ( 'NONE',  ( 0.6178305044545818747, 63.49863466993043204, -9.382169495545419124 ) ) ;
#37214 = FACE_OUTER_BOUND ( 'NONE', #21881, .T. ) ;
#37215 = CARTESIAN_POINT ( 'NONE',  ( 1.472469842513823179, 40.59226448433411605, -4.923371831947296329 ) ) ;
#37216 = CARTESIAN_POINT ( 'NONE',  ( 2.791683348922240793, 56.63393115100078035, 7.208316651077764092 ) ) ;
#37217 = EDGE_CURVE ( 'NONE', #76154, #80095, #11224, .T. ) ;
#37219 = ORIENTED_EDGE ( 'NONE', *, *, #44824, .F. ) ;
#37218 = CARTESIAN_POINT ( 'NONE',  ( 11.49974963341099077, 56.98753627293847757, 0.000000000000000000 ) ) ;
#37220 = CIRCLE ( 'NONE', #59536, 9.999999999999994671 ) ;
#37221 = DIRECTION ( 'NONE',  ( -0.000000000000000000, -1.000000000000000000, -0.000000000000000000 ) ) ;
#37222 = LINE ( 'NONE', #67707, #61053 ) ;
#37223 = CARTESIAN_POINT ( 'NONE',  ( 6.880000000000009663, 40.99999999999999289, -4.250000000000000000 ) ) ;
#37224 = CARTESIAN_POINT ( 'NONE',  ( 0.000000000000000000, 15.00000000000000000, 0.000000000000000000 ) ) ;
#37225 = CARTESIAN_POINT ( 'NONE',  ( 19.84674366389459621, 18.50893115100078745, 7.409399052514197653E-17 ) ) ;
#37226 = DIRECTION ( 'NONE',  ( 0.000000000000000000, 0.000000000000000000, -1.000000000000000000 ) ) ;
#37227 = EDGE_LOOP ( 'NONE', ( #14372, #91786, #13160, #9643 ) ) ;
#37228 = CARTESIAN_POINT ( 'NONE',  ( 19.84674366389459266, 53.30059781766744464, 2.638427012816836559 ) ) ;
#37229 = CARTESIAN_POINT ( 'NONE',  ( 0.1532563361054083140, 46.00893115100079456, 1.131784320476157264E-15 ) ) ;
#37230 = CARTESIAN_POINT ( 'NONE',  ( 6.204703633549690345, 32.84541550158063927, 14.16423886937410082 ) ) ;
#37231 = CARTESIAN_POINT ( 'NONE',  ( 7.361572987183169658, 49.96726448433410894, -9.846743663894592657 ) ) ;
#37232 = CARTESIAN_POINT ( 'NONE',  ( 10.00000000000000178, 50.37363466993042493, 12.81628187352647608 ) ) ;
#37233 = DIRECTION ( 'NONE',  ( 0.000000000000000000, 0.000000000000000000, -1.000000000000000000 ) ) ;
#37234 = CARTESIAN_POINT ( 'NONE',  ( 14.92337183194729633, 2.675597817667451750, 8.527530157486181039 ) ) ;
#37235 = CARTESIAN_POINT ( 'NONE',  ( 20.36894250292379382, 3.678748834913967869, 10.36894250292379205 ) ) ;
#37236 = CARTESIAN_POINT ( 'NONE',  ( 7.361572987183169658, 54.96726448433413026, -9.846743663894592657 ) ) ;
#37237 = CARTESIAN_POINT ( 'NONE',  ( -0.8801773607110991993, 42.85535201082150536, -2.915334737309923874 ) ) ;
#37238 = MECHANICAL_DESIGN_GEOMETRIC_PRESENTATION_REPRESENTATION (  '', ( #3684 ), #26021 ) ;
#37239 = CARTESIAN_POINT ( 'NONE',  ( 10.00000000000000178, 42.25893115100078745, 9.846743663894594434 ) ) ;
#37240 = CARTESIAN_POINT ( 'NONE',  ( 20.03743638938529159, 31.75197528031016603, 6.399506433553909801 ) ) ;
#37241 = CARTESIAN_POINT ( 'NONE',  ( 10.00000000000000178, 44.31368534415484106, 10.88017736071110342 ) ) ;
#37242 = AXIS2_PLACEMENT_3D ( 'NONE', #36602, #4630, #20103 ) ;
#37243 = VERTEX_POINT ( 'NONE', #80870 ) ;
#37244 = DIRECTION ( 'NONE',  ( 0.000000000000000000, 1.000000000000000000, 0.000000000000000000 ) ) ;
#37245 = CARTESIAN_POINT ( 'NONE',  ( 10.00000000000000000, 21.81368534415484106, -10.88017736071110342 ) ) ;
#37247 = CARTESIAN_POINT ( 'NONE',  ( 20.88017736071110164, 45.35535201082149115, 2.915334737309930979 ) ) ;
#37246 = CARTESIAN_POINT ( 'NONE',  ( 10.00000000000000000, -2.126365330069579951, -12.81628187352647608 ) ) ;
#37248 = AXIS2_PLACEMENT_3D ( 'NONE', #7121, #90112, #83614 ) ;
#37249 = LINE ( 'NONE', #77190, #66708 ) ;
#37250 = DIRECTION ( 'NONE',  ( -1.000000000000000000, 0.000000000000000000, 0.000000000000000000 ) ) ;
#37252 = DIRECTION ( 'NONE',  ( 0.000000000000000000, 0.000000000000000000, -1.000000000000000000 ) ) ;
#37251 = CARTESIAN_POINT ( 'NONE',  ( 10.00000000000000178, 39.31368534415484106, 10.88017736071110342 ) ) ;
#37253 = CARTESIAN_POINT ( 'NONE',  ( 12.63842701281683922, 14.55059781766744997, -9.846743663894590881 ) ) ;
#37254 = EDGE_CURVE ( 'NONE', #295, #53155, #20371, .T. ) ;
#37255 = CARTESIAN_POINT ( 'NONE',  ( 5.076628168052704559, 25.17559781766745175, -8.527530157486179263 ) ) ;
#37256 = PLANE ( 'NONE',  #72881 ) ;
#37257 = VECTOR ( 'NONE', #58833, 1000.000000000000000 ) ;
#37258 = CARTESIAN_POINT ( 'NONE',  ( 7.082119434687047743, 15.13708216824730890, -12.26659068614894821 ) ) ;
#37259 = CARTESIAN_POINT ( 'NONE',  ( 10.00000000000000178, 0.3736346699304200492, 12.81628187352647608 ) ) ;
#37260 = CARTESIAN_POINT ( 'NONE',  ( -2.266590686148945544, 66.38708216824730357, -7.082119434687050408 ) ) ;
#37261 = DIRECTION ( 'NONE',  ( -0.9997628902338895340, 0.02177529129954166101, 1.734723475976803939E-15 ) ) ;
#37262 = ADVANCED_FACE ( 'NONE', ( #43353 ), #74983, .F. ) ;
#37263 = CARTESIAN_POINT ( 'NONE',  ( 13.79529636645030344, 23.26208216824730002, 14.16423886937410614 ) ) ;
#37264 = CARTESIAN_POINT ( 'NONE',  ( 10.00000000000000000, 45.55374883491397497, -14.16423886937410082 ) ) ;
#37265 = CARTESIAN_POINT ( 'NONE',  ( 20.88017736071110875, 5.772018677488170546, -2.915334737309920765 ) ) ;
#37266 = EDGE_LOOP ( 'NONE', ( #95845, #30047 ) ) ;
#37267 = CARTESIAN_POINT ( 'NONE',  ( 0.1532563361054100626, 25.80059781766744820, -2.638427012816831230 ) ) ;
#37268 = CARTESIAN_POINT ( 'NONE',  ( 20.88017736071110164, 15.35535201082150358, 2.915334737309930979 ) ) ;
#37269 = CARTESIAN_POINT ( 'NONE',  ( 2.791683348922240793, 46.63393115100077324, 7.208316651077764092 ) ) ;
#37270 = CARTESIAN_POINT ( 'NONE',  ( 2.917880565312948704, 2.637082168247300906, 12.26659068614894643 ) ) ;
#37271 = DIRECTION ( 'NONE',  ( 0.000000000000000000, 0.000000000000000000, 1.000000000000000000 ) ) ;
#37272 = CARTESIAN_POINT ( 'NONE',  ( 0.1532563361054082862, 1.217264484334117824, 2.638427012816831674 ) ) ;
#37273 = CARTESIAN_POINT ( 'NONE',  ( 16.40814093676323893, 40.79030133659708923, 11.09922568453595026 ) ) ;
#37274 = CARTESIAN_POINT ( 'NONE',  ( 0.1532563361054083140, 36.00893115100078745, 1.131784320476157264E-15 ) ) ;
#37275 = VERTEX_POINT ( 'NONE', #90826 ) ;
#37276 = CARTESIAN_POINT ( 'NONE',  ( 0.1532563361054083140, 6.008931151000784787, 1.131784320476157264E-15 ) ) ;
#37277 = CARTESIAN_POINT ( 'NONE',  ( 11.18126922390458589, -92.99194761432693213, -3.999999999999103384 ) ) ;
#37278 = CARTESIAN_POINT ( 'NONE',  ( 19.88701968852526036, 16.79427333184085569, 6.480634945678614756 ) ) ;
#37279 = CARTESIAN_POINT ( 'NONE',  ( -0.8801773607110991993, 12.85535201082150358, -2.915334737309923874 ) ) ;
#37280 = CARTESIAN_POINT ( 'NONE',  ( -0.3689425029237898834, 51.17874883491397497, -10.36894250292378850 ) ) ;
#37281 = CARTESIAN_POINT ( 'NONE',  ( 1.472469842513823179, 20.59226448433411960, -4.923371831947296329 ) ) ;
#37282 = CARTESIAN_POINT ( 'NONE',  ( 10.00000000000000178, 4.313685344154837509, 10.88017736071110342 ) ) ;
#37283 = CARTESIAN_POINT ( 'NONE',  ( 19.84674366389459266, 3.300597817667451750, 2.638427012816836559 ) ) ;
#37284 = CARTESIAN_POINT ( 'NONE',  ( 4.841308736149698255, 0.2301500557980281081, -14.13449535775533050 ) ) ;
#37285 = CARTESIAN_POINT ( 'NONE',  ( 10.00000000000000178, 47.25893115100078745, 9.846743663894594434 ) ) ;
#37286 = AXIS2_PLACEMENT_3D ( 'NONE', #5650, #12148, #73129 ) ;
#37287 = CARTESIAN_POINT ( 'NONE',  ( 17.96484262340118221, 36.18868534415484106, -7.964842623401177768 ) ) ;
#37288 = UNCERTAINTY_MEASURE_WITH_UNIT (LENGTH_MEASURE( 1.000000000000000082E-05 ), #30566, 'distance_accuracy_value', 'NONE');
#37289 = TOROIDAL_SURFACE ( 'NONE', #26070, 9.900000000000002132, 0.1000000000000000056 ) ;
#37290 = EDGE_CURVE ( 'NONE', #71843, #80716, #79148, .T. ) ;
#37291 = ORIENTED_EDGE ( 'NONE', *, *, #52783, .F. ) ;
#37292 = CARTESIAN_POINT ( 'NONE',  ( 10.00000000000000178, 65.37363466993042493, 12.81628187352647608 ) ) ;
#37293 = CARTESIAN_POINT ( 'NONE',  ( 9.742785792574936821, 5.838468844518209799, -5.625000000000004441 ) ) ;
#37294 = CARTESIAN_POINT ( 'NONE',  ( 17.20831665107776587, 9.133931151000787452, -7.208316651077762316 ) ) ;
#37295 = CARTESIAN_POINT ( 'NONE',  ( -1.099225684535947600, 39.54030133659708923, 6.408140936763237150 ) ) ;
#37297 = CARTESIAN_POINT ( 'NONE',  ( 12.63842701281683922, 29.55059781766745175, -9.846743663894590881 ) ) ;
#37296 = CARTESIAN_POINT ( 'NONE',  ( 6.204703633549690345, 67.84541550158060375, 14.16423886937410082 ) ) ;
#37298 = CARTESIAN_POINT ( 'NONE',  ( -19.64999999999999858, 0.000000000000000000, 7.750000000000000000 ) ) ;
#37299 = CARTESIAN_POINT ( 'NONE',  ( 22.26659068614895176, 34.72041550158063927, -7.082119434687042414 ) ) ;
#37300 = EDGE_CURVE ( 'NONE', #21605, #70392, #55309, .T. ) ;
#37301 = CARTESIAN_POINT ( 'NONE',  ( 6.204703633549690345, 47.84541550158064638, 14.16423886937410082 ) ) ;
#37302 = CARTESIAN_POINT ( 'NONE',  ( 1.472469842513823179, 51.42559781766745886, 4.923371831947296329 ) ) ;
#37303 = CYLINDRICAL_SURFACE ( 'NONE', #52300, 2.999999999999998224 ) ;
#37304 = CARTESIAN_POINT ( 'NONE',  ( -0.8801773607111009756, 43.06368534415484106, 1.068504757029289695E-15 ) ) ;
#37305 = CARTESIAN_POINT ( 'NONE',  ( 0.5774900079438607392, 68.48035201082150536, 5.440088680355550821 ) ) ;
#37306 = FACE_OUTER_BOUND ( 'NONE', #53962, .T. ) ;
#37307 = ORIENTED_EDGE ( 'NONE', *, *, #64553, .T. ) ;
#37308 = CARTESIAN_POINT ( 'NONE',  ( 21.09922568453595559, 52.04030133659708923, -6.408140936763230044 ) ) ;
#37309 = ORIENTED_EDGE ( 'NONE', *, *, #45060, .T. ) ;
#37310 = CARTESIAN_POINT ( 'NONE',  ( 19.42250999205614548, 65.98035201082151957, -5.440088680355545492 ) ) ;
#37311 = ORIENTED_EDGE ( 'NONE', *, *, #96135, .F. ) ;
#37312 = CARTESIAN_POINT ( 'NONE',  ( 24.16423886937410614, 9.512082168247301794, -3.795296366450302550 ) ) ;
#37313 = CARTESIAN_POINT ( 'NONE',  ( 17.20831665107776587, 2.883931151000785231, 7.208316651077764980 ) ) ;
#37314 = CARTESIAN_POINT ( 'NONE',  ( 7.084665262690076126, 24.10535201082150181, 10.88017736071109987 ) ) ;
#37315 = VERTEX_POINT ( 'NONE', #41176 ) ;
#37316 = CARTESIAN_POINT ( 'NONE',  ( 4.559911319644449179, 23.89701867748817321, 9.422509992056141925 ) ) ;
#37317 = AXIS2_PLACEMENT_3D ( 'NONE', #22591, #84563, #16065 ) ;
#37318 = VERTEX_POINT ( 'NONE', #42628 ) ;
#37319 = CARTESIAN_POINT ( 'NONE',  ( 17.96484262340118221, 31.18868534415483751, -7.964842623401177768 ) ) ;
#37320 = CARTESIAN_POINT ( 'NONE',  ( 0.2751277870542875315, 65.30223176428830811, 6.499999999999984901 ) ) ;
#37321 = ORIENTED_EDGE ( 'NONE', *, *, #10567, .F. ) ;
#37322 = CIRCLE ( 'NONE', #85195, 14.49999999999999822 ) ;
#37323 = EDGE_CURVE ( 'NONE', #62057, #51581, #68061, .T. ) ;
#37324 = ORIENTED_EDGE ( 'NONE', *, *, #27880, .F. ) ;
#37325 = CARTESIAN_POINT ( 'NONE',  ( 22.81628187352648496, 11.83196800326375531, -3.434112377981050290 ) ) ;
#37326 = SURFACE_STYLE_USAGE ( .BOTH. , #83798 ) ;
#37327 = CARTESIAN_POINT ( 'NONE',  ( 10.00000000000000000, -0.2410688489992152128, -9.846743663894594434 ) ) ;
#37328 = CARTESIAN_POINT ( 'NONE',  ( 13.86186289918442505, 1.490777987167568597E-16, 4.667665767315075875 ) ) ;
#37330 = CARTESIAN_POINT ( 'NONE',  ( -0.1503990784575328643, 70.00000000000000000, -6.262539305110068177 ) ) ;
#37329 = CARTESIAN_POINT ( 'NONE',  ( 10.00000000000000000, 16.81368534415483751, -10.88017736071110342 ) ) ;
#37331 = CARTESIAN_POINT ( 'NONE',  ( 17.20831665107776587, 7.883931151000784787, 7.208316651077764980 ) ) ;
#37332 = CARTESIAN_POINT ( 'NONE',  ( 17.96484262340118221, 14.93868534415484106, 7.964842623401181321 ) ) ;
#37333 =( BOUNDED_SURFACE ( )  B_SPLINE_SURFACE ( 1, 2, ( 
 ( #6377, #50896, #96418, #27892, #37395, #58381, #81391, #36892, #36393, #73888, #19906, #97909, #82372, #80907, #20904, #97405, #67380, #74371, #12401, #29369, #90358, #43875, #42907, #21896, #66887, #73390, #4918, #12893, #5419, #58889, #51393, #35889, #28395, #81880, #92346, #68381, #84373, #24362, #67883, #8845, #46838, #62326, #60363, #16850, #31830, #76364, #91860, #68872, #98405, #39359, #69358, #60859, #7878, #98900, #22390, #85337, #38371, #9339, #29860, #7390, #53862, #402, #69853, #90859, #37888, #92834, #61351, #8359, #30854, #23378, #54825, #38867, #30352, #15872, #47325, #52866, #77824, #46357, #77333, #76845, #91359, #879, #83372, #22885, #31339, #45365, #61839, #23872, #54336, #84850, #16357, #1376, #14895, #75869, #53357, #83864, #15388, #45873, #71810, #94798, #1865, #3316, #17350, #33303, #17830, #2849, #47820, #93818, #72287, #9840, #78320, #79799, #56800, #48312, #63795, #2357, #19299, #94303, #33779, #80293, #71330, #18322, #79312, #11301, #25826, #40341, #26792, #32812, #70844, #78820, #63308, #56324, #25349, #93326, #87296, #55832, #86326, #10819, #32323, #24847, #10330, #48803, #70347, #64286, #18815, #34273, #40829, #86819, #95290, #41821, #41339, #26300, #49297, #3818, #64774, #57289, #49785, #87783, #39841, #62826, #55329, #85836, #21275, #4308, #34782, #50271, #89758, #20286, #29257, #36775, #88775, #81275, #5297, #89271, #59257, #36273, #50784, #66768, #97795, #28765, #90249, #20782, #12775, #28272, #51771, #73277, #43272, #73767, #35774, #82255, #51273, #96299, #74252, #59754, #66262, #13771, #96797, #58767, #43763, #81759, #5784, #13271, #21781, #65270, #58260, #97291, #44258, #95798, #72771, #80788, #42792, #35275, #27279, #12285, #4799, #67267, #57777, #88284, #74762, #52260, #6270, #11791, #42299, #65770, #19783, #27775, #8726, #22275, #15760, #68267, #52747, #84736, #7269, #90746, #23758, #61236, #15273, #69248, #1259, #54221, #14779, #91743, #45251, #37280, #29743, #75747, #769, #67769, #31715, #31221, #62211, #46246, #38747, #44751, #76731, #60253, #76251, #60738, #45754, #83256, #37771, #16241, #98786, #30234, #46723, #61717, #91240, #7765, #22764, #92716, #38260, #8249, #24242, #68751, #75254, #84257, #53245, #39244, #82755, #23263, #83750, #92232, #283, #30730, #53739, #14278, #77222, #69734, #6767, #98289, #2240, #64654, #56686, #18208, #39733, #48195, #56208, #48688, #33190, #34162, #26194, #64168, #2734, #95167, #41218, #25715, #63682, #71695, #93203, #87178, #17721, #78708, #79190, #70726, #93700, #10703, #55205, #71213, #11184, #54708, #94687, #33671, #49183, #47210, #3702 ),
 ( #9223, #72173, #25235, #85230, #16733, #24727, #40708, #63194, #18700, #77711, #85719, #79685, #10218, #94186, #55714, #86211, #41703, #86703, #17233, #3209, #70228, #1747, #32202, #62703, #47710, #78205, #9717, #40216, #32698, #65155, #96674, #4189, #73642, #12656, #88652, #13147, #50663, #81152, #58143, #82134, #5666, #80670, #59134, #95673, #27160, #66652, #43646, #35151, #20160, #88158, #6149, #43156, #58649, #67140, #5171, #19179, #28153, #73148, #13643, #74638, #35656, #57660, #36148, #50161, #19672, #12164, #36654, #42670, #4687, #97176, #66141, #65650, #26674, #28643, #89148, #11681, #20659, #51155, #81639, #74130, #57168, #89642, #21154, #51655, #87665, #44128, #49659, #80169, #42190, #96173, #72654, #34659, #27656, #61116, #14656, #37644, #23141, #98160, #15148, #54103, #97665, #38624, #76614, #92112, #90126, #46604, #161, #45627, #7140, #68631, #29131, #69125, #30610, #90620, #68141, #29616, #52140, #16120, #98668, #39125, #59635, #37154, #83633, #30114, #657, #21656, #67650, #61598, #91121, #38145, #60620, #22644, #23643, #91625, #60122, #53124, #77103, #82636, #8616, #76126, #8131, #7652, #22144, #53614, #14153, #52628, #84132, #75131, #15644, #46126, #31105, #84616, #44637, #6636, #83131, #45121, #75628, #10585, #2622, #41096, #17607, #10102, #31596, #86096, #16616, #9598, #24618, #40101, #47092, #71593, #94082, #48077, #24123, #70602, #55602, #78590, #63083, #3104, #25602, #33077, #93583, #69612, #71096, #40599, #25119, #63573, #77590, #56094, #2128, #32588, #86587, #55084, #17119, #18096, #9105, #48573, #79072, #1134, #62090, #92599, #54592, #39619, #85105, #70108, #1633, #32084, #62582, #93087, #85604, #47601, #78095, #68461, #60448, #14477, #77410, #30435, #1453, #59952, #98488, #45955, #98983, #956, #82961, #29944, #23948, #53437, #481, #60936, #91445, #84929, #30928, #90939, #15472, #8925, #21983, #39440, #22970, #69436, #76443, #22467, #7959, #44950, #52944, #61428, #37475, #38455, #68950, #83946, #46436, #91936, #23464, #53940, #16441, #38945, #69934, #8439, #90442, #84447, #15944, #52457, #76929, #67965, #31416, #37972, #61920, #83454, #14976, #92423, #45446, #75949, #54418, #46917, #75454, #6968, #7474, #9653, #16667, #71143, #79122, #46658, #62139, #2671, #32133, #41147, #48618, #1681, #93137, #17168, #2177, #33122, #48128, #62633, #78644, #10635, #40645, #3143, #32635, #77638, #56142, #92647, #24171, #63616, #94123, #24664, #85648, #85159, #69664, #47648, #47141, #25169, #78143, #16173, #55645, #70164, #71632, #33605, #63133, #54642, #25649, #9155, #39673, #55134, #64101, #40150, #70655 ) ),
 .UNSPECIFIED., .F., .F., .F. ) 
 B_SPLINE_SURFACE_WITH_KNOTS ( ( 2, 2 ),
 ( 3, 2, 2, 2, 2, 2, 2, 2, 2, 2, 2, 2, 2, 2, 2, 2, 2, 2, 2, 2, 2, 2, 2, 2, 2, 2, 2, 2, 2, 2, 2, 2, 2, 2, 2, 2, 2, 2, 2, 2, 2, 2, 2, 2, 2, 2, 2, 2, 2, 2, 2, 2, 2, 2, 2, 2, 2, 2, 2, 2, 2, 2, 2, 2, 2, 2, 2, 2, 2, 2, 2, 2, 2, 2, 2, 2, 2, 2, 2, 2, 2, 2, 2, 2, 2, 2, 2, 2, 2, 2, 2, 2, 2, 2, 2, 2, 2, 2, 2, 2, 2, 2, 2, 2, 2, 2, 2, 2, 2, 2, 2, 2, 2, 2, 2, 2, 2, 2, 2, 2, 2, 2, 2, 2, 2, 2, 2, 2, 2, 2, 2, 2, 2, 2, 2, 2, 2, 2, 2, 2, 2, 2, 2, 2, 2, 2, 2, 2, 2, 2, 2, 2, 2, 2, 2, 2, 2, 2, 2, 2, 2, 2, 3 ),
 ( 0.000000000000000000, 1.000000000000000000 ),
 ( 0.000000000000000000, 0.005952380952380952051, 0.01190476190476190410, 0.01785714285714285615, 0.02380952380952380820, 0.02976190476190476025, 0.03571428571428571230, 0.04166666666666666435, 0.04761904761904761640, 0.05357142857142856845, 0.05952380952380952051, 0.06547619047619047949, 0.07142857142857142461, 0.07738095238095238360, 0.08333333333333332871, 0.08928571428571428770, 0.09523809523809523281, 0.1011904761904761918, 0.1071428571428571369, 0.1130952380952380959, 0.1190476190476190410, 0.1250000000000000000, 0.1309523809523809590, 0.1369047619047619180, 0.1428571428571428492, 0.1488095238095238082, 0.1547619047619047672, 0.1607142857142857262, 0.1666666666666666574, 0.1726190476190476164, 0.1785714285714285754, 0.1845238095238095344, 0.1904761904761904656, 0.1964285714285714246, 0.2023809523809523836, 0.2083333333333333426, 0.2142857142857142738, 0.2202380952380952328, 0.2261904761904761918, 0.2321428571428571508, 0.2380952380952380820, 0.2440476190476190410, 0.2500000000000000000, 0.2559523809523809312, 0.2619047619047619180, 0.2678571428571428492, 0.2738095238095238360, 0.2797619047619047672, 0.2857142857142856984, 0.2916666666666666852, 0.2976190476190476164, 0.3035714285714285476, 0.3095238095238095344, 0.3154761904761904656, 0.3214285714285714524, 0.3273809523809523836, 0.3333333333333333148, 0.3392857142857143016, 0.3452380952380952328, 0.3511904761904761640, 0.3571428571428571508, 0.3630952380952380820, 0.3690476190476190688, 0.3750000000000000000, 0.3809523809523809312, 0.3869047619047619180, 0.3928571428571428492, 0.3988095238095238360, 0.4047619047619047672, 0.4107142857142856984, 0.4166666666666666852, 0.4226190476190476164, 0.4285714285714285476, 0.4345238095238095344, 0.4404761904761904656, 0.4464285714285714524, 0.4523809523809523836, 0.4583333333333333148, 0.4642857142857143016, 0.4702380952380952328, 0.4761904761904761640, 0.4821428571428571508, 0.4880952380952380820, 0.4940476190476190688, 0.5000000000000000000, 0.5059523809523809312, 0.5119047619047618625, 0.5178571428571429047, 0.5238095238095238360, 0.5297619047619047672, 0.5357142857142856984, 0.5416666666666666297, 0.5476190476190476719, 0.5535714285714286031, 0.5595238095238095344, 0.5654761904761904656, 0.5714285714285713969, 0.5773809523809523281, 0.5833333333333333703, 0.5892857142857143016, 0.5952380952380952328, 0.6011904761904761640, 0.6071428571428570953, 0.6130952380952381375, 0.6190476190476190688, 0.6250000000000000000, 0.6309523809523809312, 0.6369047619047618625, 0.6428571428571429047, 0.6488095238095238360, 0.6547619047619047672, 0.6607142857142856984, 0.6666666666666666297, 0.6726190476190476719, 0.6785714285714286031, 0.6845238095238095344, 0.6904761904761904656, 0.6964285714285713969, 0.7023809523809523281, 0.7083333333333333703, 0.7142857142857143016, 0.7202380952380952328, 0.7261904761904761640, 0.7321428571428570953, 0.7380952380952381375, 0.7440476190476190688, 0.7500000000000000000, 0.7559523809523809312, 0.7619047619047618625, 0.7678571428571429047, 0.7738095238095238360, 0.7797619047619047672, 0.7857142857142856984, 0.7916666666666666297, 0.7976190476190476719, 0.8035714285714286031, 0.8095238095238095344, 0.8154761904761904656, 0.8214285714285713969, 0.8273809523809523281, 0.8333333333333333703, 0.8392857142857143016, 0.8452380952380952328, 0.8511904761904761640, 0.8571428571428570953, 0.8630952380952381375, 0.8690476190476190688, 0.8750000000000000000, 0.8809523809523809312, 0.8869047619047618625, 0.8928571428571429047, 0.8988095238095238360, 0.9047619047619047672, 0.9107142857142856984, 0.9166666666666666297, 0.9226190476190476719, 0.9285714285714286031, 0.9345238095238095344, 0.9404761904761904656, 0.9464285714285713969, 0.9523809523809523281, 0.9583333333333333703, 0.9642857142857143016 ),
 .UNSPECIFIED. ) 
 GEOMETRIC_REPRESENTATION_ITEM ( )  RATIONAL_B_SPLINE_SURFACE ( (
 ( 1.000000000000000000, 0.9659258262890683122, 1.000000000000000000, 0.9659258262890683122, 1.000000000000000000, 0.9659258262890683122, 1.000000000000000000, 0.9659258262890683122, 1.000000000000000000, 0.9659258262890683122, 1.000000000000000000, 0.9659258262890683122, 1.000000000000000000, 0.9659258262890683122, 1.000000000000000000, 0.9659258262890683122, 1.000000000000000000, 0.9659258262890683122, 1.000000000000000000, 0.9659258262890683122, 1.000000000000000000, 0.9659258262890683122, 1.000000000000000000, 0.9659258262890683122, 1.000000000000000000, 0.9659258262890683122, 1.000000000000000000, 0.9659258262890683122, 1.000000000000000000, 0.9659258262890683122, 1.000000000000000000, 0.9659258262890683122, 1.000000000000000000, 0.9659258262890683122, 1.000000000000000000, 0.9659258262890683122, 1.000000000000000000, 0.9659258262890683122, 1.000000000000000000, 0.9659258262890683122, 1.000000000000000000, 0.9659258262890683122, 1.000000000000000000, 0.9659258262890683122, 1.000000000000000000, 0.9659258262890683122, 1.000000000000000000, 0.9659258262890683122, 1.000000000000000000, 0.9659258262890683122, 1.000000000000000000, 0.9659258262890683122, 1.000000000000000000, 0.9659258262890683122, 1.000000000000000000, 0.9659258262890683122, 1.000000000000000000, 0.9659258262890683122, 1.000000000000000000, 0.9659258262890683122, 1.000000000000000000, 0.9659258262890683122, 1.000000000000000000, 0.9659258262890683122, 1.000000000000000000, 0.9659258262890683122, 1.000000000000000000, 0.9659258262890683122, 1.000000000000000000, 0.9659258262890683122, 1.000000000000000000, 0.9659258262890683122, 1.000000000000000000, 0.9659258262890683122, 1.000000000000000000, 0.9659258262890683122, 1.000000000000000000, 0.9659258262890683122, 1.000000000000000000, 0.9659258262890683122, 1.000000000000000000, 0.9659258262890683122, 1.000000000000000000, 0.9659258262890683122, 1.000000000000000000, 0.9659258262890683122, 1.000000000000000000, 0.9659258262890683122, 1.000000000000000000, 0.9659258262890683122, 1.000000000000000000, 0.9659258262890683122, 1.000000000000000000, 0.9659258262890683122, 1.000000000000000000, 0.9659258262890683122, 1.000000000000000000, 0.9659258262890683122, 1.000000000000000000, 0.9659258262890683122, 1.000000000000000000, 0.9659258262890683122, 1.000000000000000000, 0.9659258262890683122, 1.000000000000000000, 0.9659258262890683122, 1.000000000000000000, 0.9659258262890683122, 1.000000000000000000, 0.9659258262890683122, 1.000000000000000000, 0.9659258262890683122, 1.000000000000000000, 0.9659258262890683122, 1.000000000000000000, 0.9659258262890683122, 1.000000000000000000, 0.9659258262890683122, 1.000000000000000000, 0.9659258262890683122, 1.000000000000000000, 0.9659258262890683122, 1.000000000000000000, 0.9659258262890683122, 1.000000000000000000, 0.9659258262890683122, 1.000000000000000000, 0.9659258262890683122, 1.000000000000000000, 0.9659258262890683122, 1.000000000000000000, 0.9659258262890683122, 1.000000000000000000, 0.9659258262890683122, 1.000000000000000000, 0.9659258262890683122, 1.000000000000000000, 0.9659258262890683122, 1.000000000000000000, 0.9659258262890683122, 1.000000000000000000, 0.9659258262890683122, 1.000000000000000000, 0.9659258262890683122, 1.000000000000000000, 0.9659258262890683122, 1.000000000000000000, 0.9659258262890683122, 1.000000000000000000, 0.9659258262890683122, 1.000000000000000000, 0.9659258262890683122, 1.000000000000000000, 0.9659258262890683122, 1.000000000000000000, 0.9659258262890683122, 1.000000000000000000, 0.9659258262890683122, 1.000000000000000000, 0.9659258262890683122, 1.000000000000000000, 0.9659258262890683122, 1.000000000000000000, 0.9659258262890683122, 1.000000000000000000, 0.9659258262890683122, 1.000000000000000000, 0.9659258262890683122, 1.000000000000000000, 0.9659258262890683122, 1.000000000000000000, 0.9659258262890683122, 1.000000000000000000, 0.9659258262890683122, 1.000000000000000000, 0.9659258262890683122, 1.000000000000000000, 0.9659258262890683122, 1.000000000000000000, 0.9659258262890683122, 1.000000000000000000, 0.9659258262890683122, 1.000000000000000000, 0.9659258262890683122, 1.000000000000000000, 0.9659258262890683122, 1.000000000000000000, 0.9659258262890683122, 1.000000000000000000, 0.9659258262890683122, 1.000000000000000000, 0.9659258262890683122, 1.000000000000000000, 0.9659258262890683122, 1.000000000000000000, 0.9659258262890683122, 1.000000000000000000, 0.9659258262890683122, 1.000000000000000000, 0.9659258262890683122, 1.000000000000000000, 0.9659258262890683122, 1.000000000000000000, 0.9659258262890683122, 1.000000000000000000, 0.9659258262890683122, 1.000000000000000000, 0.9659258262890683122, 1.000000000000000000, 0.9659258262890683122, 1.000000000000000000, 0.9659258262890683122, 1.000000000000000000, 0.9659258262890683122, 1.000000000000000000, 0.9659258262890683122, 1.000000000000000000, 0.9659258262890683122, 1.000000000000000000, 0.9659258262890683122, 1.000000000000000000, 0.9659258262890683122, 1.000000000000000000, 0.9659258262890683122, 1.000000000000000000, 0.9659258262890683122, 1.000000000000000000, 0.9659258262890683122, 1.000000000000000000, 0.9659258262890683122, 1.000000000000000000, 0.9659258262890683122, 1.000000000000000000, 0.9659258262890683122, 1.000000000000000000, 0.9659258262890683122, 1.000000000000000000, 0.9659258262890683122, 1.000000000000000000, 0.9659258262890683122, 1.000000000000000000, 0.9659258262890683122, 1.000000000000000000, 0.9659258262890683122, 1.000000000000000000, 0.9659258262890683122, 1.000000000000000000, 0.9659258262890683122, 1.000000000000000000, 0.9659258262890683122, 1.000000000000000000, 0.9659258262890683122, 1.000000000000000000, 0.9659258262890683122, 1.000000000000000000, 0.9659258262890683122, 1.000000000000000000, 0.9659258262890683122, 1.000000000000000000, 0.9659258262890683122, 1.000000000000000000, 0.9659258262890683122, 1.000000000000000000, 0.9659258262890683122, 1.000000000000000000, 0.9659258262890683122, 1.000000000000000000, 0.9659258262890683122, 1.000000000000000000, 0.9659258262890683122, 1.000000000000000000, 0.9659258262890683122, 1.000000000000000000, 0.9659258262890683122, 1.000000000000000000, 0.9659258262890683122, 1.000000000000000000, 0.9659258262890683122, 1.000000000000000000, 0.9659258262890683122, 1.000000000000000000, 0.9659258262890683122, 1.000000000000000000, 0.9659258262890683122, 1.000000000000000000, 0.9659258262890683122, 1.000000000000000000, 0.9659258262890683122, 1.000000000000000000, 0.9659258262890683122, 1.000000000000000000, 0.9659258262890683122, 1.000000000000000000, 0.9659258262890683122, 1.000000000000000000, 0.9659258262890683122, 1.000000000000000000, 0.9659258262890683122, 1.000000000000000000, 0.9659258262890683122, 1.000000000000000000, 0.9659258262890683122, 1.000000000000000000, 0.9659258262890683122, 1.000000000000000000, 0.9659258262890683122, 1.000000000000000000, 0.9659258262890683122, 1.000000000000000000, 0.9659258262890683122, 1.000000000000000000, 0.9659258262890683122, 1.000000000000000000, 0.9659258262890683122, 1.000000000000000000, 0.9659258262890683122, 1.000000000000000000, 0.9659258262890683122, 1.000000000000000000, 0.9659258262890683122, 1.000000000000000000, 0.9659258262890683122, 1.000000000000000000, 0.9659258262890683122, 1.000000000000000000),
 ( 1.000000000000000000, 0.9659258262890683122, 1.000000000000000000, 0.9659258262890683122, 1.000000000000000000, 0.9659258262890683122, 1.000000000000000000, 0.9659258262890683122, 1.000000000000000000, 0.9659258262890683122, 1.000000000000000000, 0.9659258262890683122, 1.000000000000000000, 0.9659258262890683122, 1.000000000000000000, 0.9659258262890683122, 1.000000000000000000, 0.9659258262890683122, 1.000000000000000000, 0.9659258262890683122, 1.000000000000000000, 0.9659258262890683122, 1.000000000000000000, 0.9659258262890683122, 1.000000000000000000, 0.9659258262890683122, 1.000000000000000000, 0.9659258262890683122, 1.000000000000000000, 0.9659258262890683122, 1.000000000000000000, 0.9659258262890683122, 1.000000000000000000, 0.9659258262890683122, 1.000000000000000000, 0.9659258262890683122, 1.000000000000000000, 0.9659258262890683122, 1.000000000000000000, 0.9659258262890683122, 1.000000000000000000, 0.9659258262890683122, 1.000000000000000000, 0.9659258262890683122, 1.000000000000000000, 0.9659258262890683122, 1.000000000000000000, 0.9659258262890683122, 1.000000000000000000, 0.9659258262890683122, 1.000000000000000000, 0.9659258262890683122, 1.000000000000000000, 0.9659258262890683122, 1.000000000000000000, 0.9659258262890683122, 1.000000000000000000, 0.9659258262890683122, 1.000000000000000000, 0.9659258262890683122, 1.000000000000000000, 0.9659258262890683122, 1.000000000000000000, 0.9659258262890683122, 1.000000000000000000, 0.9659258262890683122, 1.000000000000000000, 0.9659258262890683122, 1.000000000000000000, 0.9659258262890683122, 1.000000000000000000, 0.9659258262890683122, 1.000000000000000000, 0.9659258262890683122, 1.000000000000000000, 0.9659258262890683122, 1.000000000000000000, 0.9659258262890683122, 1.000000000000000000, 0.9659258262890683122, 1.000000000000000000, 0.9659258262890683122, 1.000000000000000000, 0.9659258262890683122, 1.000000000000000000, 0.9659258262890683122, 1.000000000000000000, 0.9659258262890683122, 1.000000000000000000, 0.9659258262890683122, 1.000000000000000000, 0.9659258262890683122, 1.000000000000000000, 0.9659258262890683122, 1.000000000000000000, 0.9659258262890683122, 1.000000000000000000, 0.9659258262890683122, 1.000000000000000000, 0.9659258262890683122, 1.000000000000000000, 0.9659258262890683122, 1.000000000000000000, 0.9659258262890683122, 1.000000000000000000, 0.9659258262890683122, 1.000000000000000000, 0.9659258262890683122, 1.000000000000000000, 0.9659258262890683122, 1.000000000000000000, 0.9659258262890683122, 1.000000000000000000, 0.9659258262890683122, 1.000000000000000000, 0.9659258262890683122, 1.000000000000000000, 0.9659258262890683122, 1.000000000000000000, 0.9659258262890683122, 1.000000000000000000, 0.9659258262890683122, 1.000000000000000000, 0.9659258262890683122, 1.000000000000000000, 0.9659258262890683122, 1.000000000000000000, 0.9659258262890683122, 1.000000000000000000, 0.9659258262890683122, 1.000000000000000000, 0.9659258262890683122, 1.000000000000000000, 0.9659258262890683122, 1.000000000000000000, 0.9659258262890683122, 1.000000000000000000, 0.9659258262890683122, 1.000000000000000000, 0.9659258262890683122, 1.000000000000000000, 0.9659258262890683122, 1.000000000000000000, 0.9659258262890683122, 1.000000000000000000, 0.9659258262890683122, 1.000000000000000000, 0.9659258262890683122, 1.000000000000000000, 0.9659258262890683122, 1.000000000000000000, 0.9659258262890683122, 1.000000000000000000, 0.9659258262890683122, 1.000000000000000000, 0.9659258262890683122, 1.000000000000000000, 0.9659258262890683122, 1.000000000000000000, 0.9659258262890683122, 1.000000000000000000, 0.9659258262890683122, 1.000000000000000000, 0.9659258262890683122, 1.000000000000000000, 0.9659258262890683122, 1.000000000000000000, 0.9659258262890683122, 1.000000000000000000, 0.9659258262890683122, 1.000000000000000000, 0.9659258262890683122, 1.000000000000000000, 0.9659258262890683122, 1.000000000000000000, 0.9659258262890683122, 1.000000000000000000, 0.9659258262890683122, 1.000000000000000000, 0.9659258262890683122, 1.000000000000000000, 0.9659258262890683122, 1.000000000000000000, 0.9659258262890683122, 1.000000000000000000, 0.9659258262890683122, 1.000000000000000000, 0.9659258262890683122, 1.000000000000000000, 0.9659258262890683122, 1.000000000000000000, 0.9659258262890683122, 1.000000000000000000, 0.9659258262890683122, 1.000000000000000000, 0.9659258262890683122, 1.000000000000000000, 0.9659258262890683122, 1.000000000000000000, 0.9659258262890683122, 1.000000000000000000, 0.9659258262890683122, 1.000000000000000000, 0.9659258262890683122, 1.000000000000000000, 0.9659258262890683122, 1.000000000000000000, 0.9659258262890683122, 1.000000000000000000, 0.9659258262890683122, 1.000000000000000000, 0.9659258262890683122, 1.000000000000000000, 0.9659258262890683122, 1.000000000000000000, 0.9659258262890683122, 1.000000000000000000, 0.9659258262890683122, 1.000000000000000000, 0.9659258262890683122, 1.000000000000000000, 0.9659258262890683122, 1.000000000000000000, 0.9659258262890683122, 1.000000000000000000, 0.9659258262890683122, 1.000000000000000000, 0.9659258262890683122, 1.000000000000000000, 0.9659258262890683122, 1.000000000000000000, 0.9659258262890683122, 1.000000000000000000, 0.9659258262890683122, 1.000000000000000000, 0.9659258262890683122, 1.000000000000000000, 0.9659258262890683122, 1.000000000000000000, 0.9659258262890683122, 1.000000000000000000, 0.9659258262890683122, 1.000000000000000000, 0.9659258262890683122, 1.000000000000000000, 0.9659258262890683122, 1.000000000000000000, 0.9659258262890683122, 1.000000000000000000, 0.9659258262890683122, 1.000000000000000000, 0.9659258262890683122, 1.000000000000000000, 0.9659258262890683122, 1.000000000000000000, 0.9659258262890683122, 1.000000000000000000, 0.9659258262890683122, 1.000000000000000000, 0.9659258262890683122, 1.000000000000000000, 0.9659258262890683122, 1.000000000000000000, 0.9659258262890683122, 1.000000000000000000, 0.9659258262890683122, 1.000000000000000000, 0.9659258262890683122, 1.000000000000000000, 0.9659258262890683122, 1.000000000000000000, 0.9659258262890683122, 1.000000000000000000, 0.9659258262890683122, 1.000000000000000000, 0.9659258262890683122, 1.000000000000000000, 0.9659258262890683122, 1.000000000000000000, 0.9659258262890683122, 1.000000000000000000, 0.9659258262890683122, 1.000000000000000000, 0.9659258262890683122, 1.000000000000000000, 0.9659258262890683122, 1.000000000000000000, 0.9659258262890683122, 1.000000000000000000, 0.9659258262890683122, 1.000000000000000000, 0.9659258262890683122, 1.000000000000000000, 0.9659258262890683122, 1.000000000000000000, 0.9659258262890683122, 1.000000000000000000, 0.9659258262890683122, 1.000000000000000000, 0.9659258262890683122, 1.000000000000000000, 0.9659258262890683122, 1.000000000000000000, 0.9659258262890683122, 1.000000000000000000, 0.9659258262890683122, 1.000000000000000000, 0.9659258262890683122, 1.000000000000000000, 0.9659258262890683122, 1.000000000000000000, 0.9659258262890683122, 1.000000000000000000, 0.9659258262890683122, 1.000000000000000000, 0.9659258262890683122, 1.000000000000000000, 0.9659258262890683122, 1.000000000000000000, 0.9659258262890683122, 1.000000000000000000, 0.9659258262890683122, 1.000000000000000000, 0.9659258262890683122, 1.000000000000000000) ) ) 
 REPRESENTATION_ITEM ( '' )  SURFACE ( )  );
#37334 = VERTEX_POINT ( 'NONE', #34615 ) ;
#37335 = CARTESIAN_POINT ( 'NONE',  ( -2.816281873526473856, 54.33196800326376064, 3.434112377981055619 ) ) ;
#37336 = CARTESIAN_POINT ( 'NONE',  ( 17.96484262340118221, 46.18868534415484106, -7.964842623401177768 ) ) ;
#37337 = DIRECTION ( 'NONE',  ( 0.000000000000000000, 1.000000000000000000, 0.000000000000000000 ) ) ;
#37338 = CARTESIAN_POINT ( 'NONE',  ( 19.38216949554541202, 50.99863466993042493, 9.382169495545424454 ) ) ;
#37339 = CARTESIAN_POINT ( 'NONE',  ( 12.91533473730993009, 46.60535201082150536, -10.88017736071109987 ) ) ;
#37340 = CARTESIAN_POINT ( 'NONE',  ( 0.1532563361054082862, 66.21726448433413736, 2.638427012816831674 ) ) ;
#37341 = DIRECTION ( 'NONE',  ( -0.5547001962252290364, -0.8320502943378437211, 0.000000000000000000 ) ) ;
#37342 = CARTESIAN_POINT ( 'NONE',  ( 0.1532563361054082862, 16.21726448433411960, 2.638427012816831674 ) ) ;
#37343 = CARTESIAN_POINT ( 'NONE',  ( 10.00000000000000000, 52.87363466993041783, -12.81628187352647608 ) ) ;
#37344 = CARTESIAN_POINT ( 'NONE',  ( 4.920097194114470440, -13.81670059445664300, -3.749999999999997780 ) ) ;
#37345 = CARTESIAN_POINT ( 'NONE',  ( 19.38216949554541557, 7.248634669930421381, -9.382169495545420901 ) ) ;
#37347 = FACE_OUTER_BOUND ( 'NONE', #94859, .T. ) ;
#37346 = PRESENTATION_STYLE_ASSIGNMENT (( #68821 ) ) ;
#37348 = CARTESIAN_POINT ( 'NONE',  ( 4.559911319644449179, 42.23035201082151247, -9.422509992056141925 ) ) ;
#37349 = CARTESIAN_POINT ( 'NONE',  ( 10.00000000000000178, 52.25893115100078745, 9.846743663894594434 ) ) ;
#37350 = CARTESIAN_POINT ( 'NONE',  ( -0.000000000000000000, 37.25000000000000000, -3.750000000000000000 ) ) ;
#37351 = CARTESIAN_POINT ( 'NONE',  ( 12.63842701281683034, 22.46726448433411605, 9.846743663894596210 ) ) ;
#37352 = CARTESIAN_POINT ( 'NONE',  ( 12.63842701281683034, 12.46726448433411782, 9.846743663894596210 ) ) ;
#37354 = ORIENTED_EDGE ( 'NONE', *, *, #49422, .F. ) ;
#37353 = CARTESIAN_POINT ( 'NONE',  ( 22.81628187352648496, 1.831968003263753753, -3.434112377981050290 ) ) ;
#37355 = CARTESIAN_POINT ( 'NONE',  ( 20.88017736071110875, 5.772018677488170546, -2.915334737309920765 ) ) ;
#37356 = CARTESIAN_POINT ( 'NONE',  ( 18.52753015748618282, 63.92559781766745886, -4.923371831947291888 ) ) ;
#37357 = CARTESIAN_POINT ( 'NONE',  ( -0.8801773607110991993, 7.855352010821506248, -2.915334737309923874 ) ) ;
#37358 = CARTESIAN_POINT ( 'NONE',  ( 2.791683348922237240, 40.38393115100078035, -7.208316651077763204 ) ) ;
#37359 = ORIENTED_EDGE ( 'NONE', *, *, #6837, .T. ) ;
#37360 = DIRECTION ( 'NONE',  ( -1.000000000000000000, 0.000000000000000000, 0.000000000000000000 ) ) ;
#37361 = CARTESIAN_POINT ( 'NONE',  ( 2.035157376598824452, 3.688685344154837953, 7.964842623401179544 ) ) ;
#37362 = FACE_OUTER_BOUND ( 'NONE', #54130, .T. ) ;
#37363 = CARTESIAN_POINT ( 'NONE',  ( 7.084665262690076126, 14.10535201082150358, 10.88017736071109987 ) ) ;
#37364 = CARTESIAN_POINT ( 'NONE',  ( 6.204703633549690345, 45.76208216824729647, -14.16423886937410259 ) ) ;
#37366 = DIRECTION ( 'NONE',  ( 0.000000000000000000, 1.000000000000000000, 0.000000000000000000 ) ) ;
#37365 = CARTESIAN_POINT ( 'NONE',  ( 22.26659068614895176, 64.72041550158064638, -7.082119434687042414 ) ) ;
#37367 = CARTESIAN_POINT ( 'NONE',  ( 2.791683348922237240, 0.3839311510007847872, -7.208316651077763204 ) ) ;
#37368 = CARTESIAN_POINT ( 'NONE',  ( 19.84674366389459266, 23.71726448433412315, -2.638427012816827677 ) ) ;
#37369 = CARTESIAN_POINT ( 'NONE',  ( -1.099225684535947600, 9.540301336597087456, 6.408140936763237150 ) ) ;
#37370 = DIRECTION ( 'NONE',  ( 0.000000000000000000, 0.000000000000000000, 1.000000000000000000 ) ) ;
#37371 = CARTESIAN_POINT ( 'NONE',  ( -41.28048780487802105, 33.02439024390238131, -8.000000000000000000 ) ) ;
#37372 = ADVANCED_FACE ( 'NONE', ( #71657 ), #10626, .T. ) ;
#37373 = CARTESIAN_POINT ( 'NONE',  ( 10.00000000000000178, 57.25893115100078745, 9.846743663894594434 ) ) ;
#37374 = DIRECTION ( 'NONE',  ( 8.881784197001252323E-16, 0.000000000000000000, 1.000000000000000000 ) ) ;
#37375 = DIRECTION ( 'NONE',  ( 0.02970531260826360376, -0.9995586998285020952, -0.000000000000000000 ) ) ;
#37376 = CARTESIAN_POINT ( 'NONE',  ( 22.26659068614895176, 9.720415501580633943, -7.082119434687042414 ) ) ;
#37377 = CARTESIAN_POINT ( 'NONE',  ( 2.791683348922237240, 30.38393115100078390, -7.208316651077763204 ) ) ;
#37378 =( NAMED_UNIT ( * ) PLANE_ANGLE_UNIT ( ) SI_UNIT ( $, .RADIAN. ) );
#37379 = ORIENTED_EDGE ( 'NONE', *, *, #97512, .F. ) ;
#37380 = VECTOR ( 'NONE', #4702, 1000.000000000000000 ) ;
#37381 = CARTESIAN_POINT ( 'NONE',  ( -4.164238869374099927, 42.01208216824728936, 3.795296366450308767 ) ) ;
#37382 = CARTESIAN_POINT ( 'NONE',  ( 1.472469842513823179, 6.425597817667451750, 4.923371831947296329 ) ) ;
#37384 = DIRECTION ( 'NONE',  ( 0.000000000000000000, -1.000000000000000000, 0.000000000000000000 ) ) ;
#37383 = DIRECTION ( 'NONE',  ( 0.000000000000000000, 1.000000000000000000, 0.000000000000000000 ) ) ;
#37385 = CARTESIAN_POINT ( 'NONE',  ( 0.5774900079438590739, 27.64701867748817676, -5.440088680355550821 ) ) ;
#37386 = CARTESIAN_POINT ( 'NONE',  ( 13.43411237798105340, 50.58196800326375353, 12.81628187352647963 ) ) ;
#37387 = CARTESIAN_POINT ( 'NONE',  ( -0.8801773607111008646, 8.272018677488171434, 2.915334737309923430 ) ) ;
#37388 = CARTESIAN_POINT ( 'NONE',  ( 16.40814093676323893, 35.79030133659708923, 11.09922568453595026 ) ) ;
#37389 = CARTESIAN_POINT ( 'NONE',  ( 1.472469842513823179, 5.592264484334118713, -4.923371831947296329 ) ) ;
#37390 = ORIENTED_EDGE ( 'NONE', *, *, #55770, .F. ) ;
#37391 = CIRCLE ( 'NONE', #8612, 14.49999999999999822 ) ;
#37392 =( NAMED_UNIT ( * ) PLANE_ANGLE_UNIT ( ) SI_UNIT ( $, .RADIAN. ) );
#37393 = CARTESIAN_POINT ( 'NONE',  ( 14.88232117145529720, 15.00000000000000000, 1.875237731503240024 ) ) ;
#37394 = CARTESIAN_POINT ( 'NONE',  ( 20.36894250292379382, 38.67874883491396076, 10.36894250292379205 ) ) ;
#37395 = CARTESIAN_POINT ( 'NONE',  ( -2.266590686148945544, 1.387082168247301128, -7.082119434687050408 ) ) ;
#37396 = CARTESIAN_POINT ( 'NONE',  ( 19.42250999205614193, 10.14701867748816966, 5.440088680355555262 ) ) ;
#37397 = CARTESIAN_POINT ( 'NONE',  ( 4.559911319644449179, 22.23035201082150536, -9.422509992056141925 ) ) ;
#37398 = DIRECTION ( 'NONE',  ( -0.2334453638559087219, 0.000000000000000000, 0.9723699203976758909 ) ) ;
#37399 = DIRECTION ( 'NONE',  ( 0.000000000000000000, 1.000000000000000000, 0.000000000000000000 ) ) ;
#37400 = CARTESIAN_POINT ( 'NONE',  ( 17.96484262340118221, 51.18868534415483396, -7.964842623401177768 ) ) ;
#37401 = CARTESIAN_POINT ( 'NONE',  ( 20.88017736071110519, 60.56368534415484106, 2.639326808657452039E-16 ) ) ;
#37402 = CARTESIAN_POINT ( 'NONE',  ( -1.099225684535947600, 28.70696800326375353, -6.408140936763238038 ) ) ;
#37403 = LINE ( 'NONE', #51401, #63454 ) ;
#37404 = CARTESIAN_POINT ( 'NONE',  ( -10.32896413005680536, 2.245456701841147762, -5.963430220938272797 ) ) ;
#37405 = CARTESIAN_POINT ( 'NONE',  ( 10.00000000000000000, 24.75893115100078745, -9.846743663894594434 ) ) ;
#37406 = CARTESIAN_POINT ( 'NONE',  ( 2.035157376598824452, 58.68868534415482685, 7.964842623401179544 ) ) ;
#37407 = EDGE_CURVE ( 'NONE', #85917, #66682, #28171, .T. ) ;
#37408 = CARTESIAN_POINT ( 'NONE',  ( -2.816281873526473856, 19.33196800326375708, 3.434112377981055619 ) ) ;
#37409 = B_SPLINE_CURVE_WITH_KNOTS ( 'NONE', 3,
 ( #56332, #18824, #3324, #11308, #64294, #95806 ),
 .UNSPECIFIED., .F., .F.,
 ( 4, 2, 4 ),
 ( 3.409110551493783393E-05, 0.0004400426677367841322, 0.0008459942299586303491 ),
 .UNSPECIFIED. ) ;
#37410 = CARTESIAN_POINT ( 'NONE',  ( 0.8952175423694819223, 43.52576239577081907, 5.990408912944316100 ) ) ;
#37411 = CARTESIAN_POINT ( 'NONE',  ( 10.00000000000000178, 9.313685344154839285, 10.88017736071110342 ) ) ;
#37412 = CARTESIAN_POINT ( 'NONE',  ( 14.92337183194729633, 42.67559781766745886, 8.527530157486181039 ) ) ;
#37413 = CARTESIAN_POINT ( 'NONE',  ( 22.81628187352648496, 56.83196800326374643, -3.434112377981050290 ) ) ;
#37414 = CARTESIAN_POINT ( 'NONE',  ( 14.92337183194729988, 19.34226448433411960, -8.527530157486177487 ) ) ;
#37415 = EDGE_CURVE ( 'NONE', #85865, #2342, #20795, .T. ) ;
#37416 = CARTESIAN_POINT ( 'NONE',  ( 34.56412365047463453, 26.99999999999999645, 9.500000000000000000 ) ) ;
#37417 = CARTESIAN_POINT ( 'NONE',  ( 19.42250999205614548, 30.98035201082150536, -5.440088680355545492 ) ) ;
#37419 = CARTESIAN_POINT ( 'NONE',  ( 22.26659068614894466, 33.88708216824730357, 7.082119434687054849 ) ) ;
#37418 = CARTESIAN_POINT ( 'NONE',  ( 7.084665262690076126, 4.105352010821503583, 10.88017736071109987 ) ) ;
#37420 = CARTESIAN_POINT ( 'NONE',  ( 2.791683348922240793, 41.63393115100078745, 7.208316651077764092 ) ) ;
#37421 = CARTESIAN_POINT ( 'NONE',  ( 12.91533473730992121, 34.52201867748817676, 10.88017736071110164 ) ) ;
#37422 = CARTESIAN_POINT ( 'NONE',  ( 20.88017736071110164, 10.35535201082150714, 2.915334737309930979 ) ) ;
#37423 = ORIENTED_EDGE ( 'NONE', *, *, #15028, .F. ) ;
#37424 = CARTESIAN_POINT ( 'NONE',  ( 19.42250999205614193, 25.14701867748817321, 5.440088680355555262 ) ) ;
#37425 = CARTESIAN_POINT ( 'NONE',  ( 22.81628187352647785, 41.62363466993042493, 6.195893100308588602E-16 ) ) ;
#37426 = CARTESIAN_POINT ( 'NONE',  ( 19.42250999205614193, 50.14701867748817676, 5.440088680355555262 ) ) ;
#37427 =( LENGTH_UNIT ( ) NAMED_UNIT ( * ) SI_UNIT ( .MILLI., .METRE. ) );
#37428 = EDGE_LOOP ( 'NONE', ( #55866, #89257, #464, #47897 ) ) ;
#37429 = CARTESIAN_POINT ( 'NONE',  ( 1.472469842513823179, 60.59226448433412315, -4.923371831947296329 ) ) ;
#37430 = CARTESIAN_POINT ( 'NONE',  ( 0.5774900079438590739, 42.64701867748816966, -5.440088680355550821 ) ) ;
#37431 = CARTESIAN_POINT ( 'NONE',  ( 7.007893109692266087, -58.32153039260716554, 4.000000000000000000 ) ) ;
#37432 = CARTESIAN_POINT ( 'NONE',  ( 19.89103541497711447, 30.66234555792570049, -6.479102184480773907 ) ) ;
#37433 = CARTESIAN_POINT ( 'NONE',  ( 10.00000000000000178, 48.05374883491396787, 14.16423886937410082 ) ) ;
#37434 = CARTESIAN_POINT ( 'NONE',  ( 10.00000000000000000, 46.81368534415484106, -10.88017736071110342 ) ) ;
#37435 = DIRECTION ( 'NONE',  ( 0.000000000000000000, 1.000000000000000000, 0.000000000000000000 ) ) ;
#37436 = DIRECTION ( 'NONE',  ( 0.000000000000000000, 0.000000000000000000, 1.000000000000000000 ) ) ;
#37437 = CARTESIAN_POINT ( 'NONE',  ( 10.00000000000000178, 57.25893115100078745, 9.846743663894594434 ) ) ;
#37438 = CARTESIAN_POINT ( 'NONE',  ( 0.5774900079438607392, 3.480352010821504027, 5.440088680355550821 ) ) ;
#37439 = CARTESIAN_POINT ( 'NONE',  ( 12.63842701281683922, 29.55059781766745175, -9.846743663894590881 ) ) ;
#37440 = VERTEX_POINT ( 'NONE', #80128 ) ;
#37441 = CARTESIAN_POINT ( 'NONE',  ( 5.076628168052704559, 30.17559781766745175, -8.527530157486179263 ) ) ;
#37442 = CARTESIAN_POINT ( 'NONE',  ( 6.408140936763243367, -14.20969866340290899, 11.09922568453594494 ) ) ;
#37443 = CARTESIAN_POINT ( 'NONE',  ( -0.8801773607111008646, 23.27201867748817676, 2.915334737309923430 ) ) ;
#37444 = CARTESIAN_POINT ( 'NONE',  ( 18.52753015748618282, 28.92559781766745175, -4.923371831947291888 ) ) ;
#37445 = CARTESIAN_POINT ( 'NONE',  ( 13.43411237798106583, 22.66530133659708923, -12.81628187352647252 ) ) ;
#37447 = CARTESIAN_POINT ( 'NONE',  ( -0.8801773607110991993, 62.85535201082150536, -2.915334737309923874 ) ) ;
#37446 = CARTESIAN_POINT ( 'NONE',  ( 1.707155281725177609, 37.90189080397285437, 6.499999999999955591 ) ) ;
#37448 = CARTESIAN_POINT ( 'NONE',  ( 10.00000000000000000, 26.81368534415484106, -10.88017736071110342 ) ) ;
#37449 = CARTESIAN_POINT ( 'NONE',  ( -2.266590686148945544, 47.22041550158063927, 7.082119434687048631 ) ) ;
#37450 = EDGE_CURVE ( 'NONE', #37161, #17162, #12127, .T. ) ;
#37451 = VECTOR ( 'NONE', #10038, 1000.000000000000000 ) ;
#37452 = CARTESIAN_POINT ( 'NONE',  ( -9.519554572442809004, -3.087435092741923553E-15, -11.10344954678193119 ) ) ;
#37453 = ORIENTED_EDGE ( 'NONE', *, *, #19004, .F. ) ;
#37454 = B_SPLINE_CURVE_WITH_KNOTS ( 'NONE', 3,
 ( #11304, #80791, #37637, #96302, #50274, #43275 ),
 .UNSPECIFIED., .F., .F.,
 ( 4, 2, 4 ),
 ( 0.0002800005319541506261, 0.0006862057665733079306, 0.001092411001192465344 ),
 .UNSPECIFIED. ) ;
#37455 = CARTESIAN_POINT ( 'NONE',  ( -1.099225684535947600, 19.54030133659708568, 6.408140936763237150 ) ) ;
#37456 = CARTESIAN_POINT ( 'NONE',  ( -0.8801773607110991993, 7.855352010821504471, -2.915334737309923874 ) ) ;
#37457 = CARTESIAN_POINT ( 'NONE',  ( 7.084665262690076126, 49.10535201082149825, 10.88017736071109987 ) ) ;
#37458 = SURFACE_STYLE_FILL_AREA ( #6446 ) ;
#37459 = AXIS2_PLACEMENT_3D ( 'NONE', #66511, #66007, #97037 ) ;
#37460 = ORIENTED_EDGE ( 'NONE', *, *, #34736, .F. ) ;
#37461 = CARTESIAN_POINT ( 'NONE',  ( -0.8801773607110991993, 57.85535201082149825, -2.915334737309923874 ) ) ;
#37462 = CARTESIAN_POINT ( 'NONE',  ( 1.472469842513823179, 41.42559781766745886, 4.923371831947296329 ) ) ;
#37463 = CARTESIAN_POINT ( 'NONE',  ( 0.1532563361054082862, 26.21726448433411605, 2.638427012816831674 ) ) ;
#37464 = CARTESIAN_POINT ( 'NONE',  ( 19.84674366389459266, 13.30059781766745353, 2.638427012816836559 ) ) ;
#37466 = CARTESIAN_POINT ( 'NONE',  ( 6.565887622018943937, 35.16530133659708923, 12.81628187352647430 ) ) ;
#37465 = CARTESIAN_POINT ( 'NONE',  ( 4.219999999999999751, 10.25000000000000000, 2.500000000000000000 ) ) ;
#37468 = FACE_OUTER_BOUND ( 'NONE', #25040, .T. ) ;
#37467 = CARTESIAN_POINT ( 'NONE',  ( 18.52753015748617571, 18.09226448433411960, 4.923371831947298993 ) ) ;
#37469 = CARTESIAN_POINT ( 'NONE',  ( 0.4278561937608114096, 0.000000000000000000, 5.436428395565744864 ) ) ;
#37471 = ORIENTED_EDGE ( 'NONE', *, *, #77348, .F. ) ;
#37470 = CARTESIAN_POINT ( 'NONE',  ( 17.20831665107776587, 32.88393115100078745, 7.208316651077764980 ) ) ;
#37472 = CARTESIAN_POINT ( 'NONE',  ( 19.38216949554541202, 50.99863466993042493, 9.382169495545424454 ) ) ;
#37473 = LINE ( 'NONE', #67962, #72529 ) ;
#37474 = CARTESIAN_POINT ( 'NONE',  ( -2.816281873526471635, 8.915301336597083903, -3.434112377981056508 ) ) ;
#37475 = CARTESIAN_POINT ( 'NONE',  ( 0.5774900079438590739, 52.64701867748817676, -5.440088680355550821 ) ) ;
#37476 = CARTESIAN_POINT ( 'NONE',  ( -0.3689425029237898834, 36.17874883491396787, -10.36894250292378850 ) ) ;
#37477 = PRODUCT_DEFINITION_CONTEXT ( 'detailed design', #25126, 'design' ) ;
#37478 = CARTESIAN_POINT ( 'NONE',  ( -8.665245649996185406, 87.00799529562631562, 4.320095926137915932 ) ) ;
#37479 = CARTESIAN_POINT ( 'NONE',  ( 10.00000000000000000, 25.55374883491396787, -14.16423886937410082 ) ) ;
#37480 = CARTESIAN_POINT ( 'NONE',  ( -4.164238869374098151, 51.59541550158063217, -3.795296366450310543 ) ) ;
#37481 = CARTESIAN_POINT ( 'NONE',  ( 24.16423886937410614, 4.303748834913967869, 8.672049930838204340E-16 ) ) ;
#37483 = CARTESIAN_POINT ( 'NONE',  ( 8.879999999999991900, 21.00000000000000000, -2.900000000000000799 ) ) ;
#37482 = CARTESIAN_POINT ( 'NONE',  ( 20.36894250292379738, 9.928748834913966093, -10.36894250292379027 ) ) ;
#37484 = CARTESIAN_POINT ( 'NONE',  ( -0.8801773607111009756, 43.06368534415484106, 1.068504757029289695E-15 ) ) ;
#37485 = CARTESIAN_POINT ( 'NONE',  ( 6.533420211785746723, -50.31490269211863620, -3.750000000000000888 ) ) ;
#37486 = CARTESIAN_POINT ( 'NONE',  ( 18.52753015748618282, 33.92559781766745886, -4.923371831947291888 ) ) ;
#37488 = CARTESIAN_POINT ( 'NONE',  ( 10.00000000000000000, 44.75893115100078745, -9.846743663894594434 ) ) ;
#37487 = CARTESIAN_POINT ( 'NONE',  ( 2.035157376598824452, 63.68868534415484106, 7.964842623401179544 ) ) ;
#37489 = CARTESIAN_POINT ( 'NONE',  ( 7.084665262690076126, 29.10535201082150181, 10.88017736071109987 ) ) ;
#37490 = CARTESIAN_POINT ( 'NONE',  ( 13.43411237798105340, 55.58196800326374643, 12.81628187352647963 ) ) ;
#37491 = CARTESIAN_POINT ( 'NONE',  ( 17.20831665107776587, 59.13393115100078745, -7.208316651077762316 ) ) ;
#37492 = CARTESIAN_POINT ( 'NONE',  ( -9.520529577030321988, 15.00000000000000888, -11.10395710204432973 ) ) ;
#37493 = EDGE_CURVE ( 'NONE', #48192, #3803, #93624, .T. ) ;
#37494 = CARTESIAN_POINT ( 'NONE',  ( -2.816281873526473856, 39.12363466993041783, 9.499525473075851096E-16 ) ) ;
#37495 = CARTESIAN_POINT ( 'NONE',  ( 14.16423886937410437, -20.90458449841936428, 3.795296366450304770 ) ) ;
#37496 = CARTESIAN_POINT ( 'NONE',  ( 7.084665262690076126, 44.10535201082151247, 10.88017736071109987 ) ) ;
#37497 = CARTESIAN_POINT ( 'NONE',  ( 0.1532563361054082862, 46.21726448433411605, 2.638427012816831674 ) ) ;
#37498 = CARTESIAN_POINT ( 'NONE',  ( 22.26659068614895176, 24.72041550158063572, -7.082119434687042414 ) ) ;
#37499 = ORIENTED_EDGE ( 'NONE', *, *, #85946, .T. ) ;
#37500 =( NAMED_UNIT ( * ) PLANE_ANGLE_UNIT ( ) SI_UNIT ( $, .RADIAN. ) );
#37501 = CARTESIAN_POINT ( 'NONE',  ( 7.084665262690076126, 62.02201867748816966, -10.88017736071110164 ) ) ;
#37502 = CARTESIAN_POINT ( 'NONE',  ( 0.5774900079438590739, 67.64701867748817676, -5.440088680355550821 ) ) ;
#37503 = CARTESIAN_POINT ( 'NONE',  ( 20.36894250292379382, 53.67874883491397497, 10.36894250292379205 ) ) ;
#37504 = CARTESIAN_POINT ( 'NONE',  ( 6.565887622018943937, 0.1653013365970866511, 12.81628187352647430 ) ) ;
#37505 = CARTESIAN_POINT ( 'NONE',  ( -6.430724159521292727, -88.51069574204372259, 4.000000000000000000 ) ) ;
#37506 = CARTESIAN_POINT ( 'NONE',  ( 7.084665262690076126, 49.10535201082149825, 10.88017736071109987 ) ) ;
#37507 = CARTESIAN_POINT ( 'NONE',  ( 2.148416515056622789, 57.23726573380439930, 6.499999999999959144 ) ) ;
#37508 = CARTESIAN_POINT ( 'NONE',  ( -4.164238869374099927, 47.01208216824729647, 3.795296366450308767 ) ) ;
#37509 = CARTESIAN_POINT ( 'NONE',  ( -7.964842623401172439, 23.68868534415484106, 7.964842623401183097 ) ) ;
#37510 = CARTESIAN_POINT ( 'NONE',  ( 19.42250999205614548, 10.98035201082150358, -5.440088680355545492 ) ) ;
#37511 = CARTESIAN_POINT ( 'NONE',  ( 12.91533473730992121, 19.52201867748816611, 10.88017736071110164 ) ) ;
#37512 = PRESENTATION_LAYER_ASSIGNMENT (  '', '', ( #7171 ) ) ;
#37513 = CARTESIAN_POINT ( 'NONE',  ( 14.92337183194729633, 52.67559781766745175, 8.527530157486181039 ) ) ;
#37514 = CARTESIAN_POINT ( 'NONE',  ( 16.40814093676324603, 47.45696800326375353, -11.09922568453594671 ) ) ;
#37515 = CARTESIAN_POINT ( 'NONE',  ( -35.44000000000001194, 93.50000000000000000, -9.500000000000000000 ) ) ;
#37516 = VERTEX_POINT ( 'NONE', #4646 ) ;
#37517 = CARTESIAN_POINT ( 'NONE',  ( 2.035157376598824452, 18.68868534415484106, 7.964842623401179544 ) ) ;
#37518 = CARTESIAN_POINT ( 'NONE',  ( 16.40814093676323893, 20.79030133659708923, 11.09922568453595026 ) ) ;
#37519 = CARTESIAN_POINT ( 'NONE',  ( 0.000000000000000000, 12.49999999999999112, 0.000000000000000000 ) ) ;
#37520 = EDGE_CURVE ( 'NONE', #20819, #67069, #4150, .T. ) ;
#37521 = MECHANICAL_DESIGN_GEOMETRIC_PRESENTATION_REPRESENTATION (  '', ( #59829 ), #56627 ) ;
#37522 = CARTESIAN_POINT ( 'NONE',  ( 10.00000000000000000, 49.75893115100078745, -9.846743663894594434 ) ) ;
#37523 = CARTESIAN_POINT ( 'NONE',  ( 7.084665262690076126, 34.10535201082151247, 10.88017736071109987 ) ) ;
#37524 = PRESENTATION_LAYER_ASSIGNMENT (  '', '', ( #80616 ) ) ;
#37525 = CARTESIAN_POINT ( 'NONE',  ( 22.81628187352648496, 16.83196800326374998, -3.434112377981050290 ) ) ;
#37527 = CARTESIAN_POINT ( 'NONE',  ( -5.093587308868599450, -0.03417435944610275333, 15.16353404595993837 ) ) ;
#37526 = CARTESIAN_POINT ( 'NONE',  ( -0.8801773607111009756, 48.06368534415484817, 1.068504757029289695E-15 ) ) ;
#37528 =( NAMED_UNIT ( * ) SI_UNIT ( $, .STERADIAN. ) SOLID_ANGLE_UNIT ( ) );
#37529 = CARTESIAN_POINT ( 'NONE',  ( -2.816281873526471635, 53.91530133659709634, -3.434112377981056508 ) ) ;
#37530 = EDGE_LOOP ( 'NONE', ( #57993, #1662, #71146, #32987, #95393, #97834 ) ) ;
#37531 = ADVANCED_FACE ( 'NONE', ( #39322 ), #71170, .T. ) ;
#37532 = CARTESIAN_POINT ( 'NONE',  ( 7.084665262690076126, 54.10535201082151247, 10.88017736071109987 ) ) ;
#37533 = CARTESIAN_POINT ( 'NONE',  ( 10.00000000000000178, 40.37363466993042493, 12.81628187352647608 ) ) ;
#37534 = CARTESIAN_POINT ( 'NONE',  ( 2.791683348922240793, 6.633931151000785675, 7.208316651077764092 ) ) ;
#37535 = CARTESIAN_POINT ( 'NONE',  ( 17.96484262340118221, 46.18868534415484106, -7.964842623401177768 ) ) ;
#37536 = CARTESIAN_POINT ( 'NONE',  ( 2.791683348922237240, 65.38393115100078035, -7.208316651077763204 ) ) ;
#37537 = CARTESIAN_POINT ( 'NONE',  ( 7.361572987183170547, 62.05059781766745886, 9.846743663894590881 ) ) ;
#37538 = CARTESIAN_POINT ( 'NONE',  ( 0.1532563361054100626, 20.80059781766744464, -2.638427012816831230 ) ) ;
#37539 = CARTESIAN_POINT ( 'NONE',  ( 0.1532563361054082862, 1.217264484334117824, 2.638427012816831674 ) ) ;
#37540 = PLANE ( 'NONE',  #34717 ) ;
#37541 = CARTESIAN_POINT ( 'NONE',  ( 2.917880565312950480, 40.97041550158063217, -12.26659068614894821 ) ) ;
#37542 = CARTESIAN_POINT ( 'NONE',  ( -8.000000000000000000, 1.019547802438458550, 4.000000000000000000 ) ) ;
#37543 = CARTESIAN_POINT ( 'NONE',  ( -0.8801773607110991993, 12.85535201082150358, -2.915334737309923874 ) ) ;
#37544 = CARTESIAN_POINT ( 'NONE',  ( -6.982525766850296023, -88.11956318484570261, -4.000000000000000000 ) ) ;
#37545 = ORIENTED_EDGE ( 'NONE', *, *, #91912, .F. ) ;
#37546 = CARTESIAN_POINT ( 'NONE',  ( -2.266590686148945544, 67.22041550158063217, 7.082119434687048631 ) ) ;
#37547 = CARTESIAN_POINT ( 'NONE',  ( 13.79529636645030344, 58.26208216824728936, 14.16423886937410614 ) ) ;
#37548 = CARTESIAN_POINT ( 'NONE',  ( 10.00000000000000178, 47.25893115100078745, 9.846743663894594434 ) ) ;
#37549 =( GEOMETRIC_REPRESENTATION_CONTEXT ( 3 ) GLOBAL_UNCERTAINTY_ASSIGNED_CONTEXT ( ( #36140 ) ) GLOBAL_UNIT_ASSIGNED_CONTEXT ( ( #35388, #81381, #28386 ) ) REPRESENTATION_CONTEXT ( 'NONE', 'WORKASPACE' ) );
#37550 = CARTESIAN_POINT ( 'NONE',  ( 3.591859063236763294, 33.29030133659708213, -11.09922568453595026 ) ) ;
#37551 = CARTESIAN_POINT ( 'NONE',  ( -4.265659168453120209, 14.95077488074853456, -14.12268572233456787 ) ) ;
#37553 = CARTESIAN_POINT ( 'NONE',  ( -2.266590686148945544, 1.387082168247301128, -7.082119434687050408 ) ) ;
#37552 = CARTESIAN_POINT ( 'NONE',  ( -10.03950393934837670, 88.95408272063291122, -5.473102654076496876 ) ) ;
#37554 = CARTESIAN_POINT ( 'NONE',  ( 12.91533473730993009, 6.605352010821504471, -10.88017736071109987 ) ) ;
#37555 = CARTESIAN_POINT ( 'NONE',  ( 6.204703633549690345, 50.76208216824730357, -14.16423886937410259 ) ) ;
#37556 = CARTESIAN_POINT ( 'NONE',  ( 12.63842701281683034, 47.46726448433412315, 9.846743663894596210 ) ) ;
#37557 = CARTESIAN_POINT ( 'NONE',  ( -12.34086200392816757, 0.000000000000000000, -7.125000000000143885 ) ) ;
#37558 = CARTESIAN_POINT ( 'NONE',  ( 12.63842701281683922, 24.55059781766745175, -9.846743663894590881 ) ) ;
#37559 = CARTESIAN_POINT ( 'NONE',  ( -0.8801773607111009756, 33.27201867748817676, 2.915334737309923874 ) ) ;
#37560 = CARTESIAN_POINT ( 'NONE',  ( -9.846743663894594434, 21.00893115100079100, 3.469446951953614189E-15 ) ) ;
#37561 = VERTEX_POINT ( 'NONE', #94148 ) ;
#37562 = ORIENTED_EDGE ( 'NONE', *, *, #71865, .F. ) ;
#37563 =( NAMED_UNIT ( * ) SI_UNIT ( $, .STERADIAN. ) SOLID_ANGLE_UNIT ( ) );
#37564 = ORIENTED_EDGE ( 'NONE', *, *, #3122, .T. ) ;
#37566 = CARTESIAN_POINT ( 'NONE',  ( 10.00000000000000000, 41.81368534415484106, -10.88017736071110342 ) ) ;
#37565 = CARTESIAN_POINT ( 'NONE',  ( 7.084665262690076126, 34.10535201082151247, 10.88017736071109987 ) ) ;
#37568 = CARTESIAN_POINT ( 'NONE',  ( 22.81628187352647785, 36.41530133659707502, 3.434112377981063169 ) ) ;
#37567 = CARTESIAN_POINT ( 'NONE',  ( 12.63842701281683034, 57.46726448433411605, 9.846743663894596210 ) ) ;
#37569 = CARTESIAN_POINT ( 'NONE',  ( 6.204703633549690345, 7.845415501580634832, 14.16423886937410082 ) ) ;
#37570 = VECTOR ( 'NONE', #42592, 1000.000000000000000 ) ;
#37571 = EDGE_CURVE ( 'NONE', #57022, #96588, #47366, .T. ) ;
#37572 = CARTESIAN_POINT ( 'NONE',  ( 10.00000000000000178, 69.31368534415484817, 10.88017736071110342 ) ) ;
#37573 = CARTESIAN_POINT ( 'NONE',  ( 19.38216949554541557, 27.24863466993041783, -9.382169495545420901 ) ) ;
#37574 = ORIENTED_EDGE ( 'NONE', *, *, #54836, .T. ) ;
#37575 = CARTESIAN_POINT ( 'NONE',  ( 18.52753015748618282, 38.92559781766745175, -4.923371831947291888 ) ) ;
#37576 = CARTESIAN_POINT ( 'NONE',  ( 2.035157376598824452, 3.688685344154837953, 7.964842623401179544 ) ) ;
#37577 = VERTEX_POINT ( 'NONE', #13111 ) ;
#37578 = CARTESIAN_POINT ( 'NONE',  ( 10.00000000000000000, 11.81368534415483751, -10.88017736071110342 ) ) ;
#37579 = VERTEX_POINT ( 'NONE', #67105 ) ;
#37580 = CARTESIAN_POINT ( 'NONE',  ( 15.44008868035555793, 66.39701867748817676, -9.422509992056140149 ) ) ;
#37581 = CARTESIAN_POINT ( 'NONE',  ( -0.8801773607111009756, 53.06368534415484106, 1.068504757029289695E-15 ) ) ;
#37582 = CARTESIAN_POINT ( 'NONE',  ( 20.88017736071110164, 65.35535201082150536, 2.915334737309930979 ) ) ;
#37583 = CARTESIAN_POINT ( 'NONE',  ( 20.88017736071110164, 50.35535201082151247, 2.915334737309930979 ) ) ;
#37584 = CARTESIAN_POINT ( 'NONE',  ( -1.926860441876564023, 52.87045670184114954, 3.195792623639529761 ) ) ;
#37586 = ORIENTED_EDGE ( 'NONE', *, *, #86646, .F. ) ;
#37585 = CARTESIAN_POINT ( 'NONE',  ( 10.69983265767916514, -97.11219342806609234, 3.999999999999999112 ) ) ;
#37587 = CARTESIAN_POINT ( 'NONE',  ( 1.472469842513823179, 36.42559781766745175, 4.923371831947296329 ) ) ;
#37588 = ORIENTED_EDGE ( 'NONE', *, *, #44271, .F. ) ;
#37589 = LINE ( 'NONE', #61548, #39460 ) ;
#37590 = AXIS2_PLACEMENT_3D ( 'NONE', #20856, #88853, #51346 ) ;
#37591 = DIRECTION ( 'NONE',  ( -0.000000000000000000, 0.000000000000000000, 1.000000000000000000 ) ) ;
#37592 = CARTESIAN_POINT ( 'NONE',  ( 22.26659068614894466, 8.887082168247300018, 7.082119434687054849 ) ) ;
#37593 = CARTESIAN_POINT ( 'NONE',  ( -0.2418659066527775181, 8.090145880403570189, 6.114288769123032985 ) ) ;
#37595 = CARTESIAN_POINT ( 'NONE',  ( 7.361572987183170547, 37.05059781766744464, 9.846743663894590881 ) ) ;
#37594 = CARTESIAN_POINT ( 'NONE',  ( 2.603489959281060973, 26.58210964143323096, 6.499999999999401368 ) ) ;
#37596 = CARTESIAN_POINT ( 'NONE',  ( 7.084665262690076126, 7.022018677488170546, -10.88017736071110164 ) ) ;
#37597 = FACE_OUTER_BOUND ( 'NONE', #65605, .T. ) ;
#37599 = ORIENTED_EDGE ( 'NONE', *, *, #7727, .T. ) ;
#37598 = CARTESIAN_POINT ( 'NONE',  ( 22.81628187352647785, 46.62363466993041783, 6.195893100308588602E-16 ) ) ;
#37600 = CARTESIAN_POINT ( 'NONE',  ( -5.963430220938290560, 3.854976035794183353, -10.32896413005679648 ) ) ;
#37601 = CARTESIAN_POINT ( 'NONE',  ( 2.791683348922237240, 45.38393115100079456, -7.208316651077763204 ) ) ;
#37602 = DIRECTION ( 'NONE',  ( 0.000000000000000000, 0.000000000000000000, 1.000000000000000000 ) ) ;
#37603 = CARTESIAN_POINT ( 'NONE',  ( 19.38216949554541557, 17.24863466993041783, -9.382169495545420901 ) ) ;
#37604 = CARTESIAN_POINT ( 'NONE',  ( 12.63842701281683922, 29.55059781766745175, -9.846743663894590881 ) ) ;
#37605 = CARTESIAN_POINT ( 'NONE',  ( 12.24319267753454099, 54.01141590572476048, 2.899999999999999467 ) ) ;
#37606 = ADVANCED_FACE ( 'NONE', ( #44090 ), #82098, .F. ) ;
#37607 = CARTESIAN_POINT ( 'NONE',  ( 13.43411237798105340, 5.581968003263753531, 12.81628187352647963 ) ) ;
#37608 =( GEOMETRIC_REPRESENTATION_CONTEXT ( 3 ) GLOBAL_UNCERTAINTY_ASSIGNED_CONTEXT ( ( #50154 ) ) GLOBAL_UNIT_ASSIGNED_CONTEXT ( ( #94015, #64481, #55020 ) ) REPRESENTATION_CONTEXT ( 'NONE', 'WORKASPACE' ) );
#37609 = ORIENTED_EDGE ( 'NONE', *, *, #44829, .F. ) ;
#37610 = ADVANCED_FACE ( 'NONE', ( #43607 ), #40968, .T. ) ;
#37611 = EDGE_CURVE ( 'NONE', #81206, #88856, #13610, .T. ) ;
#37612 = VERTEX_POINT ( 'NONE', #60585 ) ;
#37613 = CARTESIAN_POINT ( 'NONE',  ( 20.88017736071110519, 20.56368534415484106, 2.639326808657452039E-16 ) ) ;
#37614 = CARTESIAN_POINT ( 'NONE',  ( 6.204703633549690345, 15.76208216824730179, -14.16423886937410259 ) ) ;
#37615 = CARTESIAN_POINT ( 'NONE',  ( 17.20831665107776587, 34.13393115100078745, -7.208316651077762316 ) ) ;
#37616 = CARTESIAN_POINT ( 'NONE',  ( -0.8801773607111009756, 68.06368534415484817, 1.068504757029289695E-15 ) ) ;
#37618 = LINE ( 'NONE', #13619, #11278 ) ;
#37617 = CARTESIAN_POINT ( 'NONE',  ( 19.38216949554541202, 35.99863466993041072, 9.382169495545424454 ) ) ;
#37619 = CARTESIAN_POINT ( 'NONE',  ( 20.88017736071110875, 15.77201867748817143, -2.915334737309920765 ) ) ;
#37620 = CARTESIAN_POINT ( 'NONE',  ( 5.419894505350582925, 15.00000000000000000, -13.98659156302458761 ) ) ;
#37621 = CARTESIAN_POINT ( 'NONE',  ( 22.81628187352648496, 1.831968003263753753, -3.434112377981050290 ) ) ;
#37622 = CARTESIAN_POINT ( 'NONE',  ( 14.92337183194729988, 24.34226448433411960, -8.527530157486177487 ) ) ;
#37623 = CARTESIAN_POINT ( 'NONE',  ( 5.440088680355556150, -15.26964798917848931, 9.422509992056138373 ) ) ;
#37624 = CARTESIAN_POINT ( 'NONE',  ( 6.565887622018943937, 30.16530133659708568, 12.81628187352647430 ) ) ;
#37625 = LINE ( 'NONE', #90602, #33994 ) ;
#37627 = DIRECTION ( 'NONE',  ( -0.7716245833877234395, 0.000000000000000000, 0.6360782202777597316 ) ) ;
#37626 = CARTESIAN_POINT ( 'NONE',  ( 12.91533473730993009, 41.60535201082149825, -10.88017736071109987 ) ) ;
#37628 = AXIS2_PLACEMENT_3D ( 'NONE', #81125, #88130, #3670 ) ;
#37629 = PLANE ( 'NONE',  #94318 ) ;
#37630 = CARTESIAN_POINT ( 'NONE',  ( 12.91533473730993009, 41.60535201082149825, -10.88017736071109987 ) ) ;
#37631 = CARTESIAN_POINT ( 'NONE',  ( 12.91533473730993009, 41.60535201082149825, -10.88017736071109987 ) ) ;
#37632 = CARTESIAN_POINT ( 'NONE',  ( 19.84674366389459266, 58.30059781766745886, 2.638427012816836559 ) ) ;
#37633 = CARTESIAN_POINT ( 'NONE',  ( 4.559911319644449179, 68.89701867748817676, 9.422509992056141925 ) ) ;
#37634 = PRESENTATION_LAYER_ASSIGNMENT (  '', '', ( #64713 ) ) ;
#37635 = CARTESIAN_POINT ( 'NONE',  ( 5.076628168052703671, 51.84226448433412315, 8.527530157486179263 ) ) ;
#37637 = CARTESIAN_POINT ( 'NONE',  ( -13.34989199100162871, 14.95037102702517906, 6.279943681065644157 ) ) ;
#37636 = CARTESIAN_POINT ( 'NONE',  ( 10.00000000000000178, 14.31368534415483751, 10.88017736071110342 ) ) ;
#37638 = CARTESIAN_POINT ( 'NONE',  ( 19.38216949554541557, 7.248634669930421381, -9.382169495545420901 ) ) ;
#37639 = ORIENTED_EDGE ( 'NONE', *, *, #55130, .T. ) ;
#37640 = CARTESIAN_POINT ( 'NONE',  ( 12.91533473730992121, 39.52201867748817676, 10.88017736071110164 ) ) ;
#37641 = EDGE_CURVE ( 'NONE', #63345, #31263, #6439, .T. ) ;
#37642 = CARTESIAN_POINT ( 'NONE',  ( 19.05866839779138999, 15.95508385108959004, -6.499999999999970690 ) ) ;
#37643 = CARTESIAN_POINT ( 'NONE',  ( 15.44008868035555260, 4.730352010821504471, 9.422509992056143702 ) ) ;
#37644 = CARTESIAN_POINT ( 'NONE',  ( 12.91533473730993009, 21.60535201082150536, -10.88017736071109987 ) ) ;
#37645 = CARTESIAN_POINT ( 'NONE',  ( 0.5774900079438607392, 68.48035201082150536, 5.440088680355550821 ) ) ;
#37646 = CARTESIAN_POINT ( 'NONE',  ( 10.00000000000000178, 38.05374883491396787, 14.16423886937410082 ) ) ;
#37647 = CARTESIAN_POINT ( 'NONE',  ( 2.791683348922240793, 31.63393115100078745, 7.208316651077764092 ) ) ;
#37648 = CARTESIAN_POINT ( 'NONE',  ( 10.00000000000000178, 49.31368534415484106, 10.88017736071110342 ) ) ;
#37649 = CARTESIAN_POINT ( 'NONE',  ( 18.95386800104995118, 38.23810908735726599, -6.499999999999988454 ) ) ;
#37650 = CARTESIAN_POINT ( 'NONE',  ( -4.164238869374098151, 6.595415501580634832, -3.795296366450310543 ) ) ;
#37651 = VECTOR ( 'NONE', #61496, 1000.000000000000000 ) ;
#37652 = LINE ( 'NONE', #74648, #40171 ) ;
#37653 = CARTESIAN_POINT ( 'NONE',  ( 18.52753015748618282, 58.92559781766745886, -4.923371831947291888 ) ) ;
#37654 = ORIENTED_EDGE ( 'NONE', *, *, #29887, .F. ) ;
#37655 = EDGE_LOOP ( 'NONE', ( #91707, #90234, #75141, #74216 ) ) ;
#37656 = CIRCLE ( 'NONE', #50411, 0.2500000000000002220 ) ;
#37657 = CARTESIAN_POINT ( 'NONE',  ( -4.164238869374099039, 21.80374883491396787, 8.674139862899312516E-16 ) ) ;
#37658 = CARTESIAN_POINT ( 'NONE',  ( 24.16423886937410614, 19.30374883491397142, 8.672049930838204340E-16 ) ) ;
#37659 = CARTESIAN_POINT ( 'NONE',  ( 12.91533473730993009, 66.60535201082150536, -10.88017736071109987 ) ) ;
#37660 = CARTESIAN_POINT ( 'NONE',  ( 22.26659068614895176, 64.72041550158064638, -7.082119434687042414 ) ) ;
#37661 = CARTESIAN_POINT ( 'NONE',  ( 19.84674366389459266, 48.30059781766745175, 2.638427012816836559 ) ) ;
#37662 = CARTESIAN_POINT ( 'NONE',  ( -8.159331231749115787, -4.163042900881196218, 3.750000000000000000 ) ) ;
#37664 = CARTESIAN_POINT ( 'NONE',  ( -1.099225684535947600, 19.54030133659708568, 6.408140936763237150 ) ) ;
#37663 = CARTESIAN_POINT ( 'NONE',  ( 12.91533473730993009, 46.60535201082150536, -10.88017736071109987 ) ) ;
#37665 = CARTESIAN_POINT ( 'NONE',  ( 22.26659068614894466, 13.88708216824730179, 7.082119434687054849 ) ) ;
#37666 = CARTESIAN_POINT ( 'NONE',  ( 15.44008868035555260, 9.730352010821505360, 9.422509992056143702 ) ) ;
#37667 = CARTESIAN_POINT ( 'NONE',  ( 10.00000000000000178, 19.31368534415484106, 10.88017736071110342 ) ) ;
#37668 = PRESENTATION_STYLE_ASSIGNMENT (( #29642 ) ) ;
#37669 = CARTESIAN_POINT ( 'NONE',  ( 20.88017736071110164, 55.35535201082149825, 2.915334737309930979 ) ) ;
#37670 = CARTESIAN_POINT ( 'NONE',  ( 3.591859063236761518, 44.95696800326376064, 11.09922568453594849 ) ) ;
#37671 = CARTESIAN_POINT ( 'NONE',  ( 8.527530157486179263, -21.90773551566587685, 4.923371831947292776 ) ) ;
#37672 = VERTEX_POINT ( 'NONE', #37605 ) ;
#37673 = DIRECTION ( 'NONE',  ( 1.000000000000000000, 0.000000000000000000, 0.000000000000000000 ) ) ;
#37674 = VERTEX_POINT ( 'NONE', #52105 ) ;
#37675 =( NAMED_UNIT ( * ) SI_UNIT ( $, .STERADIAN. ) SOLID_ANGLE_UNIT ( ) );
#37676 = CYLINDRICAL_SURFACE ( 'NONE', #71864, 0.5000000000000004441 ) ;
#37677 = ORIENTED_EDGE ( 'NONE', *, *, #54989, .F. ) ;
#37678 = LINE ( 'NONE', #30145, #90373 ) ;
#37680 = CARTESIAN_POINT ( 'NONE',  ( -2.266590686148945544, 67.22041550158063217, 7.082119434687048631 ) ) ;
#37679 = CARTESIAN_POINT ( 'NONE',  ( 6.204703633549690345, 65.76208216824731778, -14.16423886937410259 ) ) ;
#37682 = CARTESIAN_POINT ( 'NONE',  ( 19.84674366389459621, 58.50893115100078745, 7.409399052514197653E-17 ) ) ;
#37681 = CARTESIAN_POINT ( 'NONE',  ( 10.00000000000000000, 29.75893115100078745, -9.846743663894594434 ) ) ;
#37683 = CARTESIAN_POINT ( 'NONE',  ( 10.00000000000000178, 64.31368534415483396, 10.88017736071110342 ) ) ;
#37684 = CARTESIAN_POINT ( 'NONE',  ( 19.89220837332778657, 44.74062864464239908, 6.478736007405907493 ) ) ;
#37685 = EDGE_CURVE ( 'NONE', #31232, #90628, #45765, .T. ) ;
#37686 = CARTESIAN_POINT ( 'NONE',  ( 15.44008868035555793, 66.39701867748817676, -9.422509992056140149 ) ) ;
#37687 =( GEOMETRIC_REPRESENTATION_CONTEXT ( 3 ) GLOBAL_UNCERTAINTY_ASSIGNED_CONTEXT ( ( #27153 ) ) GLOBAL_UNIT_ASSIGNED_CONTEXT ( ( #5641, #42166, #4661 ) ) REPRESENTATION_CONTEXT ( 'NONE', 'WORKASPACE' ) );
#37688 = CARTESIAN_POINT ( 'NONE',  ( 6.408140936763236262, 17.45696800326376774, -11.09922568453595026 ) ) ;
#37689 = ORIENTED_EDGE ( 'NONE', *, *, #58130, .T. ) ;
#37690 = CARTESIAN_POINT ( 'NONE',  ( 17.08211943468705840, 40.13708216824731068, -12.26659068614894466 ) ) ;
#37691 = CARTESIAN_POINT ( 'NONE',  ( -2.266590686148945544, 46.38708216824730357, -7.082119434687050408 ) ) ;
#37692 = EDGE_LOOP ( 'NONE', ( #61279, #19593, #67056, #93166 ) ) ;
#37693 = CARTESIAN_POINT ( 'NONE',  ( 10.00000000000000178, 60.37363466993041783, 12.81628187352647608 ) ) ;
#37694 = CARTESIAN_POINT ( 'NONE',  ( 4.559911319644449179, 27.23035201082150536, -9.422509992056141925 ) ) ;
#37695 = CARTESIAN_POINT ( 'NONE',  ( 2.791683348922237240, 50.38393115100078035, -7.208316651077763204 ) ) ;
#37696 = CARTESIAN_POINT ( 'NONE',  ( -0.8801773607110991993, 22.85535201082150181, -2.915334737309923874 ) ) ;
#37697 = CARTESIAN_POINT ( 'NONE',  ( 22.81628187352647785, 61.62363466993041783, 6.195893100308588602E-16 ) ) ;
#37698 = DIRECTION ( 'NONE',  ( 0.000000000000000000, 1.000000000000000000, 0.000000000000000000 ) ) ;
#37699 = CARTESIAN_POINT ( 'NONE',  ( 5.076628168052703671, 51.84226448433412315, 8.527530157486179263 ) ) ;
#37700 = CARTESIAN_POINT ( 'NONE',  ( 5.076628168052703671, 51.84226448433412315, 8.527530157486179263 ) ) ;
#37701 = FACE_OUTER_BOUND ( 'NONE', #76276, .T. ) ;
#37702 = CARTESIAN_POINT ( 'NONE',  ( -0.1558782227856948255, 1.143494478793305150E-17, -14.62632331952783993 ) ) ;
#37703 = DIRECTION ( 'NONE',  ( 0.000000000000000000, 1.000000000000000000, 0.000000000000000000 ) ) ;
#37704 = ORIENTED_EDGE ( 'NONE', *, *, #1732, .T. ) ;
#37705 = CARTESIAN_POINT ( 'NONE',  ( 19.64275089555620113, 84.99790889484839340, 5.306638067702549755 ) ) ;
#37706 = CARTESIAN_POINT ( 'NONE',  ( 5.076628168052703671, 26.84226448433411960, 8.527530157486179263 ) ) ;
#37707 = CARTESIAN_POINT ( 'NONE',  ( 6.742022620658147503, 14.95037102811560281, 13.12259272460509862 ) ) ;
#37708 = CARTESIAN_POINT ( 'NONE',  ( -2.816281873526473856, 34.33196800326376064, 3.434112377981055619 ) ) ;
#37709 = CYLINDRICAL_SURFACE ( 'NONE', #75486, 15.00000000000000000 ) ;
#37710 = CARTESIAN_POINT ( 'NONE',  ( 0.1129803114748731130, 39.29427333184090543, -6.480634945678677816 ) ) ;
#37711 = VERTEX_POINT ( 'NONE', #58609 ) ;
#37712 = CARTESIAN_POINT ( 'NONE',  ( 7.850000000000003197, 98.49999999999998579, -8.525133428036873795 ) ) ;
#37713 = CARTESIAN_POINT ( 'NONE',  ( -6.581680125707233486, -88.31141629936868753, -2.750000000000000000 ) ) ;
#37714 = CARTESIAN_POINT ( 'NONE',  ( 0.1532563361054082862, 36.21726448433410894, 2.638427012816831674 ) ) ;
#37715 = CARTESIAN_POINT ( 'NONE',  ( 17.08211943468705130, 33.47041550158063927, 12.26659068614894998 ) ) ;
#37716 = CARTESIAN_POINT ( 'NONE',  ( 1.472469842513823179, 51.42559781766745886, 4.923371831947296329 ) ) ;
#37717 = LINE ( 'NONE', #67722, #22446 ) ;
#37718 = CARTESIAN_POINT ( 'NONE',  ( 19.84674366389459621, 3.508931151000785231, 7.409399052514197653E-17 ) ) ;
#37719 = EDGE_CURVE ( 'NONE', #54738, #32902, #48936, .T. ) ;
#37720 = CARTESIAN_POINT ( 'NONE',  ( -0.3689425029237898834, 6.178748834913968757, -10.36894250292378850 ) ) ;
#37721 = CARTESIAN_POINT ( 'NONE',  ( 12.63842701281683922, 44.55059781766745175, -9.846743663894590881 ) ) ;
#37722 = CARTESIAN_POINT ( 'NONE',  ( 2.035157376598824452, 48.68868534415483396, 7.964842623401179544 ) ) ;
#37723 = PRESENTATION_LAYER_ASSIGNMENT (  '', '', ( #85610 ) ) ;
#37724 = CARTESIAN_POINT ( 'NONE',  ( 14.92337183194729988, 44.34226448433412315, -8.527530157486177487 ) ) ;
#37726 = VECTOR ( 'NONE', #63280, 1000.000000000000227 ) ;
#37725 = DIRECTION ( 'NONE',  ( -0.06975647374412544122, -0.9975640502598241977, 0.000000000000000000 ) ) ;
#37727 = VECTOR ( 'NONE', #15181, 999.9999999999998863 ) ;
#37728 = ADVANCED_FACE ( 'NONE', ( #29093 ), #28608, .T. ) ;
#37729 = ORIENTED_EDGE ( 'NONE', *, *, #19659, .F. ) ;
#37730 = CARTESIAN_POINT ( 'NONE',  ( 15.44008868035555793, 41.39701867748817676, -9.422509992056140149 ) ) ;
#37731 = EDGE_CURVE ( 'NONE', #10095, #28167, #27665, .T. ) ;
#37732 = VECTOR ( 'NONE', #53181, 1000.000000000000000 ) ;
#37733 = ADVANCED_FACE ( 'NONE', ( #21618 ), #14113, .F. ) ;
#37734 = ORIENTED_EDGE ( 'NONE', *, *, #80127, .F. ) ;
#37735 = DIRECTION ( 'NONE',  ( -0.000000000000000000, -1.000000000000000000, -0.000000000000000000 ) ) ;
#37736 = CARTESIAN_POINT ( 'NONE',  ( 20.88017736071110519, 10.56368534415483751, 2.639326808657452039E-16 ) ) ;
#37738 = CARTESIAN_POINT ( 'NONE',  ( 19.42250999205614193, 50.14701867748817676, 5.440088680355555262 ) ) ;
#37737 = CARTESIAN_POINT ( 'NONE',  ( 19.84674366389459621, 63.50893115100078745, 7.409399052514197653E-17 ) ) ;
#37739 = CARTESIAN_POINT ( 'NONE',  ( -0.2418659066527643342, 47.23410085661203084, -6.114288769123057854 ) ) ;
#37740 = CARTESIAN_POINT ( 'NONE',  ( 19.89103541497709671, 10.66234555792571115, -6.479102184480792559 ) ) ;
#37741 = DIRECTION ( 'NONE',  ( 0.8070303256584298035, -0.5905099943842175847, 0.000000000000000000 ) ) ;
#37743 = LINE ( 'NONE', #14246, #13688 ) ;
#37742 = CARTESIAN_POINT ( 'NONE',  ( 15.44008868035555793, 46.39701867748817676, -9.422509992056140149 ) ) ;
#37744 = CARTESIAN_POINT ( 'NONE',  ( 0.1532563361054100626, 15.80059781766745353, -2.638427012816831230 ) ) ;
#37745 = CARTESIAN_POINT ( 'NONE',  ( 18.52753015748617571, 33.09226448433411605, 4.923371831947298993 ) ) ;
#37746 =( LENGTH_UNIT ( ) NAMED_UNIT ( * ) SI_UNIT ( .MILLI., .METRE. ) );
#37747 = CARTESIAN_POINT ( 'NONE',  ( 14.16423886937410082, 14.51208216824730179, -3.795296366450314096 ) ) ;
#37748 = CARTESIAN_POINT ( 'NONE',  ( 0.6178305044545818747, -1.501365330069579951, -9.382169495545419124 ) ) ;
#37749 = CARTESIAN_POINT ( 'NONE',  ( 20.88017736071110875, 5.772018677488170546, -2.915334737309920765 ) ) ;
#37750 = ADVANCED_FACE ( 'NONE', ( #75093 ), #17054, .T. ) ;
#37751 = CARTESIAN_POINT ( 'NONE',  ( 6.204703633549690345, 25.76208216824730712, -14.16423886937410259 ) ) ;
#37752 = CIRCLE ( 'NONE', #71290, 15.00000000000000000 ) ;
#37753 = CARTESIAN_POINT ( 'NONE',  ( 2.917880565312948704, 52.63708216824730357, 12.26659068614894643 ) ) ;
#37754 = CARTESIAN_POINT ( 'NONE',  ( 4.559911319644449179, 2.230352010821504471, -9.422509992056141925 ) ) ;
#37755 = ORIENTED_EDGE ( 'NONE', *, *, #78811, .T. ) ;
#37756 = CARTESIAN_POINT ( 'NONE',  ( 14.92337183194729988, 24.34226448433411960, -8.527530157486177487 ) ) ;
#37757 = TOROIDAL_SURFACE ( 'NONE', #23417, 0.5000000000000000000, 0.2500000000000000000 ) ;
#37758 = CARTESIAN_POINT ( 'NONE',  ( 4.559911319644449179, 27.23035201082150536, -9.422509992056141925 ) ) ;
#37759 = CARTESIAN_POINT ( 'NONE',  ( 12.63842701281683922, 54.55059781766745175, -9.846743663894590881 ) ) ;
#37761 = CARTESIAN_POINT ( 'NONE',  ( 18.17884179759846930, 48.66688879859523809, -6.500000000000002665 ) ) ;
#37760 = CARTESIAN_POINT ( 'NONE',  ( 10.00000000000000000, 5.553748834913967869, -14.16423886937410082 ) ) ;
#37762 = CARTESIAN_POINT ( 'NONE',  ( 0.000000000000000000, -97.00000000000000000, -3.750000000000000000 ) ) ;
#37763 = CARTESIAN_POINT ( 'NONE',  ( 16.40814093676324603, 42.45696800326375353, -11.09922568453594671 ) ) ;
#37764 = CARTESIAN_POINT ( 'NONE',  ( 12.63842701281683922, 39.55059781766744464, -9.846743663894590881 ) ) ;
#37765 = ORIENTED_EDGE ( 'NONE', *, *, #29323, .F. ) ;
#37766 = CARTESIAN_POINT ( 'NONE',  ( 19.84674366389459266, 8.717264484334116048, -2.638427012816827677 ) ) ;
#37767 = ADVANCED_FACE ( 'NONE', ( #21115 ), #83091, .T. ) ;
#37768 = CARTESIAN_POINT ( 'NONE',  ( 11.29392812321118100, -89.88967135473500036, -3.750000000000000000 ) ) ;
#37769 = DIRECTION ( 'NONE',  ( 0.6246950475544238435, 0.7808688094430307203, 0.000000000000000000 ) ) ;
#37770 = CARTESIAN_POINT ( 'NONE',  ( -0.8801773607111009756, 3.063685344154838397, 1.068504757029289695E-15 ) ) ;
#37771 = CARTESIAN_POINT ( 'NONE',  ( 22.26659068614895176, 54.72041550158063217, -7.082119434687042414 ) ) ;
#37772 = CARTESIAN_POINT ( 'NONE',  ( 17.96484262340118221, 39.93868534415484106, 7.964842623401181321 ) ) ;
#37773 = CARTESIAN_POINT ( 'NONE',  ( 21.92686044187656336, 51.97997603579418069, 3.195792623639536423 ) ) ;
#37774 = CARTESIAN_POINT ( 'NONE',  ( 19.84674366389459266, 33.30059781766744464, 2.638427012816836559 ) ) ;
#37775 = CARTESIAN_POINT ( 'NONE',  ( 0.5774900079438590739, 7.647018677488171434, -5.440088680355550821 ) ) ;
#37776 = CARTESIAN_POINT ( 'NONE',  ( 2.791683348922237240, 45.38393115100079456, -7.208316651077763204 ) ) ;
#37777 = CARTESIAN_POINT ( 'NONE',  ( 0.8438640652791046248, 1.024801820426205776E-17, -5.642539323548857233 ) ) ;
#37778 = CARTESIAN_POINT ( 'NONE',  ( 5.076628168052703671, 46.84226448433412315, 8.527530157486179263 ) ) ;
#37779 = CARTESIAN_POINT ( 'NONE',  ( -0.8801773607110991993, 37.85535201082151247, -2.915334737309923874 ) ) ;
#37780 = EDGE_LOOP ( 'NONE', ( #88439, #46502, #86736, #94231 ) ) ;
#37781 = ORIENTED_EDGE ( 'NONE', *, *, #19309, .F. ) ;
#37782 = CARTESIAN_POINT ( 'NONE',  ( -2.816281873526473856, 59.33196800326374643, 3.434112377981055619 ) ) ;
#37783 = CARTESIAN_POINT ( 'NONE',  ( 1.780824192092403058, 0.5000000000000004441, 14.89391369643514729 ) ) ;
#37784 = CARTESIAN_POINT ( 'NONE',  ( 5.076628168052704559, 10.17559781766745175, -8.527530157486179263 ) ) ;
#37785 = CARTESIAN_POINT ( 'NONE',  ( 22.81628187352647785, 61.62363466993041783, 6.195893100308588602E-16 ) ) ;
#37787 = CARTESIAN_POINT ( 'NONE',  ( 12.63842701281683034, 52.46726448433413026, 9.846743663894596210 ) ) ;
#37786 = CARTESIAN_POINT ( 'NONE',  ( -4.164238869374099039, 66.80374883491396076, 8.674139862899312516E-16 ) ) ;
#37788 = CARTESIAN_POINT ( 'NONE',  ( 20.00000000000000711, 93.00652443313859408, 4.825407044038334980 ) ) ;
#37789 = CARTESIAN_POINT ( 'NONE',  ( 24.16423886937410614, 24.51208216824730002, -3.795296366450302550 ) ) ;
#37790 = AXIS2_PLACEMENT_3D ( 'NONE', #65434, #12439, #56476 ) ;
#37791 = CARTESIAN_POINT ( 'NONE',  ( 20.36894250292379738, 44.92874883491396787, -10.36894250292379027 ) ) ;
#37792 = CARTESIAN_POINT ( 'NONE',  ( 18.52753015748618282, 53.92559781766745175, -4.923371831947291888 ) ) ;
#37793 = CARTESIAN_POINT ( 'NONE',  ( 0.5774900079438590739, 52.64701867748817676, -5.440088680355550821 ) ) ;
#37794 = CARTESIAN_POINT ( 'NONE',  ( 0.1532563361054083140, 6.008931151000784787, 1.131784320476157264E-15 ) ) ;
#37795 =( NAMED_UNIT ( * ) SI_UNIT ( $, .STERADIAN. ) SOLID_ANGLE_UNIT ( ) );
#37796 = ORIENTED_EDGE ( 'NONE', *, *, #79282, .T. ) ;
#37797 = B_SPLINE_CURVE_WITH_KNOTS ( 'NONE', 3,
 ( #87858, #78890, #63866, #2433 ),
 .UNSPECIFIED., .F., .F.,
 ( 4, 4 ),
 ( 0.000000000000000000, 0.002657014572711350643 ),
 .UNSPECIFIED. ) ;
#37798 = CARTESIAN_POINT ( 'NONE',  ( 6.565887622018943937, 58.08196800326376064, -12.81628187352647608 ) ) ;
#37799 = ORIENTED_EDGE ( 'NONE', *, *, #79922, .T. ) ;
#37800 = CARTESIAN_POINT ( 'NONE',  ( 2.791683348922240793, 16.63393115100078745, 7.208316651077764092 ) ) ;
#37801 = ORIENTED_EDGE ( 'NONE', *, *, #6118, .T. ) ;
#37802 = CARTESIAN_POINT ( 'NONE',  ( -4.164238869374099927, 22.01208216824730357, 3.795296366450308767 ) ) ;
#37803 = CARTESIAN_POINT ( 'NONE',  ( 0.1532563361054100626, 0.8005978176674514168, -2.638427012816831230 ) ) ;
#37804 = CARTESIAN_POINT ( 'NONE',  ( 15.44008868035555260, 24.73035201082150891, 9.422509992056143702 ) ) ;
#37805 = SURFACE_STYLE_USAGE ( .BOTH. , #60289 ) ;
#37806 = VECTOR ( 'NONE', #49768, 1000.000000000000000 ) ;
#37807 = ORIENTED_EDGE ( 'NONE', *, *, #5865, .T. ) ;
#37808 = STYLED_ITEM ( 'NONE', ( #85265 ), #17991 ) ;
#37809 = CARTESIAN_POINT ( 'NONE',  ( 0.5774900079438607392, 33.48035201082150536, 5.440088680355550821 ) ) ;
#37810 = VERTEX_POINT ( 'NONE', #73604 ) ;
#37811 = CARTESIAN_POINT ( 'NONE',  ( 0.5774900079438590739, 37.64701867748817676, -5.440088680355550821 ) ) ;
#37812 = CARTESIAN_POINT ( 'NONE',  ( 1.821158202401529369, 46.16688879859523098, 6.500000000000007105 ) ) ;
#37813 = ORIENTED_EDGE ( 'NONE', *, *, #50365, .F. ) ;
#37814 = CARTESIAN_POINT ( 'NONE',  ( -1.099225684535947600, 18.70696800326375353, -6.408140936763238038 ) ) ;
#37815 = EDGE_CURVE ( 'NONE', #70878, #83825, #5129, .T. ) ;
#37816 = DIRECTION ( 'NONE',  ( 0.000000000000000000, 1.000000000000000000, 0.000000000000000000 ) ) ;
#37817 = CARTESIAN_POINT ( 'NONE',  ( -0.8801773607111009756, 63.06368534415484106, 1.068504757029289695E-15 ) ) ;
#37818 = FACE_OUTER_BOUND ( 'NONE', #23151, .T. ) ;
#37819 = SURFACE_SIDE_STYLE ('',( #75798 ) ) ;
#37820 = CARTESIAN_POINT ( 'NONE',  ( 14.92337183194729633, 17.67559781766745175, 8.527530157486181039 ) ) ;
#37821 = CARTESIAN_POINT ( 'NONE',  ( 12.91533473730993009, 36.60535201082151247, -10.88017736071109987 ) ) ;
#37822 = EDGE_CURVE ( 'NONE', #9521, #98326, #96633, .T. ) ;
#37823 = MECHANICAL_DESIGN_GEOMETRIC_PRESENTATION_REPRESENTATION (  '', ( #5910 ), #50583 ) ;
#37824 = PRESENTATION_LAYER_ASSIGNMENT (  '', '', ( #9044 ) ) ;
#37825 = VERTEX_POINT ( 'NONE', #15108 ) ;
#37826 = COLOUR_RGB ( '', 0.09019608, 0.27058824, 0.51372549) ;
#37827 = DIRECTION ( 'NONE',  ( 0.000000000000000000, 0.000000000000000000, 1.000000000000000000 ) ) ;
#37828 = CARTESIAN_POINT ( 'NONE',  ( 4.559911319644449179, 37.23035201082150536, -9.422509992056141925 ) ) ;
#37829 = CARTESIAN_POINT ( 'NONE',  ( -46.43955761922751435, 103.5181700978648820, -6.245201398087227851 ) ) ;
#37830 = CARTESIAN_POINT ( 'NONE',  ( -2.816281873526473856, 49.33196800326374643, 3.434112377981055619 ) ) ;
#37831 = CARTESIAN_POINT ( 'NONE',  ( 15.44008868035555260, 59.73035201082151247, 9.422509992056143702 ) ) ;
#37832 = CARTESIAN_POINT ( 'NONE',  ( 19.38216949554541202, 0.9986346699304200492, 9.382169495545424454 ) ) ;
#37833 = CARTESIAN_POINT ( 'NONE',  ( -10.64017930668212664, 0.5000000000000004441, 10.57291749337208309 ) ) ;
#37834 = CARTESIAN_POINT ( 'NONE',  ( 7.361572987183170547, 22.05059781766745530, 9.846743663894590881 ) ) ;
#37835 = CARTESIAN_POINT ( 'NONE',  ( 13.43411237798106583, 57.66530133659708923, -12.81628187352647252 ) ) ;
#37836 = CARTESIAN_POINT ( 'NONE',  ( 2.377183314880002563, 35.78593319516821225, -6.500000000000057732 ) ) ;
#37837 = CARTESIAN_POINT ( 'NONE',  ( 0.1532563361054100626, 5.800597817667452638, -2.638427012816831230 ) ) ;
#37838 = CARTESIAN_POINT ( 'NONE',  ( 0.6178305044545818747, 8.498634669930421381, -9.382169495545419124 ) ) ;
#37840 = CARTESIAN_POINT ( 'NONE',  ( 18.52753015748617571, 63.09226448433412315, 4.923371831947298993 ) ) ;
#37839 = CARTESIAN_POINT ( 'NONE',  ( 14.88640444357867665, 0.2306972965111609708, -1.277895705730255571 ) ) ;
#37841 = CARTESIAN_POINT ( 'NONE',  ( 20.88017736071110875, 35.77201867748816966, -2.915334737309920765 ) ) ;
#37842 = CARTESIAN_POINT ( 'NONE',  ( 5.076628168052703671, 46.84226448433412315, 8.527530157486179263 ) ) ;
#37843 = FACE_OUTER_BOUND ( 'NONE', #27690, .T. ) ;
#37844 = CARTESIAN_POINT ( 'NONE',  ( 2.791683348922240793, 16.63393115100078745, 7.208316651077764092 ) ) ;
#37845 = CARTESIAN_POINT ( 'NONE',  ( 0.1532563361054100626, 10.80059781766745175, -2.638427012816831230 ) ) ;
#37847 = ORIENTED_EDGE ( 'NONE', *, *, #55919, .F. ) ;
#37846 = CARTESIAN_POINT ( 'NONE',  ( 6.565887622018943937, 3.081968003263753531, -12.81628187352647608 ) ) ;
#37849 = CARTESIAN_POINT ( 'NONE',  ( 17.96484262340118221, 6.188685344154836621, -7.964842623401177768 ) ) ;
#37848 = MECHANICAL_DESIGN_GEOMETRIC_PRESENTATION_REPRESENTATION (  '', ( #12265 ), #77722 ) ;
#37850 = DIRECTION ( 'NONE',  ( 0.000000000000000000, 0.000000000000000000, -1.000000000000000000 ) ) ;
#37851 = EDGE_CURVE ( 'NONE', #82904, #81875, #61154, .T. ) ;
#37852 = CARTESIAN_POINT ( 'NONE',  ( 6.574584770565365055, -50.88238473842167053, -2.749999999998390177 ) ) ;
#37853 = CARTESIAN_POINT ( 'NONE',  ( 20.88017736071110519, 5.563685344154838397, 2.639326808657452039E-16 ) ) ;
#37854 = CARTESIAN_POINT ( 'NONE',  ( 5.076628168052703671, 41.84226448433411605, 8.527530157486179263 ) ) ;
#37855 = EDGE_CURVE ( 'NONE', #28474, #44602, #52157, .T. ) ;
#37856 = CARTESIAN_POINT ( 'NONE',  ( 1.379999999999981908, 20.99999999999999645, 1.249999999999987121 ) ) ;
#37857 = CARTESIAN_POINT ( 'NONE',  ( 6.204703633549690345, 67.84541550158060375, 14.16423886937410082 ) ) ;
#37858 = DIRECTION ( 'NONE',  ( 0.000000000000000000, 0.000000000000000000, 1.000000000000000000 ) ) ;
#37859 = CARTESIAN_POINT ( 'NONE',  ( 12.91533473730992121, 39.52201867748817676, 10.88017736071110164 ) ) ;
#37860 = CARTESIAN_POINT ( 'NONE',  ( -0.3689425029237898834, 46.17874883491397497, -10.36894250292378850 ) ) ;
#37861 = CARTESIAN_POINT ( 'NONE',  ( 6.204703633549690345, 67.84541550158060375, 14.16423886937410082 ) ) ;
#37862 = CARTESIAN_POINT ( 'NONE',  ( 2.791683348922237240, 20.38393115100078745, -7.208316651077763204 ) ) ;
#37863 = CARTESIAN_POINT ( 'NONE',  ( 22.81628187352648496, 16.83196800326374998, -3.434112377981050290 ) ) ;
#37864 = DIRECTION ( 'NONE',  ( 0.000000000000000000, 1.000000000000000000, 0.000000000000000000 ) ) ;
#37865 = ORIENTED_EDGE ( 'NONE', *, *, #6805, .F. ) ;
#37866 = CARTESIAN_POINT ( 'NONE',  ( 6.715867195167449566, 4.285122813354096929E-16, -12.85095824508326956 ) ) ;
#37867 = CARTESIAN_POINT ( 'NONE',  ( 14.92337183194729988, 59.34226448433412315, -8.527530157486177487 ) ) ;
#37868 = DIRECTION ( 'NONE',  ( 0.000000000000000000, 0.000000000000000000, 1.000000000000000000 ) ) ;
#37869 = CARTESIAN_POINT ( 'NONE',  ( -8.081452932198143202, -7.288464344205941359, -4.000000000000000000 ) ) ;
#37870 = CARTESIAN_POINT ( 'NONE',  ( -2.266590686148945544, 7.220415501580634832, 7.082119434687048631 ) ) ;
#37871 = CARTESIAN_POINT ( 'NONE',  ( 0.1532563361054083140, 31.00893115100078390, 1.131784320476157264E-15 ) ) ;
#37872 = CARTESIAN_POINT ( 'NONE',  ( 6.579634127946654587, -87.99828267815715321, 3.750000000000000000 ) ) ;
#37873 = ORIENTED_EDGE ( 'NONE', *, *, #3396, .F. ) ;
#37874 = CARTESIAN_POINT ( 'NONE',  ( 10.00000000000000000, 55.55374883491396787, -14.16423886937410082 ) ) ;
#37875 = TOROIDAL_SURFACE ( 'NONE', #82544, 14.49999999999999822, 0.5000000000000000000 ) ;
#37876 = CARTESIAN_POINT ( 'NONE',  ( 14.92337183194729988, 4.342264484334117824, -8.527530157486177487 ) ) ;
#37878 = DIRECTION ( 'NONE',  ( 0.000000000000000000, 0.000000000000000000, 1.000000000000000000 ) ) ;
#37877 = DIRECTION ( 'NONE',  ( -0.8141155183563226760, 0.000000000000000000, 0.5807029557109348872 ) ) ;
#37879 = CARTESIAN_POINT ( 'NONE',  ( 12.91533473730993009, 26.60535201082150536, -10.88017736071109987 ) ) ;
#37880 = CARTESIAN_POINT ( 'NONE',  ( 16.40814093676323893, 45.79030133659708923, 11.09922568453595026 ) ) ;
#37881 = CARTESIAN_POINT ( 'NONE',  ( 13.43411237798105340, 35.58196800326375353, 12.81628187352647963 ) ) ;
#37882 = CARTESIAN_POINT ( 'NONE',  ( 10.00000000000000178, 2.258931151000784787, 9.846743663894594434 ) ) ;
#37883 = ORIENTED_EDGE ( 'NONE', *, *, #82737, .T. ) ;
#37884 = DIRECTION ( 'NONE',  ( -1.000000000000000000, 0.000000000000000000, 0.000000000000000000 ) ) ;
#37885 = EDGE_CURVE ( 'NONE', #47405, #46987, #69487, .T. ) ;
#37886 = CARTESIAN_POINT ( 'NONE',  ( -8.957305892841448625, -19.72688805321238448, -4.000000000000000000 ) ) ;
#37887 = CARTESIAN_POINT ( 'NONE',  ( 10.00000000000000178, 43.05374883491397497, 14.16423886937410082 ) ) ;
#37888 = CARTESIAN_POINT ( 'NONE',  ( 22.26659068614894466, 13.88708216824730179, 7.082119434687054849 ) ) ;
#37889 = CARTESIAN_POINT ( 'NONE',  ( 15.44008868035555793, 6.397018677488170546, -9.422509992056140149 ) ) ;
#37890 = AXIS2_PLACEMENT_3D ( 'NONE', #77250, #85257, #8758 ) ;
#37891 = CARTESIAN_POINT ( 'NONE',  ( 17.96484262340118221, 41.18868534415484106, -7.964842623401177768 ) ) ;
#37892 = CARTESIAN_POINT ( 'NONE',  ( -45.94000000000001194, 100.9999999999999858, -9.500000000000000000 ) ) ;
#37893 = CARTESIAN_POINT ( 'NONE',  ( 17.96484262340118221, 59.93868534415484106, 7.964842623401181321 ) ) ;
#37894 = CARTESIAN_POINT ( 'NONE',  ( -0.8801773607110991993, 67.85535201082151957, -2.915334737309923874 ) ) ;
#37895 = CARTESIAN_POINT ( 'NONE',  ( -2.816281873526473856, 29.12363466993041783, 9.499525473075851096E-16 ) ) ;
#37896 = CARTESIAN_POINT ( 'NONE',  ( 14.82679024690671099, 14.76930270348882068, -1.845086899513286527 ) ) ;
#37897 = FACE_OUTER_BOUND ( 'NONE', #33668, .T. ) ;
#37898 = CARTESIAN_POINT ( 'NONE',  ( 2.791683348922240793, 31.63393115100078745, 7.208316651077764092 ) ) ;
#37899 = AXIS2_PLACEMENT_3D ( 'NONE', #27928, #58422, #88936 ) ;
#37900 = AXIS2_PLACEMENT_3D ( 'NONE', #86402, #2432, #49859 ) ;
#37901 = CIRCLE ( 'NONE', #68228, 0.2500000000000002220 ) ;
#37902 = CARTESIAN_POINT ( 'NONE',  ( 10.00000000000000000, 22.87363466993042138, -12.81628187352647608 ) ) ;
#37903 = DIRECTION ( 'NONE',  ( 0.000000000000000000, 0.000000000000000000, 1.000000000000000000 ) ) ;
#37904 = CARTESIAN_POINT ( 'NONE',  ( 20.88017736071110519, 15.56368534415483751, 2.639326808657452039E-16 ) ) ;
#37905 = CARTESIAN_POINT ( 'NONE',  ( 10.00000000000000178, 42.25893115100078745, 9.846743663894594434 ) ) ;
#37906 = CARTESIAN_POINT ( 'NONE',  ( 19.38216949554541202, 55.99863466993041072, 9.382169495545424454 ) ) ;
#37908 = CARTESIAN_POINT ( 'NONE',  ( 13.79529636645030344, 3.262082168247301350, 14.16423886937410614 ) ) ;
#37907 = CARTESIAN_POINT ( 'NONE',  ( 19.84674366389459621, 18.50893115100078745, 7.409399052514197653E-17 ) ) ;
#37909 = CARTESIAN_POINT ( 'NONE',  ( 6.204703633549690345, 2.845415501580634388, 14.16423886937410082 ) ) ;
#37910 = CARTESIAN_POINT ( 'NONE',  ( 5.817157072110801685, 14.63595249122789177, -13.82608706751087979 ) ) ;
#37911 = CARTESIAN_POINT ( 'NONE',  ( 15.44008868035555260, 34.73035201082151247, 9.422509992056143702 ) ) ;
#37913 = CARTESIAN_POINT ( 'NONE',  ( -4.164238869374099927, 42.01208216824728936, 3.795296366450308767 ) ) ;
#37912 = CARTESIAN_POINT ( 'NONE',  ( 7.084665262690076126, 17.02201867748817676, -10.88017736071110164 ) ) ;
#37914 = B_SPLINE_CURVE_WITH_KNOTS ( 'NONE', 3,
 ( #35374, #20382, #65369, #12379, #89852, #27378 ),
 .UNSPECIFIED., .F., .F.,
 ( 4, 2, 4 ),
 ( 0.0002800032591535108481, 0.0006862085204461408280, 0.001092413781738770916 ),
 .UNSPECIFIED. ) ;
#37915 = CARTESIAN_POINT ( 'NONE',  ( -0.8801773607111009756, 28.06368534415484106, 1.068504757029289695E-15 ) ) ;
#37916 = CARTESIAN_POINT ( 'NONE',  ( 7.084665262690076126, 14.10535201082150358, 10.88017736071109987 ) ) ;
#37917 = VERTEX_POINT ( 'NONE', #24081 ) ;
#37918 = CARTESIAN_POINT ( 'NONE',  ( 15.44008868035555260, 24.73035201082150891, 9.422509992056143702 ) ) ;
#37919 = CARTESIAN_POINT ( 'NONE',  ( 16.40814093676323893, 45.79030133659708923, 11.09922568453595026 ) ) ;
#37920 = CARTESIAN_POINT ( 'NONE',  ( 7.084665262690076126, 47.02201867748818387, -10.88017736071110164 ) ) ;
#37922 = CARTESIAN_POINT ( 'NONE',  ( -0.8801773607111009756, 48.06368534415484817, 1.068504757029289695E-15 ) ) ;
#37921 = FILL_AREA_STYLE_COLOUR ( '', #95148 ) ;
#37923 = ORIENTED_EDGE ( 'NONE', *, *, #20324, .T. ) ;
#37924 = CARTESIAN_POINT ( 'NONE',  ( 7.084665262690076126, 39.10535201082150536, 10.88017736071109987 ) ) ;
#37925 = CARTESIAN_POINT ( 'NONE',  ( 5.115475850225431387, -17.53855045868316154, 4.000000000004829914 ) ) ;
#37926 = CARTESIAN_POINT ( 'NONE',  ( -5.817157072110893168, 0.5000000000000004441, 13.82608706751082828 ) ) ;
#37927 = CARTESIAN_POINT ( 'NONE',  ( 6.204703633549690345, 40.76208216824731778, -14.16423886937410259 ) ) ;
#37928 = CARTESIAN_POINT ( 'NONE',  ( 20.88017736071110519, 60.56368534415484106, 2.639326808657452039E-16 ) ) ;
#37929 = CARTESIAN_POINT ( 'NONE',  ( 0.000000000000000000, 0.5000000000000004441, 0.000000000000000000 ) ) ;
#37930 = CARTESIAN_POINT ( 'NONE',  ( 5.076628168052704559, 0.1755978176674514724, -8.527530157486179263 ) ) ;
#37931 = CARTESIAN_POINT ( 'NONE',  ( 0.1532563361054082862, 61.21726448433412315, 2.638427012816831674 ) ) ;
#37932 = DIRECTION ( 'NONE',  ( 1.000000000000000000, -5.818595309480552676E-17, 0.000000000000000000 ) ) ;
#37933 = CARTESIAN_POINT ( 'NONE',  ( 0.1532563361054082862, 31.21726448433412315, 2.638427012816831674 ) ) ;
#37934 = ORIENTED_EDGE ( 'NONE', *, *, #38319, .T. ) ;
#37935 = CARTESIAN_POINT ( 'NONE',  ( 10.00000000000000000, 39.75893115100078745, -9.846743663894594434 ) ) ;
#37936 = CARTESIAN_POINT ( 'NONE',  ( -9.382169495545422677, -21.50136533006957862, -9.382169495545417348 ) ) ;
#37937 = CARTESIAN_POINT ( 'NONE',  ( 19.42250999205614548, 30.98035201082150536, -5.440088680355545492 ) ) ;
#37938 = CARTESIAN_POINT ( 'NONE',  ( 18.52753015748617571, 33.09226448433411605, 4.923371831947298993 ) ) ;
#37939 = CARTESIAN_POINT ( 'NONE',  ( 13.43411237798105340, 25.58196800326374998, 12.81628187352647963 ) ) ;
#37941 = CARTESIAN_POINT ( 'NONE',  ( 10.00000000000000178, 54.31368534415484106, 10.88017736071110342 ) ) ;
#37940 = CARTESIAN_POINT ( 'NONE',  ( 4.559911319644449179, 67.23035201082150536, -9.422509992056141925 ) ) ;
#37943 = CARTESIAN_POINT ( 'NONE',  ( 15.44008868035555260, 4.730352010821504471, 9.422509992056143702 ) ) ;
#37942 = CARTESIAN_POINT ( 'NONE',  ( -0.8801773607110991993, 27.85535201082150181, -2.915334737309923874 ) ) ;
#37944 = CARTESIAN_POINT ( 'NONE',  ( -4.164238869374098151, 61.59541550158063217, -3.795296366450310543 ) ) ;
#37945 = ADVANCED_FACE ( 'NONE', ( #54548 ), #618, .F. ) ;
#37946 = CARTESIAN_POINT ( 'NONE',  ( 21.09922568453595559, 27.04030133659708568, -6.408140936763230044 ) ) ;
#37947 = DIRECTION ( 'NONE',  ( 0.000000000000000000, 0.000000000000000000, 1.000000000000000000 ) ) ;
#37948 = ORIENTED_EDGE ( 'NONE', *, *, #19309, .T. ) ;
#37949 = CARTESIAN_POINT ( 'NONE',  ( 19.38216949554541202, 20.99863466993042138, 9.382169495545424454 ) ) ;
#37950 = CARTESIAN_POINT ( 'NONE',  ( 20.88017736071110519, 5.563685344154837509, 2.639326808657452039E-16 ) ) ;
#37951 = CARTESIAN_POINT ( 'NONE',  ( -0.8801773607111008646, 48.27201867748816966, 2.915334737309923430 ) ) ;
#37952 = ORIENTED_EDGE ( 'NONE', *, *, #10801, .F. ) ;
#37953 = MECHANICAL_DESIGN_GEOMETRIC_PRESENTATION_REPRESENTATION (  '', ( #28368 ), #33218 ) ;
#37954 = CARTESIAN_POINT ( 'NONE',  ( 17.96484262340118221, 59.93868534415484106, 7.964842623401181321 ) ) ;
#37955 = CARTESIAN_POINT ( 'NONE',  ( 14.92337183194729633, 37.67559781766745175, 8.527530157486181039 ) ) ;
#37956 = CARTESIAN_POINT ( 'NONE',  ( 14.92337183194729988, 24.34226448433411960, -8.527530157486177487 ) ) ;
#37957 = B_SPLINE_CURVE_WITH_KNOTS ( 'NONE', 3,
 ( #23576, #25046, #54045, #84555, #57968, #58457 ),
 .UNSPECIFIED., .F., .F.,
 ( 4, 2, 4 ),
 ( 3.409110551474090893E-05, 0.0004400426677365675086, 0.0008459942299583938846 ),
 .UNSPECIFIED. ) ;
#37958 = AXIS2_PLACEMENT_3D ( 'NONE', #95905, #6359, #59851 ) ;
#37959 = CARTESIAN_POINT ( 'NONE',  ( 18.52753015748618282, 18.92559781766745175, -4.923371831947291888 ) ) ;
#37960 = CARTESIAN_POINT ( 'NONE',  ( 14.56089864660132349, 14.99999999999807088, -1.374314915483334731 ) ) ;
#37961 = DIRECTION ( 'NONE',  ( 0.000000000000000000, 0.000000000000000000, -1.000000000000000000 ) ) ;
#37964 = DIRECTION ( 'NONE',  ( 0.000000000000000000, 1.000000000000000000, 0.000000000000000000 ) ) ;
#37963 = VECTOR ( 'NONE', #39687, 1000.000000000000000 ) ;
#37962 = CARTESIAN_POINT ( 'NONE',  ( 12.63842701281683922, 14.55059781766744997, -9.846743663894590881 ) ) ;
#37965 = DIRECTION ( 'NONE',  ( 1.000000000000000000, -0.000000000000000000, 0.000000000000000000 ) ) ;
#37967 = ORIENTED_EDGE ( 'NONE', *, *, #96884, .T. ) ;
#37966 = CARTESIAN_POINT ( 'NONE',  ( 19.84674366389459266, 28.30059781766745886, 2.638427012816836559 ) ) ;
#37968 = AXIS2_PLACEMENT_3D ( 'NONE', #29280, #59776, #90269 ) ;
#37969 = CARTESIAN_POINT ( 'NONE',  ( 7.850000000000003197, 98.49999999999998579, 8.000000000000000000 ) ) ;
#37970 = EDGE_CURVE ( 'NONE', #32864, #91030, #55042, .T. ) ;
#37971 = CARTESIAN_POINT ( 'NONE',  ( -1.099225684535947600, 14.54030133659708568, 6.408140936763237150 ) ) ;
#37972 = CARTESIAN_POINT ( 'NONE',  ( 12.91533473730993009, 56.60535201082151247, -10.88017736071109987 ) ) ;
#37973 = CARTESIAN_POINT ( 'NONE',  ( -2.266590686148945544, 36.38708216824730357, -7.082119434687050408 ) ) ;
#37974 = EDGE_CURVE ( 'NONE', #18747, #79425, #78053, .T. ) ;
#37975 = CARTESIAN_POINT ( 'NONE',  ( 1.821708436314945612, 41.66792564121896447, -6.500000000000040856 ) ) ;
#37976 = CARTESIAN_POINT ( 'NONE',  ( 20.36894250292379382, 33.67874883491396076, 10.36894250292379205 ) ) ;
#37977 = CARTESIAN_POINT ( 'NONE',  ( 10.00000000000000178, 58.05374883491397497, 14.16423886937410082 ) ) ;
#37978 = CARTESIAN_POINT ( 'NONE',  ( 24.16423886937410614, 14.51208216824730179, -3.795296366450302550 ) ) ;
#37980 = LINE ( 'NONE', #37483, #89301 ) ;
#37979 = CARTESIAN_POINT ( 'NONE',  ( 2.917880565312950480, 20.97041550158063217, -12.26659068614894821 ) ) ;
#37981 = CARTESIAN_POINT ( 'NONE',  ( 12.91533473730992121, 49.52201867748817676, 10.88017736071110164 ) ) ;
#37983 = CARTESIAN_POINT ( 'NONE',  ( 14.92337183194729633, 42.67559781766745886, 8.527530157486181039 ) ) ;
#37982 = CARTESIAN_POINT ( 'NONE',  ( 17.39651004071838614, 62.93575266056827644, 6.500000000000032863 ) ) ;
#37984 = CARTESIAN_POINT ( 'NONE',  ( 10.00000000000000178, 19.31368534415484106, 10.88017736071110342 ) ) ;
#37985 = CARTESIAN_POINT ( 'NONE',  ( -2.816281873526473856, 54.33196800326376064, 3.434112377981055619 ) ) ;
#37986 = CARTESIAN_POINT ( 'NONE',  ( 0.1532563361054100626, 60.80059781766744464, -2.638427012816831230 ) ) ;
#37987 = CARTESIAN_POINT ( 'NONE',  ( 20.00000000000286349, 82.51979501594313149, -5.046714348924735027 ) ) ;
#37988 = CARTESIAN_POINT ( 'NONE',  ( -1.099225684535947600, 53.70696800326376064, -6.408140936763238038 ) ) ;
#37989 = CARTESIAN_POINT ( 'NONE',  ( 14.16423886937410437, -15.90458449841935895, 3.795296366450304770 ) ) ;
#37990 = CARTESIAN_POINT ( 'NONE',  ( -0.8801773607111008646, 43.27201867748817676, 2.915334737309923430 ) ) ;
#37991 = CARTESIAN_POINT ( 'NONE',  ( 12.63842701281683922, 54.55059781766745175, -9.846743663894590881 ) ) ;
#37992 = CARTESIAN_POINT ( 'NONE',  ( 17.08211943468705840, 45.13708216824730357, -12.26659068614894466 ) ) ;
#37993 = VERTEX_POINT ( 'NONE', #45585 ) ;
#37994 = CARTESIAN_POINT ( 'NONE',  ( 20.36894250292379738, 4.928748834913967869, -10.36894250292379027 ) ) ;
#37995 = CARTESIAN_POINT ( 'NONE',  ( 15.44008868035555793, 66.39701867748817676, -9.422509992056140149 ) ) ;
#37996 = DIRECTION ( 'NONE',  ( 1.000000000000000000, 0.000000000000000000, 0.000000000000000000 ) ) ;
#37997 = CARTESIAN_POINT ( 'NONE',  ( -0.3689425029237898834, 56.17874883491396076, -10.36894250292378850 ) ) ;
#37998 = CARTESIAN_POINT ( 'NONE',  ( 21.09922568453595559, 17.04030133659708923, -6.408140936763230044 ) ) ;
#37999 = CARTESIAN_POINT ( 'NONE',  ( 2.815433093577016876, 14.63606915880329851, 14.73340885523756327 ) ) ;
#38000 = CARTESIAN_POINT ( 'NONE',  ( 7.084665262690076126, 52.02201867748816255, -10.88017736071110164 ) ) ;
#38001 = CYLINDRICAL_SURFACE ( 'NONE', #78982, 0.5000000000000004441 ) ;
#38002 = CARTESIAN_POINT ( 'NONE',  ( -46.94000000000001194, 100.7103534007538883, -8.569772222592094479 ) ) ;
#38003 = CARTESIAN_POINT ( 'NONE',  ( 6.204703633549690345, 62.84541550158063927, 14.16423886937410082 ) ) ;
#38004 = CARTESIAN_POINT ( 'NONE',  ( -5.440088680355558814, 32.23035201082149825, -9.422509992056136596 ) ) ;
#38005 = CARTESIAN_POINT ( 'NONE',  ( 2.035157376598824452, 13.68868534415483751, 7.964842623401179544 ) ) ;
#38006 = CARTESIAN_POINT ( 'NONE',  ( 4.559911319644449179, 22.23035201082150536, -9.422509992056141925 ) ) ;
#38007 = CARTESIAN_POINT ( 'NONE',  ( 10.00000000000000178, 62.25893115100078745, 9.846743663894594434 ) ) ;
#38008 = CARTESIAN_POINT ( 'NONE',  ( 19.38216949554541202, 45.99863466993041072, 9.382169495545424454 ) ) ;
#38009 = EDGE_LOOP ( 'NONE', ( #809, #86714, #87596, #3055 ) ) ;
#38010 = ADVANCED_FACE ( 'NONE', ( #84085 ), #2084, .T. ) ;
#38011 = CARTESIAN_POINT ( 'NONE',  ( 12.91533473730992121, 19.52201867748816611, 10.88017736071110164 ) ) ;
#38012 = CARTESIAN_POINT ( 'NONE',  ( 16.40814093676324603, 22.45696800326375353, -11.09922568453594671 ) ) ;
#38013 = CARTESIAN_POINT ( 'NONE',  ( -13.78891971893217239, 14.49999999999999112, 5.904717858191482094 ) ) ;
#38014 = CARTESIAN_POINT ( 'NONE',  ( 10.00000000000000178, 42.25893115100078745, 9.846743663894594434 ) ) ;
#38015 = CARTESIAN_POINT ( 'NONE',  ( 2.035157376598822676, 37.43868534415484106, -7.964842623401177768 ) ) ;
#38016 = CARTESIAN_POINT ( 'NONE',  ( 21.09922568453595559, 27.04030133659708568, -6.408140936763230044 ) ) ;
#38018 = FACE_OUTER_BOUND ( 'NONE', #97895, .T. ) ;
#38017 = CARTESIAN_POINT ( 'NONE',  ( 15.44008868035555260, 49.73035201082150536, 9.422509992056143702 ) ) ;
#38019 = DIRECTION ( 'NONE',  ( 0.000000000000000000, 0.000000000000000000, -1.000000000000000000 ) ) ;
#38020 = CARTESIAN_POINT ( 'NONE',  ( 16.40814093676323893, 45.79030133659708923, 11.09922568453595026 ) ) ;
#38021 = EDGE_LOOP ( 'NONE', ( #12349, #88843, #80903, #38246, #42500, #22083 ) ) ;
#38022 = DIRECTION ( 'NONE',  ( 0.000000000000000000, 0.000000000000000000, -1.000000000000000000 ) ) ;
#38023 = CARTESIAN_POINT ( 'NONE',  ( 20.88017736071110875, 55.77201867748816966, -2.915334737309920765 ) ) ;
#38025 = CARTESIAN_POINT ( 'NONE',  ( -4.164238869374098151, 1.595415501580634388, -3.795296366450310543 ) ) ;
#38024 = CARTESIAN_POINT ( 'NONE',  ( 19.38216949554541202, 30.99863466993042138, 9.382169495545424454 ) ) ;
#38026 = CARTESIAN_POINT ( 'NONE',  ( 0.1532563361054083140, 6.008931151000784787, 1.131784320476157264E-15 ) ) ;
#38027 = CARTESIAN_POINT ( 'NONE',  ( 0.5774900079438607392, 58.48035201082151247, 5.440088680355550821 ) ) ;
#38028 = CARTESIAN_POINT ( 'NONE',  ( 6.204703633549690345, 47.84541550158064638, 14.16423886937410082 ) ) ;
#38029 = VECTOR ( 'NONE', #4139, 999.9999999999998863 ) ;
#38030 = CARTESIAN_POINT ( 'NONE',  ( 5.076628168052704559, 65.17559781766745175, -8.527530157486179263 ) ) ;
#38031 = CARTESIAN_POINT ( 'NONE',  ( 14.92337183194729633, 17.67559781766745175, 8.527530157486181039 ) ) ;
#38032 = CARTESIAN_POINT ( 'NONE',  ( 0.1532563361054083140, 6.008931151000784787, 1.131784320476157264E-15 ) ) ;
#38033 = DIRECTION ( 'NONE',  ( 0.000000000000000000, 0.000000000000000000, 1.000000000000000000 ) ) ;
#38034 = CARTESIAN_POINT ( 'NONE',  ( 6.204703633549690345, 42.84541550158063217, 14.16423886937410082 ) ) ;
#38035 = DIRECTION ( 'NONE',  ( 0.000000000000000000, 0.000000000000000000, -1.000000000000000000 ) ) ;
#38036 = CIRCLE ( 'NONE', #98720, 0.2500000000000002220 ) ;
#38037 = CARTESIAN_POINT ( 'NONE',  ( 19.42250999205614548, 10.98035201082150358, -5.440088680355545492 ) ) ;
#38038 = CARTESIAN_POINT ( 'NONE',  ( -7.080143328648153656, -69.54337233422633346, -3.749999999999999556 ) ) ;
#38039 = VECTOR ( 'NONE', #70133, 1000.000000000000000 ) ;
#38040 = ORIENTED_EDGE ( 'NONE', *, *, #37641, .F. ) ;
#38041 = CARTESIAN_POINT ( 'NONE',  ( 7.084665262690076126, 4.105352010821503583, 10.88017736071109987 ) ) ;
#38042 = CARTESIAN_POINT ( 'NONE',  ( -0.3689425029237898834, 61.17874883491396076, -10.36894250292378850 ) ) ;
#38043 = CARTESIAN_POINT ( 'NONE',  ( 10.00000000000000000, 49.75893115100078745, -9.846743663894594434 ) ) ;
#38044 = CARTESIAN_POINT ( 'NONE',  ( 0.6178305044545838731, 44.74863466993042493, 9.382169495545420901 ) ) ;
#38046 = CARTESIAN_POINT ( 'NONE',  ( 22.26659068614894466, 3.887082168247300906, 7.082119434687054849 ) ) ;
#38045 = CARTESIAN_POINT ( 'NONE',  ( 2.189666204609302724, 2.388632911257126956E-16, -14.46180170876169058 ) ) ;
#38047 = CARTESIAN_POINT ( 'NONE',  ( 0.5774900079438607392, 8.480352010821505360, 5.440088680355550821 ) ) ;
#38048 = CARTESIAN_POINT ( 'NONE',  ( -4.164238869374099039, 66.80374883491396076, 8.674139862899312516E-16 ) ) ;
#38049 = CARTESIAN_POINT ( 'NONE',  ( 1.472469842513823179, 41.42559781766745886, 4.923371831947296329 ) ) ;
#38050 = CARTESIAN_POINT ( 'NONE',  ( 17.84635730667658393, 43.63791097397316321, 6.499999999999926281 ) ) ;
#38051 = CARTESIAN_POINT ( 'NONE',  ( 14.92337183194729633, 27.67559781766745530, 8.527530157486181039 ) ) ;
#38052 = CARTESIAN_POINT ( 'NONE',  ( 19.50000000000000711, 105.0000000000000000, 4.500000000000000888 ) ) ;
#38053 = CARTESIAN_POINT ( 'NONE',  ( 2.638427012816835227, 12.46726448433412315, 9.846743663894590881 ) ) ;
#38054 = ORIENTED_EDGE ( 'NONE', *, *, #8530, .T. ) ;
#38055 = ORIENTED_EDGE ( 'NONE', *, *, #63417, .F. ) ;
#38056 = CARTESIAN_POINT ( 'NONE',  ( 14.62617646268085281, 15.00000000000000000, 3.327906561566980503 ) ) ;
#38057 = VERTEX_POINT ( 'NONE', #91078 ) ;
#38059 = CARTESIAN_POINT ( 'NONE',  ( 4.559911319644449179, 32.23035201082150536, -9.422509992056141925 ) ) ;
#38058 = CARTESIAN_POINT ( 'NONE',  ( 4.559911319644449179, 32.23035201082150536, -9.422509992056141925 ) ) ;
#38061 = CARTESIAN_POINT ( 'NONE',  ( 3.591859063236763294, 28.29030133659708568, -11.09922568453595026 ) ) ;
#38060 = CARTESIAN_POINT ( 'NONE',  ( 19.84674366389459621, 63.50893115100078745, 7.409399052514197653E-17 ) ) ;
#38062 = CARTESIAN_POINT ( 'NONE',  ( 17.08211943468705840, 10.13708216824730179, -12.26659068614894466 ) ) ;
#38064 = ADVANCED_FACE ( 'NONE', ( #92554 ), #9046, .T. ) ;
#38063 = CARTESIAN_POINT ( 'NONE',  ( 10.00000000000000178, 64.31368534415483396, 10.88017736071110342 ) ) ;
#38065 = B_SPLINE_CURVE_WITH_KNOTS ( 'NONE', 3,
 ( #79899, #50382, #11904, #20885, #34387, #57395 ),
 .UNSPECIFIED., .F., .F.,
 ( 4, 2, 4 ),
 ( 3.409110551496096809E-05, 0.0004400426677367864632, 0.0008459942299586120261 ),
 .UNSPECIFIED. ) ;
#38066 = CARTESIAN_POINT ( 'NONE',  ( 13.43411237798106583, 42.66530133659707502, -12.81628187352647252 ) ) ;
#38067 = EDGE_LOOP ( 'NONE', ( #81036, #80376, #98299, #15351, #78962, #84021 ) ) ;
#38068 = CARTESIAN_POINT ( 'NONE',  ( 1.472469842513823179, 50.59226448433411605, -4.923371831947296329 ) ) ;
#38069 = CARTESIAN_POINT ( 'NONE',  ( 17.96484262340118221, 11.18868534415484106, -7.964842623401177768 ) ) ;
#38070 = ORIENTED_EDGE ( 'NONE', *, *, #29511, .T. ) ;
#38071 = CARTESIAN_POINT ( 'NONE',  ( 2.035157376598824452, 13.68868534415483751, 7.964842623401179544 ) ) ;
#38072 = B_SPLINE_CURVE_WITH_KNOTS ( 'NONE', 3,
 ( #31473, #85481, #61976, #15999, #76983, #24001 ),
 .UNSPECIFIED., .F., .F.,
 ( 4, 2, 4 ),
 ( 0.000000000000000000, 0.0002701661927229447686, 0.0005403323854458895372 ),
 .UNSPECIFIED. ) ;
#38073 = ORIENTED_EDGE ( 'NONE', *, *, #1499, .F. ) ;
#38074 = CARTESIAN_POINT ( 'NONE',  ( 15.44008868035555260, 54.73035201082150536, 9.422509992056143702 ) ) ;
#38075 = CARTESIAN_POINT ( 'NONE',  ( 19.42250999205614548, 60.98035201082151247, -5.440088680355545492 ) ) ;
#38076 = CARTESIAN_POINT ( 'NONE',  ( 2.035157376598824452, 63.68868534415484106, 7.964842623401179544 ) ) ;
#38077 = VECTOR ( 'NONE', #58764, 1000.000000000000000 ) ;
#38078 = ADVANCED_FACE ( 'NONE', ( #9066 ), #37757, .T. ) ;
#38079 = DIRECTION ( 'NONE',  ( 0.000000000000000000, 1.000000000000000000, 0.000000000000000000 ) ) ;
#38080 = CARTESIAN_POINT ( 'NONE',  ( 20.88017736071110164, 55.35535201082149825, 2.915334737309930979 ) ) ;
#38081 = CARTESIAN_POINT ( 'NONE',  ( -46.94000000000001194, 103.0000000000000000, 5.997726559847112782 ) ) ;
#38082 = CARTESIAN_POINT ( 'NONE',  ( -46.94000000000001194, 100.4344880109628093, 9.014049137172644777 ) ) ;
#38084 = ORIENTED_EDGE ( 'NONE', *, *, #47570, .F. ) ;
#38083 = CARTESIAN_POINT ( 'NONE',  ( 8.650320195642805743, -1.048895414480025323, 4.000000000000000000 ) ) ;
#38085 = EDGE_CURVE ( 'NONE', #65595, #94683, #51329, .T. ) ;
#38086 = CARTESIAN_POINT ( 'NONE',  ( 14.92337183194729633, 42.67559781766745886, 8.527530157486181039 ) ) ;
#38087 = VERTEX_POINT ( 'NONE', #34501 ) ;
#38088 = CARTESIAN_POINT ( 'NONE',  ( 3.558677480090427725, 70.40124509038875544, 12.00000000000000000 ) ) ;
#38089 = CARTESIAN_POINT ( 'NONE',  ( 0.2751277870542891413, 24.36607318730131411, -6.499999999999989342 ) ) ;
#38090 = ADVANCED_FACE ( 'NONE', ( #94039 ), #48033, .F. ) ;
#38091 = CARTESIAN_POINT ( 'NONE',  ( 17.08211943468705130, 3.470415501580634388, 12.26659068614894998 ) ) ;
#38092 = MECHANICAL_DESIGN_GEOMETRIC_PRESENTATION_REPRESENTATION (  '', ( #68426 ), #25466 ) ;
#38093 = ORIENTED_EDGE ( 'NONE', *, *, #28003, .T. ) ;
#38095 = CARTESIAN_POINT ( 'NONE',  ( 10.00000000000000000, 61.81368534415484106, -10.88017736071110342 ) ) ;
#38094 = DIRECTION ( 'NONE',  ( -2.042810365310288034E-14, 0.000000000000000000, 1.000000000000000000 ) ) ;
#38096 = CARTESIAN_POINT ( 'NONE',  ( 17.96484262340118221, 4.938685344154837509, 7.964842623401181321 ) ) ;
#38097 = PRESENTATION_STYLE_ASSIGNMENT (( #38578 ) ) ;
#38099 = ORIENTED_EDGE ( 'NONE', *, *, #50212, .T. ) ;
#38098 = CARTESIAN_POINT ( 'NONE',  ( 22.81628187352647785, 41.62363466993042493, 6.195893100308588602E-16 ) ) ;
#38100 = CARTESIAN_POINT ( 'NONE',  ( 13.21236992757670059, -0.03417435944610275333, 5.338143956176803151 ) ) ;
#38101 = CARTESIAN_POINT ( 'NONE',  ( 10.00000000000000000, 44.75893115100078745, -9.846743663894594434 ) ) ;
#38102 = CARTESIAN_POINT ( 'NONE',  ( -1.099225684535947600, 14.54030133659708568, 6.408140936763237150 ) ) ;
#38103 = CARTESIAN_POINT ( 'NONE',  ( 1.472469842513823179, 26.42559781766745175, 4.923371831947296329 ) ) ;
#38104 = CIRCLE ( 'NONE', #55649, 0.2500000000000002220 ) ;
#38105 = CARTESIAN_POINT ( 'NONE',  ( 0.6178305044545838731, 9.748634669930416052, 9.382169495545420901 ) ) ;
#38106 = VECTOR ( 'NONE', #80078, 1000.000000000000000 ) ;
#38107 = CYLINDRICAL_SURFACE ( 'NONE', #38804, 2.000000000000000888 ) ;
#38108 = CARTESIAN_POINT ( 'NONE',  ( 2.791683348922240793, 1.633931151000784565, 7.208316651077764092 ) ) ;
#38109 = ORIENTED_EDGE ( 'NONE', *, *, #8903, .T. ) ;
#38110 = ORIENTED_EDGE ( 'NONE', *, *, #90514, .T. ) ;
#38111 = CARTESIAN_POINT ( 'NONE',  ( 4.559911319644449179, 22.23035201082150536, -9.422509992056141925 ) ) ;
#38112 = CARTESIAN_POINT ( 'NONE',  ( 22.26659068614895176, 14.72041550158063572, -7.082119434687042414 ) ) ;
#38113 = CARTESIAN_POINT ( 'NONE',  ( 0.1532563361054083140, 46.00893115100079456, 1.131784320476157264E-15 ) ) ;
#38114 = CARTESIAN_POINT ( 'NONE',  ( 14.92337183194729633, 2.675597817667451750, 8.527530157486181039 ) ) ;
#38116 = CARTESIAN_POINT ( 'NONE',  ( -7.081429851441987999, -84.79152421822192309, -2.750000000000000444 ) ) ;
#38115 = CARTESIAN_POINT ( 'NONE',  ( 13.43411237798105340, 35.58196800326375353, 12.81628187352647963 ) ) ;
#38117 = CARTESIAN_POINT ( 'NONE',  ( 2.035157376598824452, 8.688685344154839285, 7.964842623401179544 ) ) ;
#38118 = DIRECTION ( 'NONE',  ( 0.4461978131097943945, 0.000000000000000000, 0.8949343616020322134 ) ) ;
#38119 = EDGE_CURVE ( 'NONE', #35357, #25656, #96932, .T. ) ;
#38120 = CARTESIAN_POINT ( 'NONE',  ( 3.591859063236761518, 9.956968003263753531, 11.09922568453594849 ) ) ;
#38121 = CARTESIAN_POINT ( 'NONE',  ( 17.20831665107776587, 29.13393115100078390, -7.208316651077762316 ) ) ;
#38122 = CARTESIAN_POINT ( 'NONE',  ( 2.915334737309928315, -15.47798132251182857, 10.88017736071109987 ) ) ;
#38123 = CARTESIAN_POINT ( 'NONE',  ( -2.816281873526473856, 29.12363466993041783, 9.499525473075851096E-16 ) ) ;
#38124 = LINE ( 'NONE', #53593, #19670 ) ;
#38126 = CARTESIAN_POINT ( 'NONE',  ( 14.16722289976681814, 0.5000000000000004441, 4.928467845925615265 ) ) ;
#38125 = CARTESIAN_POINT ( 'NONE',  ( 0.5774900079438590739, 37.64701867748817676, -5.440088680355550821 ) ) ;
#38127 = EDGE_CURVE ( 'NONE', #51757, #78249, #15495, .T. ) ;
#38128 = CARTESIAN_POINT ( 'NONE',  ( 13.86102707272223356, -3.662993980401220239E-15, -4.666951904077198954 ) ) ;
#38129 = CARTESIAN_POINT ( 'NONE',  ( 15.44008868035555793, 66.39701867748817676, -9.422509992056140149 ) ) ;
#38130 = CARTESIAN_POINT ( 'NONE',  ( 17.96484262340118221, 34.93868534415482685, 7.964842623401181321 ) ) ;
#38131 = CARTESIAN_POINT ( 'NONE',  ( 20.88017736071110875, 40.77201867748818387, -2.915334737309920765 ) ) ;
#38132 = CARTESIAN_POINT ( 'NONE',  ( 20.10421743870887212, 60.60736173766203194, -6.337391062633416006 ) ) ;
#38133 = CARTESIAN_POINT ( 'NONE',  ( 2.035157376598824452, 63.68868534415484106, 7.964842623401179544 ) ) ;
#38134 = UNCERTAINTY_MEASURE_WITH_UNIT (LENGTH_MEASURE( 1.000000000000000082E-05 ), #12870, 'distance_accuracy_value', 'NONE');
#38135 = CARTESIAN_POINT ( 'NONE',  ( 18.52753015748617571, 53.09226448433412315, 4.923371831947298993 ) ) ;
#38137 = CARTESIAN_POINT ( 'NONE',  ( 70.19910379943081580, 41.67447916666664298, 10.00000000000000000 ) ) ;
#38136 = CARTESIAN_POINT ( 'NONE',  ( 0.5774900079438607392, 13.48035201082150358, 5.440088680355550821 ) ) ;
#38138 = CARTESIAN_POINT ( 'NONE',  ( 10.00000000000000178, 15.37363466993042138, 12.81628187352647608 ) ) ;
#38139 = VERTEX_POINT ( 'NONE', #25561 ) ;
#38140 = CARTESIAN_POINT ( 'NONE',  ( -0.8801773607111009756, 33.06368534415484106, 1.068504757029289695E-15 ) ) ;
#38141 = ADVANCED_FACE ( 'NONE', ( #80016 ), #88914, .T. ) ;
#38143 = DIRECTION ( 'NONE',  ( 1.000000000000000000, 0.000000000000000000, 0.000000000000000000 ) ) ;
#38142 = CARTESIAN_POINT ( 'NONE',  ( 3.591859063236763294, -1.709698663402913210, -11.09922568453595026 ) ) ;
#38144 = CARTESIAN_POINT ( 'NONE',  ( 17.96484262340118221, 19.93868534415484106, 7.964842623401181321 ) ) ;
#38145 = CARTESIAN_POINT ( 'NONE',  ( 2.035157376598824452, 28.68868534415484106, 7.964842623401179544 ) ) ;
#38146 = CARTESIAN_POINT ( 'NONE',  ( 22.26659068614895176, 39.72041550158063217, -7.082119434687042414 ) ) ;
#38147 = CARTESIAN_POINT ( 'NONE',  ( 5.076628168052703671, 21.84226448433411960, 8.527530157486179263 ) ) ;
#38148 = VECTOR ( 'NONE', #81150, 1000.000000000000114 ) ;
#38149 = CARTESIAN_POINT ( 'NONE',  ( 12.91533473730993009, 51.60535201082149825, -10.88017736071109987 ) ) ;
#38150 = CARTESIAN_POINT ( 'NONE',  ( 2.917880565312950480, 0.9704155015806342766, -12.26659068614894821 ) ) ;
#38151 = CARTESIAN_POINT ( 'NONE',  ( 2.791683348922237240, 55.38393115100078745, -7.208316651077763204 ) ) ;
#38152 = ORIENTED_EDGE ( 'NONE', *, *, #66289, .T. ) ;
#38153 = ORIENTED_EDGE ( 'NONE', *, *, #39772, .T. ) ;
#38154 = CARTESIAN_POINT ( 'NONE',  ( 17.08211943468705840, 35.13708216824730357, -12.26659068614894466 ) ) ;
#38155 = CARTESIAN_POINT ( 'NONE',  ( 20.36894250292379738, 24.92874883491396787, -10.36894250292379027 ) ) ;
#38156 = CARTESIAN_POINT ( 'NONE',  ( 5.076628168052704559, 10.17559781766745175, -8.527530157486179263 ) ) ;
#38157 = CARTESIAN_POINT ( 'NONE',  ( 6.565887622018943937, 10.16530133659708746, 12.81628187352647430 ) ) ;
#38158 = CARTESIAN_POINT ( 'NONE',  ( 14.92337183194729988, 54.34226448433412315, -8.527530157486177487 ) ) ;
#38159 = CARTESIAN_POINT ( 'NONE',  ( -11.60563658639003037, -81.99692803277919495, 3.750000000000000000 ) ) ;
#38161 = CARTESIAN_POINT ( 'NONE',  ( 19.38216949554541557, 17.24863466993041783, -9.382169495545420901 ) ) ;
#38160 = CARTESIAN_POINT ( 'NONE',  ( 2.035157376598824452, 43.68868534415484106, 7.964842623401179544 ) ) ;
#38162 = CARTESIAN_POINT ( 'NONE',  ( 22.26659068614895176, 34.72041550158063927, -7.082119434687042414 ) ) ;
#38163 = CARTESIAN_POINT ( 'NONE',  ( 20.88017736071110875, 10.77201867748817143, -2.915334737309920765 ) ) ;
#38164 = CARTESIAN_POINT ( 'NONE',  ( 20.88017736071110164, 25.35535201082150891, 2.915334737309930979 ) ) ;
#38165 = CARTESIAN_POINT ( 'NONE',  ( 20.15039907845753930, 5.601585745166425490, -6.262539305110069954 ) ) ;
#38166 = CARTESIAN_POINT ( 'NONE',  ( 0.5774900079438590739, 62.64701867748817676, -5.440088680355550821 ) ) ;
#38167 = TOROIDAL_SURFACE ( 'NONE', #3050, 10.65000000000026326, 0.2500000000000000000 ) ;
#38168 = CARTESIAN_POINT ( 'NONE',  ( 4.923371831947295441, -25.65773551566588040, -8.527530157486179263 ) ) ;
#38169 = ORIENTED_EDGE ( 'NONE', *, *, #67548, .F. ) ;
#38170 = DIRECTION ( 'NONE',  ( -0.000000000000000000, 1.000000000000000000, 4.510281037539694028E-14 ) ) ;
#38171 = CARTESIAN_POINT ( 'NONE',  ( -13.55255535720589322, -0.03417435944610275333, -4.403492169843143067 ) ) ;
#38172 = EDGE_LOOP ( 'NONE', ( #46183, #91151, #74053, #78854 ) ) ;
#38173 = CARTESIAN_POINT ( 'NONE',  ( -4.249999999999994671, 43.00000000000000000, 6.250000000000000000 ) ) ;
#38175 = CARTESIAN_POINT ( 'NONE',  ( 10.00000000000000178, 63.05374883491396076, 14.16423886937410082 ) ) ;
#38174 = CARTESIAN_POINT ( 'NONE',  ( -0.3689425029237898834, 61.17874883491396076, -10.36894250292378850 ) ) ;
#38177 = CARTESIAN_POINT ( 'NONE',  ( 14.92337183194729633, 62.67559781766745886, 8.527530157486181039 ) ) ;
#38176 = CARTESIAN_POINT ( 'NONE',  ( 17.20831665107776587, 19.13393115100078035, -7.208316651077762316 ) ) ;
#38178 = CYLINDRICAL_SURFACE ( 'NONE', #83803, 0.2500000000000002220 ) ;
#38179 = CIRCLE ( 'NONE', #39742, 2.000000000000001776 ) ;
#38180 = CARTESIAN_POINT ( 'NONE',  ( -2.258855624577742027, 14.95037108984192820, 14.57926203528949038 ) ) ;
#38181 = EDGE_CURVE ( 'NONE', #6552, #18240, #56053, .T. ) ;
#38183 = CARTESIAN_POINT ( 'NONE',  ( 1.472469842513823179, 11.42559781766745175, 4.923371831947296329 ) ) ;
#38182 = AXIS2_PLACEMENT_3D ( 'NONE', #96238, #33729, #72233 ) ;
#38184 = EDGE_CURVE ( 'NONE', #31822, #6951, #15834, .T. ) ;
#38185 = CARTESIAN_POINT ( 'NONE',  ( 3.469446951953614189E-15, 20.37363466993041783, 12.81628187352647608 ) ) ;
#38186 = EDGE_LOOP ( 'NONE', ( #45442, #78881, #1733, #91031 ) ) ;
#38187 = CARTESIAN_POINT ( 'NONE',  ( -2.266590686148945544, 31.38708216824730002, -7.082119434687050408 ) ) ;
#38188 = CARTESIAN_POINT ( 'NONE',  ( 24.16423886937410614, 49.30374883491396787, 8.672049930838204340E-16 ) ) ;
#38189 = ORIENTED_EDGE ( 'NONE', *, *, #77791, .T. ) ;
#38190 = CARTESIAN_POINT ( 'NONE',  ( -2.816281873526473856, 54.33196800326376064, 3.434112377981055619 ) ) ;
#38191 = CARTESIAN_POINT ( 'NONE',  ( 20.88017736071110164, 25.35535201082150891, 2.915334737309930979 ) ) ;
#38192 = CARTESIAN_POINT ( 'NONE',  ( 19.84674366389459266, 43.71726448433410894, -2.638427012816827677 ) ) ;
#38193 = CARTESIAN_POINT ( 'NONE',  ( 10.00000000000000000, 21.81368534415484106, -10.88017736071110342 ) ) ;
#38194 = CARTESIAN_POINT ( 'NONE',  ( -5.845017550302832987, -0.03417435944610275333, -14.89003580495041668 ) ) ;
#38195 = CARTESIAN_POINT ( 'NONE',  ( 10.64017930668204670, 14.49999999999999112, 10.57291749337225362 ) ) ;
#38196 = CARTESIAN_POINT ( 'NONE',  ( 0.1532563361054100626, 60.80059781766744464, -2.638427012816831230 ) ) ;
#38197 = CARTESIAN_POINT ( 'NONE',  ( 17.20831665107776587, 44.13393115100078745, -7.208316651077762316 ) ) ;
#38198 = STYLED_ITEM ( 'NONE', ( #45069 ), #26526 ) ;
#38199 = CARTESIAN_POINT ( 'NONE',  ( 0.000000000000000000, 14.49999999999999822, 0.000000000000000000 ) ) ;
#38200 = EDGE_CURVE ( 'NONE', #73080, #71557, #88007, .T. ) ;
#38201 = CARTESIAN_POINT ( 'NONE',  ( -14.76044511231849299, 0.2301501264598455332, -2.313329003772577774 ) ) ;
#38202 = ORIENTED_EDGE ( 'NONE', *, *, #31510, .T. ) ;
#38203 = SURFACE_STYLE_FILL_AREA ( #45689 ) ;
#38204 = CARTESIAN_POINT ( 'NONE',  ( 18.52753015748618282, 33.92559781766745886, -4.923371831947291888 ) ) ;
#38205 = LINE ( 'NONE', #712, #5340 ) ;
#38206 = CARTESIAN_POINT ( 'NONE',  ( 6.565887622018943937, 33.08196800326374643, -12.81628187352647608 ) ) ;
#38207 = EDGE_CURVE ( 'NONE', #27291, #39290, #41034, .T. ) ;
#38208 = CARTESIAN_POINT ( 'NONE',  ( 0.6081133539230532126, 38.33703382326400089, 6.499999999999970690 ) ) ;
#38209 = CARTESIAN_POINT ( 'NONE',  ( 0.2751277870542874204, 39.36607318730131055, -6.499999999999984901 ) ) ;
#38210 = ORIENTED_EDGE ( 'NONE', *, *, #9970, .F. ) ;
#38211 = VECTOR ( 'NONE', #31913, 999.9999999999998863 ) ;
#38212 = CARTESIAN_POINT ( 'NONE',  ( 17.20831665107776587, 64.13393115100079456, -7.208316651077762316 ) ) ;
#38213 = CARTESIAN_POINT ( 'NONE',  ( -11.42891328973558451, 14.99999999999803002, -9.126250717934663470 ) ) ;
#38214 = CARTESIAN_POINT ( 'NONE',  ( 1.472469842513823179, 35.59226448433412315, -4.923371831947296329 ) ) ;
#38215 = CARTESIAN_POINT ( 'NONE',  ( -0.3689425029237898834, 36.17874883491396787, -10.36894250292378850 ) ) ;
#38216 = CARTESIAN_POINT ( 'NONE',  ( 5.076628168052704559, 55.17559781766745175, -8.527530157486179263 ) ) ;
#38217 = CARTESIAN_POINT ( 'NONE',  ( -9.282040431732752950, 15.00000000000000888, 11.30407325590330103 ) ) ;
#38218 = CARTESIAN_POINT ( 'NONE',  ( 18.52753015748617571, 8.092264484334117824, 4.923371831947298993 ) ) ;
#38219 = CARTESIAN_POINT ( 'NONE',  ( -0.3689425029237898834, 1.178748834913967869, -10.36894250292378850 ) ) ;
#38220 = CARTESIAN_POINT ( 'NONE',  ( 1.472469842513823179, 50.59226448433411605, -4.923371831947296329 ) ) ;
#38221 = CARTESIAN_POINT ( 'NONE',  ( -0.8801773607111008646, 58.27201867748816966, 2.915334737309923430 ) ) ;
#38222 = CARTESIAN_POINT ( 'NONE',  ( 18.52753015748618282, 43.92559781766745175, -4.923371831947291888 ) ) ;
#38223 = DIRECTION ( 'NONE',  ( -0.2503800040544323924, 0.000000000000000000, -0.9681476403781101858 ) ) ;
#38224 = CARTESIAN_POINT ( 'NONE',  ( 2.035157376598822676, 42.43868534415483396, -7.964842623401177768 ) ) ;
#38225 = VERTEX_POINT ( 'NONE', #73000 ) ;
#38226 = CARTESIAN_POINT ( 'NONE',  ( -0.1503990784575277573, 63.10158574516643171, 6.262539305110076171 ) ) ;
#38227 = CARTESIAN_POINT ( 'NONE',  ( 15.44008868035555793, 26.39701867748817321, -9.422509992056140149 ) ) ;
#38229 = CARTESIAN_POINT ( 'NONE',  ( -0.8801773607111008646, 58.27201867748816966, 2.915334737309923430 ) ) ;
#38228 = CARTESIAN_POINT ( 'NONE',  ( -1.099225684535947600, -1.293031996736246469, -6.408140936763238038 ) ) ;
#38230 = CARTESIAN_POINT ( 'NONE',  ( -0.1503990784575247319, 47.22266099184918886, -6.262539305110083276 ) ) ;
#38231 = CARTESIAN_POINT ( 'NONE',  ( -7.618303901328673078, -3.182726299308032341E-15, 12.48478900416256288 ) ) ;
#38233 = LINE ( 'NONE', #44228, #4131 ) ;
#38232 = CARTESIAN_POINT ( 'NONE',  ( 12.91533473730992121, 44.52201867748816966, 10.88017736071110164 ) ) ;
#38234 = CARTESIAN_POINT ( 'NONE',  ( 7.361572987183169658, 14.96726448433411960, -9.846743663894592657 ) ) ;
#38235 = CARTESIAN_POINT ( 'NONE',  ( 5.076628168052703671, 41.84226448433411605, 8.527530157486179263 ) ) ;
#38236 = DIRECTION ( 'NONE',  ( -1.000000000000000000, 0.000000000000000000, 0.000000000000000000 ) ) ;
#38237 = CARTESIAN_POINT ( 'NONE',  ( 7.082119434687054849, 18.47041550158062861, 12.26659068614894288 ) ) ;
#38238 = CARTESIAN_POINT ( 'NONE',  ( 21.09922568453595559, 2.040301336597086568, -6.408140936763230044 ) ) ;
#38239 = CARTESIAN_POINT ( 'NONE',  ( -0.3689425029237898834, 61.17874883491396076, -10.36894250292378850 ) ) ;
#38240 = CARTESIAN_POINT ( 'NONE',  ( 0.000000000000000000, 0.5000000000000004441, 0.000000000000000000 ) ) ;
#38241 = CARTESIAN_POINT ( 'NONE',  ( -4.164238869374099927, 27.01208216824730357, 3.795296366450308767 ) ) ;
#38242 = EDGE_CURVE ( 'NONE', #29326, #52526, #24158, .T. ) ;
#38243 = CARTESIAN_POINT ( 'NONE',  ( 6.204703633549690345, 55.76208216824730357, -14.16423886937410259 ) ) ;
#38244 = CARTESIAN_POINT ( 'NONE',  ( 14.92337183194729988, 19.34226448433411960, -8.527530157486177487 ) ) ;
#38245 = CARTESIAN_POINT ( 'NONE',  ( 10.00000000000000178, 4.313685344154837509, 10.88017736071110342 ) ) ;
#38246 = ORIENTED_EDGE ( 'NONE', *, *, #68592, .T. ) ;
#38247 = CARTESIAN_POINT ( 'NONE',  ( 10.00000000000000000, 29.75893115100078745, -9.846743663894594434 ) ) ;
#38248 = CARTESIAN_POINT ( 'NONE',  ( 2.035157376598824452, 33.68868534415484106, 7.964842623401179544 ) ) ;
#38249 = CARTESIAN_POINT ( 'NONE',  ( 14.92337183194729988, 54.34226448433412315, -8.527530157486177487 ) ) ;
#38250 = CARTESIAN_POINT ( 'NONE',  ( -2.266590686148945544, 2.220415501580634388, 7.082119434687048631 ) ) ;
#38251 = FACE_OUTER_BOUND ( 'NONE', #81420, .T. ) ;
#38252 = CARTESIAN_POINT ( 'NONE',  ( 10.00000000000000178, 17.25893115100078745, 9.846743663894594434 ) ) ;
#38253 = CARTESIAN_POINT ( 'NONE',  ( -2.816281873526471635, 38.91530133659708213, -3.434112377981056508 ) ) ;
#38254 = CARTESIAN_POINT ( 'NONE',  ( 0.1532563361054100626, 45.80059781766745886, -2.638427012816831230 ) ) ;
#38255 = ORIENTED_EDGE ( 'NONE', *, *, #70369, .F. ) ;
#38256 = CARTESIAN_POINT ( 'NONE',  ( 18.52753015748617571, 28.09226448433411960, 4.923371831947298993 ) ) ;
#38257 = CARTESIAN_POINT ( 'NONE',  ( 10.83696084481538691, -98.17058944465519232, -3.750000000000000000 ) ) ;
#38258 = LINE ( 'NONE', #21273, #79391 ) ;
#38259 = AXIS2_PLACEMENT_3D ( 'NONE', #93123, #18616, #40138 ) ;
#38260 = CARTESIAN_POINT ( 'NONE',  ( -4.164238869374099039, 56.80374883491397497, 8.674139862899312516E-16 ) ) ;
#38261 = CARTESIAN_POINT ( 'NONE',  ( 4.559911319644449179, 52.23035201082151247, -9.422509992056141925 ) ) ;
#38262 = CARTESIAN_POINT ( 'NONE',  ( 0.1077916266722474814, 32.24062864464239198, -6.478736007405950126 ) ) ;
#38263 = CARTESIAN_POINT ( 'NONE',  ( 14.92337183194729988, 39.34226448433412315, -8.527530157486177487 ) ) ;
#38264 = CARTESIAN_POINT ( 'NONE',  ( 0.5774900079438607392, 8.480352010821505360, 5.440088680355550821 ) ) ;
#38265 = CARTESIAN_POINT ( 'NONE',  ( 1.472469842513823179, 45.59226448433412315, -4.923371831947296329 ) ) ;
#38266 = CARTESIAN_POINT ( 'NONE',  ( 5.817157072110704874, 0.5000000000000004441, 13.82608706751090821 ) ) ;
#38267 = CARTESIAN_POINT ( 'NONE',  ( 0.1532563361054082862, 46.21726448433411605, 2.638427012816831674 ) ) ;
#38268 = AXIS2_PLACEMENT_3D ( 'NONE', #58032, #53993, #38022 ) ;
#38269 = CARTESIAN_POINT ( 'NONE',  ( 7.084665262690076126, 52.02201867748816255, -10.88017736071110164 ) ) ;
#38270 =( BOUNDED_CURVE ( )  B_SPLINE_CURVE ( 2, ( #18899, #2930, #33377, #63873, #70920, #25902, #47898, #11383, #56404 ),
 .UNSPECIFIED., .F., .F. ) 
 B_SPLINE_CURVE_WITH_KNOTS ( ( 3, 2, 2, 2, 3 ),
 ( 0.08200037436403688484, 0.08333333333333332871, 0.08928571428571428770, 0.09523809523809523281, 0.09657105420739148238 ),
 .UNSPECIFIED. ) 
 CURVE ( )  GEOMETRIC_REPRESENTATION_ITEM ( )  RATIONAL_B_SPLINE_CURVE ( ( 0.9881565478350731180, 0.9923695281211489805, 1.000000000000000000, 0.9659258262890683122, 1.000000000000000000, 0.9659258262890683122, 1.000000000000000000, 0.9923695281211499797, 0.9881565478350742282 ) ) 
 REPRESENTATION_ITEM ( '' )  );
#38271 = VERTEX_POINT ( 'NONE', #11033 ) ;
#38272 = ORIENTED_EDGE ( 'NONE', *, *, #7405, .F. ) ;
#38273 = CARTESIAN_POINT ( 'NONE',  ( -14.48718990079892954, 4.238615592650390652E-16, 0.6093675230839495915 ) ) ;
#38274 = CARTESIAN_POINT ( 'NONE',  ( 3.014428414850127691, 6.463468844518203582, -11.25000000000000000 ) ) ;
#38275 = CARTESIAN_POINT ( 'NONE',  ( 7.361572987183170547, 12.05059781766744997, 9.846743663894590881 ) ) ;
#38276 = CARTESIAN_POINT ( 'NONE',  ( 22.81628187352648496, 51.83196800326376064, -3.434112377981050290 ) ) ;
#38278 = CARTESIAN_POINT ( 'NONE',  ( 10.00000000000000178, 47.25893115100078745, 9.846743663894594434 ) ) ;
#38277 = CARTESIAN_POINT ( 'NONE',  ( 20.88017736071110519, 10.56368534415483929, 2.639326808657452039E-16 ) ) ;
#38279 = FACE_OUTER_BOUND ( 'NONE', #20777, .T. ) ;
#38280 = CARTESIAN_POINT ( 'NONE',  ( -0.3689425029237881626, 27.42874883491397142, 10.36894250292379027 ) ) ;
#38281 = CARTESIAN_POINT ( 'NONE',  ( -2.266590686148945544, 56.38708216824731068, -7.082119434687050408 ) ) ;
#38282 = CARTESIAN_POINT ( 'NONE',  ( 2.791683348922240793, 61.63393115100079456, 7.208316651077764092 ) ) ;
#38283 =( NAMED_UNIT ( * ) PLANE_ANGLE_UNIT ( ) SI_UNIT ( $, .RADIAN. ) );
#38284 = CARTESIAN_POINT ( 'NONE',  ( 19.42250999205614548, 55.98035201082150536, -5.440088680355545492 ) ) ;
#38285 = CARTESIAN_POINT ( 'NONE',  ( 2.035157376598824452, 68.68868534415484817, 7.964842623401179544 ) ) ;
#38286 = CARTESIAN_POINT ( 'NONE',  ( -3.500000000000000444, 1.019547802438453887, 3.750000000000000000 ) ) ;
#38287 = ORIENTED_EDGE ( 'NONE', *, *, #65694, .F. ) ;
#38288 = CARTESIAN_POINT ( 'NONE',  ( 22.81628187352647785, 61.62363466993041783, 6.195893100308588602E-16 ) ) ;
#38289 = ORIENTED_EDGE ( 'NONE', *, *, #72108, .T. ) ;
#38290 = CARTESIAN_POINT ( 'NONE',  ( 14.92337183194729988, 4.342264484334117824, -8.527530157486177487 ) ) ;
#38291 = VERTEX_POINT ( 'NONE', #94525 ) ;
#38292 = CARTESIAN_POINT ( 'NONE',  ( 10.00000000000000178, 18.05374883491396787, 14.16423886937410082 ) ) ;
#38293 = CARTESIAN_POINT ( 'NONE',  ( 1.472469842513823179, 20.59226448433411960, -4.923371831947296329 ) ) ;
#38294 = CARTESIAN_POINT ( 'NONE',  ( 10.00000000000000000, 31.81368534415483751, -10.88017736071110342 ) ) ;
#38295 = VECTOR ( 'NONE', #46355, 1000.000000000000000 ) ;
#38296 = CARTESIAN_POINT ( 'NONE',  ( 3.843478602184544624, 14.76930270348881535, -14.43834224996323101 ) ) ;
#38297 = VERTEX_POINT ( 'NONE', #93541 ) ;
#38298 = CARTESIAN_POINT ( 'NONE',  ( 15.44008868035555793, 31.39701867748817676, -9.422509992056140149 ) ) ;
#38299 = EDGE_CURVE ( 'NONE', #24437, #44141, #25073, .T. ) ;
#38300 = EDGE_CURVE ( 'NONE', #70551, #243, #92129, .T. ) ;
#38301 = ORIENTED_EDGE ( 'NONE', *, *, #67956, .T. ) ;
#38302 = CARTESIAN_POINT ( 'NONE',  ( 20.88017736071110164, 40.35535201082150536, 2.915334737309930979 ) ) ;
#38303 = CARTESIAN_POINT ( 'NONE',  ( 19.89103541497709315, 55.66234555792568983, -6.479102184480829862 ) ) ;
#38304 = VERTEX_POINT ( 'NONE', #41555 ) ;
#38305 = CARTESIAN_POINT ( 'NONE',  ( 21.09922568453594849, 21.20696800326375353, 6.408140936763242479 ) ) ;
#38306 = CARTESIAN_POINT ( 'NONE',  ( 1.821158202401629067, 21.16688879859529138, 6.499999999999990230 ) ) ;
#38307 = CARTESIAN_POINT ( 'NONE',  ( 0.1532563361054083140, 11.00893115100078568, 1.131784320476157264E-15 ) ) ;
#38308 = FILL_AREA_STYLE ('',( #7813 ) ) ;
#38309 = CARTESIAN_POINT ( 'NONE',  ( 0.1532563361054082862, 21.21726448433412315, 2.638427012816831674 ) ) ;
#38310 = CARTESIAN_POINT ( 'NONE',  ( 10.00000000000000000, 26.81368534415484106, -10.88017736071110342 ) ) ;
#38311 = ORIENTED_EDGE ( 'NONE', *, *, #2317, .T. ) ;
#38312 = VERTEX_POINT ( 'NONE', #72019 ) ;
#38313 = DIRECTION ( 'NONE',  ( 1.000000000000000000, 0.000000000000000000, 0.000000000000000000 ) ) ;
#38314 = CARTESIAN_POINT ( 'NONE',  ( 2.035157376598824452, 53.68868534415484817, 7.964842623401179544 ) ) ;
#38315 = CARTESIAN_POINT ( 'NONE',  ( 2.603489959281584998, 6.582109641433292246, 6.499999999999998224 ) ) ;
#38316 = CARTESIAN_POINT ( 'NONE',  ( 16.40814093676324603, 52.45696800326375353, -11.09922568453594671 ) ) ;
#38317 = CARTESIAN_POINT ( 'NONE',  ( -0.8801773607111009756, 58.06368534415484106, 1.068504757029289695E-15 ) ) ;
#38318 = CARTESIAN_POINT ( 'NONE',  ( 12.63842701281683922, 64.55059781766745175, -9.846743663894590881 ) ) ;
#38319 = EDGE_CURVE ( 'NONE', #27398, #58242, #53800, .T. ) ;
#38320 = CARTESIAN_POINT ( 'NONE',  ( -6.382347221874242749, 15.00000000000000000, -13.57444820018235987 ) ) ;
#38321 = AXIS2_PLACEMENT_3D ( 'NONE', #94111, #24650, #33594 ) ;
#38322 = CARTESIAN_POINT ( 'NONE',  ( 14.92337183194729633, 37.67559781766745175, 8.527530157486181039 ) ) ;
#38323 = CARTESIAN_POINT ( 'NONE',  ( 22.81628187352647785, 51.41530133659708923, 3.434112377981063169 ) ) ;
#38324 = DIRECTION ( 'NONE',  ( -0.000000000000000000, -0.000000000000000000, -1.000000000000000000 ) ) ;
#38325 = CARTESIAN_POINT ( 'NONE',  ( 14.92337183194729633, 12.67559781766745353, 8.527530157486181039 ) ) ;
#38326 = CARTESIAN_POINT ( 'NONE',  ( -1.099225684535947600, 14.54030133659708568, 6.408140936763237150 ) ) ;
#38328 = DIRECTION ( 'NONE',  ( 0.000000000000000000, 0.000000000000000000, 1.000000000000000000 ) ) ;
#38327 = LINE ( 'NONE', #97855, #83570 ) ;
#38329 = CARTESIAN_POINT ( 'NONE',  ( 10.00000000000000178, 39.31368534415484106, 10.88017736071110342 ) ) ;
#38330 = COLOUR_RGB ( '', 0.08235294, 0.09019608, 0.10196078) ;
#38331 = CARTESIAN_POINT ( 'NONE',  ( 1.472469842513823179, 61.42559781766745175, 4.923371831947296329 ) ) ;
#38332 = CARTESIAN_POINT ( 'NONE',  ( -2.621477372531479055, 15.00000000000000000, -15.77990027919564575 ) ) ;
#38333 = VECTOR ( 'NONE', #87465, 1000.000000000000000 ) ;
#38334 = CARTESIAN_POINT ( 'NONE',  ( 17.20831665107776587, 19.13393115100078035, -7.208316651077762316 ) ) ;
#38335 = CARTESIAN_POINT ( 'NONE',  ( 12.63842701281683034, 2.467264484334118269, 9.846743663894596210 ) ) ;
#38336 = CARTESIAN_POINT ( 'NONE',  ( 12.91533473730993009, 16.60535201082150891, -10.88017736071109987 ) ) ;
#38337 = CARTESIAN_POINT ( 'NONE',  ( -1.099225684535947600, 19.54030133659708568, 6.408140936763237150 ) ) ;
#38338 = CARTESIAN_POINT ( 'NONE',  ( 12.63842701281683034, 57.46726448433411605, 9.846743663894596210 ) ) ;
#38339 = CARTESIAN_POINT ( 'NONE',  ( 4.130000001237588592, 0.09091675484614469838, -2.500000000000000000 ) ) ;
#38340 = CARTESIAN_POINT ( 'NONE',  ( 19.42250999205614548, 10.98035201082150536, -5.440088680355545492 ) ) ;
#38341 = CARTESIAN_POINT ( 'NONE',  ( 2.791683348922240793, 46.63393115100077324, 7.208316651077764092 ) ) ;
#38342 = ORIENTED_EDGE ( 'NONE', *, *, #29792, .F. ) ;
#38343 = CARTESIAN_POINT ( 'NONE',  ( 4.441302488725760611, -2.692589364095749005, 2.750000000000000888 ) ) ;
#38344 = CARTESIAN_POINT ( 'NONE',  ( 10.00000000000000000, 6.813685344154838397, -10.88017736071110342 ) ) ;
#38345 = CARTESIAN_POINT ( 'NONE',  ( -25.69000000000001194, 93.50000000000000000, 9.500000000000000000 ) ) ;
#38346 = CARTESIAN_POINT ( 'NONE',  ( 7.084665262690076126, 27.02201867748817676, -10.88017736071110164 ) ) ;
#38348 = DIRECTION ( 'NONE',  ( 0.7716245833877105609, 0.000000000000000000, 0.6360782202777752747 ) ) ;
#38347 = CARTESIAN_POINT ( 'NONE',  ( 24.16423886937410614, 64.51208216824728936, -3.795296366450302550 ) ) ;
#38349 = CARTESIAN_POINT ( 'NONE',  ( 0.1532563361054100626, 0.8005978176674514168, -2.638427012816831230 ) ) ;
#38350 = AXIS2_PLACEMENT_3D ( 'NONE', #80265, #72266, #43244 ) ;
#38351 = CARTESIAN_POINT ( 'NONE',  ( 1.472469842513823179, 21.42559781766745175, 4.923371831947296329 ) ) ;
#38352 = CARTESIAN_POINT ( 'NONE',  ( 19.38216949554541202, 10.99863466993042138, 9.382169495545424454 ) ) ;
#38353 = CARTESIAN_POINT ( 'NONE',  ( -46.94000000000001194, 103.0000000000000000, 5.997726559847112782 ) ) ;
#38354 = CARTESIAN_POINT ( 'NONE',  ( 67.06412365047464164, 14.00000000000001243, 9.500000000000000000 ) ) ;
#38355 = CARTESIAN_POINT ( 'NONE',  ( 10.00000000000000000, -2.126365330069579951, -12.81628187352647608 ) ) ;
#38356 = DIRECTION ( 'NONE',  ( -0.000000000000000000, -1.000000000000000000, -0.000000000000000000 ) ) ;
#38357 = EDGE_CURVE ( 'NONE', #68676, #64082, #7523, .T. ) ;
#38358 = CARTESIAN_POINT ( 'NONE',  ( -2.266590686148945544, 17.22041550158063572, 7.082119434687048631 ) ) ;
#38359 = CARTESIAN_POINT ( 'NONE',  ( 18.52753015748617571, 28.09226448433411960, 4.923371831947298993 ) ) ;
#38360 = CARTESIAN_POINT ( 'NONE',  ( 20.36894250292379738, 54.92874883491396076, -10.36894250292379027 ) ) ;
#38361 = CARTESIAN_POINT ( 'NONE',  ( 7.361572987183170547, 12.05059781766744997, 9.846743663894590881 ) ) ;
#38362 = CARTESIAN_POINT ( 'NONE',  ( -13.30119215211272810, 14.76984893004878785, -6.804450086557387145 ) ) ;
#38363 = CARTESIAN_POINT ( 'NONE',  ( 4.559911319644449179, 27.23035201082150536, -9.422509992056141925 ) ) ;
#38364 = CARTESIAN_POINT ( 'NONE',  ( 6.565887622018943937, 50.16530133659708213, 12.81628187352647430 ) ) ;
#38365 = CARTESIAN_POINT ( 'NONE',  ( 7.084665262690076126, 22.02201867748817321, -10.88017736071110164 ) ) ;
#38366 = CARTESIAN_POINT ( 'NONE',  ( 10.00000000000000178, 45.37363466993041783, 12.81628187352647608 ) ) ;
#38367 = CARTESIAN_POINT ( 'NONE',  ( 1.472469842513823179, 66.42559781766745175, 4.923371831947296329 ) ) ;
#38368 = ORIENTED_EDGE ( 'NONE', *, *, #27143, .T. ) ;
#38369 = CARTESIAN_POINT ( 'NONE',  ( -2.999999999999999556, 23.03999999999999915, 0.000000000000000000 ) ) ;
#38370 = CARTESIAN_POINT ( 'NONE',  ( 10.00000000000000000, 35.55374883491396787, -14.16423886937410082 ) ) ;
#38371 = CARTESIAN_POINT ( 'NONE',  ( -2.266590686148945544, 12.22041550158063394, 7.082119434687048631 ) ) ;
#38372 = CARTESIAN_POINT ( 'NONE',  ( -0.8801773607111009756, 8.063685344154837509, 1.068504757029289695E-15 ) ) ;
#38373 = CARTESIAN_POINT ( 'NONE',  ( 7.084665262690076126, 39.10535201082150536, 10.88017736071109987 ) ) ;
#38374 = CARTESIAN_POINT ( 'NONE',  ( 18.72515096720572458, 40.05509018479936145, 6.499999999999964473 ) ) ;
#38375 = CARTESIAN_POINT ( 'NONE',  ( 14.91886229468041947, 0.2301503527634121971, -0.8060919667644429465 ) ) ;
#38376 = CARTESIAN_POINT ( 'NONE',  ( 17.96484262340118221, 64.93868534415483396, 7.964842623401181321 ) ) ;
#38377 = CARTESIAN_POINT ( 'NONE',  ( 0.5774900079438607392, 68.48035201082150536, 5.440088680355550821 ) ) ;
#38378 = CARTESIAN_POINT ( 'NONE',  ( 21.09922568453594849, 31.20696800326375353, 6.408140936763242479 ) ) ;
#38379 = LINE ( 'NONE', #70354, #89009 ) ;
#38380 = CARTESIAN_POINT ( 'NONE',  ( -5.888281321711915872, 1.823139558123406223, -10.37198838585826266 ) ) ;
#38381 = CARTESIAN_POINT ( 'NONE',  ( 5.076628168052704559, 40.17559781766745175, -8.527530157486179263 ) ) ;
#38382 = ADVANCED_FACE ( 'NONE', ( #35499 ), #36236, .T. ) ;
#38383 = CARTESIAN_POINT ( 'NONE',  ( -0.8801773607111009756, 18.06368534415484106, 1.068504757029289695E-15 ) ) ;
#38384 = AXIS2_PLACEMENT_3D ( 'NONE', #10224, #73154, #40713 ) ;
#38385 = CARTESIAN_POINT ( 'NONE',  ( 3.591859063236763294, 13.29030133659708746, -11.09922568453595026 ) ) ;
#38386 = CARTESIAN_POINT ( 'NONE',  ( 1.472469842513823179, 11.42559781766745175, 4.923371831947296329 ) ) ;
#38387 = CARTESIAN_POINT ( 'NONE',  ( 15.44008868035555793, 11.39701867748817143, -9.422509992056140149 ) ) ;
#38388 = CARTESIAN_POINT ( 'NONE',  ( 14.92337183194729633, 37.67559781766745175, 8.527530157486181039 ) ) ;
#38389 = CARTESIAN_POINT ( 'NONE',  ( 21.09922568453594849, 61.20696800326376064, 6.408140936763242479 ) ) ;
#38391 = CARTESIAN_POINT ( 'NONE',  ( 10.00000000000000000, 0.5537488349139675359, -14.16423886937410082 ) ) ;
#38390 = CARTESIAN_POINT ( 'NONE',  ( 7.361572987183170547, 37.05059781766744464, 9.846743663894590881 ) ) ;
#38392 = CARTESIAN_POINT ( 'NONE',  ( 13.79529636645030344, 18.26208216824730002, 14.16423886937410614 ) ) ;
#38393 = VECTOR ( 'NONE', #61957, 1000.000000000000000 ) ;
#38394 = CARTESIAN_POINT ( 'NONE',  ( 7.084665262690076126, 29.10535201082150181, 10.88017736071109987 ) ) ;
#38396 = CARTESIAN_POINT ( 'NONE',  ( 24.16423886937409904, 39.09541550158062506, 3.795296366450317205 ) ) ;
#38395 = CARTESIAN_POINT ( 'NONE',  ( 4.559911319644449179, 8.897018677488171434, 9.422509992056141925 ) ) ;
#38397 = CARTESIAN_POINT ( 'NONE',  ( 10.00000000000000000, 36.81368534415484106, -10.88017736071110342 ) ) ;
#38398 = CARTESIAN_POINT ( 'NONE',  ( 20.88017736071110519, 15.56368534415483751, 2.639326808657452039E-16 ) ) ;
#38399 = VERTEX_POINT ( 'NONE', #66493 ) ;
#38400 = ADVANCED_FACE ( 'NONE', ( #90462 ), #12992, .T. ) ;
#38401 = AXIS2_PLACEMENT_3D ( 'NONE', #4008, #5486, #28465 ) ;
#38402 = CARTESIAN_POINT ( 'NONE',  ( 19.42250999205614548, 45.98035201082150536, -5.440088680355545492 ) ) ;
#38403 = CARTESIAN_POINT ( 'NONE',  ( 21.09922568453595559, 62.04030133659709634, -6.408140936763230044 ) ) ;
#38404 = CARTESIAN_POINT ( 'NONE',  ( 15.44008868035555793, 41.39701867748817676, -9.422509992056140149 ) ) ;
#38405 = CARTESIAN_POINT ( 'NONE',  ( 7.084665262690076126, 52.02201867748816255, -10.88017736071110164 ) ) ;
#38406 = ORIENTED_EDGE ( 'NONE', *, *, #95242, .F. ) ;
#38408 = ADVANCED_FACE ( 'NONE', ( #28975 ), #61776, .T. ) ;
#38407 = CARTESIAN_POINT ( 'NONE',  ( 10.00000000000000178, 44.31368534415484106, 10.88017736071110342 ) ) ;
#38409 =( LENGTH_UNIT ( ) NAMED_UNIT ( * ) SI_UNIT ( .MILLI., .METRE. ) );
#38410 = CARTESIAN_POINT ( 'NONE',  ( 14.04867373755350890, 15.00000000000000000, 7.649324326489743697 ) ) ;
#38411 = CARTESIAN_POINT ( 'NONE',  ( 10.00000000000000000, 50.55374883491396787, -14.16423886937410082 ) ) ;
#38412 = CARTESIAN_POINT ( 'NONE',  ( 1.472469842513823179, 0.5922644843341181575, -4.923371831947296329 ) ) ;
#38413 = CARTESIAN_POINT ( 'NONE',  ( -14.09397099617995508, 14.95037102751076752, 4.360881834954074776 ) ) ;
#38414 = ADVANCED_FACE ( 'NONE', ( #21998 ), #75472, .T. ) ;
#38415 = FILL_AREA_STYLE ('',( #8886 ) ) ;
#38416 = CARTESIAN_POINT ( 'NONE',  ( 17.20831665107776587, 62.88393115100078745, 7.208316651077764980 ) ) ;
#38417 = CARTESIAN_POINT ( 'NONE',  ( -14.16722289976679505, 0.3640475087720985159, -4.928467845925709412 ) ) ;
#38418 = CARTESIAN_POINT ( 'NONE',  ( 17.20831665107776587, 37.88393115100078745, 7.208316651077764980 ) ) ;
#38419 = ORIENTED_EDGE ( 'NONE', *, *, #26094, .F. ) ;
#38420 = CARTESIAN_POINT ( 'NONE',  ( 19.84674366389459621, 33.50893115100078745, 7.409399052514197653E-17 ) ) ;
#38421 = AXIS2_PLACEMENT_3D ( 'NONE', #30592, #1116, #48055 ) ;
#38422 = CARTESIAN_POINT ( 'NONE',  ( 2.035157376598824452, 43.68868534415484106, 7.964842623401179544 ) ) ;
#38423 = CARTESIAN_POINT ( 'NONE',  ( 19.84674366389459621, 33.50893115100078745, 7.409399052514197653E-17 ) ) ;
#38424 = CARTESIAN_POINT ( 'NONE',  ( 3.591859063236761518, 19.95696800326375353, 11.09922568453594849 ) ) ;
#38426 = CARTESIAN_POINT ( 'NONE',  ( 0.5774900079438607392, 53.48035201082151247, 5.440088680355550821 ) ) ;
#38425 = DIRECTION ( 'NONE',  ( 0.000000000000000000, 0.000000000000000000, -1.000000000000000000 ) ) ;
#38427 = CARTESIAN_POINT ( 'NONE',  ( 19.42250999205614548, 45.98035201082150536, -5.440088680355545492 ) ) ;
#38428 = CARTESIAN_POINT ( 'NONE',  ( 6.204703633549690345, 60.76208216824730357, -14.16423886937410259 ) ) ;
#38429 = AXIS2_PLACEMENT_3D ( 'NONE', #19623, #50617, #81108 ) ;
#38430 = CARTESIAN_POINT ( 'NONE',  ( 13.43411237798106583, 17.66530133659708923, -12.81628187352647252 ) ) ;
#38431 = FACE_OUTER_BOUND ( 'NONE', #36420, .T. ) ;
#38432 = ORIENTED_EDGE ( 'NONE', *, *, #44531, .T. ) ;
#38433 = CARTESIAN_POINT ( 'NONE',  ( 22.81628187352647785, 16.62363466993042138, 6.195893100308588602E-16 ) ) ;
#38434 = CARTESIAN_POINT ( 'NONE',  ( 20.88017736071110875, 15.77201867748817143, -2.915334737309920765 ) ) ;
#38435 = CARTESIAN_POINT ( 'NONE',  ( 10.00000000000000000, 56.81368534415484106, -10.88017736071110342 ) ) ;
#38437 = ORIENTED_EDGE ( 'NONE', *, *, #36889, .F. ) ;
#38436 = EDGE_CURVE ( 'NONE', #21745, #70649, #20249, .T. ) ;
#38438 = CARTESIAN_POINT ( 'NONE',  ( -12.07856007377833407, 3.961594683405543780E-16, 8.022367888854752493 ) ) ;
#38439 = CARTESIAN_POINT ( 'NONE',  ( 20.88017736071110519, 65.56368534415483396, 2.639326808657452039E-16 ) ) ;
#38440 = CARTESIAN_POINT ( 'NONE',  ( 17.20831665107776587, 54.13393115100079456, -7.208316651077762316 ) ) ;
#38441 = CARTESIAN_POINT ( 'NONE',  ( 2.791683348922237240, 40.38393115100078035, -7.208316651077763204 ) ) ;
#38442 = CARTESIAN_POINT ( 'NONE',  ( 19.84674366389459266, 23.71726448433412315, -2.638427012816827677 ) ) ;
#38443 = CARTESIAN_POINT ( 'NONE',  ( -0.1023957841222409432, 40.13377557478296609, 6.340343622311920058 ) ) ;
#38445 = CARTESIAN_POINT ( 'NONE',  ( 10.00000000000000000, 37.87363466993041783, -12.81628187352647608 ) ) ;
#38444 = CARTESIAN_POINT ( 'NONE',  ( 1.915564264621439472, 15.00000000000000000, -14.37291249357988043 ) ) ;
#38447 = DIRECTION ( 'NONE',  ( 0.000000000000000000, 0.000000000000000000, 1.000000000000000000 ) ) ;
#38446 = CARTESIAN_POINT ( 'NONE',  ( 7.361572987183169658, 9.967264484334119601, -9.846743663894592657 ) ) ;
#38448 = CARTESIAN_POINT ( 'NONE',  ( 14.94699059465101776, 15.00000000000000000, -1.259949270174818059 ) ) ;
#38450 = ORIENTED_EDGE ( 'NONE', *, *, #11246, .T. ) ;
#38449 = CARTESIAN_POINT ( 'NONE',  ( 7.361572987183170547, 47.05059781766745175, 9.846743663894590881 ) ) ;
#38451 = COLOUR_RGB ( '', 0.40784314, 0.44705882, 0.49803922) ;
#38452 = CARTESIAN_POINT ( 'NONE',  ( 11.62719953690064933, 14.49999999999999822, -9.476720473301794456 ) ) ;
#38453 = B_SPLINE_CURVE_WITH_KNOTS ( 'NONE', 3,
 ( #46696, #63653, #33644, #17695, #71183, #8700 ),
 .UNSPECIFIED., .F., .F.,
 ( 4, 2, 4 ),
 ( 0.000000000000000000, 0.0002565770811490921863, 0.0005131541622981843727 ),
 .UNSPECIFIED. ) ;
#38454 = CARTESIAN_POINT ( 'NONE',  ( 6.565887622018943937, 13.08196800326374998, -12.81628187352647608 ) ) ;
#38455 = CARTESIAN_POINT ( 'NONE',  ( -0.8801773607110991993, 52.85535201082151247, -2.915334737309923874 ) ) ;
#38456 = CARTESIAN_POINT ( 'NONE',  ( 2.917880565312950480, 35.97041550158063217, -12.26659068614894821 ) ) ;
#38457 = B_SPLINE_CURVE_WITH_KNOTS ( 'NONE', 3,
 ( #4129, #43095, #36086, #58586, #43584, #50104 ),
 .UNSPECIFIED., .F., .F.,
 ( 4, 2, 4 ),
 ( 0.0002800170536516692881, 0.0006862224498868429523, 0.001092427846122016617 ),
 .UNSPECIFIED. ) ;
#38458 = TOROIDAL_SURFACE ( 'NONE', #67212, 11.15000000000026326, 0.2500000000000000000 ) ;
#38459 = FACE_OUTER_BOUND ( 'NONE', #78717, .T. ) ;
#38460 = CARTESIAN_POINT ( 'NONE',  ( 2.917880565312948704, 27.63708216824730357, 12.26659068614894643 ) ) ;
#38461 = VECTOR ( 'NONE', #30490, 1000.000000000000000 ) ;
#38462 = CARTESIAN_POINT ( 'NONE',  ( 10.00000000000000000, 60.55374883491397497, -14.16423886937410082 ) ) ;
#38463 = CARTESIAN_POINT ( 'NONE',  ( 17.08211943468705840, 10.13708216824730179, -12.26659068614894466 ) ) ;
#38465 = CARTESIAN_POINT ( 'NONE',  ( -6.767445849361066301, 15.00000000000000000, -13.38662304974505801 ) ) ;
#38464 = CARTESIAN_POINT ( 'NONE',  ( -0.3689425029237898834, 31.17874883491396787, -10.36894250292378850 ) ) ;
#38466 = CARTESIAN_POINT ( 'NONE',  ( 15.44008868035555260, 64.73035201082151957, 9.422509992056143702 ) ) ;
#38467 = CARTESIAN_POINT ( 'NONE',  ( 20.10493008474206178, 24.71697413083879624, 6.336235997365763595 ) ) ;
#38470 = AXIS2_PLACEMENT_3D ( 'NONE', #21194, #49699, #97216 ) ;
#38469 = CARTESIAN_POINT ( 'NONE',  ( 17.20831665107776587, 37.88393115100078745, 7.208316651077764980 ) ) ;
#38468 = CARTESIAN_POINT ( 'NONE',  ( -3.193136578977206597, 2.219226321806266888E-16, 14.27383009353652454 ) ) ;
#38471 = CARTESIAN_POINT ( 'NONE',  ( 4.559911319644449179, 22.23035201082150536, -9.422509992056141925 ) ) ;
#38472 = CARTESIAN_POINT ( 'NONE',  ( 17.39651004071838969, 44.08210964143329846, -6.500000000000027534 ) ) ;
#38473 = CARTESIAN_POINT ( 'NONE',  ( 0.1532563361054082862, 66.21726448433413736, 2.638427012816831674 ) ) ;
#38474 = CARTESIAN_POINT ( 'NONE',  ( 20.00000000000000711, 85.76239730488823909, -5.246947360776204050 ) ) ;
#38475 = CARTESIAN_POINT ( 'NONE',  ( 14.92337183194729633, 37.67559781766745175, 8.527530157486181039 ) ) ;
#38476 = CARTESIAN_POINT ( 'NONE',  ( 13.43411237798105340, 60.58196800326376064, 12.81628187352647963 ) ) ;
#38477 = CARTESIAN_POINT ( 'NONE',  ( -12.26659068614895354, -3.612917831752694653, -7.082119434687038861 ) ) ;
#38478 = CARTESIAN_POINT ( 'NONE',  ( 10.00000000000000178, 42.25893115100078745, 9.846743663894594434 ) ) ;
#38479 = CARTESIAN_POINT ( 'NONE',  ( 17.20831665107776587, 54.13393115100079456, -7.208316651077762316 ) ) ;
#38480 = CARTESIAN_POINT ( 'NONE',  ( 22.26659068614895176, 39.72041550158063217, -7.082119434687042414 ) ) ;
#38481 = ORIENTED_EDGE ( 'NONE', *, *, #29842, .T. ) ;
#38482 = CARTESIAN_POINT ( 'NONE',  ( 13.79529636645031943, 20.34541550158063572, -14.16423886937409904 ) ) ;
#38483 = CARTESIAN_POINT ( 'NONE',  ( 0.5774900079438590739, 57.64701867748817676, -5.440088680355550821 ) ) ;
#38484 = DIRECTION ( 'NONE',  ( 0.000000000000000000, -1.000000000000000000, 0.000000000000000000 ) ) ;
#38485 = CARTESIAN_POINT ( 'NONE',  ( -0.3689425029237881626, 57.42874883491397497, 10.36894250292379027 ) ) ;
#38486 = CARTESIAN_POINT ( 'NONE',  ( 21.09922568453594849, 16.20696800326375353, 6.408140936763242479 ) ) ;
#38487 = CARTESIAN_POINT ( 'NONE',  ( 0.000000000000000000, 15.00000000000000000, 0.000000000000000000 ) ) ;
#38488 = CARTESIAN_POINT ( 'NONE',  ( 7.084665262690076126, 62.02201867748816966, -10.88017736071110164 ) ) ;
#38489 = DIRECTION ( 'NONE',  ( 0.000000000000000000, -1.000000000000000000, 0.000000000000000000 ) ) ;
#38490 = CARTESIAN_POINT ( 'NONE',  ( -46.94000000000000483, 100.7316555907688809, -8.991040189367279112 ) ) ;
#38491 = CARTESIAN_POINT ( 'NONE',  ( -4.164238869374098151, 56.59541550158063927, -3.795296366450310543 ) ) ;
#38492 = CARTESIAN_POINT ( 'NONE',  ( 4.559911319644449179, 32.23035201082150536, -9.422509992056141925 ) ) ;
#38493 = CARTESIAN_POINT ( 'NONE',  ( 0.5774900079438607392, 28.48035201082150891, 5.440088680355550821 ) ) ;
#38494 = CARTESIAN_POINT ( 'NONE',  ( 0.1532563361054083140, 51.00893115100078745, 1.131784320476157264E-15 ) ) ;
#38495 = CARTESIAN_POINT ( 'NONE',  ( 19.84674366389459621, 48.50893115100078745, 7.409399052514197653E-17 ) ) ;
#38496 = CARTESIAN_POINT ( 'NONE',  ( -1.099225684535947600, 53.70696800326376064, -6.408140936763238038 ) ) ;
#38497 = ORIENTED_EDGE ( 'NONE', *, *, #92478, .F. ) ;
#38498 = VECTOR ( 'NONE', #33047, 1000.000000000000000 ) ;
#38499 = ADVANCED_FACE ( 'NONE', ( #21003 ), #56997, .T. ) ;
#38500 = CARTESIAN_POINT ( 'NONE',  ( 10.00000000000000178, 19.31368534415484106, 10.88017736071110342 ) ) ;
#38501 = CARTESIAN_POINT ( 'NONE',  ( 21.09922568453595559, 17.04030133659708923, -6.408140936763230044 ) ) ;
#38502 = CARTESIAN_POINT ( 'NONE',  ( -13.59943737456463708, 14.95077488074852390, 5.718514076972763149 ) ) ;
#38503 = CARTESIAN_POINT ( 'NONE',  ( 14.92337183194729633, 47.67559781766745175, 8.527530157486181039 ) ) ;
#38504 = CARTESIAN_POINT ( 'NONE',  ( 2.035157376598824452, 48.68868534415483396, 7.964842623401179544 ) ) ;
#38505 = CARTESIAN_POINT ( 'NONE',  ( 10.00000000000000000, 22.87363466993042138, -12.81628187352647608 ) ) ;
#38507 = CARTESIAN_POINT ( 'NONE',  ( 13.34343830728406743, 0.3639313252796093079, -6.852200678592626382 ) ) ;
#38506 = CARTESIAN_POINT ( 'NONE',  ( 7.084665262690076126, 44.10535201082151247, 10.88017736071109987 ) ) ;
#38508 = SURFACE_SIDE_STYLE ('',( #68018 ) ) ;
#38509 = CARTESIAN_POINT ( 'NONE',  ( -1.099225684535947600, 53.70696800326376064, -6.408140936763238038 ) ) ;
#38510 = ORIENTED_EDGE ( 'NONE', *, *, #427, .T. ) ;
#38511 = CARTESIAN_POINT ( 'NONE',  ( 14.43100913236849614, 4.781026887021415124E-16, 1.412789942453260839 ) ) ;
#38512 = CARTESIAN_POINT ( 'NONE',  ( 15.44008868035555260, 44.73035201082151247, 9.422509992056143702 ) ) ;
#38514 = CARTESIAN_POINT ( 'NONE',  ( 22.26659068614895176, 19.72041550158063572, -7.082119434687042414 ) ) ;
#38513 = CARTESIAN_POINT ( 'NONE',  ( 6.565887622018943937, 50.16530133659708213, 12.81628187352647430 ) ) ;
#38515 = CARTESIAN_POINT ( 'NONE',  ( 19.84674366389459266, 8.300597817667451750, 2.638427012816836559 ) ) ;
#38516 = CARTESIAN_POINT ( 'NONE',  ( 0.1532563361054083140, 61.00893115100078745, 1.131784320476157264E-15 ) ) ;
#38517 = CARTESIAN_POINT ( 'NONE',  ( 18.52753015748618282, 33.92559781766745886, -4.923371831947291888 ) ) ;
#38518 = CARTESIAN_POINT ( 'NONE',  ( 5.076628168052704559, 10.17559781766745175, -8.527530157486179263 ) ) ;
#38519 = CARTESIAN_POINT ( 'NONE',  ( -0.3329122712635644854, 0.000000000000000000, -5.443067521379392204 ) ) ;
#38520 = CARTESIAN_POINT ( 'NONE',  ( -4.164238869374098151, 46.59541550158063927, -3.795296366450310543 ) ) ;
#38521 = VECTOR ( 'NONE', #67222, 1000.000000000000000 ) ;
#38522 = DIRECTION ( 'NONE',  ( 0.000000000000000000, 1.000000000000000000, 0.000000000000000000 ) ) ;
#38523 = CARTESIAN_POINT ( 'NONE',  ( 15.44008868035555260, 4.730352010821504471, 9.422509992056143702 ) ) ;
#38524 = CARTESIAN_POINT ( 'NONE',  ( -6.031993939728319987, -39.82530731229964971, -4.000000000000000000 ) ) ;
#38525 = AXIS2_PLACEMENT_3D ( 'NONE', #44811, #45316, #98847 ) ;
#38526 = VERTEX_POINT ( 'NONE', #50506 ) ;
#38527 = CARTESIAN_POINT ( 'NONE',  ( -0.8801773607110991993, 12.85535201082150358, -2.915334737309923874 ) ) ;
#38529 = ADVANCED_FACE ( 'NONE', ( #43006 ), #74564, .T. ) ;
#38528 = CARTESIAN_POINT ( 'NONE',  ( 17.96484262340118221, 11.18868534415484106, -7.964842623401177768 ) ) ;
#38530 = CARTESIAN_POINT ( 'NONE',  ( 10.00000000000000178, 42.25893115100078745, 9.846743663894594434 ) ) ;
#38531 = CARTESIAN_POINT ( 'NONE',  ( 21.09922568453595559, 42.04030133659708213, -6.408140936763230044 ) ) ;
#38533 = CARTESIAN_POINT ( 'NONE',  ( -4.164238869374099927, 12.01208216824730357, 3.795296366450308767 ) ) ;
#38532 = CARTESIAN_POINT ( 'NONE',  ( -8.000343251535921851, 84.06932101904432386, -3.750000000000000000 ) ) ;
#38534 = CARTESIAN_POINT ( 'NONE',  ( 0.5774900079438590739, 32.64701867748816966, -5.440088680355550821 ) ) ;
#38535 = CARTESIAN_POINT ( 'NONE',  ( 0.5774900079438607392, 3.480352010821504916, 5.440088680355550821 ) ) ;
#38536 = CARTESIAN_POINT ( 'NONE',  ( 10.00000000000000178, 42.25893115100078745, 9.846743663894594434 ) ) ;
#38537 = ADVANCED_FACE ( 'NONE', ( #81986 ), #54464, .T. ) ;
#38538 = FILL_AREA_STYLE ('',( #55506 ) ) ;
#38539 = CARTESIAN_POINT ( 'NONE',  ( 5.076628168052703671, 26.84226448433411960, 8.527530157486179263 ) ) ;
#38540 = TOROIDAL_SURFACE ( 'NONE', #16186, 14.49999999999999822, 0.5000000000000000000 ) ;
#38541 = CARTESIAN_POINT ( 'NONE',  ( -0.8801773607110990882, 32.85535201082150536, -2.915334737309924318 ) ) ;
#38542 = CARTESIAN_POINT ( 'NONE',  ( -11.09922568453595382, -41.29303199673624647, -6.408140936763226492 ) ) ;
#38543 = ORIENTED_EDGE ( 'NONE', *, *, #82290, .T. ) ;
#38544 = TOROIDAL_SURFACE ( 'NONE', #1874, 14.49999999999999822, 0.5000000000000000000 ) ;
#38545 = VERTEX_POINT ( 'NONE', #89979 ) ;
#38546 = CARTESIAN_POINT ( 'NONE',  ( 19.84674366389459266, 53.30059781766744464, 2.638427012816836559 ) ) ;
#38548 = CARTESIAN_POINT ( 'NONE',  ( 2.035157376598822676, 32.43868534415483396, -7.964842623401177768 ) ) ;
#38547 = CARTESIAN_POINT ( 'NONE',  ( 17.96484262340118221, 34.93868534415482685, 7.964842623401181321 ) ) ;
#38550 = CARTESIAN_POINT ( 'NONE',  ( -2.816281873526471635, 28.91530133659708213, -3.434112377981056508 ) ) ;
#38549 = CARTESIAN_POINT ( 'NONE',  ( 0.5774900079438590739, 2.647018677488170990, -5.440088680355550821 ) ) ;
#38551 = CARTESIAN_POINT ( 'NONE',  ( 13.79529636645030344, 18.26208216824730002, 14.16423886937410614 ) ) ;
#38552 = B_SPLINE_CURVE_WITH_KNOTS ( 'NONE', 3,
 ( #27381, #11896, #26392, #86425, #3911, #57387 ),
 .UNSPECIFIED., .F., .F.,
 ( 4, 2, 4 ),
 ( 0.0002800518438628012163, 0.0006862575805706620877, 0.001092463317278523013 ),
 .UNSPECIFIED. ) ;
#38553 = CARTESIAN_POINT ( 'NONE',  ( 19.38216949554541557, 47.24863466993041783, -9.382169495545420901 ) ) ;
#38554 = ORIENTED_EDGE ( 'NONE', *, *, #41817, .T. ) ;
#38555 = CARTESIAN_POINT ( 'NONE',  ( 14.92337183194729988, 44.34226448433412315, -8.527530157486177487 ) ) ;
#38556 = CARTESIAN_POINT ( 'NONE',  ( 20.88017736071110519, 25.56368534415483751, 2.639326808657452039E-16 ) ) ;
#38557 = VERTEX_POINT ( 'NONE', #15487 ) ;
#38558 = CARTESIAN_POINT ( 'NONE',  ( 4.559911319644449179, 13.89701867748817321, 9.422509992056141925 ) ) ;
#38559 = ORIENTED_EDGE ( 'NONE', *, *, #90955, .T. ) ;
#38560 = CARTESIAN_POINT ( 'NONE',  ( 4.559911319644449179, 57.23035201082150536, -9.422509992056141925 ) ) ;
#38561 = CARTESIAN_POINT ( 'NONE',  ( 7.084665262690076126, 64.10535201082150536, 10.88017736071109987 ) ) ;
#38562 = CARTESIAN_POINT ( 'NONE',  ( 14.92337183194729633, 12.67559781766745353, 8.527530157486181039 ) ) ;
#38563 = CARTESIAN_POINT ( 'NONE',  ( 2.035157376598824452, 48.68868534415483396, 7.964842623401179544 ) ) ;
#38564 = MECHANICAL_DESIGN_GEOMETRIC_PRESENTATION_REPRESENTATION (  '', ( #46543 ), #8231 ) ;
#38565 = LINE ( 'NONE', #78030, #76194 ) ;
#38566 = CARTESIAN_POINT ( 'NONE',  ( 0.1532563361054100626, 10.80059781766745175, -2.638427012816831230 ) ) ;
#38568 = ORIENTED_EDGE ( 'NONE', *, *, #55136, .F. ) ;
#38567 = CARTESIAN_POINT ( 'NONE',  ( -9.399392868737892925, 4.026710370808002065E-16, 11.04089732309467919 ) ) ;
#38569 =( GEOMETRIC_REPRESENTATION_CONTEXT ( 3 ) GLOBAL_UNCERTAINTY_ASSIGNED_CONTEXT ( ( #96288 ) ) GLOBAL_UNIT_ASSIGNED_CONTEXT ( ( #43868, #44372, #6370 ) ) REPRESENTATION_CONTEXT ( 'NONE', 'WORKASPACE' ) );
#38570 = CARTESIAN_POINT ( 'NONE',  ( 1.472469842513823179, 41.42559781766745886, 4.923371831947296329 ) ) ;
#38571 = ORIENTED_EDGE ( 'NONE', *, *, #51544, .F. ) ;
#38572 = FACE_OUTER_BOUND ( 'NONE', #21958, .T. ) ;
#38573 = CARTESIAN_POINT ( 'NONE',  ( 0.000000000000000000, 0.5000000000000000000, -6.500000000000000888 ) ) ;
#38574 = CARTESIAN_POINT ( 'NONE',  ( 13.79529636645030344, 18.26208216824730002, 14.16423886937410614 ) ) ;
#38575 = CARTESIAN_POINT ( 'NONE',  ( -0.3289641300568009741, 7.245456701841137992, -5.963430220938281678 ) ) ;
#38576 = CARTESIAN_POINT ( 'NONE',  ( 19.39235739573468820, 9.875764716086008477, 6.500000000000000000 ) ) ;
#38577 = CARTESIAN_POINT ( 'NONE',  ( 19.42250999205614548, 10.98035201082150536, -5.440088680355545492 ) ) ;
#38578 = SURFACE_STYLE_USAGE ( .BOTH. , #47549 ) ;
#38580 = VERTEX_POINT ( 'NONE', #30453 ) ;
#38579 = CARTESIAN_POINT ( 'NONE',  ( 10.00000000000000178, 40.37363466993042493, 12.81628187352647608 ) ) ;
#38581 = CARTESIAN_POINT ( 'NONE',  ( 19.84674366389459266, 3.300597817667451750, 2.638427012816836559 ) ) ;
#38582 = CARTESIAN_POINT ( 'NONE',  ( 5.076628168052704559, 0.1755978176674514724, -8.527530157486179263 ) ) ;
#38583 = CARTESIAN_POINT ( 'NONE',  ( 21.09922568453595559, 32.04030133659708923, -6.408140936763230044 ) ) ;
#38584 = CARTESIAN_POINT ( 'NONE',  ( 17.20831665107776587, 17.88393115100078745, 7.208316651077764980 ) ) ;
#38585 = CARTESIAN_POINT ( 'NONE',  ( 7.595945211628325922, 15.00000000000000000, -12.35117874301639240 ) ) ;
#38586 = CARTESIAN_POINT ( 'NONE',  ( 17.20831665107776587, 19.13393115100078035, -7.208316651077762316 ) ) ;
#38587 = CARTESIAN_POINT ( 'NONE',  ( 13.43411237798106583, 12.66530133659708746, -12.81628187352647252 ) ) ;
#38588 = CARTESIAN_POINT ( 'NONE',  ( -7.750000000000000000, 83.99999999999994316, -4.000000000000000000 ) ) ;
#38589 = AXIS2_PLACEMENT_3D ( 'NONE', #7637, #90607, #61098 ) ;
#38590 = CARTESIAN_POINT ( 'NONE',  ( 12.63842701281683034, 7.467264484334118713, 9.846743663894596210 ) ) ;
#38591 = ORIENTED_EDGE ( 'NONE', *, *, #23056, .T. ) ;
#38592 = EDGE_LOOP ( 'NONE', ( #33376, #87568, #18017, #24758 ) ) ;
#38593 = CARTESIAN_POINT ( 'NONE',  ( -0.8801773607111008646, 23.27201867748817676, 2.915334737309923430 ) ) ;
#38594 = CARTESIAN_POINT ( 'NONE',  ( 13.79529636645031943, 20.34541550158063572, -14.16423886937409904 ) ) ;
#38595 = CARTESIAN_POINT ( 'NONE',  ( 2.791683348922237240, 40.38393115100078035, -7.208316651077763204 ) ) ;
#38596 = CARTESIAN_POINT ( 'NONE',  ( 7.361572987183170547, 2.050597817667451750, 9.846743663894590881 ) ) ;
#38598 = CARTESIAN_POINT ( 'NONE',  ( -5.812563760649267941, -35.09659463721938977, -2.750000000000000444 ) ) ;
#38597 = CARTESIAN_POINT ( 'NONE',  ( 22.81628187352647785, 46.41530133659708213, 3.434112377981063169 ) ) ;
#38599 = CARTESIAN_POINT ( 'NONE',  ( 20.88017736071110519, 30.56368534415484106, 2.639326808657452039E-16 ) ) ;
#38600 = CARTESIAN_POINT ( 'NONE',  ( -8.924603092375777535, 75.06466731010172566, -3.000000000000000000 ) ) ;
#38601 = CARTESIAN_POINT ( 'NONE',  ( -2.816281873526473856, 14.12363466993041961, 9.499525473075851096E-16 ) ) ;
#38602 = CARTESIAN_POINT ( 'NONE',  ( 0.1532563361054082862, 31.21726448433412315, 2.638427012816831674 ) ) ;
#38603 = CARTESIAN_POINT ( 'NONE',  ( -9.422509992056145478, -17.35298132251182324, -5.440088680355541939 ) ) ;
#38604 = CARTESIAN_POINT ( 'NONE',  ( -1.099225684535947600, 53.70696800326376064, -6.408140936763238038 ) ) ;
#38605 = VECTOR ( 'NONE', #59088, 1000.000000000000000 ) ;
#38607 = FACE_OUTER_BOUND ( 'NONE', #168, .T. ) ;
#38606 = CARTESIAN_POINT ( 'NONE',  ( 0.5774900079438607392, 53.48035201082151247, 5.440088680355550821 ) ) ;
#38608 = EDGE_CURVE ( 'NONE', #43096, #39731, #95685, .T. ) ;
#38609 = CARTESIAN_POINT ( 'NONE',  ( 10.19513985507833276, 15.00000000000000000, -11.00268709613217055 ) ) ;
#38610 = CARTESIAN_POINT ( 'NONE',  ( -0.2078314800230414150, 14.95037105884406792, 14.75174957775970519 ) ) ;
#38611 = CARTESIAN_POINT ( 'NONE',  ( 0.5774900079438590739, 37.64701867748817676, -5.440088680355550821 ) ) ;
#38612 = CARTESIAN_POINT ( 'NONE',  ( 12.91533473730992121, 49.52201867748817676, 10.88017736071110164 ) ) ;
#38613 = CARTESIAN_POINT ( 'NONE',  ( 17.20831665107776587, 64.13393115100079456, -7.208316651077762316 ) ) ;
#38614 = CARTESIAN_POINT ( 'NONE',  ( 17.96484262340118221, 64.93868534415483396, 7.964842623401181321 ) ) ;
#38615 = CARTESIAN_POINT ( 'NONE',  ( 2.791683348922240793, 51.63393115100078745, 7.208316651077764092 ) ) ;
#38617 = CARTESIAN_POINT ( 'NONE',  ( 0.000000000000000000, 14.49999999999999822, 0.000000000000000000 ) ) ;
#38616 = CARTESIAN_POINT ( 'NONE',  ( 10.00000000000000000, 11.81368534415483751, -10.88017736071110342 ) ) ;
#38618 = CARTESIAN_POINT ( 'NONE',  ( -2.816281873526473856, 9.331968003263753531, 3.434112377981055619 ) ) ;
#38619 = EDGE_LOOP ( 'NONE', ( #57763, #29662, #8173, #35596 ) ) ;
#38620 = CARTESIAN_POINT ( 'NONE',  ( 0.5774900079438590739, 37.64701867748817676, -5.440088680355550821 ) ) ;
#38622 = LINE ( 'NONE', #92110, #66957 ) ;
#38621 = CARTESIAN_POINT ( 'NONE',  ( -2.816281873526471635, 3.915301336597087456, -3.434112377981056508 ) ) ;
#38623 = CARTESIAN_POINT ( 'NONE',  ( -0.8801773607111008646, 13.27201867748817143, 2.915334737309923430 ) ) ;
#38624 = CARTESIAN_POINT ( 'NONE',  ( -0.8801773607110991993, 22.85535201082150181, -2.915334737309923874 ) ) ;
#38625 = CARTESIAN_POINT ( 'NONE',  ( 20.36894250292379382, 38.67874883491396076, 10.36894250292379205 ) ) ;
#38626 = CARTESIAN_POINT ( 'NONE',  ( 19.84674366389459266, 33.71726448433410894, -2.638427012816827677 ) ) ;
#38627 = CARTESIAN_POINT ( 'NONE',  ( 15.44008868035555793, 46.39701867748817676, -9.422509992056140149 ) ) ;
#38628 =( LENGTH_UNIT ( ) NAMED_UNIT ( * ) SI_UNIT ( .MILLI., .METRE. ) );
#38629 = CARTESIAN_POINT ( 'NONE',  ( -0.3689425029237881626, 7.428748834913967869, 10.36894250292379027 ) ) ;
#38630 = SURFACE_STYLE_FILL_AREA ( #31603 ) ;
#38631 = CARTESIAN_POINT ( 'NONE',  ( 17.20831665107776587, 59.13393115100078745, -7.208316651077762316 ) ) ;
#38632 = ORIENTED_EDGE ( 'NONE', *, *, #8576, .F. ) ;
#38633 = VERTEX_POINT ( 'NONE', #30947 ) ;
#38634 = CIRCLE ( 'NONE', #22724, 14.49999999999999822 ) ;
#38635 = CARTESIAN_POINT ( 'NONE',  ( 17.08211943468705840, 30.13708216824730357, -12.26659068614894466 ) ) ;
#38637 = EDGE_CURVE ( 'NONE', #95614, #50302, #54435, .T. ) ;
#38636 = CARTESIAN_POINT ( 'NONE',  ( -4.164238869374099039, 31.80374883491396432, 8.674139862899312516E-16 ) ) ;
#38638 = CARTESIAN_POINT ( 'NONE',  ( 1.472469842513823179, 6.425597817667451750, 4.923371831947296329 ) ) ;
#38639 = CARTESIAN_POINT ( 'NONE',  ( 19.84674366389459266, 63.71726448433412315, -2.638427012816827677 ) ) ;
#38640 = CARTESIAN_POINT ( 'NONE',  ( -11.30179204363884082, -57.06033576789361206, 4.000000000000000000 ) ) ;
#38642 = CARTESIAN_POINT ( 'NONE',  ( 16.40814093676323893, 15.79030133659708746, 11.09922568453595026 ) ) ;
#38641 = CARTESIAN_POINT ( 'NONE',  ( 20.88017736071110164, 65.35535201082150536, 2.915334737309930979 ) ) ;
#38643 = CARTESIAN_POINT ( 'NONE',  ( -4.164238869374099927, 32.01208216824730357, 3.795296366450308767 ) ) ;
#38644 = CARTESIAN_POINT ( 'NONE',  ( 7.084665262690076126, 19.10535201082150181, 10.88017736071109987 ) ) ;
#38645 = CARTESIAN_POINT ( 'NONE',  ( 20.88017736071110519, 30.56368534415484106, 2.639326808657452039E-16 ) ) ;
#38646 = DIRECTION ( 'NONE',  ( 0.000000000000000000, 0.000000000000000000, -1.000000000000000000 ) ) ;
#38647 = CARTESIAN_POINT ( 'NONE',  ( 7.084665262690076126, 59.10535201082150536, 10.88017736071109987 ) ) ;
#38648 = CARTESIAN_POINT ( 'NONE',  ( 8.527530157486175710, -11.07440218233254114, -4.923371831947298993 ) ) ;
#38649 = ORIENTED_EDGE ( 'NONE', *, *, #77886, .F. ) ;
#38650 = FILL_AREA_STYLE ('',( #8158 ) ) ;
#38651 = ORIENTED_EDGE ( 'NONE', *, *, #41920, .F. ) ;
#38652 = CARTESIAN_POINT ( 'NONE',  ( -1.926860441876564023, 12.87045670184114066, 3.195792623639529761 ) ) ;
#38653 = ORIENTED_EDGE ( 'NONE', *, *, #97234, .T. ) ;
#38654 = CARTESIAN_POINT ( 'NONE',  ( 5.200846386093622264, 0.000000000000000000, 1.639820566680979308 ) ) ;
#38656 = CARTESIAN_POINT ( 'NONE',  ( 22.26659068614895176, 64.72041550158064638, -7.082119434687042414 ) ) ;
#38655 = CARTESIAN_POINT ( 'NONE',  ( 6.204703633549690345, 55.76208216824730357, -14.16423886937410259 ) ) ;
#38658 = CARTESIAN_POINT ( 'NONE',  ( 2.791683348922240793, 56.63393115100078035, 7.208316651077764092 ) ) ;
#38657 = CARTESIAN_POINT ( 'NONE',  ( 5.076628168052704559, 20.17559781766745175, -8.527530157486179263 ) ) ;
#38659 = SURFACE_STYLE_USAGE ( .BOTH. , #16154 ) ;
#38660 = CARTESIAN_POINT ( 'NONE',  ( 3.469446951953614189E-15, 11.36803362898265135, 11.25000000000000178 ) ) ;
#38661 = CARTESIAN_POINT ( 'NONE',  ( 18.52753015748618282, 8.925597817667451750, -4.923371831947291888 ) ) ;
#38662 = MECHANICAL_DESIGN_GEOMETRIC_PRESENTATION_REPRESENTATION (  '', ( #97775 ), #27504 ) ;
#38663 = CARTESIAN_POINT ( 'NONE',  ( 19.38216949554541202, 0.9986346699304200492, 9.382169495545424454 ) ) ;
#38664 = CARTESIAN_POINT ( 'NONE',  ( 9.382169495545419124, 15.99863466993042493, 9.382169495545417348 ) ) ;
#38665 = ORIENTED_EDGE ( 'NONE', *, *, #40774, .T. ) ;
#38666 = CIRCLE ( 'NONE', #94537, 10.65000000000000036 ) ;
#38667 = CARTESIAN_POINT ( 'NONE',  ( 6.204703633549690345, 30.76208216824730357, -14.16423886937410259 ) ) ;
#38668 = ORIENTED_EDGE ( 'NONE', *, *, #93804, .T. ) ;
#38669 = CIRCLE ( 'NONE', #8331, 0.7500000000000006661 ) ;
#38670 = CARTESIAN_POINT ( 'NONE',  ( 13.79529636645030344, 48.26208216824728936, 14.16423886937410614 ) ) ;
#38671 = ORIENTED_EDGE ( 'NONE', *, *, #75522, .T. ) ;
#38672 = CARTESIAN_POINT ( 'NONE',  ( 22.81628187352647785, 56.41530133659708213, 3.434112377981063169 ) ) ;
#38673 = EDGE_CURVE ( 'NONE', #18498, #69579, #91217, .T. ) ;
#38674 = B_SPLINE_CURVE_WITH_KNOTS ( 'NONE', 3,
 ( #79384, #10890, #94871, #56870, #87373, #18888 ),
 .UNSPECIFIED., .F., .F.,
 ( 4, 2, 4 ),
 ( 3.409110551496121881E-05, 0.0004400426677367870595, 0.0008459942299586128934 ),
 .UNSPECIFIED. ) ;
#38675 = CARTESIAN_POINT ( 'NONE',  ( 5.076628168052704559, 50.17559781766745886, -8.527530157486179263 ) ) ;
#38676 = CARTESIAN_POINT ( 'NONE',  ( 0.5774900079438607392, 23.48035201082150536, 5.440088680355550821 ) ) ;
#38677 = AXIS2_PLACEMENT_3D ( 'NONE', #81996, #15004, #74491 ) ;
#38678 = CARTESIAN_POINT ( 'NONE',  ( -6.787878914541003006, -86.25326249609904039, 2.499999999999999556 ) ) ;
#38679 = CARTESIAN_POINT ( 'NONE',  ( 18.52753015748617571, 53.09226448433412315, 4.923371831947298993 ) ) ;
#38680 = CARTESIAN_POINT ( 'NONE',  ( 10.00000000000000000, 54.75893115100078745, -9.846743663894594434 ) ) ;
#38681 = EDGE_CURVE ( 'NONE', #48202, #35666, #48115, .T. ) ;
#38682 = DIRECTION ( 'NONE',  ( 0.000000000000000000, 0.000000000000000000, -1.000000000000000000 ) ) ;
#38683 = CARTESIAN_POINT ( 'NONE',  ( -14.82269085861165792, 0.5000000000000004441, -2.299529454047158250 ) ) ;
#38684 = CARTESIAN_POINT ( 'NONE',  ( 5.076628168052703671, 6.842264484334118713, 8.527530157486179263 ) ) ;
#38685 = FACE_OUTER_BOUND ( 'NONE', #6080, .T. ) ;
#38686 = ORIENTED_EDGE ( 'NONE', *, *, #85357, .F. ) ;
#38687 = B_SPLINE_SURFACE_WITH_KNOTS ( 'NONE', 3, 1, ( 
 ( #18699, #41702 ),
 ( #80168, #42189 ),
 ( #43154, #35149 ),
 ( #18207, #26673 ),
 ( #95672, #11680 ),
 ( #4686, #73641 ),
 ( #26193, #65649 ),
 ( #72653, #50160 ),
 ( #96172, #95166 ),
 ( #27159, #94185 ),
 ( #3701, #4188 ),
 ( #88651, #34658 ),
 ( #86702, #3207 ),
 ( #34161, #19178 ),
 ( #57167, #87664 ),
 ( #79684, #87177 ),
 ( #58142, #33670 ),
 ( #64653, #48687 ) ),
 .UNSPECIFIED., .F., .F., .F.,
 ( 4, 2, 2, 2, 2, 2, 2, 2, 4 ),
 ( 2, 2 ),
 ( 0.1401766717507622606, 0.2499999999999989453, 0.3749999999999986122, 0.4374999999999986677, 0.4999999999999986677, 0.7499999999999992228, 0.8749999999999996669, 0.9374999999999997780, 1.000000000000000000 ),
 ( 0.000000000000000000, 1.000000000000000000 ),
 .UNSPECIFIED. ) ;
#38688 = CARTESIAN_POINT ( 'NONE',  ( 8.880000000000000782, -0.01162444801151916833, 3.750000000006731060 ) ) ;
#38689 = CARTESIAN_POINT ( 'NONE',  ( 14.92337183194729988, 34.34226448433411605, -8.527530157486177487 ) ) ;
#38690 = PLANE ( 'NONE',  #94746 ) ;
#38691 = CARTESIAN_POINT ( 'NONE',  ( 19.38216949554541557, 42.24863466993041783, -9.382169495545420901 ) ) ;
#38692 = DIRECTION ( 'NONE',  ( -0.8526401643540884034, 0.000000000000000000, -0.5224985647159551272 ) ) ;
#38693 = ORIENTED_EDGE ( 'NONE', *, *, #67304, .F. ) ;
#38694 = FACE_OUTER_BOUND ( 'NONE', #13458, .T. ) ;
#38695 = CARTESIAN_POINT ( 'NONE',  ( 0.000000000000000000, 14.49999999999999822, 0.000000000000000000 ) ) ;
#38696 = CARTESIAN_POINT ( 'NONE',  ( 12.63842701281683922, 54.55059781766745175, -9.846743663894590881 ) ) ;
#38697 = CARTESIAN_POINT ( 'NONE',  ( 10.00000000000000000, 35.55374883491396787, -14.16423886937410082 ) ) ;
#38698 = CARTESIAN_POINT ( 'NONE',  ( 19.84674366389459621, 58.50893115100078745, 7.409399052514197653E-17 ) ) ;
#38699 = CARTESIAN_POINT ( 'NONE',  ( -9.322910753578032228, 14.95077488074853456, 11.43369735623869765 ) ) ;
#38700 = CARTESIAN_POINT ( 'NONE',  ( 7.361572987183169658, 24.96726448433412315, -9.846743663894592657 ) ) ;
#38701 = CARTESIAN_POINT ( 'NONE',  ( 0.6178305044545818747, 48.49863466993042493, -9.382169495545419124 ) ) ;
#38702 = CARTESIAN_POINT ( 'NONE',  ( 17.08211943468705130, 3.470415501580634388, 12.26659068614894998 ) ) ;
#38703 = CARTESIAN_POINT ( 'NONE',  ( 14.92337183194729633, 57.67559781766745886, 8.527530157486181039 ) ) ;
#38704 = CARTESIAN_POINT ( 'NONE',  ( 17.96484262340118221, 51.18868534415483396, -7.964842623401177768 ) ) ;
#38705 = CARTESIAN_POINT ( 'NONE',  ( 12.63842701281683034, 42.46726448433412315, 9.846743663894596210 ) ) ;
#38706 = CARTESIAN_POINT ( 'NONE',  ( -5.963430220938290560, 6.828790035174475470, -10.32896413005679648 ) ) ;
#38707 = EDGE_LOOP ( 'NONE', ( #25529, #19329, #33237, #71807 ) ) ;
#38708 = CARTESIAN_POINT ( 'NONE',  ( 10.00000000000000178, 59.31368534415484106, 10.88017736071110342 ) ) ;
#38709 = ORIENTED_EDGE ( 'NONE', *, *, #15078, .F. ) ;
#38710 = CARTESIAN_POINT ( 'NONE',  ( 6.767445849361153343, 0.5000000000000004441, 13.38662304974501360 ) ) ;
#38711 = CARTESIAN_POINT ( 'NONE',  ( -0.8801773607110991993, 27.85535201082150181, -2.915334737309923874 ) ) ;
#38713 = CARTESIAN_POINT ( 'NONE',  ( -0.8801773607111009756, 58.06368534415484106, 1.068504757029289695E-15 ) ) ;
#38712 = CARTESIAN_POINT ( 'NONE',  ( 19.38216949554541557, 2.248634669930420049, -9.382169495545420901 ) ) ;
#38714 = CARTESIAN_POINT ( 'NONE',  ( 9.879999999999990123, 20.99999999999999645, 0.000000000000000000 ) ) ;
#38715 = CARTESIAN_POINT ( 'NONE',  ( 19.72487221294570858, 10.71833443783938655, -6.500000000000000888 ) ) ;
#38716 = FACE_OUTER_BOUND ( 'NONE', #41168, .T. ) ;
#38718 = DIRECTION ( 'NONE',  ( -0.000000000000000000, -0.000000000000000000, -1.000000000000000000 ) ) ;
#38717 = CARTESIAN_POINT ( 'NONE',  ( 0.5774900079438607392, 43.48035201082151247, 5.440088680355550821 ) ) ;
#38719 = CARTESIAN_POINT ( 'NONE',  ( 1.472469842513823179, 31.42559781766745530, 4.923371831947296329 ) ) ;
#38720 = SURFACE_STYLE_USAGE ( .BOTH. , #31198 ) ;
#38721 = CARTESIAN_POINT ( 'NONE',  ( 12.26659068614894821, 18.88708216824730357, 7.082119434687044190 ) ) ;
#38722 = CARTESIAN_POINT ( 'NONE',  ( 5.076628168052703671, 61.84226448433412315, 8.527530157486179263 ) ) ;
#38723 = CARTESIAN_POINT ( 'NONE',  ( 15.44008868035555260, 19.73035201082150536, 9.422509992056143702 ) ) ;
#38724 = CARTESIAN_POINT ( 'NONE',  ( 19.88565890683628368, 27.71691075486304001, -6.480892540919854561 ) ) ;
#38725 = CARTESIAN_POINT ( 'NONE',  ( 20.36894250292379382, 23.67874883491397142, 10.36894250292379205 ) ) ;
#38726 = EDGE_CURVE ( 'NONE', #587, #28267, #50331, .T. ) ;
#38727 = CARTESIAN_POINT ( 'NONE',  ( 13.79529636645031943, 60.34541550158063927, -14.16423886937409904 ) ) ;
#38728 = CARTESIAN_POINT ( 'NONE',  ( 17.20831665107776587, 34.13393115100078745, -7.208316651077762316 ) ) ;
#38729 = CARTESIAN_POINT ( 'NONE',  ( 5.076628168052703671, 11.84226448433411960, 8.527530157486179263 ) ) ;
#38730 = CARTESIAN_POINT ( 'NONE',  ( 2.035157376598824452, 3.688685344154837953, 7.964842623401179544 ) ) ;
#38731 = ORIENTED_EDGE ( 'NONE', *, *, #76887, .F. ) ;
#38732 = CARTESIAN_POINT ( 'NONE',  ( 19.84674366389459266, 23.71726448433412315, -2.638427012816827677 ) ) ;
#38733 = CARTESIAN_POINT ( 'NONE',  ( 15.44008868035555260, 24.73035201082150891, 9.422509992056143702 ) ) ;
#38734 = CARTESIAN_POINT ( 'NONE',  ( 7.361572987183170547, 57.05059781766744464, 9.846743663894590881 ) ) ;
#38736 = LINE ( 'NONE', #84727, #53514 ) ;
#38735 = CARTESIAN_POINT ( 'NONE',  ( 13.79529636645030344, 3.262082168247301350, 14.16423886937410614 ) ) ;
#38737 = CARTESIAN_POINT ( 'NONE',  ( -11.42891328973231069, -3.194161244095965395E-15, 9.126250717928300560 ) ) ;
#38738 = VECTOR ( 'NONE', #39794, 1000.000000000000000 ) ;
#38739 =( GEOMETRIC_REPRESENTATION_CONTEXT ( 3 ) GLOBAL_UNCERTAINTY_ASSIGNED_CONTEXT ( ( #51284 ) ) GLOBAL_UNIT_ASSIGNED_CONTEXT ( ( #1583, #1088, #8570 ) ) REPRESENTATION_CONTEXT ( 'NONE', 'WORKASPACE' ) );
#38740 = CARTESIAN_POINT ( 'NONE',  ( 17.20831665107776587, 9.133931151000787452, -7.208316651077762316 ) ) ;
#38741 = CARTESIAN_POINT ( 'NONE',  ( -2.816281873526473856, 44.33196800326375353, 3.434112377981055619 ) ) ;
#38742 = CARTESIAN_POINT ( 'NONE',  ( 5.076628168052704559, 35.17559781766745175, -8.527530157486179263 ) ) ;
#38743 = ORIENTED_EDGE ( 'NONE', *, *, #61633, .T. ) ;
#38744 = CARTESIAN_POINT ( 'NONE',  ( 19.84674366389459621, 18.50893115100078745, 7.409399052514197653E-17 ) ) ;
#38745 = TOROIDAL_SURFACE ( 'NONE', #94612, 14.49999999999999822, 0.5000000000000000000 ) ;
#38746 = CARTESIAN_POINT ( 'NONE',  ( 11.04808542157948992, -95.57857389791176672, -3.750000000000000000 ) ) ;
#38747 = CARTESIAN_POINT ( 'NONE',  ( 10.00000000000000178, 53.05374883491396787, 14.16423886937410082 ) ) ;
#38748 = CARTESIAN_POINT ( 'NONE',  ( 7.084665262690076126, 54.10535201082151247, 10.88017736071109987 ) ) ;
#38749 = CARTESIAN_POINT ( 'NONE',  ( 0.000000000000000000, 15.00000000000000000, 0.000000000000000000 ) ) ;
#38750 = CARTESIAN_POINT ( 'NONE',  ( 5.076628168052703671, 41.84226448433411605, 8.527530157486179263 ) ) ;
#38751 = CARTESIAN_POINT ( 'NONE',  ( 20.88017736071110519, 10.56368534415483751, 2.639326808657452039E-16 ) ) ;
#38752 = AXIS2_PLACEMENT_3D ( 'NONE', #36261, #73755, #95786 ) ;
#38753 = FILL_AREA_STYLE_COLOUR ( '', #32001 ) ;
#38754 = CARTESIAN_POINT ( 'NONE',  ( 19.84674366389459266, 53.71726448433411605, -2.638427012816827677 ) ) ;
#38755 = CARTESIAN_POINT ( 'NONE',  ( 10.00000000000000000, 46.81368534415484106, -10.88017736071110342 ) ) ;
#38756 = CARTESIAN_POINT ( 'NONE',  ( 12.63842701281683034, 2.467264484334118269, 9.846743663894596210 ) ) ;
#38757 = AXIS2_PLACEMENT_3D ( 'NONE', #7260, #59249, #98779 ) ;
#38758 = VERTEX_POINT ( 'NONE', #15960 ) ;
#38759 = ORIENTED_EDGE ( 'NONE', *, *, #82536, .T. ) ;
#38760 = CARTESIAN_POINT ( 'NONE',  ( 8.879999999999991900, 76.07179676972447169, -4.250000000000000000 ) ) ;
#38762 = EDGE_CURVE ( 'NONE', #31539, #34814, #14595, .T. ) ;
#38761 = FACE_OUTER_BOUND ( 'NONE', #84397, .T. ) ;
#38763 = CARTESIAN_POINT ( 'NONE',  ( 0.1532563361054100626, 25.80059781766744820, -2.638427012816831230 ) ) ;
#38764 = CARTESIAN_POINT ( 'NONE',  ( -1.099225684535947600, 63.70696800326376774, -6.408140936763238038 ) ) ;
#38766 = CARTESIAN_POINT ( 'NONE',  ( 10.00000000000000000, 44.75893115100078745, -9.846743663894594434 ) ) ;
#38765 = CARTESIAN_POINT ( 'NONE',  ( 15.44008868035555260, 14.73035201082150536, 9.422509992056143702 ) ) ;
#38767 = CARTESIAN_POINT ( 'NONE',  ( 13.79529636645030344, 58.26208216824728936, 14.16423886937410614 ) ) ;
#38768 = CARTESIAN_POINT ( 'NONE',  ( 0.1532563361054083140, 51.00893115100078745, 1.131784320476157264E-15 ) ) ;
#38769 = CARTESIAN_POINT ( 'NONE',  ( 18.00000000000000000, 78.68095262110993815, 3.967704011867259517 ) ) ;
#38770 = CARTESIAN_POINT ( 'NONE',  ( 12.91533473730993009, 51.60535201082149825, -10.88017736071109987 ) ) ;
#38771 = ADVANCED_FACE ( 'NONE', ( #16455 ), #78787, .T. ) ;
#38772 = CARTESIAN_POINT ( 'NONE',  ( 2.791683348922237240, 10.38393115100078390, -7.208316651077763204 ) ) ;
#38773 = AXIS2_PLACEMENT_3D ( 'NONE', #38194, #68681, #82191 ) ;
#38774 = ORIENTED_EDGE ( 'NONE', *, *, #45616, .T. ) ;
#38775 = DIRECTION ( 'NONE',  ( 0.7716245833877106719, 0.000000000000000000, 0.6360782202777751637 ) ) ;
#38776 =( BOUNDED_CURVE ( )  B_SPLINE_CURVE ( 3, ( #26222, #88683, #73672, #89180 ),
 .UNSPECIFIED., .F., .T. ) 
 B_SPLINE_CURVE_WITH_KNOTS ( ( 4, 4 ),
 ( 4.712388980384689674, 6.283185307179586232 ),
 .UNSPECIFIED. ) 
 CURVE ( )  GEOMETRIC_REPRESENTATION_ITEM ( )  RATIONAL_B_SPLINE_CURVE ( ( 1.000000000000000000, 0.8047378541243649375, 0.8047378541243649375, 1.000000000000000000 ) ) 
 REPRESENTATION_ITEM ( '' )  );
#38777 = VERTEX_POINT ( 'NONE', #55433 ) ;
#38778 = CARTESIAN_POINT ( 'NONE',  ( 17.20831665107776587, 7.883931151000784787, 7.208316651077764980 ) ) ;
#38779 = ORIENTED_EDGE ( 'NONE', *, *, #43120, .T. ) ;
#38780 = CARTESIAN_POINT ( 'NONE',  ( 2.917880565312948704, 17.63708216824730357, 12.26659068614894643 ) ) ;
#38781 = CARTESIAN_POINT ( 'NONE',  ( 0.1532563361054082862, 26.21726448433411605, 2.638427012816831674 ) ) ;
#38782 = CARTESIAN_POINT ( 'NONE',  ( 10.00000000000000178, 24.31368534415484106, 10.88017736071110342 ) ) ;
#38783 = ORIENTED_EDGE ( 'NONE', *, *, #62519, .F. ) ;
#38784 = CARTESIAN_POINT ( 'NONE',  ( 10.00000000000000178, 29.31368534415483751, 10.88017736071110342 ) ) ;
#38785 = CIRCLE ( 'NONE', #42000, 0.2500000000000002220 ) ;
#38786 = ORIENTED_EDGE ( 'NONE', *, *, #62767, .T. ) ;
#38787 = CARTESIAN_POINT ( 'NONE',  ( 4.559911319644449179, 37.23035201082150536, -9.422509992056141925 ) ) ;
#38788 = CARTESIAN_POINT ( 'NONE',  ( 2.603489959281590771, 66.58210964143327715, 6.500000000000003553 ) ) ;
#38789 = ORIENTED_EDGE ( 'NONE', *, *, #49339, .T. ) ;
#38790 =( NAMED_UNIT ( * ) SI_UNIT ( $, .STERADIAN. ) SOLID_ANGLE_UNIT ( ) );
#38791 = ORIENTED_EDGE ( 'NONE', *, *, #88589, .T. ) ;
#38792 = CARTESIAN_POINT ( 'NONE',  ( 0.6178305044545838731, 19.74863466993042138, 9.382169495545420901 ) ) ;
#38793 = CARTESIAN_POINT ( 'NONE',  ( 12.63842701281683922, 4.550597817667451750, -9.846743663894590881 ) ) ;
#38794 = CARTESIAN_POINT ( 'NONE',  ( -12.34086200392831678, 15.00000000000000000, 7.124999999999885425 ) ) ;
#38795 = LINE ( 'NONE', #9274, #62280 ) ;
#38796 = CARTESIAN_POINT ( 'NONE',  ( 0.1532563361054100626, 15.80059781766745353, -2.638427012816831230 ) ) ;
#38797 = CARTESIAN_POINT ( 'NONE',  ( 17.96484262340118221, 29.93868534415484106, 7.964842623401181321 ) ) ;
#38798 = EDGE_CURVE ( 'NONE', #61558, #63207, #74234, .T. ) ;
#38799 = PRESENTATION_LAYER_ASSIGNMENT (  '', '', ( #85112 ) ) ;
#38800 = ORIENTED_EDGE ( 'NONE', *, *, #91919, .F. ) ;
#38801 = DIRECTION ( 'NONE',  ( 5.818595309480553908E-17, 1.000000000000000000, -0.000000000000000000 ) ) ;
#38802 = CARTESIAN_POINT ( 'NONE',  ( -0.8801773607111008646, 63.27201867748817676, 2.915334737309923430 ) ) ;
#38803 = CARTESIAN_POINT ( 'NONE',  ( -1.114591949025130369, 3.902037737440774503E-16, 14.45709807627963706 ) ) ;
#38804 = AXIS2_PLACEMENT_3D ( 'NONE', #14116, #7613, #36108 ) ;
#38805 = CARTESIAN_POINT ( 'NONE',  ( 32.26500600480481040, 44.99999999999999289, 0.000000000000000000 ) ) ;
#38806 = CARTESIAN_POINT ( 'NONE',  ( 0.5774900079438607392, 63.48035201082149825, 5.440088680355550821 ) ) ;
#38807 = COLOUR_RGB ( '', 0.72549020, 0.75294118, 0.79215686) ;
#38808 = VECTOR ( 'NONE', #29454, 1000.000000000000000 ) ;
#38809 = CARTESIAN_POINT ( 'NONE',  ( 6.565887622018943937, 5.165301336597086568, 12.81628187352647430 ) ) ;
#38811 = CARTESIAN_POINT ( 'NONE',  ( 10.00000000000000178, 70.00000000000000000, 0.000000000000000000 ) ) ;
#38810 = VECTOR ( 'NONE', #61581, 1000.000000000000000 ) ;
#38812 = CARTESIAN_POINT ( 'NONE',  ( 12.63842701281683922, 34.55059781766745886, -9.846743663894590881 ) ) ;
#38813 = CARTESIAN_POINT ( 'NONE',  ( 0.6178305044545818747, 53.49863466993041072, -9.382169495545419124 ) ) ;
#38814 = CARTESIAN_POINT ( 'NONE',  ( 1.602071938427540809, 37.02224192338639597, -6.500000000000066613 ) ) ;
#38815 = CARTESIAN_POINT ( 'NONE',  ( 2.791683348922237240, 25.38393115100078390, -7.208316651077763204 ) ) ;
#38816 = VECTOR ( 'NONE', #91306, 1000.000000000000000 ) ;
#38817 = CARTESIAN_POINT ( 'NONE',  ( 22.81628187352647785, 16.41530133659708923, 3.434112377981063169 ) ) ;
#38819 = DIRECTION ( 'NONE',  ( 0.000000000000000000, 0.000000000000000000, 1.000000000000000000 ) ) ;
#38818 = CARTESIAN_POINT ( 'NONE',  ( -46.30928139467842897, 104.0823827281712255, 5.529860068218143354 ) ) ;
#38820 = CARTESIAN_POINT ( 'NONE',  ( 17.96484262340118221, 31.18868534415483751, -7.964842623401177768 ) ) ;
#38821 = CARTESIAN_POINT ( 'NONE',  ( 2.791683348922240793, 66.63393115100079456, 7.208316651077764092 ) ) ;
#38822 = CARTESIAN_POINT ( 'NONE',  ( 12.54342190210040187, 0.2301501149690343417, 8.116945096741376986 ) ) ;
#38823 = CARTESIAN_POINT ( 'NONE',  ( 0.1532563361054083140, 26.00893115100078745, 1.131784320476157264E-15 ) ) ;
#38824 = CARTESIAN_POINT ( 'NONE',  ( 0.1532563361054082862, 6.217264484334118713, 2.638427012816831674 ) ) ;
#38825 = CARTESIAN_POINT ( 'NONE',  ( 2.035157376598824452, 8.688685344154839285, 7.964842623401179544 ) ) ;
#38826 = CARTESIAN_POINT ( 'NONE',  ( 16.40814093676323893, 20.79030133659708923, 11.09922568453595026 ) ) ;
#38827 =( NAMED_UNIT ( * ) PLANE_ANGLE_UNIT ( ) SI_UNIT ( $, .RADIAN. ) );
#38828 = CARTESIAN_POINT ( 'NONE',  ( 17.20831665107776587, 62.88393115100078745, 7.208316651077764980 ) ) ;
#38829 = CARTESIAN_POINT ( 'NONE',  ( 6.933985542720472850, -73.15302115696529484, -2.750000000000000444 ) ) ;
#38830 = CARTESIAN_POINT ( 'NONE',  ( 2.035157376598822676, 22.43868534415483396, -7.964842623401177768 ) ) ;
#38831 = CARTESIAN_POINT ( 'NONE',  ( 7.361572987183169658, 44.96726448433412315, -9.846743663894592657 ) ) ;
#38832 = CARTESIAN_POINT ( 'NONE',  ( -2.815433093577223378, 0.5000000000000004441, 14.73340885523747978 ) ) ;
#38833 = CARTESIAN_POINT ( 'NONE',  ( -0.8801773607111009756, 18.06368534415484106, 1.068504757029289695E-15 ) ) ;
#38834 = DIRECTION ( 'NONE',  ( 0.000000000000000000, 1.000000000000000000, 0.000000000000000000 ) ) ;
#38835 = CARTESIAN_POINT ( 'NONE',  ( -0.8801773607111009756, 33.06368534415484106, 1.068504757029289695E-15 ) ) ;
#38837 = CARTESIAN_POINT ( 'NONE',  ( 17.35999999999999943, 37.99999999999997868, -7.000000000000000888 ) ) ;
#38836 = CARTESIAN_POINT ( 'NONE',  ( -4.164238869374098151, 61.59541550158063217, -3.795296366450310543 ) ) ;
#38838 = CARTESIAN_POINT ( 'NONE',  ( 12.63842701281683034, 2.467264484334118269, 9.846743663894596210 ) ) ;
#38839 = CARTESIAN_POINT ( 'NONE',  ( 0.1532563361054082862, 21.21726448433412315, 2.638427012816831674 ) ) ;
#38840 = CARTESIAN_POINT ( 'NONE',  ( 21.09922568453595559, 7.040301336597086568, -6.408140936763230044 ) ) ;
#38841 = FACE_OUTER_BOUND ( 'NONE', #68993, .T. ) ;
#38842 = DIRECTION ( 'NONE',  ( 0.9025852843498560762, 0.000000000000000000, 0.4305110968083047940 ) ) ;
#38843 = AXIS2_PLACEMENT_3D ( 'NONE', #51134, #34638, #20141 ) ;
#38844 = CARTESIAN_POINT ( 'NONE',  ( -0.2838433074297238012, 13.12729635533385597, -9.500000000000000000 ) ) ;
#38845 = EDGE_CURVE ( 'NONE', #76622, #73812, #36919, .T. ) ;
#38846 = CARTESIAN_POINT ( 'NONE',  ( -8.897294703554354811, -15.56348197609296058, -3.750000000000000000 ) ) ;
#38847 = CARTESIAN_POINT ( 'NONE',  ( 17.08211943468705130, 13.47041550158063572, 12.26659068614894998 ) ) ;
#38848 = AXIS2_PLACEMENT_3D ( 'NONE', #54647, #93145, #92652 ) ;
#38849 = CARTESIAN_POINT ( 'NONE',  ( 10.00000000000000000, 34.75893115100078745, -9.846743663894594434 ) ) ;
#38850 = CARTESIAN_POINT ( 'NONE',  ( -13.82671409943298357, -0.03417435944610275333, 3.447387012295131115 ) ) ;
#38851 = VERTEX_POINT ( 'NONE', #2461 ) ;
#38852 = CARTESIAN_POINT ( 'NONE',  ( 20.36894250292379382, 53.67874883491397497, 10.36894250292379205 ) ) ;
#38853 = ADVANCED_FACE ( 'NONE', ( #63418 ), #41440, .F. ) ;
#38854 = CARTESIAN_POINT ( 'NONE',  ( 2.791683348922237240, 25.38393115100078390, -7.208316651077763204 ) ) ;
#38856 = CYLINDRICAL_SURFACE ( 'NONE', #75786, 11.92686044187656513 ) ;
#38855 = CARTESIAN_POINT ( 'NONE',  ( 15.81765804549837107, -0.03417435944610275333, 2.383084218346927408 ) ) ;
#38857 = CARTESIAN_POINT ( 'NONE',  ( 12.91533473730992121, 44.52201867748816966, 10.88017736071110164 ) ) ;
#38858 = CARTESIAN_POINT ( 'NONE',  ( 0.6178305044545838731, 54.74863466993042493, 9.382169495545420901 ) ) ;
#38859 = CARTESIAN_POINT ( 'NONE',  ( 0.5774900079438607392, 23.48035201082150536, 5.440088680355550821 ) ) ;
#38860 = CARTESIAN_POINT ( 'NONE',  ( 16.40814093676324603, 42.45696800326375353, -11.09922568453594671 ) ) ;
#38861 = CARTESIAN_POINT ( 'NONE',  ( 3.591859063236763294, 3.290301336597087012, -11.09922568453595026 ) ) ;
#38862 = CARTESIAN_POINT ( 'NONE',  ( 0.1532563361054083140, 6.008931151000784787, 1.131784320476157264E-15 ) ) ;
#38863 = ORIENTED_EDGE ( 'NONE', *, *, #62916, .T. ) ;
#38864 = CARTESIAN_POINT ( 'NONE',  ( -8.900000000000002132, 83.99999999999994316, 0.000000000000000000 ) ) ;
#38865 = CARTESIAN_POINT ( 'NONE',  ( 12.00809552683959325, 14.49999999999999112, 8.989195838243645653 ) ) ;
#38866 = CARTESIAN_POINT ( 'NONE',  ( -4.164238869374099039, 51.80374883491396787, 8.674139862899312516E-16 ) ) ;
#38867 = CARTESIAN_POINT ( 'NONE',  ( 13.79529636645031943, 15.34541550158063750, -14.16423886937409904 ) ) ;
#38868 = CARTESIAN_POINT ( 'NONE',  ( 20.88017736071110164, 15.35535201082150358, 2.915334737309930979 ) ) ;
#38869 = CARTESIAN_POINT ( 'NONE',  ( 10.00000000000000178, 39.31368534415484106, 10.88017736071110342 ) ) ;
#38870 = CARTESIAN_POINT ( 'NONE',  ( 10.19513985507835763, 14.49999999999999112, -11.00268709613223450 ) ) ;
#38871 = CARTESIAN_POINT ( 'NONE',  ( -0.04758788293976230072, 0.000000000000000000, 5.453031268574419776 ) ) ;
#38872 = CARTESIAN_POINT ( 'NONE',  ( 10.00000000000000000, 66.81368534415484817, -10.88017736071110342 ) ) ;
#38873 = CARTESIAN_POINT ( 'NONE',  ( 0.5774900079438607392, 63.48035201082149825, 5.440088680355550821 ) ) ;
#38874 = CARTESIAN_POINT ( 'NONE',  ( -1.099225684535947600, 29.54030133659708923, 6.408140936763237150 ) ) ;
#38875 = CARTESIAN_POINT ( 'NONE',  ( 5.376821459230018974, 0.2301511342434729712, 13.93958558162640493 ) ) ;
#38876 = CYLINDRICAL_SURFACE ( 'NONE', #13229, 0.2500000000000002220 ) ;
#38877 = CARTESIAN_POINT ( 'NONE',  ( 5.076628168052704559, 10.17559781766745175, -8.527530157486179263 ) ) ;
#38878 = CARTESIAN_POINT ( 'NONE',  ( 18.52753015748618282, 33.92559781766745886, -4.923371831947291888 ) ) ;
#38879 = CARTESIAN_POINT ( 'NONE',  ( 20.88017736071110875, 15.77201867748817143, -2.915334737309920765 ) ) ;
#38881 = EDGE_CURVE ( 'NONE', #87349, #71629, #62379, .T. ) ;
#38880 = CARTESIAN_POINT ( 'NONE',  ( -1.099225684535947600, 38.70696800326375353, -6.408140936763238038 ) ) ;
#38882 = TOROIDAL_SURFACE ( 'NONE', #26297, 0.5000000000000043299, 0.5000000000000000000 ) ;
#38883 = B_SPLINE_CURVE_WITH_KNOTS ( 'NONE', 3,
 ( #98755, #31192, #44224, #98255 ),
 .UNSPECIFIED., .F., .F.,
 ( 4, 4 ),
 ( 9.215718466126787689E-19, 0.002657014572710872727 ),
 .UNSPECIFIED. ) ;
#38884 = CARTESIAN_POINT ( 'NONE',  ( 0.1532563361054082862, 6.217264484334118713, 2.638427012816831674 ) ) ;
#38885 = DIRECTION ( 'NONE',  ( -0.1059530667249615893, 0.9943711317468825195, 0.000000000000000000 ) ) ;
#38886 = CARTESIAN_POINT ( 'NONE',  ( 2.791683348922240793, 51.63393115100078745, 7.208316651077764092 ) ) ;
#38887 = TOROIDAL_SURFACE ( 'NONE', #584, 14.49999999999999822, 0.5000000000000000000 ) ;
#38888 = CARTESIAN_POINT ( 'NONE',  ( 2.791683348922240793, 31.63393115100078745, 7.208316651077764092 ) ) ;
#38889 = CARTESIAN_POINT ( 'NONE',  ( 24.16423886937409904, 14.09541550158063217, 3.795296366450317205 ) ) ;
#38890 = CARTESIAN_POINT ( 'NONE',  ( 10.00000000000000178, 34.31368534415484106, 10.88017736071110342 ) ) ;
#38891 = CARTESIAN_POINT ( 'NONE',  ( 17.96484262340118221, 4.938685344154837509, 7.964842623401181321 ) ) ;
#38892 = ADVANCED_FACE ( 'NONE', ( #24950 ), #93922, .T. ) ;
#38893 = CIRCLE ( 'NONE', #85273, 14.49999999999999822 ) ;
#38894 = CARTESIAN_POINT ( 'NONE',  ( 4.559911319644449179, 28.89701867748817321, 9.422509992056141925 ) ) ;
#38895 = CARTESIAN_POINT ( 'NONE',  ( 20.88017736071110164, 35.35535201082150536, 2.915334737309930979 ) ) ;
#38896 = VERTEX_POINT ( 'NONE', #63894 ) ;
#38897 = AXIS2_PLACEMENT_3D ( 'NONE', #81710, #81229, #19249 ) ;
#38898 = CARTESIAN_POINT ( 'NONE',  ( -0.8801773607110991993, 37.85535201082151247, -2.915334737309923874 ) ) ;
#38899 = VERTEX_POINT ( 'NONE', #55931 ) ;
#38900 = CARTESIAN_POINT ( 'NONE',  ( 22.81628187352648496, 61.83196800326376774, -3.434112377981050290 ) ) ;
#38901 = CARTESIAN_POINT ( 'NONE',  ( 17.96484262340118221, 49.93868534415484106, 7.964842623401181321 ) ) ;
#38902 = ORIENTED_EDGE ( 'NONE', *, *, #67752, .F. ) ;
#38903 = CARTESIAN_POINT ( 'NONE',  ( 7.084665262690076126, 54.10535201082151247, 10.88017736071109987 ) ) ;
#38904 = CARTESIAN_POINT ( 'NONE',  ( 6.034747819266367053, -36.07388523691940918, 3.999999999999999556 ) ) ;
#38905 = CARTESIAN_POINT ( 'NONE',  ( -0.3289641300568005855, 25.10497603579417358, 5.963430220938281678 ) ) ;
#38906 = CARTESIAN_POINT ( 'NONE',  ( -4.164238869374099039, 66.80374883491396076, 8.674139862899312516E-16 ) ) ;
#38907 = CARTESIAN_POINT ( 'NONE',  ( 0.5774900079438607392, 63.48035201082149825, 5.440088680355550821 ) ) ;
#38908 = CARTESIAN_POINT ( 'NONE',  ( 18.72515096720583827, 56.07228050351029225, -6.499999999999803713 ) ) ;
#38909 = CARTESIAN_POINT ( 'NONE',  ( -3.878335320991981305, -3.629921146508663821, -4.000000000000000000 ) ) ;
#38910 = CARTESIAN_POINT ( 'NONE',  ( 10.00000000000000000, 1.813685344154837731, -10.88017736071110342 ) ) ;
#38911 = CARTESIAN_POINT ( 'NONE',  ( 5.076628168052703671, 26.84226448433411960, 8.527530157486179263 ) ) ;
#38912 = ORIENTED_EDGE ( 'NONE', *, *, #94646, .T. ) ;
#38913 = CARTESIAN_POINT ( 'NONE',  ( 12.63842701281683034, 37.46726448433411605, 9.846743663894596210 ) ) ;
#38914 = CARTESIAN_POINT ( 'NONE',  ( 19.42250999205614548, 35.98035201082151247, -5.440088680355545492 ) ) ;
#38915 = CARTESIAN_POINT ( 'NONE',  ( 10.00000000000000000, 34.75893115100078745, -9.846743663894594434 ) ) ;
#38916 = CARTESIAN_POINT ( 'NONE',  ( 6.565887622018943937, 23.08196800326375708, -12.81628187352647608 ) ) ;
#38918 = CARTESIAN_POINT ( 'NONE',  ( 20.10384461210894003, 1.743024370107933319, 6.337995344473744019 ) ) ;
#38917 = CARTESIAN_POINT ( 'NONE',  ( 12.50534872682732690, 4.484280952698287085E-16, -7.339363270777523596 ) ) ;
#38919 = CARTESIAN_POINT ( 'NONE',  ( 0.5774900079438607392, 43.48035201082151247, 5.440088680355550821 ) ) ;
#38920 = CARTESIAN_POINT ( 'NONE',  ( 17.08211943468705130, 53.47041550158063217, 12.26659068614894998 ) ) ;
#38921 = VECTOR ( 'NONE', #15253, 1000.000000000000000 ) ;
#38922 = EDGE_CURVE ( 'NONE', #72511, #12076, #52824, .T. ) ;
#38923 = CARTESIAN_POINT ( 'NONE',  ( 22.81628187352647785, 26.62363466993042138, 6.195893100308588602E-16 ) ) ;
#38924 = CARTESIAN_POINT ( 'NONE',  ( 1.472469842513823179, 50.59226448433411605, -4.923371831947296329 ) ) ;
#38925 = ORIENTED_EDGE ( 'NONE', *, *, #96003, .F. ) ;
#38926 = CARTESIAN_POINT ( 'NONE',  ( 16.40814093676324603, 17.45696800326375353, -11.09922568453594671 ) ) ;
#38927 = CARTESIAN_POINT ( 'NONE',  ( 4.559911319644449179, 18.89701867748817321, 9.422509992056141925 ) ) ;
#38928 = CARTESIAN_POINT ( 'NONE',  ( 4.559911319644449179, 63.89701867748817676, 9.422509992056141925 ) ) ;
#38929 = B_SPLINE_CURVE_WITH_KNOTS ( 'NONE', 3,
 ( #69326, #62793, #93786, #38343, #847, #55801, #62293, #68838, #30818, #1832, #61316, #23345, #31305, #61807, #11762, #26268, #42270, #73239 ),
 .UNSPECIFIED., .F., .F.,
 ( 4, 2, 2, 2, 2, 2, 2, 2, 4 ),
 ( 2.168404344971008868E-18, 0.002783570816222668415, 0.005567141632445335095, 0.01113428326489066672, 0.02226856652978132997, 0.04453713305956264606, 0.06680569958934397257, 0.07793998285423464623, 0.08907426611912530601 ),
 .UNSPECIFIED. ) ;
#38930 = ORIENTED_EDGE ( 'NONE', *, *, #77246, .T. ) ;
#38931 = CARTESIAN_POINT ( 'NONE',  ( 2.791683348922237240, 5.383931151000785675, -7.208316651077763204 ) ) ;
#38932 = CARTESIAN_POINT ( 'NONE',  ( 7.361572987183170547, 52.05059781766745175, 9.846743663894590881 ) ) ;
#38933 = CARTESIAN_POINT ( 'NONE',  ( 2.791683348922237240, 35.38393115100079456, -7.208316651077763204 ) ) ;
#38934 = DIRECTION ( 'NONE',  ( 0.000000000000000000, 0.000000000000000000, -1.000000000000000000 ) ) ;
#38935 = CARTESIAN_POINT ( 'NONE',  ( 19.84674366389459266, 28.71726448433411960, -2.638427012816827677 ) ) ;
#38936 = CARTESIAN_POINT ( 'NONE',  ( -0.1503990784575328643, 40.12777174578613426, 6.262539305110068177 ) ) ;
#38937 = DIRECTION ( 'NONE',  ( -0.000000000000000000, 1.000000000000000000, 0.000000000000000000 ) ) ;
#38939 = CARTESIAN_POINT ( 'NONE',  ( 20.15039907845753575, 50.60158574516642460, -6.262539305110073506 ) ) ;
#38938 = CARTESIAN_POINT ( 'NONE',  ( 19.84674366389459266, 8.300597817667451750, 2.638427012816836559 ) ) ;
#38940 = CARTESIAN_POINT ( 'NONE',  ( -6.382347221874242749, 0.5000000000000004441, -13.57444820018235987 ) ) ;
#38942 = ORIENTED_EDGE ( 'NONE', *, *, #77550, .F. ) ;
#38941 = CARTESIAN_POINT ( 'NONE',  ( 10.00000000000000178, 42.25893115100078745, 9.846743663894594434 ) ) ;
#38943 = CARTESIAN_POINT ( 'NONE',  ( 11.62719953690064933, 14.63595249122790598, -9.476720473301801562 ) ) ;
#38944 = CARTESIAN_POINT ( 'NONE',  ( -2.816281873526473856, 9.331968003263753531, 3.434112377981055619 ) ) ;
#38945 = CARTESIAN_POINT ( 'NONE',  ( 12.91533473730992121, 54.52201867748816255, 10.88017736071110164 ) ) ;
#38946 = CARTESIAN_POINT ( 'NONE',  ( 20.36894250292379382, 38.67874883491396076, 10.36894250292379205 ) ) ;
#38947 = LINE ( 'NONE', #92425, #77527 ) ;
#38948 = CIRCLE ( 'NONE', #94824, 3.000000000000002665 ) ;
#38949 = CARTESIAN_POINT ( 'NONE',  ( 2.917880565312950480, 40.97041550158063217, -12.26659068614894821 ) ) ;
#38950 = CARTESIAN_POINT ( 'NONE',  ( 20.36894250292379738, 64.92874883491397497, -10.36894250292379027 ) ) ;
#38951 = CARTESIAN_POINT ( 'NONE',  ( 2.917880565312950480, 25.97041550158063572, -12.26659068614894821 ) ) ;
#38952 = CARTESIAN_POINT ( 'NONE',  ( 22.26659068614895176, 29.72041550158063572, -7.082119434687042414 ) ) ;
#38953 = CARTESIAN_POINT ( 'NONE',  ( 20.04068437667225311, 24.71974360917720759, 6.396802510829709298 ) ) ;
#38954 = EDGE_CURVE ( 'NONE', #92057, #60197, #66865, .T. ) ;
#38956 = CARTESIAN_POINT ( 'NONE',  ( 19.84674366389459266, 38.71726448433412315, -2.638427012816827677 ) ) ;
#38955 = CARTESIAN_POINT ( 'NONE',  ( 4.130000001237588592, 0.09091675483695403626, 2.500000000000000000 ) ) ;
#38957 = ORIENTED_EDGE ( 'NONE', *, *, #20199, .F. ) ;
#38958 = CARTESIAN_POINT ( 'NONE',  ( 20.88017736071110875, 25.77201867748816966, -2.915334737309920765 ) ) ;
#38959 = CARTESIAN_POINT ( 'NONE',  ( 6.829574850505127692, -88.00372650098204019, -3.749999999999998668 ) ) ;
#38960 = LINE ( 'NONE', #69452, #7493 ) ;
#38961 = DIRECTION ( 'NONE',  ( -0.04361938736533987893, 0.000000000000000000, 0.9990482215818576872 ) ) ;
#38962 = CARTESIAN_POINT ( 'NONE',  ( 18.52753015748618282, 33.92559781766745886, -4.923371831947291888 ) ) ;
#38963 = CARTESIAN_POINT ( 'NONE',  ( 10.00000000000000000, 57.87363466993042493, -12.81628187352647608 ) ) ;
#38964 = CARTESIAN_POINT ( 'NONE',  ( 14.16423886937410082, -10.48791783175269643, -3.795296366450314096 ) ) ;
#38965 = CARTESIAN_POINT ( 'NONE',  ( 18.52753015748617571, 38.09226448433412315, 4.923371831947298993 ) ) ;
#38966 = CARTESIAN_POINT ( 'NONE',  ( 18.52753015748617571, 58.09226448433411605, 4.923371831947298993 ) ) ;
#38967 = ADVANCED_FACE ( 'NONE', ( #51868 ), #59237, .T. ) ;
#38968 = CARTESIAN_POINT ( 'NONE',  ( 20.36894250292379738, 44.92874883491396787, -10.36894250292379027 ) ) ;
#38969 = ORIENTED_EDGE ( 'NONE', *, *, #38300, .F. ) ;
#38970 = CARTESIAN_POINT ( 'NONE',  ( 13.79529636645030344, 18.26208216824730002, 14.16423886937410614 ) ) ;
#38971 = ADVANCED_FACE ( 'NONE', ( #5398 ), #59354, .T. ) ;
#38972 = CARTESIAN_POINT ( 'NONE',  ( -0.8801773607111009756, 58.06368534415484106, 1.068504757029289695E-15 ) ) ;
#38974 = DIRECTION ( 'NONE',  ( 0.000000000000000000, 0.000000000000000000, 1.000000000000000000 ) ) ;
#38973 = CYLINDRICAL_SURFACE ( 'NONE', #19537, 0.2500000000000002220 ) ;
#38975 = CARTESIAN_POINT ( 'NONE',  ( -4.164238869374099927, 67.01208216824728936, 3.795296366450308767 ) ) ;
#38976 = CARTESIAN_POINT ( 'NONE',  ( 13.43411237798105340, 5.581968003263753531, 12.81628187352647963 ) ) ;
#38977 = SURFACE_STYLE_USAGE ( .BOTH. , #54449 ) ;
#38978 = CARTESIAN_POINT ( 'NONE',  ( 17.20831665107776587, 4.133931151000785675, -7.208316651077762316 ) ) ;
#38979 = CARTESIAN_POINT ( 'NONE',  ( 13.99999999999999822, 60.50000000000000000, 6.500000000000000888 ) ) ;
#38980 = CARTESIAN_POINT ( 'NONE',  ( 15.67879934938582664, 15.00000000000000000, -3.170591017105818921 ) ) ;
#38981 = DIRECTION ( 'NONE',  ( -1.000000000000000000, 0.000000000000000000, 0.000000000000000000 ) ) ;
#38982 = CARTESIAN_POINT ( 'NONE',  ( 13.79529636645030344, 58.26208216824728936, 14.16423886937410614 ) ) ;
#38983 = DIRECTION ( 'NONE',  ( 1.000000000000000000, -0.000000000000000000, -0.000000000000000000 ) ) ;
#38984 = CARTESIAN_POINT ( 'NONE',  ( 20.88017736071110519, 20.56368534415484106, 2.639326808657452039E-16 ) ) ;
#38985 = CARTESIAN_POINT ( 'NONE',  ( 15.44008868035555793, 26.39701867748817321, -9.422509992056140149 ) ) ;
#38986 = CARTESIAN_POINT ( 'NONE',  ( 12.63842701281683922, 54.55059781766745175, -9.846743663894590881 ) ) ;
#38987 = CARTESIAN_POINT ( 'NONE',  ( 12.63842701281683922, 49.55059781766744464, -9.846743663894590881 ) ) ;
#38988 = CARTESIAN_POINT ( 'NONE',  ( 3.591859063236761518, 59.95696800326375353, 11.09922568453594849 ) ) ;
#38989 = DIRECTION ( 'NONE',  ( 0.9848077530122084644, 0.1736481776669282495, 0.000000000000000000 ) ) ;
#38990 = VERTEX_POINT ( 'NONE', #97384 ) ;
#38991 = EDGE_CURVE ( 'NONE', #86252, #63207, #48037, .T. ) ;
#38992 = CARTESIAN_POINT ( 'NONE',  ( 19.42250999205614548, 10.98035201082150358, -5.440088680355545492 ) ) ;
#38993 = CARTESIAN_POINT ( 'NONE',  ( 0.6178305044545818747, 13.49863466993041783, -9.382169495545419124 ) ) ;
#38994 = CYLINDRICAL_SURFACE ( 'NONE', #54488, 9.999999999999996447 ) ;
#38995 = CARTESIAN_POINT ( 'NONE',  ( 5.076628168052704559, 60.17559781766745175, -8.527530157486179263 ) ) ;
#38996 = CARTESIAN_POINT ( 'NONE',  ( 17.96484262340118221, 44.93868534415483396, 7.964842623401181321 ) ) ;
#38997 = CARTESIAN_POINT ( 'NONE',  ( -1.099225684535947600, 24.54030133659708923, 6.408140936763237150 ) ) ;
#38999 = DIRECTION ( 'NONE',  ( -0.000000000000000000, -1.000000000000000000, -0.000000000000000000 ) ) ;
#38998 = CARTESIAN_POINT ( 'NONE',  ( 0.5774900079438590739, 62.64701867748817676, -5.440088680355550821 ) ) ;
#39000 = CARTESIAN_POINT ( 'NONE',  ( 10.82344394350224803, 0.04922511925147020351, 10.02492699998885328 ) ) ;
#39001 = CARTESIAN_POINT ( 'NONE',  ( 13.43411237798105340, 60.58196800326376064, 12.81628187352647963 ) ) ;
#39002 = ORIENTED_EDGE ( 'NONE', *, *, #9021, .T. ) ;
#39003 = CARTESIAN_POINT ( 'NONE',  ( 0.8952175423694801459, 47.60160829253886305, -5.990408912944315212 ) ) ;
#39004 = LINE ( 'NONE', #39500, #23922 ) ;
#39005 = CARTESIAN_POINT ( 'NONE',  ( 15.44008868035555793, 46.39701867748817676, -9.422509992056140149 ) ) ;
#39007 = CARTESIAN_POINT ( 'NONE',  ( -4.164238869374099927, 17.01208216824730357, 3.795296366450308767 ) ) ;
#39006 = CARTESIAN_POINT ( 'NONE',  ( 6.565887622018943937, 53.08196800326374643, -12.81628187352647608 ) ) ;
#39008 = EDGE_CURVE ( 'NONE', #37711, #35624, #2743, .T. ) ;
#39009 = CARTESIAN_POINT ( 'NONE',  ( 4.219999999999999751, 37.25000000000000000, 4.000000000000000000 ) ) ;
#39010 = CARTESIAN_POINT ( 'NONE',  ( 19.84674366389459266, 23.71726448433412315, -2.638427012816827677 ) ) ;
#39011 = CARTESIAN_POINT ( 'NONE',  ( 0.000000000000000000, 15.00000000000000000, 0.000000000000000000 ) ) ;
#39012 = CARTESIAN_POINT ( 'NONE',  ( -0.3689425029237898834, 56.17874883491396076, -10.36894250292378850 ) ) ;
#39013 = ORIENTED_EDGE ( 'NONE', *, *, #55858, .T. ) ;
#39014 = CARTESIAN_POINT ( 'NONE',  ( 4.559911319644449179, 8.897018677488171434, 9.422509992056141925 ) ) ;
#39015 = CARTESIAN_POINT ( 'NONE',  ( -0.7166339456633684657, 15.00000000000000000, 15.98010739087745868 ) ) ;
#39016 = ORIENTED_EDGE ( 'NONE', *, *, #7405, .T. ) ;
#39017 = EDGE_LOOP ( 'NONE', ( #92758, #9366, #26685, #55729 ) ) ;
#39018 = CARTESIAN_POINT ( 'NONE',  ( -0.8801773607110991993, 2.855352010821504471, -2.915334737309923874 ) ) ;
#39019 = CARTESIAN_POINT ( 'NONE',  ( 7.084665262690076126, 4.105352010821503583, 10.88017736071109987 ) ) ;
#39020 = CARTESIAN_POINT ( 'NONE',  ( 10.00000000000000178, 37.25893115100078745, 9.846743663894594434 ) ) ;
#39021 = CARTESIAN_POINT ( 'NONE',  ( 22.81628187352647785, 41.41530133659708923, 3.434112377981063169 ) ) ;
#39022 = CARTESIAN_POINT ( 'NONE',  ( -0.1503990784575279516, 43.10158574516643171, 6.262539305110076171 ) ) ;
#39025 = CARTESIAN_POINT ( 'NONE',  ( 13.79529636645030344, 18.26208216824730002, 14.16423886937410614 ) ) ;
#39024 = CARTESIAN_POINT ( 'NONE',  ( 0.6076426042653170212, 2.375764716086009365, -6.500000000000000888 ) ) ;
#39023 = AXIS2_PLACEMENT_3D ( 'NONE', #36476, #5497, #88981 ) ;
#39026 = CARTESIAN_POINT ( 'NONE',  ( 7.084665262690076126, 24.10535201082150181, 10.88017736071109987 ) ) ;
#39027 = CARTESIAN_POINT ( 'NONE',  ( -2.266590686148945544, 67.22041550158063217, 7.082119434687048631 ) ) ;
#39028 = CARTESIAN_POINT ( 'NONE',  ( 5.076628168052704559, 40.17559781766745175, -8.527530157486179263 ) ) ;
#39029 = DIRECTION ( 'NONE',  ( -0.000000000000000000, -1.000000000000000000, -0.000000000000000000 ) ) ;
#39030 = CARTESIAN_POINT ( 'NONE',  ( 19.84674366389459621, 23.50893115100078390, 7.409399052514197653E-17 ) ) ;
#39031 = VECTOR ( 'NONE', #74496, 1000.000000000000000 ) ;
#39032 = CARTESIAN_POINT ( 'NONE',  ( 2.638427012816835227, 27.46726448433411960, 9.846743663894590881 ) ) ;
#39033 = ORIENTED_EDGE ( 'NONE', *, *, #13086, .T. ) ;
#39034 = DIRECTION ( 'NONE',  ( -0.08715574274766037244, -0.9961946980917453232, -0.000000000000000000 ) ) ;
#39035 = B_SPLINE_CURVE_WITH_KNOTS ( 'NONE', 3,
 ( #92062, #54055, #17064, #68581 ),
 .UNSPECIFIED., .F., .F.,
 ( 4, 4 ),
 ( 5.553824967135426632E-18, 0.0003153927346766718259 ),
 .UNSPECIFIED. ) ;
#39036 = VERTEX_POINT ( 'NONE', #50880 ) ;
#39037 = CARTESIAN_POINT ( 'NONE',  ( 10.00000000000000178, 57.25893115100078745, 9.846743663894594434 ) ) ;
#39039 = CARTESIAN_POINT ( 'NONE',  ( -0.8801773607110991993, 42.85535201082150536, -2.915334737309923874 ) ) ;
#39038 = CARTESIAN_POINT ( 'NONE',  ( 19.42250999205614193, 30.14701867748817321, 5.440088680355555262 ) ) ;
#39041 = CARTESIAN_POINT ( 'NONE',  ( 16.40814093676324603, 27.45696800326375708, -11.09922568453594671 ) ) ;
#39040 = CARTESIAN_POINT ( 'NONE',  ( 15.44008868035555260, 4.730352010821504471, 9.422509992056143702 ) ) ;
#39042 = CARTESIAN_POINT ( 'NONE',  ( -4.164238869374099927, 12.01208216824730357, 3.795296366450308767 ) ) ;
#39043 = ORIENTED_EDGE ( 'NONE', *, *, #9128, .F. ) ;
#39044 = CARTESIAN_POINT ( 'NONE',  ( 22.81628187352647785, 46.62363466993041783, 6.195893100308588602E-16 ) ) ;
#39045 = ORIENTED_EDGE ( 'NONE', *, *, #25034, .T. ) ;
#39046 = CARTESIAN_POINT ( 'NONE',  ( 14.92337183194729633, 42.67559781766745886, 8.527530157486181039 ) ) ;
#39047 = CARTESIAN_POINT ( 'NONE',  ( 20.88017736071110164, 20.35535201082150891, 2.915334737309930979 ) ) ;
#39048 = ORIENTED_EDGE ( 'NONE', *, *, #19779, .F. ) ;
#39049 = CARTESIAN_POINT ( 'NONE',  ( 4.559911319644449179, 18.89701867748817321, 9.422509992056141925 ) ) ;
#39050 = ORIENTED_EDGE ( 'NONE', *, *, #45977, .T. ) ;
#39051 = CARTESIAN_POINT ( 'NONE',  ( 4.559911319644449179, 58.89701867748817676, 9.422509992056141925 ) ) ;
#39052 = DIRECTION ( 'NONE',  ( 0.000000000000000000, -1.000000000000000000, 0.000000000000000000 ) ) ;
#39054 = EDGE_CURVE ( 'NONE', #23604, #11760, #71023, .T. ) ;
#39053 = DIRECTION ( 'NONE',  ( 1.000000000000000000, 0.000000000000000000, -1.224646799147353207E-16 ) ) ;
#39055 =( BOUNDED_SURFACE ( )  B_SPLINE_SURFACE ( 1, 2, ( 
 ( #52050, #22551, #60528, #7049, #37553, #44541, #30515, #91530, #14058, #30022, #36559, #23045, #23543, #7557, #61018, #97571, #38046, #82541, #68043, #52533, #98569, #75037, #29522, #8035, #6543, #37053, #15549, #53517, #83041, #91018, #67552, #54015, #53021, #68538, #16021, #83536, #29034, #76026, #22059, #31010, #84524, #15055, #98063, #84029, #60029, #90524, #14557, #74540, #45026, #75533, #46034, #45528, #69, #6060, #76519, #38533, #59543, #69029, #564, #61506, #92013, #90038, #21561, #46510, #2028, #9004, #78489, #17513, #55502, #63481, #85011, #48476, #9500, #70504, #10003, #8522, #56480, #17014, #25014, #40002, #31982, #33457, #32490, #25507, #40996, #39025, #47979, #62985, #85504, #40505, #93491, #71001, #86002, #25983, #69520, #47492, #86494, #92992, #54985, #39520, #3008, #2524, #77995, #1035, #16524, #46999, #63954, #24526, #32977, #93985, #55994, #54496, #24028, #17994, #78975, #10485, #77492, #71493, #94466, #86966, #62488, #70012, #77010, #31496, #61999, #92498, #1538, #49953, #4957, #35931, #58425, #49452, #95961, #79958, #71964, #64448, #11462, #35437, #3487, #80458, #27443, #57937, #88939, #72444, #57453, #34443, #43430, #41980, #87946, #18974, #11956, #96961, #87459, #42461, #19461, #20448, #33944, #64934, #12443, #56956, #88445, #48965, #42951, #65932, #12936, #3974, #95462, #73931, #50938, #26953, #19945, #72943, #26457, #4473, #66428, #28433, #34939, #65437, #81432, #5459, #50440, #27932, #10974, #41495, #80945, #96460, #73430, #58931, #18480, #79475, #94955, #82916, #67923, #37927, #14933, #29405, #45400, #76400, #7431, #68911, #98444, #67423, #6926, #68416, #51931, #97948, #21937, #14434, #98939, #29900, #74920, #91396, #15433, #81922, #82415, #59908, #52417, #44905, #30393, #60405, #6418, #22924, #45911, #13430, #90901, #75407, #90398, #22429, #37433, #83412, #52901, #439, #43916, #75906, #60897, #36931, #53393, #13939, #7915, #83903, #38411, #74414, #59414, #89920, #30892, #89431, #20945, #51432, #5943, #97447, #66927, #36434, #28912, #21434, #44416, #16890, #24399, #93364, #46878, #31378, #63355, #55376, #93859, #78859, #10371, #92869, #47858, #40872, #2399, #92381, #39881, #23907, #15906, #8397, #54376, #78364, #46396, #54867, #70387, #1906, #32856, #16396, #1412, #77370, #86369, #84889, #31865, #61876, #85378, #71377, #8881, #47369, #62364, #25387, #76884, #39399, #85877, #915, #32361, #91895, #17389, #9883, #55870, #69892, #77867, #17870, #48353, #9378, #62868, #24892, #69393, #40383, #2889, #61386, #70882, #23420, #53899, #84407, #38906, #42832, #25867, #56364, #71848, #12328, #41861 ),
 ( #94839, #73317, #42341, #79836, #44672, #36692, #95838, #18363, #34822, #27321, #11833, #14188, #6188, #33340, #87821, #26341, #65312, #4356, #72816, #50314, #3358, #67180, #95334, #57327, #57819, #94348, #75166, #3857, #88327, #26833, #18856, #21692, #19341, #97703, #29169, #86857, #82672, #72324, #49824, #19825, #80334, #80828, #52178, #11341, #87341, #59670, #90162, #33821, #63834, #34317, #48842, #79353, #64327, #10860, #41381, #56842, #49336, #64815, #74692, #73692, #20714, #81208, #20211, #6202, #51205, #50206, #96725, #97720, #42237, #90176, #12708, #89691, #28201, #43202, #21706, #82187, #72703, #81688, #57709, #89201, #43695, #5227, #67195, #73202, #29184, #80220, #4734, #11724, #4239, #34708, #65203, #95724, #27208, #88209, #96227, #27706, #45676, #30164, #15194, #60177, #7191, #84660, #22200, #90674, #23687, #69175, #60668, #76174, #45178, #31644, #7695, #15690, #52191, #38191, #44684, #46175, #22694, #8657, #1185, #30656, #52679, #54150, #37694, #83180, #83679, #14203, #68678, #206, #16168, #61163, #91671, #6691, #46652, #76659, #37210, #23190, #698, #39170, #67698, #31151, #69659, #98210, #29668, #24661, #55131, #72105, #62629, #85645, #33604, #33120, #70651, #34099, #26131, #86635, #9151, #17656, #25647, #18145, #2669, #3632, #94616, #24167, #78641, #17164, #56140, #94121, #63614, #41146, #93134, #56622, #86143, #48126, #48617, #85155, #64590, #93632, #79121, #10148, #9650, #11121, #40643, #3142, #18626, #16663, #54637, #63130, #71141, #10634, #71631, #64100, #41640, #2174, #78140, #87111, #49118, #47645, #79620, #25167, #47137, #77634, #40147, #39669, #70160, #32631, #55643, #1677, #32130, #88585, #35591, #65580, #35081, #21089, #66079, #34587, #50597, #13583, #57104, #74574, #96107, #5603, #81089, #58081, #6088, #97112, #87600, #96607, #72590, #43090, #12590, #27591, #20093, #65082, #51085, #13083, #95605, #73575, #19110, #43578, #44067, #28084, #81576, #49590, #58582, #4124, #5100, #73083, #89084, #27091, #50099, #28584, #57594, #88091, #36082, #74071, #4620, #20599, #19604, #36591, #66585, #59074, #95098, #89578, #80102, #51587, #82073, #26606, #11607, #42124, #80604, #12102, #42605, #91052, #84059, #37086, #22579, #60561, #98, #52564, #67585, #69057, #61045, #593, #84552, #16052, #98602, #53546, #46540, #8065, #98094, #45560, #29554, #21591, #44570, #60058, #46059, #52082, #53050, #38076, #30545, #38561, #22088, #7080, #83068, #92045, #90559, #37582, #14588, #83569, #77041, #45057, #15089, #68075, #31036, #82575, #75567, #91558, #23077, #61536, #97605, #23573, #54042, #8554, #67078, #29066, #59574 ) ),
 .UNSPECIFIED., .F., .F., .T. ) 
 B_SPLINE_SURFACE_WITH_KNOTS ( ( 2, 2 ),
 ( 3, 2, 2, 2, 2, 2, 2, 2, 2, 2, 2, 2, 2, 2, 2, 2, 2, 2, 2, 2, 2, 2, 2, 2, 2, 2, 2, 2, 2, 2, 2, 2, 2, 2, 2, 2, 2, 2, 2, 2, 2, 2, 2, 2, 2, 2, 2, 2, 2, 2, 2, 2, 2, 2, 2, 2, 2, 2, 2, 2, 2, 2, 2, 2, 2, 2, 2, 2, 2, 2, 2, 2, 2, 2, 2, 2, 2, 2, 2, 2, 2, 2, 2, 2, 2, 2, 2, 2, 2, 2, 2, 2, 2, 2, 2, 2, 2, 2, 2, 2, 2, 2, 2, 2, 2, 2, 2, 2, 2, 2, 2, 2, 2, 2, 2, 2, 2, 2, 2, 2, 2, 2, 2, 2, 2, 2, 2, 2, 2, 2, 2, 2, 2, 2, 2, 2, 2, 2, 2, 2, 2, 2, 2, 2, 2, 2, 2, 2, 2, 2, 2, 2, 2, 2, 2, 2, 2, 2, 2, 2, 2, 2, 3 ),
 ( 0.000000000000000000, 1.000000000000000000 ),
 ( 0.000000000000000000, 0.005952380952380952051, 0.01190476190476190410, 0.01785714285714285615, 0.02380952380952380820, 0.02976190476190476025, 0.03571428571428571230, 0.04166666666666666435, 0.04761904761904761640, 0.05357142857142856845, 0.05952380952380952051, 0.06547619047619047949, 0.07142857142857142461, 0.07738095238095238360, 0.08333333333333332871, 0.08928571428571428770, 0.09523809523809523281, 0.1011904761904761918, 0.1071428571428571369, 0.1130952380952380959, 0.1190476190476190410, 0.1250000000000000000, 0.1309523809523809590, 0.1369047619047619180, 0.1428571428571428492, 0.1488095238095238082, 0.1547619047619047672, 0.1607142857142857262, 0.1666666666666666574, 0.1726190476190476164, 0.1785714285714285754, 0.1845238095238095344, 0.1904761904761904656, 0.1964285714285714246, 0.2023809523809523836, 0.2083333333333333426, 0.2142857142857142738, 0.2202380952380952328, 0.2261904761904761918, 0.2321428571428571508, 0.2380952380952380820, 0.2440476190476190410, 0.2500000000000000000, 0.2559523809523809312, 0.2619047619047619180, 0.2678571428571428492, 0.2738095238095238360, 0.2797619047619047672, 0.2857142857142856984, 0.2916666666666666852, 0.2976190476190476164, 0.3035714285714285476, 0.3095238095238095344, 0.3154761904761904656, 0.3214285714285714524, 0.3273809523809523836, 0.3333333333333333148, 0.3392857142857143016, 0.3452380952380952328, 0.3511904761904761640, 0.3571428571428571508, 0.3630952380952380820, 0.3690476190476190688, 0.3750000000000000000, 0.3809523809523809312, 0.3869047619047619180, 0.3928571428571428492, 0.3988095238095238360, 0.4047619047619047672, 0.4107142857142856984, 0.4166666666666666852, 0.4226190476190476164, 0.4285714285714285476, 0.4345238095238095344, 0.4404761904761904656, 0.4464285714285714524, 0.4523809523809523836, 0.4583333333333333148, 0.4642857142857143016, 0.4702380952380952328, 0.4761904761904761640, 0.4821428571428571508, 0.4880952380952380820, 0.4940476190476190688, 0.5000000000000000000, 0.5059523809523809312, 0.5119047619047618625, 0.5178571428571429047, 0.5238095238095238360, 0.5297619047619047672, 0.5357142857142856984, 0.5416666666666666297, 0.5476190476190476719, 0.5535714285714286031, 0.5595238095238095344, 0.5654761904761904656, 0.5714285714285713969, 0.5773809523809523281, 0.5833333333333333703, 0.5892857142857143016, 0.5952380952380952328, 0.6011904761904761640, 0.6071428571428570953, 0.6130952380952381375, 0.6190476190476190688, 0.6250000000000000000, 0.6309523809523809312, 0.6369047619047618625, 0.6428571428571429047, 0.6488095238095238360, 0.6547619047619047672, 0.6607142857142856984, 0.6666666666666666297, 0.6726190476190476719, 0.6785714285714286031, 0.6845238095238095344, 0.6904761904761904656, 0.6964285714285713969, 0.7023809523809523281, 0.7083333333333333703, 0.7142857142857143016, 0.7202380952380952328, 0.7261904761904761640, 0.7321428571428570953, 0.7380952380952381375, 0.7440476190476190688, 0.7500000000000000000, 0.7559523809523809312, 0.7619047619047618625, 0.7678571428571429047, 0.7738095238095238360, 0.7797619047619047672, 0.7857142857142856984, 0.7916666666666666297, 0.7976190476190476719, 0.8035714285714286031, 0.8095238095238095344, 0.8154761904761904656, 0.8214285714285713969, 0.8273809523809523281, 0.8333333333333333703, 0.8392857142857143016, 0.8452380952380952328, 0.8511904761904761640, 0.8571428571428570953, 0.8630952380952381375, 0.8690476190476190688, 0.8750000000000000000, 0.8809523809523809312, 0.8869047619047618625, 0.8928571428571429047, 0.8988095238095238360, 0.9047619047619047672, 0.9107142857142856984, 0.9166666666666666297, 0.9226190476190476719, 0.9285714285714286031, 0.9345238095238095344, 0.9404761904761904656, 0.9464285714285713969, 0.9523809523809523281, 0.9583333333333333703, 0.9642857142857143016 ),
 .UNSPECIFIED. ) 
 GEOMETRIC_REPRESENTATION_ITEM ( )  RATIONAL_B_SPLINE_SURFACE ( (
 ( 1.000000000000000000, 0.9659258262890683122, 1.000000000000000000, 0.9659258262890683122, 1.000000000000000000, 0.9659258262890683122, 1.000000000000000000, 0.9659258262890683122, 1.000000000000000000, 0.9659258262890683122, 1.000000000000000000, 0.9659258262890683122, 1.000000000000000000, 0.9659258262890683122, 1.000000000000000000, 0.9659258262890683122, 1.000000000000000000, 0.9659258262890683122, 1.000000000000000000, 0.9659258262890683122, 1.000000000000000000, 0.9659258262890683122, 1.000000000000000000, 0.9659258262890683122, 1.000000000000000000, 0.9659258262890683122, 1.000000000000000000, 0.9659258262890683122, 1.000000000000000000, 0.9659258262890683122, 1.000000000000000000, 0.9659258262890683122, 1.000000000000000000, 0.9659258262890683122, 1.000000000000000000, 0.9659258262890683122, 1.000000000000000000, 0.9659258262890683122, 1.000000000000000000, 0.9659258262890683122, 1.000000000000000000, 0.9659258262890683122, 1.000000000000000000, 0.9659258262890683122, 1.000000000000000000, 0.9659258262890683122, 1.000000000000000000, 0.9659258262890683122, 1.000000000000000000, 0.9659258262890683122, 1.000000000000000000, 0.9659258262890683122, 1.000000000000000000, 0.9659258262890683122, 1.000000000000000000, 0.9659258262890683122, 1.000000000000000000, 0.9659258262890683122, 1.000000000000000000, 0.9659258262890683122, 1.000000000000000000, 0.9659258262890683122, 1.000000000000000000, 0.9659258262890683122, 1.000000000000000000, 0.9659258262890683122, 1.000000000000000000, 0.9659258262890683122, 1.000000000000000000, 0.9659258262890683122, 1.000000000000000000, 0.9659258262890683122, 1.000000000000000000, 0.9659258262890683122, 1.000000000000000000, 0.9659258262890683122, 1.000000000000000000, 0.9659258262890683122, 1.000000000000000000, 0.9659258262890683122, 1.000000000000000000, 0.9659258262890683122, 1.000000000000000000, 0.9659258262890683122, 1.000000000000000000, 0.9659258262890683122, 1.000000000000000000, 0.9659258262890683122, 1.000000000000000000, 0.9659258262890683122, 1.000000000000000000, 0.9659258262890683122, 1.000000000000000000, 0.9659258262890683122, 1.000000000000000000, 0.9659258262890683122, 1.000000000000000000, 0.9659258262890683122, 1.000000000000000000, 0.9659258262890683122, 1.000000000000000000, 0.9659258262890683122, 1.000000000000000000, 0.9659258262890683122, 1.000000000000000000, 0.9659258262890683122, 1.000000000000000000, 0.9659258262890683122, 1.000000000000000000, 0.9659258262890683122, 1.000000000000000000, 0.9659258262890683122, 1.000000000000000000, 0.9659258262890683122, 1.000000000000000000, 0.9659258262890683122, 1.000000000000000000, 0.9659258262890683122, 1.000000000000000000, 0.9659258262890683122, 1.000000000000000000, 0.9659258262890683122, 1.000000000000000000, 0.9659258262890683122, 1.000000000000000000, 0.9659258262890683122, 1.000000000000000000, 0.9659258262890683122, 1.000000000000000000, 0.9659258262890683122, 1.000000000000000000, 0.9659258262890683122, 1.000000000000000000, 0.9659258262890683122, 1.000000000000000000, 0.9659258262890683122, 1.000000000000000000, 0.9659258262890683122, 1.000000000000000000, 0.9659258262890683122, 1.000000000000000000, 0.9659258262890683122, 1.000000000000000000, 0.9659258262890683122, 1.000000000000000000, 0.9659258262890683122, 1.000000000000000000, 0.9659258262890683122, 1.000000000000000000, 0.9659258262890683122, 1.000000000000000000, 0.9659258262890683122, 1.000000000000000000, 0.9659258262890683122, 1.000000000000000000, 0.9659258262890683122, 1.000000000000000000, 0.9659258262890683122, 1.000000000000000000, 0.9659258262890683122, 1.000000000000000000, 0.9659258262890683122, 1.000000000000000000, 0.9659258262890683122, 1.000000000000000000, 0.9659258262890683122, 1.000000000000000000, 0.9659258262890683122, 1.000000000000000000, 0.9659258262890683122, 1.000000000000000000, 0.9659258262890683122, 1.000000000000000000, 0.9659258262890683122, 1.000000000000000000, 0.9659258262890683122, 1.000000000000000000, 0.9659258262890683122, 1.000000000000000000, 0.9659258262890683122, 1.000000000000000000, 0.9659258262890683122, 1.000000000000000000, 0.9659258262890683122, 1.000000000000000000, 0.9659258262890683122, 1.000000000000000000, 0.9659258262890683122, 1.000000000000000000, 0.9659258262890683122, 1.000000000000000000, 0.9659258262890683122, 1.000000000000000000, 0.9659258262890683122, 1.000000000000000000, 0.9659258262890683122, 1.000000000000000000, 0.9659258262890683122, 1.000000000000000000, 0.9659258262890683122, 1.000000000000000000, 0.9659258262890683122, 1.000000000000000000, 0.9659258262890683122, 1.000000000000000000, 0.9659258262890683122, 1.000000000000000000, 0.9659258262890683122, 1.000000000000000000, 0.9659258262890683122, 1.000000000000000000, 0.9659258262890683122, 1.000000000000000000, 0.9659258262890683122, 1.000000000000000000, 0.9659258262890683122, 1.000000000000000000, 0.9659258262890683122, 1.000000000000000000, 0.9659258262890683122, 1.000000000000000000, 0.9659258262890683122, 1.000000000000000000, 0.9659258262890683122, 1.000000000000000000, 0.9659258262890683122, 1.000000000000000000, 0.9659258262890683122, 1.000000000000000000, 0.9659258262890683122, 1.000000000000000000, 0.9659258262890683122, 1.000000000000000000, 0.9659258262890683122, 1.000000000000000000, 0.9659258262890683122, 1.000000000000000000, 0.9659258262890683122, 1.000000000000000000, 0.9659258262890683122, 1.000000000000000000, 0.9659258262890683122, 1.000000000000000000, 0.9659258262890683122, 1.000000000000000000, 0.9659258262890683122, 1.000000000000000000, 0.9659258262890683122, 1.000000000000000000, 0.9659258262890683122, 1.000000000000000000, 0.9659258262890683122, 1.000000000000000000, 0.9659258262890683122, 1.000000000000000000, 0.9659258262890683122, 1.000000000000000000, 0.9659258262890683122, 1.000000000000000000, 0.9659258262890683122, 1.000000000000000000, 0.9659258262890683122, 1.000000000000000000, 0.9659258262890683122, 1.000000000000000000, 0.9659258262890683122, 1.000000000000000000, 0.9659258262890683122, 1.000000000000000000, 0.9659258262890683122, 1.000000000000000000, 0.9659258262890683122, 1.000000000000000000, 0.9659258262890683122, 1.000000000000000000, 0.9659258262890683122, 1.000000000000000000, 0.9659258262890683122, 1.000000000000000000, 0.9659258262890683122, 1.000000000000000000, 0.9659258262890683122, 1.000000000000000000, 0.9659258262890683122, 1.000000000000000000, 0.9659258262890683122, 1.000000000000000000, 0.9659258262890683122, 1.000000000000000000, 0.9659258262890683122, 1.000000000000000000, 0.9659258262890683122, 1.000000000000000000, 0.9659258262890683122, 1.000000000000000000, 0.9659258262890683122, 1.000000000000000000, 0.9659258262890683122, 1.000000000000000000, 0.9659258262890683122, 1.000000000000000000, 0.9659258262890683122, 1.000000000000000000, 0.9659258262890683122, 1.000000000000000000, 0.9659258262890683122, 1.000000000000000000, 0.9659258262890683122, 1.000000000000000000, 0.9659258262890683122, 1.000000000000000000, 0.9659258262890683122, 1.000000000000000000, 0.9659258262890683122, 1.000000000000000000, 0.9659258262890683122, 1.000000000000000000, 0.9659258262890683122, 1.000000000000000000, 0.9659258262890683122, 1.000000000000000000, 0.9659258262890683122, 1.000000000000000000, 0.9659258262890683122, 1.000000000000000000),
 ( 1.000000000000000000, 0.9659258262890683122, 1.000000000000000000, 0.9659258262890683122, 1.000000000000000000, 0.9659258262890683122, 1.000000000000000000, 0.9659258262890683122, 1.000000000000000000, 0.9659258262890683122, 1.000000000000000000, 0.9659258262890683122, 1.000000000000000000, 0.9659258262890683122, 1.000000000000000000, 0.9659258262890683122, 1.000000000000000000, 0.9659258262890683122, 1.000000000000000000, 0.9659258262890683122, 1.000000000000000000, 0.9659258262890683122, 1.000000000000000000, 0.9659258262890683122, 1.000000000000000000, 0.9659258262890683122, 1.000000000000000000, 0.9659258262890683122, 1.000000000000000000, 0.9659258262890683122, 1.000000000000000000, 0.9659258262890683122, 1.000000000000000000, 0.9659258262890683122, 1.000000000000000000, 0.9659258262890683122, 1.000000000000000000, 0.9659258262890683122, 1.000000000000000000, 0.9659258262890683122, 1.000000000000000000, 0.9659258262890683122, 1.000000000000000000, 0.9659258262890683122, 1.000000000000000000, 0.9659258262890683122, 1.000000000000000000, 0.9659258262890683122, 1.000000000000000000, 0.9659258262890683122, 1.000000000000000000, 0.9659258262890683122, 1.000000000000000000, 0.9659258262890683122, 1.000000000000000000, 0.9659258262890683122, 1.000000000000000000, 0.9659258262890683122, 1.000000000000000000, 0.9659258262890683122, 1.000000000000000000, 0.9659258262890683122, 1.000000000000000000, 0.9659258262890683122, 1.000000000000000000, 0.9659258262890683122, 1.000000000000000000, 0.9659258262890683122, 1.000000000000000000, 0.9659258262890683122, 1.000000000000000000, 0.9659258262890683122, 1.000000000000000000, 0.9659258262890683122, 1.000000000000000000, 0.9659258262890683122, 1.000000000000000000, 0.9659258262890683122, 1.000000000000000000, 0.9659258262890683122, 1.000000000000000000, 0.9659258262890683122, 1.000000000000000000, 0.9659258262890683122, 1.000000000000000000, 0.9659258262890683122, 1.000000000000000000, 0.9659258262890683122, 1.000000000000000000, 0.9659258262890683122, 1.000000000000000000, 0.9659258262890683122, 1.000000000000000000, 0.9659258262890683122, 1.000000000000000000, 0.9659258262890683122, 1.000000000000000000, 0.9659258262890683122, 1.000000000000000000, 0.9659258262890683122, 1.000000000000000000, 0.9659258262890683122, 1.000000000000000000, 0.9659258262890683122, 1.000000000000000000, 0.9659258262890683122, 1.000000000000000000, 0.9659258262890683122, 1.000000000000000000, 0.9659258262890683122, 1.000000000000000000, 0.9659258262890683122, 1.000000000000000000, 0.9659258262890683122, 1.000000000000000000, 0.9659258262890683122, 1.000000000000000000, 0.9659258262890683122, 1.000000000000000000, 0.9659258262890683122, 1.000000000000000000, 0.9659258262890683122, 1.000000000000000000, 0.9659258262890683122, 1.000000000000000000, 0.9659258262890683122, 1.000000000000000000, 0.9659258262890683122, 1.000000000000000000, 0.9659258262890683122, 1.000000000000000000, 0.9659258262890683122, 1.000000000000000000, 0.9659258262890683122, 1.000000000000000000, 0.9659258262890683122, 1.000000000000000000, 0.9659258262890683122, 1.000000000000000000, 0.9659258262890683122, 1.000000000000000000, 0.9659258262890683122, 1.000000000000000000, 0.9659258262890683122, 1.000000000000000000, 0.9659258262890683122, 1.000000000000000000, 0.9659258262890683122, 1.000000000000000000, 0.9659258262890683122, 1.000000000000000000, 0.9659258262890683122, 1.000000000000000000, 0.9659258262890683122, 1.000000000000000000, 0.9659258262890683122, 1.000000000000000000, 0.9659258262890683122, 1.000000000000000000, 0.9659258262890683122, 1.000000000000000000, 0.9659258262890683122, 1.000000000000000000, 0.9659258262890683122, 1.000000000000000000, 0.9659258262890683122, 1.000000000000000000, 0.9659258262890683122, 1.000000000000000000, 0.9659258262890683122, 1.000000000000000000, 0.9659258262890683122, 1.000000000000000000, 0.9659258262890683122, 1.000000000000000000, 0.9659258262890683122, 1.000000000000000000, 0.9659258262890683122, 1.000000000000000000, 0.9659258262890683122, 1.000000000000000000, 0.9659258262890683122, 1.000000000000000000, 0.9659258262890683122, 1.000000000000000000, 0.9659258262890683122, 1.000000000000000000, 0.9659258262890683122, 1.000000000000000000, 0.9659258262890683122, 1.000000000000000000, 0.9659258262890683122, 1.000000000000000000, 0.9659258262890683122, 1.000000000000000000, 0.9659258262890683122, 1.000000000000000000, 0.9659258262890683122, 1.000000000000000000, 0.9659258262890683122, 1.000000000000000000, 0.9659258262890683122, 1.000000000000000000, 0.9659258262890683122, 1.000000000000000000, 0.9659258262890683122, 1.000000000000000000, 0.9659258262890683122, 1.000000000000000000, 0.9659258262890683122, 1.000000000000000000, 0.9659258262890683122, 1.000000000000000000, 0.9659258262890683122, 1.000000000000000000, 0.9659258262890683122, 1.000000000000000000, 0.9659258262890683122, 1.000000000000000000, 0.9659258262890683122, 1.000000000000000000, 0.9659258262890683122, 1.000000000000000000, 0.9659258262890683122, 1.000000000000000000, 0.9659258262890683122, 1.000000000000000000, 0.9659258262890683122, 1.000000000000000000, 0.9659258262890683122, 1.000000000000000000, 0.9659258262890683122, 1.000000000000000000, 0.9659258262890683122, 1.000000000000000000, 0.9659258262890683122, 1.000000000000000000, 0.9659258262890683122, 1.000000000000000000, 0.9659258262890683122, 1.000000000000000000, 0.9659258262890683122, 1.000000000000000000, 0.9659258262890683122, 1.000000000000000000, 0.9659258262890683122, 1.000000000000000000, 0.9659258262890683122, 1.000000000000000000, 0.9659258262890683122, 1.000000000000000000, 0.9659258262890683122, 1.000000000000000000, 0.9659258262890683122, 1.000000000000000000, 0.9659258262890683122, 1.000000000000000000, 0.9659258262890683122, 1.000000000000000000, 0.9659258262890683122, 1.000000000000000000, 0.9659258262890683122, 1.000000000000000000, 0.9659258262890683122, 1.000000000000000000, 0.9659258262890683122, 1.000000000000000000, 0.9659258262890683122, 1.000000000000000000, 0.9659258262890683122, 1.000000000000000000, 0.9659258262890683122, 1.000000000000000000, 0.9659258262890683122, 1.000000000000000000, 0.9659258262890683122, 1.000000000000000000, 0.9659258262890683122, 1.000000000000000000, 0.9659258262890683122, 1.000000000000000000, 0.9659258262890683122, 1.000000000000000000, 0.9659258262890683122, 1.000000000000000000, 0.9659258262890683122, 1.000000000000000000, 0.9659258262890683122, 1.000000000000000000, 0.9659258262890683122, 1.000000000000000000, 0.9659258262890683122, 1.000000000000000000, 0.9659258262890683122, 1.000000000000000000, 0.9659258262890683122, 1.000000000000000000, 0.9659258262890683122, 1.000000000000000000, 0.9659258262890683122, 1.000000000000000000, 0.9659258262890683122, 1.000000000000000000, 0.9659258262890683122, 1.000000000000000000, 0.9659258262890683122, 1.000000000000000000, 0.9659258262890683122, 1.000000000000000000, 0.9659258262890683122, 1.000000000000000000, 0.9659258262890683122, 1.000000000000000000, 0.9659258262890683122, 1.000000000000000000, 0.9659258262890683122, 1.000000000000000000, 0.9659258262890683122, 1.000000000000000000, 0.9659258262890683122, 1.000000000000000000, 0.9659258262890683122, 1.000000000000000000, 0.9659258262890683122, 1.000000000000000000) ) ) 
 REPRESENTATION_ITEM ( '' )  SURFACE ( )  );
#39056 = CARTESIAN_POINT ( 'NONE',  ( 14.92337183194729633, 7.675597817667451750, 8.527530157486181039 ) ) ;
#39057 = CARTESIAN_POINT ( 'NONE',  ( 2.035157376598824452, 68.68868534415484817, 7.964842623401179544 ) ) ;
#39058 = CARTESIAN_POINT ( 'NONE',  ( 5.054308323419867577, 70.51564955044841554, 5.000000000000000000 ) ) ;
#39060 = ADVANCED_FACE ( 'NONE', ( #35379 ), #73650, .T. ) ;
#39059 = VECTOR ( 'NONE', #82777, 1000.000000000000227 ) ;
#39061 = CARTESIAN_POINT ( 'NONE',  ( -46.94000000000001194, 103.0000000000000000, 5.997726559847112782 ) ) ;
#39063 = ORIENTED_EDGE ( 'NONE', *, *, #26997, .F. ) ;
#39062 = CARTESIAN_POINT ( 'NONE',  ( 19.84674366389459266, 3.717264484334118713, -2.638427012816827677 ) ) ;
#39064 = CARTESIAN_POINT ( 'NONE',  ( 19.84674366389459266, 43.71726448433410894, -2.638427012816827677 ) ) ;
#39065 = ORIENTED_EDGE ( 'NONE', *, *, #8766, .T. ) ;
#39066 = ORIENTED_EDGE ( 'NONE', *, *, #83639, .T. ) ;
#39067 = DIRECTION ( 'NONE',  ( -0.000000000000000000, -1.000000000000000000, -0.000000000000000000 ) ) ;
#39068 = DIRECTION ( 'NONE',  ( 0.000000000000000000, 1.000000000000000000, 0.000000000000000000 ) ) ;
#39069 = CARTESIAN_POINT ( 'NONE',  ( -2.266590686148945544, 7.220415501580634832, 7.082119434687048631 ) ) ;
#39070 = CARTESIAN_POINT ( 'NONE',  ( 22.26659068614894466, 23.88708216824730357, 7.082119434687054849 ) ) ;
#39071 = DIRECTION ( 'NONE',  ( 0.000000000000000000, 0.000000000000000000, 1.000000000000000000 ) ) ;
#39073 = CARTESIAN_POINT ( 'NONE',  ( 17.96484262340118221, 61.18868534415482685, -7.964842623401177768 ) ) ;
#39072 = DIRECTION ( 'NONE',  ( 0.5075383629607025382, 0.000000000000000000, -0.8616291604415267091 ) ) ;
#39074 = CARTESIAN_POINT ( 'NONE',  ( 2.035157376598822676, 27.43868534415483396, -7.964842623401177768 ) ) ;
#39075 = ORIENTED_EDGE ( 'NONE', *, *, #10286, .T. ) ;
#39076 = CARTESIAN_POINT ( 'NONE',  ( 12.63842701281683034, 7.467264484334118713, 9.846743663894596210 ) ) ;
#39077 = CARTESIAN_POINT ( 'NONE',  ( 1.472469842513823179, 5.592264484334118713, -4.923371831947296329 ) ) ;
#39078 = CARTESIAN_POINT ( 'NONE',  ( 21.09922568453594849, 26.20696800326375353, 6.408140936763242479 ) ) ;
#39079 = CARTESIAN_POINT ( 'NONE',  ( 17.20831665107776587, 27.88393115100078390, 7.208316651077764980 ) ) ;
#39080 = CARTESIAN_POINT ( 'NONE',  ( -7.749999999999996447, 83.99999999999994316, -3.750000000000000000 ) ) ;
#39081 = CARTESIAN_POINT ( 'NONE',  ( 22.81628187352647785, 16.62363466993042138, 6.195893100308588602E-16 ) ) ;
#39082 = CARTESIAN_POINT ( 'NONE',  ( 8.879999999999991900, 27.04366094290857347, -2.900000000000000799 ) ) ;
#39083 = ADVANCED_FACE ( 'NONE', ( #74350 ), #94434, .T. ) ;
#39084 = CARTESIAN_POINT ( 'NONE',  ( 10.00000000000000178, 7.258931151000785675, 9.846743663894594434 ) ) ;
#39085 = COLOUR_RGB ( '', 0.66274510, 0.83137255, 0.94901961) ;
#39086 = ORIENTED_EDGE ( 'NONE', *, *, #26992, .F. ) ;
#39087 = AXIS2_PLACEMENT_3D ( 'NONE', #72888, #95911, #12392 ) ;
#39088 = EDGE_CURVE ( 'NONE', #16656, #80097, #5876, .T. ) ;
#39089 = CARTESIAN_POINT ( 'NONE',  ( 19.42250999205614548, 20.98035201082150891, -5.440088680355545492 ) ) ;
#39090 = CARTESIAN_POINT ( 'NONE',  ( -0.3689425029237881626, 27.42874883491397142, 10.36894250292379027 ) ) ;
#39091 = CARTESIAN_POINT ( 'NONE',  ( 18.52753015748617571, 43.09226448433412315, 4.923371831947298993 ) ) ;
#39092 = CARTESIAN_POINT ( 'NONE',  ( 2.035157376598822676, 67.43868534415484817, -7.964842623401177768 ) ) ;
#39094 = CARTESIAN_POINT ( 'NONE',  ( 13.03370038005726705, 15.00000000000000000, -9.273621236547697322 ) ) ;
#39093 = CARTESIAN_POINT ( 'NONE',  ( 21.09922568453595559, 47.04030133659708923, -6.408140936763230044 ) ) ;
#39095 = CARTESIAN_POINT ( 'NONE',  ( -0.8801773607111009756, 23.06368534415484106, 1.068504757029289695E-15 ) ) ;
#39096 = CARTESIAN_POINT ( 'NONE',  ( 5.129999999999991900, 76.07179676972444327, -6.500000000000000888 ) ) ;
#39097 = CARTESIAN_POINT ( 'NONE',  ( 22.81628187352648496, 11.83196800326375531, -3.434112377981050290 ) ) ;
#39098 = CARTESIAN_POINT ( 'NONE',  ( 3.591859063236761518, 14.95696800326375531, 11.09922568453594849 ) ) ;
#39099 = CARTESIAN_POINT ( 'NONE',  ( 12.63842701281683034, 47.46726448433412315, 9.846743663894596210 ) ) ;
#39100 = CARTESIAN_POINT ( 'NONE',  ( -10.88017736071110164, -2.144647989178493308, -2.915334737309917212 ) ) ;
#39101 = CARTESIAN_POINT ( 'NONE',  ( 6.565887622018943937, 45.16530133659708923, 12.81628187352647430 ) ) ;
#39102 = VECTOR ( 'NONE', #33267, 1000.000000000000000 ) ;
#39103 = SURFACE_STYLE_USAGE ( .BOTH. , #78567 ) ;
#39105 = CARTESIAN_POINT ( 'NONE',  ( 19.80832241502127644, 9.758688159020689312, 6.499999999999999112 ) ) ;
#39104 = CARTESIAN_POINT ( 'NONE',  ( 7.084665262690076126, 47.02201867748818387, -10.88017736071110164 ) ) ;
#39106 = DIRECTION ( 'NONE',  ( 0.000000000000000000, -1.000000000000000000, 0.000000000000000000 ) ) ;
#39107 = B_SPLINE_CURVE_WITH_KNOTS ( 'NONE', 3,
 ( #79317, #78826, #10336, #71816, #33786, #64292 ),
 .UNSPECIFIED., .F., .F.,
 ( 4, 2, 4 ),
 ( 3.409110551496112395E-05, 0.0004400426677367850537, 0.0008459942299586089903 ),
 .UNSPECIFIED. ) ;
#39108 = CARTESIAN_POINT ( 'NONE',  ( 18.61655166652077042, 29.87718327197428891, 6.499999999999981348 ) ) ;
#39109 = CARTESIAN_POINT ( 'NONE',  ( -0.8801773607111009756, 53.06368534415484106, 1.068504757029289695E-15 ) ) ;
#39110 = CARTESIAN_POINT ( 'NONE',  ( 0.5774900079438590739, 47.64701867748817676, -5.440088680355550821 ) ) ;
#39111 = LINE ( 'NONE', #94554, #20116 ) ;
#39112 = VECTOR ( 'NONE', #12764, 1000.000000000000000 ) ;
#39113 = CARTESIAN_POINT ( 'NONE',  ( 10.00000000000000178, 69.31368534415484817, 10.88017736071110342 ) ) ;
#39114 = CARTESIAN_POINT ( 'NONE',  ( 19.84674366389459266, 48.71726448433413026, -2.638427012816827677 ) ) ;
#39116 = CARTESIAN_POINT ( 'NONE',  ( 9.402796353261127393, 0.5000000000000004441, -11.68706210897757103 ) ) ;
#39115 = CARTESIAN_POINT ( 'NONE',  ( 0.5774900079438590739, 22.64701867748817321, -5.440088680355550821 ) ) ;
#39117 = CARTESIAN_POINT ( 'NONE',  ( 10.00000000000000000, 27.87363466993042138, -12.81628187352647608 ) ) ;
#39118 = ORIENTED_EDGE ( 'NONE', *, *, #87589, .T. ) ;
#39119 = CARTESIAN_POINT ( 'NONE',  ( 15.44008868035555260, 39.73035201082150536, 9.422509992056143702 ) ) ;
#39120 = B_SPLINE_CURVE_WITH_KNOTS ( 'NONE', 3,
 ( #79621, #36083, #42125, #4125, #51086, #80606 ),
 .UNSPECIFIED., .F., .F.,
 ( 4, 2, 4 ),
 ( 0.000000000000000000, 0.0008870672566257227975, 0.001774134513251445595 ),
 .UNSPECIFIED. ) ;
#39122 = CARTESIAN_POINT ( 'NONE',  ( 8.879999999999991900, 27.04366094290857703, 2.958578643762690863 ) ) ;
#39121 = CARTESIAN_POINT ( 'NONE',  ( 16.40814093676323893, 10.79030133659708923, 11.09922568453595026 ) ) ;
#39123 = EDGE_CURVE ( 'NONE', #88822, #44602, #16334, .T. ) ;
#39124 = CARTESIAN_POINT ( 'NONE',  ( 7.084665262690076126, 9.105352010821503583, 10.88017736071109987 ) ) ;
#39125 = CARTESIAN_POINT ( 'NONE',  ( 12.91533473730993009, 26.60535201082150536, -10.88017736071109987 ) ) ;
#39126 = CARTESIAN_POINT ( 'NONE',  ( 13.79529636645031943, 35.34541550158063927, -14.16423886937409904 ) ) ;
#39127 = CARTESIAN_POINT ( 'NONE',  ( 0.1532563361054083140, 21.00893115100078745, 1.131784320476157264E-15 ) ) ;
#39128 = CARTESIAN_POINT ( 'NONE',  ( 4.559911319644449179, 58.89701867748817676, 9.422509992056141925 ) ) ;
#39129 = CARTESIAN_POINT ( 'NONE',  ( -14.03351048042393856, 15.00000000000000000, -2.474486531753901541 ) ) ;
#39130 = CARTESIAN_POINT ( 'NONE',  ( 20.36894250292379382, 8.678748834913967869, 10.36894250292379205 ) ) ;
#39131 = MECHANICAL_DESIGN_GEOMETRIC_PRESENTATION_REPRESENTATION (  '', ( #67823 ), #23147 ) ;
#39132 = DIRECTION ( 'NONE',  ( 0.9969173337331289630, 0.000000000000000000, -0.07845909572783234254 ) ) ;
#39133 = CARTESIAN_POINT ( 'NONE',  ( 12.63842701281683922, 59.55059781766744464, -9.846743663894590881 ) ) ;
#39134 = ORIENTED_EDGE ( 'NONE', *, *, #82857, .T. ) ;
#39135 = CARTESIAN_POINT ( 'NONE',  ( -0.3689425029237881626, 32.42874883491395366, 10.36894250292379027 ) ) ;
#39136 = CARTESIAN_POINT ( 'NONE',  ( 6.204703633549690345, 30.76208216824730357, -14.16423886937410259 ) ) ;
#39137 = CARTESIAN_POINT ( 'NONE',  ( 12.63842701281683922, 4.550597817667451750, -9.846743663894590881 ) ) ;
#39138 = CARTESIAN_POINT ( 'NONE',  ( 10.00000000000000000, 64.75893115100078035, -9.846743663894594434 ) ) ;
#39139 = CARTESIAN_POINT ( 'NONE',  ( -9.206628575834976402, -19.70849028575129935, 3.750000000000000000 ) ) ;
#39141 = CARTESIAN_POINT ( 'NONE',  ( 0.6178305044545818747, 13.49863466993041783, -9.382169495545419124 ) ) ;
#39140 = CARTESIAN_POINT ( 'NONE',  ( 4.559911319644449179, 63.89701867748817676, 9.422509992056141925 ) ) ;
#39142 = CARTESIAN_POINT ( 'NONE',  ( -4.164238869374098151, 36.59541550158063217, -3.795296366450310543 ) ) ;
#39143 = CARTESIAN_POINT ( 'NONE',  ( -0.8801773607111008646, 23.27201867748817676, 2.915334737309923430 ) ) ;
#39144 = CARTESIAN_POINT ( 'NONE',  ( 20.88017736071110875, 30.77201867748816966, -2.915334737309920765 ) ) ;
#39145 = CARTESIAN_POINT ( 'NONE',  ( 20.24186590665275176, 4.734100856612036168, 6.114288769123088052 ) ) ;
#39146 = CARTESIAN_POINT ( 'NONE',  ( 2.035157376598824452, 58.68868534415482685, 7.964842623401179544 ) ) ;
#39147 = B_SPLINE_CURVE_WITH_KNOTS ( 'NONE', 3,
 ( #52578, #90573, #53069, #89101, #14609, #20614 ),
 .UNSPECIFIED., .F., .F.,
 ( 4, 2, 4 ),
 ( 0.000000000000000000, 0.0003802939046624577652, 0.0007605878093249155304 ),
 .UNSPECIFIED. ) ;
#39148 = CARTESIAN_POINT ( 'NONE',  ( 4.923371831947295441, -10.65773551566587329, -8.527530157486179263 ) ) ;
#39149 = VERTEX_POINT ( 'NONE', #22861 ) ;
#39150 = CARTESIAN_POINT ( 'NONE',  ( 20.15039907845753930, 0.07447313448805115144, 6.262539305110068177 ) ) ;
#39151 = ORIENTED_EDGE ( 'NONE', *, *, #96468, .F. ) ;
#39152 = PRESENTATION_STYLE_ASSIGNMENT (( #32109 ) ) ;
#39153 = VERTEX_POINT ( 'NONE', #54314 ) ;
#39154 = CARTESIAN_POINT ( 'NONE',  ( -2.266590686148945544, 6.387082168247300906, -7.082119434687050408 ) ) ;
#39156 = CARTESIAN_POINT ( 'NONE',  ( 0.5774900079438590739, 2.647018677488171434, -5.440088680355550821 ) ) ;
#39155 = CARTESIAN_POINT ( 'NONE',  ( 22.26659068614895176, 59.72041550158063927, -7.082119434687042414 ) ) ;
#39158 = CARTESIAN_POINT ( 'NONE',  ( 0.1532563361054100626, 65.80059781766745175, -2.638427012816831230 ) ) ;
#39157 = CARTESIAN_POINT ( 'NONE',  ( 5.076628168052703671, 31.84226448433412315, 8.527530157486179263 ) ) ;
#39159 = DIRECTION ( 'NONE',  ( 0.000000000000000000, 1.000000000000000000, 0.000000000000000000 ) ) ;
#39160 = AXIS2_PLACEMENT_3D ( 'NONE', #57739, #72734, #44216 ) ;
#39162 = CARTESIAN_POINT ( 'NONE',  ( 22.81628187352647785, 6.415301336597088344, 3.434112377981063169 ) ) ;
#39161 = MECHANICAL_DESIGN_GEOMETRIC_PRESENTATION_REPRESENTATION (  '', ( #32719 ), #45497 ) ;
#39163 = ORIENTED_EDGE ( 'NONE', *, *, #53520, .T. ) ;
#39164 =( BOUNDED_SURFACE ( )  B_SPLINE_SURFACE ( 1, 2, ( 
 ( #40054, #8573, #38582, #47048, #23596, #45582, #22601, #91582, #53569, #84082, #68589, #93045, #92549, #119, #15597, #46080, #69080, #77544, #61560, #31060, #84574, #85557, #83589, #7606, #17069, #615, #24078, #54060, #39077, #62539, #54545, #69571, #1090, #31552, #16573, #47552, #78049, #9551, #85062, #55039, #9062, #32035, #39575, #70064, #1586, #70553, #79530, #88001, #34005, #19028, #26041, #40553, #19514, #25557, #18533, #49505, #63528, #80010, #86541, #64009, #49024, #87515, #71053, #87021, #17564, #2576, #26516, #95008, #50011, #33032, #11515, #48525, #94036, #42512, #95515, #41549, #33512, #80514, #10054, #11030, #12013, #57013, #57505, #10539, #79027, #72014, #41049, #94522, #56049, #18048, #32541, #34497, #56532, #42038, #3544, #71548, #64502, #72502, #3058, #4034, #64988, #27008, #72996, #25069, #63041, #93538, #55552, #86053, #48030, #78543, #28971, #5510, #5011, #43972, #51989, #66488, #97015, #82974, #59965, #66985, #73484, #59474, #97506, #88498, #28493, #5999, #89975, #81982, #14492, #74974, #4526, #67482, #34989, #80999, #74474, #13493, #21492, #43001, #65990, #96517, #58986, #6479, #20504, #43484, #82477, #35495, #20999, #90457, #65493, #44475, #21994, #44964, #12988, #89489, #51487, #96013, #36983, #27498, #36493, #27990, #13997, #98004, #73985, #58485, #57992, #52470, #35986, #20001, #50502, #88998, #29457, #12502, #50990, #81484, #92433, #53950, #8936, #68474, #91457, #76940, #98989, #84458, #23957, #38469, #68962, #54919, #31917, #38956, #45460, #31428, #69448, #60463, #494, #8449, #968, #15956, #85434, #46929, #75468, #39453, #6983, #52957, #46449, #61932, #54431, #14989, #37983, #30447, #30942, #77422, #22983, #15483, #84940, #75959, #91946, #62418, #37488, #16451, #92922, #16943, #83957, #61440, #23477, #67977, #69945, #98502, #1465, #60948, #24453, #29957, #45966, #7487, #90951, #22483, #76456, #83468, #53448, #7971, #40931, #47426, #40439, #70939, #64385, #25918, #79891, #2456, #63412, #48900, #32912, #56420, #33392, #33880, #78418, #94895, #93917, #78914, #63890, #3420, #85935, #2944, #32421, #17446, #41436, #10913, #64869, #47912, #26393, #25444, #9935, #57388, #11399, #86905, #48411, #95391, #24945, #94404, #26893, #71897, #72383, #55927, #86426, #18415, #17927, #10424, #55428, #71429, #77926, #49391, #79413, #56893, #87397, #18914, #41922, #3912, #34380, #87879, #9433, #39936, #70438, #1957, #62922, #93423, #74856, #67359, #96895, #88384, #43852, #20385, #19883, #58862, #49882, #95902, #89366, #28372, #36368, #57873, #80883, #12381, #73865, #21370, #35377, #58356, #74346, #50374, #35869 ),
 ( #42886, #5874, #50876, #88877, #43366, #44351, #80394, #42398, #6357, #73369, #51369, #4896, #65868, #51866, #13367, #65372, #4411, #20877, #66862, #36867, #97884, #29344, #96395, #82350, #27871, #89854, #11897, #72876, #81369, #66358, #81856, #59846, #97381, #28848, #12867, #27382, #19396, #5394, #59351, #34878, #13871, #31314, #90335, #60345, #38840, #52352, #53331, #15365, #84348, #82850, #68846, #379, #61326, #23846, #15849, #30827, #37369, #856, #61816, #76820, #90838, #7852, #8337, #38352, #76336, #68357, #91837, #23354, #53836, #46335, #22367, #92321, #21874, #69332, #6858, #52840, #14371, #30331, #44838, #75345, #22859, #45850, #67861, #98381, #29837, #83349, #83840, #7363, #14872, #45343, #75844, #37863, #98875, #60832, #91335, #43199, #89198, #13199, #5710, #97717, #59184, #66188, #96223, #21703, #67695, #22196, #20710, #36199, #66696, #60174, #14200, #90670, #97224, #5223, #44179, #43692, #51202, #81205, #35195, #98207, #81685, #80715, #12211, #20207, #74180, #42718, #73689, #35703, #29180, #89688, #44681, #96722, #28198, #82184, #58694, #21203, #28691, #67192, #12705, #59680, #51702, #13695, #74688, #36703, #50712, #6199, #65698, #90173, #52188, #82682, #29665, #75177, #6688, #37206, #73199, #4730, #27702, #58187, #88699, #79172, #95151, #57155, #19166, #73133, #4174, #26661, #10201, #19656, #50147, #65140, #25702, #34147, #95661, #64641, #3686, #64152, #87653, #49645, #80152, #42177, #63666, #12151, #42658, #34644, #86195, #2720, #72641, #71681, #80657, #88144, #41201, #33657, #27146, #4674, #94671, #57648, #94171, #17707, #63176, #11664, #3191, #93685, #49170, #25218, #55699, #56192, #26180, #56671, #87160, #48178, #41688, #48671, #78690, #18685, #40694, #71196, #79672, #11169, #33173, #72158, #86686, #18190, #10688, #22512, #83002, #23010, #68006, #90001, #96159, #6504, #67509, #38008, #14520, #91977, #84486, #15017, #37012, #60977, #37514, #98028, #75988, #83988, #98532, #29985, #15987, #23506, #29, #29483, #91490, #30476, #21518, #60490, #68501, #53478, #45486, #46474, #7998, #35135, #526, #65636, #14021, #7517, #15513, #45995, #75002, #59991, #90485, #90979, #38496, #52495, #75497, #76484, #22021, #52984, #53977, #28993, #68991, #76970, #59504, #44989, #83499, #30973, #52014, #61470, #82503, #44501, #7008, #70967, #70465, #16977, #8968, #61962, #25946, #77956, #48929, #8483, #46960, #1987, #38988, #1493, #31946, #25475, #85965, #40960, #62447, #24485, #9963, #92950, #17473, #93452, #93948, #39484, #55957, #54948, #39964, #24977, #63441, #77454, #62949, #92461, #69974, #2487, #32940, #56448, #85465 ) ),
 .UNSPECIFIED., .F., .F., .F. ) 
 B_SPLINE_SURFACE_WITH_KNOTS ( ( 2, 2 ),
 ( 3, 2, 2, 2, 2, 2, 2, 2, 2, 2, 2, 2, 2, 2, 2, 2, 2, 2, 2, 2, 2, 2, 2, 2, 2, 2, 2, 2, 2, 2, 2, 2, 2, 2, 2, 2, 2, 2, 2, 2, 2, 2, 2, 2, 2, 2, 2, 2, 2, 2, 2, 2, 2, 2, 2, 2, 2, 2, 2, 2, 2, 2, 2, 2, 2, 2, 2, 2, 2, 2, 2, 2, 2, 2, 2, 2, 2, 2, 2, 2, 2, 2, 2, 2, 2, 2, 2, 2, 2, 2, 2, 2, 2, 2, 2, 2, 2, 2, 2, 2, 2, 2, 2, 2, 2, 2, 2, 2, 2, 2, 2, 2, 2, 2, 2, 2, 2, 2, 2, 2, 2, 2, 2, 2, 2, 2, 2, 2, 2, 2, 2, 2, 2, 2, 2, 2, 2, 2, 2, 2, 2, 2, 2, 2, 2, 2, 2, 2, 2, 2, 2, 2, 2, 2, 2, 2, 2, 2, 2, 2, 2, 2, 3 ),
 ( 0.000000000000000000, 1.000000000000000000 ),
 ( 0.000000000000000000, 0.005952380952380952051, 0.01190476190476190410, 0.01785714285714285615, 0.02380952380952380820, 0.02976190476190476025, 0.03571428571428571230, 0.04166666666666666435, 0.04761904761904761640, 0.05357142857142856845, 0.05952380952380952051, 0.06547619047619047949, 0.07142857142857142461, 0.07738095238095238360, 0.08333333333333332871, 0.08928571428571428770, 0.09523809523809523281, 0.1011904761904761918, 0.1071428571428571369, 0.1130952380952380959, 0.1190476190476190410, 0.1250000000000000000, 0.1309523809523809590, 0.1369047619047619180, 0.1428571428571428492, 0.1488095238095238082, 0.1547619047619047672, 0.1607142857142857262, 0.1666666666666666574, 0.1726190476190476164, 0.1785714285714285754, 0.1845238095238095344, 0.1904761904761904656, 0.1964285714285714246, 0.2023809523809523836, 0.2083333333333333426, 0.2142857142857142738, 0.2202380952380952328, 0.2261904761904761918, 0.2321428571428571508, 0.2380952380952380820, 0.2440476190476190410, 0.2500000000000000000, 0.2559523809523809312, 0.2619047619047619180, 0.2678571428571428492, 0.2738095238095238360, 0.2797619047619047672, 0.2857142857142856984, 0.2916666666666666852, 0.2976190476190476164, 0.3035714285714285476, 0.3095238095238095344, 0.3154761904761904656, 0.3214285714285714524, 0.3273809523809523836, 0.3333333333333333148, 0.3392857142857143016, 0.3452380952380952328, 0.3511904761904761640, 0.3571428571428571508, 0.3630952380952380820, 0.3690476190476190688, 0.3750000000000000000, 0.3809523809523809312, 0.3869047619047619180, 0.3928571428571428492, 0.3988095238095238360, 0.4047619047619047672, 0.4107142857142856984, 0.4166666666666666852, 0.4226190476190476164, 0.4285714285714285476, 0.4345238095238095344, 0.4404761904761904656, 0.4464285714285714524, 0.4523809523809523836, 0.4583333333333333148, 0.4642857142857143016, 0.4702380952380952328, 0.4761904761904761640, 0.4821428571428571508, 0.4880952380952380820, 0.4940476190476190688, 0.5000000000000000000, 0.5059523809523809312, 0.5119047619047618625, 0.5178571428571429047, 0.5238095238095238360, 0.5297619047619047672, 0.5357142857142856984, 0.5416666666666666297, 0.5476190476190476719, 0.5535714285714286031, 0.5595238095238095344, 0.5654761904761904656, 0.5714285714285713969, 0.5773809523809523281, 0.5833333333333333703, 0.5892857142857143016, 0.5952380952380952328, 0.6011904761904761640, 0.6071428571428570953, 0.6130952380952381375, 0.6190476190476190688, 0.6250000000000000000, 0.6309523809523809312, 0.6369047619047618625, 0.6428571428571429047, 0.6488095238095238360, 0.6547619047619047672, 0.6607142857142856984, 0.6666666666666666297, 0.6726190476190476719, 0.6785714285714286031, 0.6845238095238095344, 0.6904761904761904656, 0.6964285714285713969, 0.7023809523809523281, 0.7083333333333333703, 0.7142857142857143016, 0.7202380952380952328, 0.7261904761904761640, 0.7321428571428570953, 0.7380952380952381375, 0.7440476190476190688, 0.7500000000000000000, 0.7559523809523809312, 0.7619047619047618625, 0.7678571428571429047, 0.7738095238095238360, 0.7797619047619047672, 0.7857142857142856984, 0.7916666666666666297, 0.7976190476190476719, 0.8035714285714286031, 0.8095238095238095344, 0.8154761904761904656, 0.8214285714285713969, 0.8273809523809523281, 0.8333333333333333703, 0.8392857142857143016, 0.8452380952380952328, 0.8511904761904761640, 0.8571428571428570953, 0.8630952380952381375, 0.8690476190476190688, 0.8750000000000000000, 0.8809523809523809312, 0.8869047619047618625, 0.8928571428571429047, 0.8988095238095238360, 0.9047619047619047672, 0.9107142857142856984, 0.9166666666666666297, 0.9226190476190476719, 0.9285714285714286031, 0.9345238095238095344, 0.9404761904761904656, 0.9464285714285713969, 0.9523809523809523281, 0.9583333333333333703, 0.9642857142857143016 ),
 .UNSPECIFIED. ) 
 GEOMETRIC_REPRESENTATION_ITEM ( )  RATIONAL_B_SPLINE_SURFACE ( (
 ( 1.000000000000000000, 0.9659258262890683122, 1.000000000000000000, 0.9659258262890683122, 1.000000000000000000, 0.9659258262890683122, 1.000000000000000000, 0.9659258262890683122, 1.000000000000000000, 0.9659258262890683122, 1.000000000000000000, 0.9659258262890683122, 1.000000000000000000, 0.9659258262890683122, 1.000000000000000000, 0.9659258262890683122, 1.000000000000000000, 0.9659258262890683122, 1.000000000000000000, 0.9659258262890683122, 1.000000000000000000, 0.9659258262890683122, 1.000000000000000000, 0.9659258262890683122, 1.000000000000000000, 0.9659258262890683122, 1.000000000000000000, 0.9659258262890683122, 1.000000000000000000, 0.9659258262890683122, 1.000000000000000000, 0.9659258262890683122, 1.000000000000000000, 0.9659258262890683122, 1.000000000000000000, 0.9659258262890683122, 1.000000000000000000, 0.9659258262890683122, 1.000000000000000000, 0.9659258262890683122, 1.000000000000000000, 0.9659258262890683122, 1.000000000000000000, 0.9659258262890683122, 1.000000000000000000, 0.9659258262890683122, 1.000000000000000000, 0.9659258262890683122, 1.000000000000000000, 0.9659258262890683122, 1.000000000000000000, 0.9659258262890683122, 1.000000000000000000, 0.9659258262890683122, 1.000000000000000000, 0.9659258262890683122, 1.000000000000000000, 0.9659258262890683122, 1.000000000000000000, 0.9659258262890683122, 1.000000000000000000, 0.9659258262890683122, 1.000000000000000000, 0.9659258262890683122, 1.000000000000000000, 0.9659258262890683122, 1.000000000000000000, 0.9659258262890683122, 1.000000000000000000, 0.9659258262890683122, 1.000000000000000000, 0.9659258262890683122, 1.000000000000000000, 0.9659258262890683122, 1.000000000000000000, 0.9659258262890683122, 1.000000000000000000, 0.9659258262890683122, 1.000000000000000000, 0.9659258262890683122, 1.000000000000000000, 0.9659258262890683122, 1.000000000000000000, 0.9659258262890683122, 1.000000000000000000, 0.9659258262890683122, 1.000000000000000000, 0.9659258262890683122, 1.000000000000000000, 0.9659258262890683122, 1.000000000000000000, 0.9659258262890683122, 1.000000000000000000, 0.9659258262890683122, 1.000000000000000000, 0.9659258262890683122, 1.000000000000000000, 0.9659258262890683122, 1.000000000000000000, 0.9659258262890683122, 1.000000000000000000, 0.9659258262890683122, 1.000000000000000000, 0.9659258262890683122, 1.000000000000000000, 0.9659258262890683122, 1.000000000000000000, 0.9659258262890683122, 1.000000000000000000, 0.9659258262890683122, 1.000000000000000000, 0.9659258262890683122, 1.000000000000000000, 0.9659258262890683122, 1.000000000000000000, 0.9659258262890683122, 1.000000000000000000, 0.9659258262890683122, 1.000000000000000000, 0.9659258262890683122, 1.000000000000000000, 0.9659258262890683122, 1.000000000000000000, 0.9659258262890683122, 1.000000000000000000, 0.9659258262890683122, 1.000000000000000000, 0.9659258262890683122, 1.000000000000000000, 0.9659258262890683122, 1.000000000000000000, 0.9659258262890683122, 1.000000000000000000, 0.9659258262890683122, 1.000000000000000000, 0.9659258262890683122, 1.000000000000000000, 0.9659258262890683122, 1.000000000000000000, 0.9659258262890683122, 1.000000000000000000, 0.9659258262890683122, 1.000000000000000000, 0.9659258262890683122, 1.000000000000000000, 0.9659258262890683122, 1.000000000000000000, 0.9659258262890683122, 1.000000000000000000, 0.9659258262890683122, 1.000000000000000000, 0.9659258262890683122, 1.000000000000000000, 0.9659258262890683122, 1.000000000000000000, 0.9659258262890683122, 1.000000000000000000, 0.9659258262890683122, 1.000000000000000000, 0.9659258262890683122, 1.000000000000000000, 0.9659258262890683122, 1.000000000000000000, 0.9659258262890683122, 1.000000000000000000, 0.9659258262890683122, 1.000000000000000000, 0.9659258262890683122, 1.000000000000000000, 0.9659258262890683122, 1.000000000000000000, 0.9659258262890683122, 1.000000000000000000, 0.9659258262890683122, 1.000000000000000000, 0.9659258262890683122, 1.000000000000000000, 0.9659258262890683122, 1.000000000000000000, 0.9659258262890683122, 1.000000000000000000, 0.9659258262890683122, 1.000000000000000000, 0.9659258262890683122, 1.000000000000000000, 0.9659258262890683122, 1.000000000000000000, 0.9659258262890683122, 1.000000000000000000, 0.9659258262890683122, 1.000000000000000000, 0.9659258262890683122, 1.000000000000000000, 0.9659258262890683122, 1.000000000000000000, 0.9659258262890683122, 1.000000000000000000, 0.9659258262890683122, 1.000000000000000000, 0.9659258262890683122, 1.000000000000000000, 0.9659258262890683122, 1.000000000000000000, 0.9659258262890683122, 1.000000000000000000, 0.9659258262890683122, 1.000000000000000000, 0.9659258262890683122, 1.000000000000000000, 0.9659258262890683122, 1.000000000000000000, 0.9659258262890683122, 1.000000000000000000, 0.9659258262890683122, 1.000000000000000000, 0.9659258262890683122, 1.000000000000000000, 0.9659258262890683122, 1.000000000000000000, 0.9659258262890683122, 1.000000000000000000, 0.9659258262890683122, 1.000000000000000000, 0.9659258262890683122, 1.000000000000000000, 0.9659258262890683122, 1.000000000000000000, 0.9659258262890683122, 1.000000000000000000, 0.9659258262890683122, 1.000000000000000000, 0.9659258262890683122, 1.000000000000000000, 0.9659258262890683122, 1.000000000000000000, 0.9659258262890683122, 1.000000000000000000, 0.9659258262890683122, 1.000000000000000000, 0.9659258262890683122, 1.000000000000000000, 0.9659258262890683122, 1.000000000000000000, 0.9659258262890683122, 1.000000000000000000, 0.9659258262890683122, 1.000000000000000000, 0.9659258262890683122, 1.000000000000000000, 0.9659258262890683122, 1.000000000000000000, 0.9659258262890683122, 1.000000000000000000, 0.9659258262890683122, 1.000000000000000000, 0.9659258262890683122, 1.000000000000000000, 0.9659258262890683122, 1.000000000000000000, 0.9659258262890683122, 1.000000000000000000, 0.9659258262890683122, 1.000000000000000000, 0.9659258262890683122, 1.000000000000000000, 0.9659258262890683122, 1.000000000000000000, 0.9659258262890683122, 1.000000000000000000, 0.9659258262890683122, 1.000000000000000000, 0.9659258262890683122, 1.000000000000000000, 0.9659258262890683122, 1.000000000000000000, 0.9659258262890683122, 1.000000000000000000, 0.9659258262890683122, 1.000000000000000000, 0.9659258262890683122, 1.000000000000000000, 0.9659258262890683122, 1.000000000000000000, 0.9659258262890683122, 1.000000000000000000, 0.9659258262890683122, 1.000000000000000000, 0.9659258262890683122, 1.000000000000000000, 0.9659258262890683122, 1.000000000000000000, 0.9659258262890683122, 1.000000000000000000, 0.9659258262890683122, 1.000000000000000000, 0.9659258262890683122, 1.000000000000000000, 0.9659258262890683122, 1.000000000000000000, 0.9659258262890683122, 1.000000000000000000, 0.9659258262890683122, 1.000000000000000000, 0.9659258262890683122, 1.000000000000000000, 0.9659258262890683122, 1.000000000000000000, 0.9659258262890683122, 1.000000000000000000, 0.9659258262890683122, 1.000000000000000000, 0.9659258262890683122, 1.000000000000000000, 0.9659258262890683122, 1.000000000000000000, 0.9659258262890683122, 1.000000000000000000, 0.9659258262890683122, 1.000000000000000000, 0.9659258262890683122, 1.000000000000000000, 0.9659258262890683122, 1.000000000000000000, 0.9659258262890683122, 1.000000000000000000),
 ( 1.000000000000000000, 0.9659258262890683122, 1.000000000000000000, 0.9659258262890683122, 1.000000000000000000, 0.9659258262890683122, 1.000000000000000000, 0.9659258262890683122, 1.000000000000000000, 0.9659258262890683122, 1.000000000000000000, 0.9659258262890683122, 1.000000000000000000, 0.9659258262890683122, 1.000000000000000000, 0.9659258262890683122, 1.000000000000000000, 0.9659258262890683122, 1.000000000000000000, 0.9659258262890683122, 1.000000000000000000, 0.9659258262890683122, 1.000000000000000000, 0.9659258262890683122, 1.000000000000000000, 0.9659258262890683122, 1.000000000000000000, 0.9659258262890683122, 1.000000000000000000, 0.9659258262890683122, 1.000000000000000000, 0.9659258262890683122, 1.000000000000000000, 0.9659258262890683122, 1.000000000000000000, 0.9659258262890683122, 1.000000000000000000, 0.9659258262890683122, 1.000000000000000000, 0.9659258262890683122, 1.000000000000000000, 0.9659258262890683122, 1.000000000000000000, 0.9659258262890683122, 1.000000000000000000, 0.9659258262890683122, 1.000000000000000000, 0.9659258262890683122, 1.000000000000000000, 0.9659258262890683122, 1.000000000000000000, 0.9659258262890683122, 1.000000000000000000, 0.9659258262890683122, 1.000000000000000000, 0.9659258262890683122, 1.000000000000000000, 0.9659258262890683122, 1.000000000000000000, 0.9659258262890683122, 1.000000000000000000, 0.9659258262890683122, 1.000000000000000000, 0.9659258262890683122, 1.000000000000000000, 0.9659258262890683122, 1.000000000000000000, 0.9659258262890683122, 1.000000000000000000, 0.9659258262890683122, 1.000000000000000000, 0.9659258262890683122, 1.000000000000000000, 0.9659258262890683122, 1.000000000000000000, 0.9659258262890683122, 1.000000000000000000, 0.9659258262890683122, 1.000000000000000000, 0.9659258262890683122, 1.000000000000000000, 0.9659258262890683122, 1.000000000000000000, 0.9659258262890683122, 1.000000000000000000, 0.9659258262890683122, 1.000000000000000000, 0.9659258262890683122, 1.000000000000000000, 0.9659258262890683122, 1.000000000000000000, 0.9659258262890683122, 1.000000000000000000, 0.9659258262890683122, 1.000000000000000000, 0.9659258262890683122, 1.000000000000000000, 0.9659258262890683122, 1.000000000000000000, 0.9659258262890683122, 1.000000000000000000, 0.9659258262890683122, 1.000000000000000000, 0.9659258262890683122, 1.000000000000000000, 0.9659258262890683122, 1.000000000000000000, 0.9659258262890683122, 1.000000000000000000, 0.9659258262890683122, 1.000000000000000000, 0.9659258262890683122, 1.000000000000000000, 0.9659258262890683122, 1.000000000000000000, 0.9659258262890683122, 1.000000000000000000, 0.9659258262890683122, 1.000000000000000000, 0.9659258262890683122, 1.000000000000000000, 0.9659258262890683122, 1.000000000000000000, 0.9659258262890683122, 1.000000000000000000, 0.9659258262890683122, 1.000000000000000000, 0.9659258262890683122, 1.000000000000000000, 0.9659258262890683122, 1.000000000000000000, 0.9659258262890683122, 1.000000000000000000, 0.9659258262890683122, 1.000000000000000000, 0.9659258262890683122, 1.000000000000000000, 0.9659258262890683122, 1.000000000000000000, 0.9659258262890683122, 1.000000000000000000, 0.9659258262890683122, 1.000000000000000000, 0.9659258262890683122, 1.000000000000000000, 0.9659258262890683122, 1.000000000000000000, 0.9659258262890683122, 1.000000000000000000, 0.9659258262890683122, 1.000000000000000000, 0.9659258262890683122, 1.000000000000000000, 0.9659258262890683122, 1.000000000000000000, 0.9659258262890683122, 1.000000000000000000, 0.9659258262890683122, 1.000000000000000000, 0.9659258262890683122, 1.000000000000000000, 0.9659258262890683122, 1.000000000000000000, 0.9659258262890683122, 1.000000000000000000, 0.9659258262890683122, 1.000000000000000000, 0.9659258262890683122, 1.000000000000000000, 0.9659258262890683122, 1.000000000000000000, 0.9659258262890683122, 1.000000000000000000, 0.9659258262890683122, 1.000000000000000000, 0.9659258262890683122, 1.000000000000000000, 0.9659258262890683122, 1.000000000000000000, 0.9659258262890683122, 1.000000000000000000, 0.9659258262890683122, 1.000000000000000000, 0.9659258262890683122, 1.000000000000000000, 0.9659258262890683122, 1.000000000000000000, 0.9659258262890683122, 1.000000000000000000, 0.9659258262890683122, 1.000000000000000000, 0.9659258262890683122, 1.000000000000000000, 0.9659258262890683122, 1.000000000000000000, 0.9659258262890683122, 1.000000000000000000, 0.9659258262890683122, 1.000000000000000000, 0.9659258262890683122, 1.000000000000000000, 0.9659258262890683122, 1.000000000000000000, 0.9659258262890683122, 1.000000000000000000, 0.9659258262890683122, 1.000000000000000000, 0.9659258262890683122, 1.000000000000000000, 0.9659258262890683122, 1.000000000000000000, 0.9659258262890683122, 1.000000000000000000, 0.9659258262890683122, 1.000000000000000000, 0.9659258262890683122, 1.000000000000000000, 0.9659258262890683122, 1.000000000000000000, 0.9659258262890683122, 1.000000000000000000, 0.9659258262890683122, 1.000000000000000000, 0.9659258262890683122, 1.000000000000000000, 0.9659258262890683122, 1.000000000000000000, 0.9659258262890683122, 1.000000000000000000, 0.9659258262890683122, 1.000000000000000000, 0.9659258262890683122, 1.000000000000000000, 0.9659258262890683122, 1.000000000000000000, 0.9659258262890683122, 1.000000000000000000, 0.9659258262890683122, 1.000000000000000000, 0.9659258262890683122, 1.000000000000000000, 0.9659258262890683122, 1.000000000000000000, 0.9659258262890683122, 1.000000000000000000, 0.9659258262890683122, 1.000000000000000000, 0.9659258262890683122, 1.000000000000000000, 0.9659258262890683122, 1.000000000000000000, 0.9659258262890683122, 1.000000000000000000, 0.9659258262890683122, 1.000000000000000000, 0.9659258262890683122, 1.000000000000000000, 0.9659258262890683122, 1.000000000000000000, 0.9659258262890683122, 1.000000000000000000, 0.9659258262890683122, 1.000000000000000000, 0.9659258262890683122, 1.000000000000000000, 0.9659258262890683122, 1.000000000000000000, 0.9659258262890683122, 1.000000000000000000, 0.9659258262890683122, 1.000000000000000000, 0.9659258262890683122, 1.000000000000000000, 0.9659258262890683122, 1.000000000000000000, 0.9659258262890683122, 1.000000000000000000, 0.9659258262890683122, 1.000000000000000000, 0.9659258262890683122, 1.000000000000000000, 0.9659258262890683122, 1.000000000000000000, 0.9659258262890683122, 1.000000000000000000, 0.9659258262890683122, 1.000000000000000000, 0.9659258262890683122, 1.000000000000000000, 0.9659258262890683122, 1.000000000000000000, 0.9659258262890683122, 1.000000000000000000, 0.9659258262890683122, 1.000000000000000000, 0.9659258262890683122, 1.000000000000000000, 0.9659258262890683122, 1.000000000000000000, 0.9659258262890683122, 1.000000000000000000, 0.9659258262890683122, 1.000000000000000000, 0.9659258262890683122, 1.000000000000000000, 0.9659258262890683122, 1.000000000000000000, 0.9659258262890683122, 1.000000000000000000, 0.9659258262890683122, 1.000000000000000000, 0.9659258262890683122, 1.000000000000000000, 0.9659258262890683122, 1.000000000000000000, 0.9659258262890683122, 1.000000000000000000, 0.9659258262890683122, 1.000000000000000000, 0.9659258262890683122, 1.000000000000000000, 0.9659258262890683122, 1.000000000000000000, 0.9659258262890683122, 1.000000000000000000) ) ) 
 REPRESENTATION_ITEM ( '' )  SURFACE ( )  );
#39165 = CARTESIAN_POINT ( 'NONE',  ( -2.266590686148945544, 51.38708216824730357, -7.082119434687050408 ) ) ;
#39166 = CARTESIAN_POINT ( 'NONE',  ( 13.79529636645030344, 38.26208216824729647, 14.16423886937410614 ) ) ;
#39167 = EDGE_LOOP ( 'NONE', ( #47562, #26191, #78851, #6933 ) ) ;
#39168 = CARTESIAN_POINT ( 'NONE',  ( 12.91533473730992121, 19.52201867748816611, 10.88017736071110164 ) ) ;
#39169 = CARTESIAN_POINT ( 'NONE',  ( 19.38216949554541557, 52.24863466993041072, -9.382169495545420901 ) ) ;
#39170 = CARTESIAN_POINT ( 'NONE',  ( 20.88017736071110164, 30.35535201082151247, 2.915334737309930979 ) ) ;
#39171 = CARTESIAN_POINT ( 'NONE',  ( 17.20831665107776587, 52.88393115100078035, 7.208316651077764980 ) ) ;
#39172 = CARTESIAN_POINT ( 'NONE',  ( 17.96484262340118221, 26.18868534415483396, -7.964842623401177768 ) ) ;
#39173 = CARTESIAN_POINT ( 'NONE',  ( 7.361572987183169658, 59.96726448433410894, -9.846743663894592657 ) ) ;
#39174 = CARTESIAN_POINT ( 'NONE',  ( 8.629999999999995453, 43.00000000000000000, 6.250000000000000000 ) ) ;
#39175 = CARTESIAN_POINT ( 'NONE',  ( 15.44008868035555793, 26.39701867748817321, -9.422509992056140149 ) ) ;
#39176 = EDGE_CURVE ( 'NONE', #29785, #87174, #62303, .T. ) ;
#39178 = ORIENTED_EDGE ( 'NONE', *, *, #11884, .F. ) ;
#39177 = CARTESIAN_POINT ( 'NONE',  ( -9.898881779040587858, 0.000000000000000000, -10.25059215482589714 ) ) ;
#39179 = CARTESIAN_POINT ( 'NONE',  ( 4.838527690343618737, 0.5000000000000004441, -14.19819177887726624 ) ) ;
#39180 = CARTESIAN_POINT ( 'NONE',  ( 1.472469842513823179, 0.5922644843341181575, -4.923371831947296329 ) ) ;
#39181 = CARTESIAN_POINT ( 'NONE',  ( -3.500000001558553286, 0.09224605988771300558, 2.499999999999595879 ) ) ;
#39182 = EDGE_LOOP ( 'NONE', ( #68277, #36310, #37460, #79219 ) ) ;
#39183 = CARTESIAN_POINT ( 'NONE',  ( 8.705946125150790138, -3.115782928412242025, 4.000000000000000000 ) ) ;
#39184 = CARTESIAN_POINT ( 'NONE',  ( 1.472469842513823179, 25.59226448433412315, -4.923371831947296329 ) ) ;
#39185 = DIRECTION ( 'NONE',  ( 1.000000000000000000, -1.257568779154408485E-17, 0.000000000000000000 ) ) ;
#39186 = CARTESIAN_POINT ( 'NONE',  ( -2.816281873526473856, 49.12363466993042493, 9.499525473075851096E-16 ) ) ;
#39187 = FILL_AREA_STYLE_COLOUR ( '', #38807 ) ;
#39188 = CARTESIAN_POINT ( 'NONE',  ( 64.56412365047461321, 11.49999999999999467, 10.00000000000000000 ) ) ;
#39189 = ORIENTED_EDGE ( 'NONE', *, *, #19903, .T. ) ;
#39190 = LINE ( 'NONE', #37712, #69994 ) ;
#39191 = CARTESIAN_POINT ( 'NONE',  ( 0.000000000000000000, 14.49999999999999822, 0.000000000000000000 ) ) ;
#39192 = CARTESIAN_POINT ( 'NONE',  ( 1.472469842513823179, 60.59226448433412315, -4.923371831947296329 ) ) ;
#39193 = CARTESIAN_POINT ( 'NONE',  ( 2.917880565312948704, 42.63708216824729647, 12.26659068614894643 ) ) ;
#39194 = CARTESIAN_POINT ( 'NONE',  ( 19.84674366389459621, 53.50893115100078745, 7.409399052514197653E-17 ) ) ;
#39195 = PRESENTATION_STYLE_ASSIGNMENT (( #54174 ) ) ;
#39196 = CARTESIAN_POINT ( 'NONE',  ( 12.63842701281683034, 17.46726448433411250, 9.846743663894596210 ) ) ;
#39197 = CARTESIAN_POINT ( 'NONE',  ( 19.38216949554541202, 55.99863466993041072, 9.382169495545424454 ) ) ;
#39198 = AXIS2_PLACEMENT_3D ( 'NONE', #69328, #90832, #83834 ) ;
#39199 = CARTESIAN_POINT ( 'NONE',  ( 7.361572987183170547, 57.05059781766744464, 9.846743663894590881 ) ) ;
#39200 = CARTESIAN_POINT ( 'NONE',  ( 17.96484262340118221, 49.93868534415484106, 7.964842623401181321 ) ) ;
#39201 = CARTESIAN_POINT ( 'NONE',  ( 5.114679605276696073, -17.52310038222973887, -2.750000000000000444 ) ) ;
#39202 = ORIENTED_EDGE ( 'NONE', *, *, #12330, .T. ) ;
#39203 = EDGE_CURVE ( 'NONE', #83367, #77859, #7367, .T. ) ;
#39204 = TOROIDAL_SURFACE ( 'NONE', #72711, 3.799999999999998934, 0.2000000000000000111 ) ;
#39205 = CARTESIAN_POINT ( 'NONE',  ( 4.559911319644449179, 53.89701867748817676, 9.422509992056141925 ) ) ;
#39206 = ORIENTED_EDGE ( 'NONE', *, *, #25638, .T. ) ;
#39207 = ADVANCED_FACE ( 'NONE', ( #98384 ), #14373, .F. ) ;
#39208 = CARTESIAN_POINT ( 'NONE',  ( 0.3093388210927642268, 15.00000000000000000, -14.99680997725065978 ) ) ;
#39209 = CARTESIAN_POINT ( 'NONE',  ( 0.5774900079438590739, 32.64701867748816966, -5.440088680355550821 ) ) ;
#39211 = CARTESIAN_POINT ( 'NONE',  ( 2.035157376598822676, 52.43868534415483396, -7.964842623401177768 ) ) ;
#39210 = CARTESIAN_POINT ( 'NONE',  ( 21.09922568453595559, 17.04030133659708923, -6.408140936763230044 ) ) ;
#39212 = CARTESIAN_POINT ( 'NONE',  ( 0.000000000000000000, 0.000000000000000000, 0.000000000000000000 ) ) ;
#39213 = CARTESIAN_POINT ( 'NONE',  ( -42.60666666666668334, 92.50000000000000000, 9.500000000000000000 ) ) ;
#39214 = DIRECTION ( 'NONE',  ( 0.5519369853120676961, 0.000000000000000000, -0.8338858220671618859 ) ) ;
#39216 = DIRECTION ( 'NONE',  ( 0.9981347984218662539, 0.000000000000000000, 0.06104853953487057033 ) ) ;
#39215 = CARTESIAN_POINT ( 'NONE',  ( 15.44008868035555260, 39.73035201082150536, 9.422509992056143702 ) ) ;
#39217 =( GEOMETRIC_REPRESENTATION_CONTEXT ( 3 ) GLOBAL_UNCERTAINTY_ASSIGNED_CONTEXT ( ( #52133 ) ) GLOBAL_UNIT_ASSIGNED_CONTEXT ( ( #30053, #60562, #91053 ) ) REPRESENTATION_CONTEXT ( 'NONE', 'WORKASPACE' ) );
#39218 = CARTESIAN_POINT ( 'NONE',  ( 17.20831665107776587, 39.13393115100079456, -7.208316651077762316 ) ) ;
#39219 = CARTESIAN_POINT ( 'NONE',  ( 5.076628168052703671, 1.842264484334118047, 8.527530157486179263 ) ) ;
#39220 = CARTESIAN_POINT ( 'NONE',  ( 7.082119434687054849, 28.47041550158063572, 12.26659068614894288 ) ) ;
#39221 = CARTESIAN_POINT ( 'NONE',  ( -2.816281873526473856, 14.12363466993041961, 9.499525473075851096E-16 ) ) ;
#39222 = B_SPLINE_CURVE_WITH_KNOTS ( 'NONE', 3,
 ( #45440, #98481, #90434, #54411, #7467, #77404, #29440, #75448, #53430, #59944, #29937, #22462, #15939, #15466, #950, #52938, #83448, #68944 ),
 .UNSPECIFIED., .F., .F.,
 ( 4, 2, 2, 2, 2, 2, 2, 2, 4 ),
 ( 0.000000000000000000, 0.01113267275063152192, 0.02226534550126304385, 0.04453069100252608770, 0.06679603650378912461, 0.07792870925442065000, 0.08349504562973641963, 0.08627821381739429751, 0.08906138200505217539 ),
 .UNSPECIFIED. ) ;
#39223 = CARTESIAN_POINT ( 'NONE',  ( 10.00000000000000178, 19.31368534415484106, 10.88017736071110342 ) ) ;
#39224 = CARTESIAN_POINT ( 'NONE',  ( -2.266590686148945544, 21.38708216824730357, -7.082119434687050408 ) ) ;
#39225 = CARTESIAN_POINT ( 'NONE',  ( 20.36894250292379382, 58.67874883491396076, 10.36894250292379205 ) ) ;
#39226 = VECTOR ( 'NONE', #76511, 1000.000000000000000 ) ;
#39227 = CARTESIAN_POINT ( 'NONE',  ( 7.361572987183170547, 32.05059781766745175, 9.846743663894590881 ) ) ;
#39228 = CARTESIAN_POINT ( 'NONE',  ( 0.1532563361054100626, 15.80059781766745353, -2.638427012816831230 ) ) ;
#39229 = PRESENTATION_STYLE_ASSIGNMENT (( #8711 ) ) ;
#39230 = AXIS2_PLACEMENT_3D ( 'NONE', #74847, #28839, #6347 ) ;
#39231 = VERTEX_POINT ( 'NONE', #44841 ) ;
#39232 = CARTESIAN_POINT ( 'NONE',  ( 2.791683348922237240, 25.38393115100078390, -7.208316651077763204 ) ) ;
#39233 = CARTESIAN_POINT ( 'NONE',  ( 12.91533473730992121, 29.52201867748817321, 10.88017736071110164 ) ) ;
#39234 = CARTESIAN_POINT ( 'NONE',  ( 14.92337183194729988, 64.34226448433412315, -8.527530157486177487 ) ) ;
#39235 = CARTESIAN_POINT ( 'NONE',  ( -2.266590686148945544, 6.387082168247300906, -7.082119434687050408 ) ) ;
#39236 = FACE_OUTER_BOUND ( 'NONE', #13872, .T. ) ;
#39237 = UNCERTAINTY_MEASURE_WITH_UNIT (LENGTH_MEASURE( 1.000000000000000082E-05 ), #47414, 'distance_accuracy_value', 'NONE');
#39238 = CARTESIAN_POINT ( 'NONE',  ( 1.472469842513823179, 5.592264484334118713, -4.923371831947296329 ) ) ;
#39239 = CARTESIAN_POINT ( 'NONE',  ( -2.816281873526471635, 33.91530133659708213, -3.434112377981056508 ) ) ;
#39240 = CARTESIAN_POINT ( 'NONE',  ( 19.84674366389459621, 43.50893115100078745, 7.409399052514197653E-17 ) ) ;
#39241 = VERTEX_POINT ( 'NONE', #75347 ) ;
#39242 = CARTESIAN_POINT ( 'NONE',  ( 12.63842701281683034, 17.46726448433411250, 9.846743663894596210 ) ) ;
#39243 = CARTESIAN_POINT ( 'NONE',  ( 2.148416515056630338, 12.23726573380443128, 6.499999999999988454 ) ) ;
#39244 = CARTESIAN_POINT ( 'NONE',  ( 13.79529636645030344, 58.26208216824728936, 14.16423886937410614 ) ) ;
#39245 = CARTESIAN_POINT ( 'NONE',  ( 17.96484262340118221, 49.93868534415484106, 7.964842623401181321 ) ) ;
#39246 =( NAMED_UNIT ( * ) SI_UNIT ( $, .STERADIAN. ) SOLID_ANGLE_UNIT ( ) );
#39247 = CARTESIAN_POINT ( 'NONE',  ( 20.88017736071110519, 60.56368534415484106, 2.639326808657452039E-16 ) ) ;
#39248 = CARTESIAN_POINT ( 'NONE',  ( 14.92337183194729633, 37.67559781766745175, 8.527530157486181039 ) ) ;
#39249 = CARTESIAN_POINT ( 'NONE',  ( 10.00000000000000178, 14.31368534415483751, 10.88017736071110342 ) ) ;
#39250 = CARTESIAN_POINT ( 'NONE',  ( -7.684764310694718326, 14.49999999999999112, -12.88194075009952222 ) ) ;
#39251 = CARTESIAN_POINT ( 'NONE',  ( 0.1532563361054083140, 56.00893115100078745, 1.131784320476157264E-15 ) ) ;
#39252 = EDGE_CURVE ( 'NONE', #92402, #41037, #1503, .T. ) ;
#39253 = CARTESIAN_POINT ( 'NONE',  ( 15.44008868035555260, 44.73035201082151247, 9.422509992056143702 ) ) ;
#39254 = CARTESIAN_POINT ( 'NONE',  ( 0.1532563361054082862, 1.217264484334117824, 2.638427012816831674 ) ) ;
#39255 = UNCERTAINTY_MEASURE_WITH_UNIT (LENGTH_MEASURE( 1.000000000000000082E-05 ), #41171, 'distance_accuracy_value', 'NONE');
#39256 = ORIENTED_EDGE ( 'NONE', *, *, #55005, .F. ) ;
#39257 = VERTEX_POINT ( 'NONE', #7854 ) ;
#39258 = DIRECTION ( 'NONE',  ( 0.7808688094430307203, -0.6246950475544238435, 0.000000000000000000 ) ) ;
#39259 = AXIS2_PLACEMENT_3D ( 'NONE', #31932, #22124, #52603 ) ;
#39260 = CARTESIAN_POINT ( 'NONE',  ( 10.00000000000000178, 3.053748834913967425, 14.16423886937410082 ) ) ;
#39261 = CARTESIAN_POINT ( 'NONE',  ( 12.63842701281683034, 47.46726448433412315, 9.846743663894596210 ) ) ;
#39262 = CARTESIAN_POINT ( 'NONE',  ( 7.361572987183170547, 22.05059781766745530, 9.846743663894590881 ) ) ;
#39263 = CARTESIAN_POINT ( 'NONE',  ( 19.38216949554541202, 50.99863466993042493, 9.382169495545424454 ) ) ;
#39265 = CARTESIAN_POINT ( 'NONE',  ( 17.20831665107776587, 54.13393115100079456, -7.208316651077762316 ) ) ;
#39264 = CARTESIAN_POINT ( 'NONE',  ( 12.91533473730993009, 21.60535201082150536, -10.88017736071109987 ) ) ;
#39266 = CARTESIAN_POINT ( 'NONE',  ( -0.3289641300568005855, 34.27164270246084499, -5.963430220938281678 ) ) ;
#39267 = CARTESIAN_POINT ( 'NONE',  ( -4.164238869374099039, 31.80374883491396432, 8.674139862899312516E-16 ) ) ;
#39268 = CARTESIAN_POINT ( 'NONE',  ( 13.79529636645031943, 55.34541550158062506, -14.16423886937409904 ) ) ;
#39269 = CARTESIAN_POINT ( 'NONE',  ( 1.472469842513823179, 55.59226448433412315, -4.923371831947296329 ) ) ;
#39270 = CARTESIAN_POINT ( 'NONE',  ( -11.35178980618986877, 14.49999999999999112, 9.804941009311868072 ) ) ;
#39271 = CARTESIAN_POINT ( 'NONE',  ( 17.96484262340118221, 44.93868534415483396, 7.964842623401181321 ) ) ;
#39272 = CARTESIAN_POINT ( 'NONE',  ( 14.92337183194729633, 12.67559781766745353, 8.527530157486181039 ) ) ;
#39273 = CARTESIAN_POINT ( 'NONE',  ( -35.44000000000001194, 93.50000000000000000, 9.500000000000000000 ) ) ;
#39274 = VERTEX_POINT ( 'NONE', #84827 ) ;
#39275 = CARTESIAN_POINT ( 'NONE',  ( -4.838527690343713772, 15.00000000000000000, 14.19819177887723605 ) ) ;
#39276 = ORIENTED_EDGE ( 'NONE', *, *, #90103, .F. ) ;
#39277 = CARTESIAN_POINT ( 'NONE',  ( 2.791683348922237240, 15.38393115100078212, -7.208316651077763204 ) ) ;
#39278 = ORIENTED_EDGE ( 'NONE', *, *, #61432, .T. ) ;
#39279 =( GEOMETRIC_REPRESENTATION_CONTEXT ( 3 ) GLOBAL_UNCERTAINTY_ASSIGNED_CONTEXT ( ( #48325 ) ) GLOBAL_UNIT_ASSIGNED_CONTEXT ( ( #60221, #76700, #59723 ) ) REPRESENTATION_CONTEXT ( 'NONE', 'WORKASPACE' ) );
#39280 = CARTESIAN_POINT ( 'NONE',  ( 2.917880565312948704, 22.63708216824730002, 12.26659068614894643 ) ) ;
#39281 = CARTESIAN_POINT ( 'NONE',  ( 5.076628168052703671, 21.84226448433411960, 8.527530157486179263 ) ) ;
#39282 = CARTESIAN_POINT ( 'NONE',  ( 12.91533473730993009, 41.60535201082149825, -10.88017736071109987 ) ) ;
#39283 = LINE ( 'NONE', #322, #84048 ) ;
#39284 = EDGE_LOOP ( 'NONE', ( #85116, #77134, #91780, #92800 ) ) ;
#39285 = CARTESIAN_POINT ( 'NONE',  ( 20.88017736071110875, 35.77201867748816966, -2.915334737309920765 ) ) ;
#39286 = CARTESIAN_POINT ( 'NONE',  ( -4.249999999999994671, 43.00000000000000711, -6.500000000000000888 ) ) ;
#39287 = ORIENTED_EDGE ( 'NONE', *, *, #72463, .T. ) ;
#39288 = CARTESIAN_POINT ( 'NONE',  ( 10.00000000000000178, 44.31368534415484106, 10.88017736071110342 ) ) ;
#39289 = CARTESIAN_POINT ( 'NONE',  ( 22.26659068614894466, 8.887082168247300018, 7.082119434687054849 ) ) ;
#39290 = VERTEX_POINT ( 'NONE', #21876 ) ;
#39291 = EDGE_LOOP ( 'NONE', ( #42748, #46753, #8723, #36043 ) ) ;
#39292 = CARTESIAN_POINT ( 'NONE',  ( 10.00000000000000178, 15.37363466993042138, 12.81628187352647608 ) ) ;
#39293 = CARTESIAN_POINT ( 'NONE',  ( 5.076628168052704559, 15.17559781766745175, -8.527530157486179263 ) ) ;
#39294 = DIRECTION ( 'NONE',  ( 0.000000000000000000, 0.000000000000000000, -1.000000000000000000 ) ) ;
#39295 = CARTESIAN_POINT ( 'NONE',  ( 12.99999999999999822, 75.00000000000000000, 6.500000000000000888 ) ) ;
#39296 = CARTESIAN_POINT ( 'NONE',  ( 18.52753015748617571, 13.09226448433411960, 4.923371831947298993 ) ) ;
#39297 = CARTESIAN_POINT ( 'NONE',  ( 0.5774900079438607392, 28.48035201082150891, 5.440088680355550821 ) ) ;
#39298 = EDGE_CURVE ( 'NONE', #34829, #70878, #52354, .T. ) ;
#39299 = AXIS2_PLACEMENT_3D ( 'NONE', #1945, #41424, #55414 ) ;
#39300 = AXIS2_PLACEMENT_3D ( 'NONE', #34821, #64326, #2888 ) ;
#39301 = EDGE_LOOP ( 'NONE', ( #66801, #91521, #14148, #8970 ) ) ;
#39302 = DIRECTION ( 'NONE',  ( -0.000000000000000000, -1.000000000000000000, -0.000000000000000000 ) ) ;
#39303 = CARTESIAN_POINT ( 'NONE',  ( 0.5774900079438590739, 57.64701867748817676, -5.440088680355550821 ) ) ;
#39304 = VECTOR ( 'NONE', #54157, 1000.000000000000000 ) ;
#39305 = CARTESIAN_POINT ( 'NONE',  ( 21.09922568453595559, 62.04030133659709634, -6.408140936763230044 ) ) ;
#39306 = CARTESIAN_POINT ( 'NONE',  ( 4.559911319644449179, 58.89701867748817676, 9.422509992056141925 ) ) ;
#39307 = CARTESIAN_POINT ( 'NONE',  ( -1.099225684535947600, 13.70696800326375353, -6.408140936763238038 ) ) ;
#39308 = LINE ( 'NONE', #77279, #14769 ) ;
#39309 = CARTESIAN_POINT ( 'NONE',  ( 5.076628168052703671, 26.84226448433411960, 8.527530157486179263 ) ) ;
#39310 = CARTESIAN_POINT ( 'NONE',  ( 19.38216949554541557, 57.24863466993042493, -9.382169495545420901 ) ) ;
#39311 = FACE_OUTER_BOUND ( 'NONE', #19095, .T. ) ;
#39312 = CARTESIAN_POINT ( 'NONE',  ( 17.20831665107776587, 19.13393115100078035, -7.208316651077762316 ) ) ;
#39313 = CARTESIAN_POINT ( 'NONE',  ( 22.81628187352647785, 16.62363466993042138, 6.195893100308588602E-16 ) ) ;
#39314 = DIRECTION ( 'NONE',  ( -0.1496197561345335991, 0.9887436111420608853, 1.038195613746000465E-15 ) ) ;
#39315 = CARTESIAN_POINT ( 'NONE',  ( 20.88017736071110875, 50.77201867748817676, -2.915334737309920765 ) ) ;
#39316 = CARTESIAN_POINT ( 'NONE',  ( 5.076628168052704559, 60.17559781766745175, -8.527530157486179263 ) ) ;
#39317 = CARTESIAN_POINT ( 'NONE',  ( 2.791683348922237240, 25.38393115100078390, -7.208316651077763204 ) ) ;
#39318 = CARTESIAN_POINT ( 'NONE',  ( 10.00000000000000000, 11.81368534415483751, -10.88017736071110342 ) ) ;
#39319 = CARTESIAN_POINT ( 'NONE',  ( 21.09922568453594849, 16.20696800326375353, 6.408140936763242479 ) ) ;
#39320 = CARTESIAN_POINT ( 'NONE',  ( -10.80370554825985430, 89.74834511847251406, 6.353281608588779328 ) ) ;
#39321 = ADVANCED_FACE ( 'NONE', ( #46336 ), #380, .F. ) ;
#39322 = FACE_OUTER_BOUND ( 'NONE', #51887, .T. ) ;
#39323 = CARTESIAN_POINT ( 'NONE',  ( 0.5774900079438607392, 23.48035201082150536, 5.440088680355550821 ) ) ;
#39324 = ORIENTED_EDGE ( 'NONE', *, *, #18631, .T. ) ;
#39325 =( NAMED_UNIT ( * ) SI_UNIT ( $, .STERADIAN. ) SOLID_ANGLE_UNIT ( ) );
#39326 = EDGE_CURVE ( 'NONE', #63343, #25266, #33740, .T. ) ;
#39328 = CARTESIAN_POINT ( 'NONE',  ( 17.96484262340118221, 14.93868534415484106, 7.964842623401181321 ) ) ;
#39327 = CARTESIAN_POINT ( 'NONE',  ( 1.472469842513823179, 25.59226448433412315, -4.923371831947296329 ) ) ;
#39329 = CARTESIAN_POINT ( 'NONE',  ( -5.815502996285044190, 14.76930270348881002, 13.76292046016118675 ) ) ;
#39330 = B_SPLINE_CURVE_WITH_KNOTS ( 'NONE', 3,
 ( #8118, #86574, #47079, #55587, #18079, #86083 ),
 .UNSPECIFIED., .F., .F.,
 ( 4, 2, 4 ),
 ( 0.000000000000000000, 0.0002626113303184824700, 0.0005252226606369649400 ),
 .UNSPECIFIED. ) ;
#39331 = CARTESIAN_POINT ( 'NONE',  ( 2.035157376598822676, 37.43868534415484106, -7.964842623401177768 ) ) ;
#39333 = CARTESIAN_POINT ( 'NONE',  ( 1.821158202401484072, 41.16688879859522388, 6.499999999999917399 ) ) ;
#39332 = CARTESIAN_POINT ( 'NONE',  ( 10.00000000000000000, 1.813685344154838175, -10.88017736071110342 ) ) ;
#39334 = CARTESIAN_POINT ( 'NONE',  ( 2.791683348922240793, 1.633931151000784565, 7.208316651077764092 ) ) ;
#39335 = CARTESIAN_POINT ( 'NONE',  ( 0.1532563361054082862, 36.21726448433410894, 2.638427012816831674 ) ) ;
#39336 = CARTESIAN_POINT ( 'NONE',  ( -5.806645064956352797, 3.422013106907373370E-16, -13.42464971017003528 ) ) ;
#39337 = AXIS2_PLACEMENT_3D ( 'NONE', #47395, #2429, #31893 ) ;
#39338 = SURFACE_STYLE_FILL_AREA ( #46817 ) ;
#39339 = DIRECTION ( 'NONE',  ( 0.000000000000000000, 0.000000000000000000, -1.000000000000000000 ) ) ;
#39340 = CARTESIAN_POINT ( 'NONE',  ( -11.16008302858703694, -52.90628376244900011, -3.999999999996394440 ) ) ;
#39341 = CARTESIAN_POINT ( 'NONE',  ( -0.3689425029237898834, 26.17874883491396432, -10.36894250292378850 ) ) ;
#39342 = CARTESIAN_POINT ( 'NONE',  ( 2.791683348922237240, 40.38393115100078035, -7.208316651077763204 ) ) ;
#39343 = CARTESIAN_POINT ( 'NONE',  ( 19.72487221294570858, 70.00000000000000000, 6.000000000000000000 ) ) ;
#39344 = VERTEX_POINT ( 'NONE', #76822 ) ;
#39345 = CARTESIAN_POINT ( 'NONE',  ( 24.16423886937410614, 49.51208216824730357, -3.795296366450302550 ) ) ;
#39346 = CARTESIAN_POINT ( 'NONE',  ( 0.1532563361054100626, 15.80059781766745353, -2.638427012816831230 ) ) ;
#39348 = DIRECTION ( 'NONE',  ( -0.000000000000000000, -0.000000000000000000, 1.000000000000000000 ) ) ;
#39347 = SURFACE_SIDE_STYLE ('',( #31327 ) ) ;
#39349 = CARTESIAN_POINT ( 'NONE',  ( 20.88017736071110519, 40.56368534415484106, 2.639326808657452039E-16 ) ) ;
#39350 = CARTESIAN_POINT ( 'NONE',  ( 10.00000000000000000, 57.87363466993042493, -12.81628187352647608 ) ) ;
#39351 = CARTESIAN_POINT ( 'NONE',  ( 19.42250999205614193, 20.14701867748817321, 5.440088680355555262 ) ) ;
#39352 = CARTESIAN_POINT ( 'NONE',  ( 0.6178305044545818747, 53.49863466993041072, -9.382169495545419124 ) ) ;
#39353 = CARTESIAN_POINT ( 'NONE',  ( 10.00000000000000000, -2.126365330069579951, -12.81628187352647608 ) ) ;
#39354 = CARTESIAN_POINT ( 'NONE',  ( 0.6081133539230503260, 53.33703382326400799, 6.499999999999974243 ) ) ;
#39355 = ORIENTED_EDGE ( 'NONE', *, *, #53491, .F. ) ;
#39356 = CARTESIAN_POINT ( 'NONE',  ( -2.815433093577222490, 14.63595249122788999, 14.73340885523749044 ) ) ;
#39357 = CARTESIAN_POINT ( 'NONE',  ( -11.36220558718850882, 3.877685541201178108E-16, -9.008345252845398221 ) ) ;
#39358 = CARTESIAN_POINT ( 'NONE',  ( 6.204703633549690345, 52.84541550158062506, 14.16423886937410082 ) ) ;
#39359 = CARTESIAN_POINT ( 'NONE',  ( 6.204703633549690345, 10.76208216824729824, -14.16423886937410259 ) ) ;
#39360 = CARTESIAN_POINT ( 'NONE',  ( 19.42250999205614193, 25.14701867748817321, 5.440088680355555262 ) ) ;
#39361 = CARTESIAN_POINT ( 'NONE',  ( -0.8801773607110991993, 42.85535201082150536, -2.915334737309923874 ) ) ;
#39362 = CARTESIAN_POINT ( 'NONE',  ( 8.879999999999991900, 69.99999999999998579, 6.250000000000000000 ) ) ;
#39363 = DIRECTION ( 'NONE',  ( -0.9999619230641711987, 0.000000000000000000, -0.008726535498381204903 ) ) ;
#39364 = CARTESIAN_POINT ( 'NONE',  ( -0.8801773607111008646, 68.27201867748817676, 2.915334737309923430 ) ) ;
#39365 = CARTESIAN_POINT ( 'NONE',  ( -0.8801773607111009756, 68.06368534415484817, 1.068504757029289695E-15 ) ) ;
#39366 = CARTESIAN_POINT ( 'NONE',  ( 2.791683348922240793, 26.63393115100078745, 7.208316651077764092 ) ) ;
#39367 = CARTESIAN_POINT ( 'NONE',  ( 1.274849032794223680, 28.57228050351031001, 6.499999999999884537 ) ) ;
#39368 = CARTESIAN_POINT ( 'NONE',  ( -2.120353041430432128, 15.00000000000000000, -14.34413130794946234 ) ) ;
#39369 = CARTESIAN_POINT ( 'NONE',  ( 18.52753015748617571, 13.09226448433411960, 4.923371831947298993 ) ) ;
#39370 = CARTESIAN_POINT ( 'NONE',  ( 10.00000000000000178, 37.25893115100078745, 9.846743663894594434 ) ) ;
#39371 = EDGE_CURVE ( 'NONE', #98693, #43481, #59902, .T. ) ;
#39372 = CARTESIAN_POINT ( 'NONE',  ( -0.8801773607111009756, 13.06368534415483929, 1.068504757029289695E-15 ) ) ;
#39373 = AXIS2_PLACEMENT_3D ( 'NONE', #28795, #88321, #59297 ) ;
#39374 = CARTESIAN_POINT ( 'NONE',  ( -2.816281873526471635, 28.91530133659708213, -3.434112377981056508 ) ) ;
#39375 = CARTESIAN_POINT ( 'NONE',  ( 17.20831665107776587, 4.133931151000785675, -7.208316651077762316 ) ) ;
#39376 = CARTESIAN_POINT ( 'NONE',  ( 0.3093388210927633941, 0.5000000000000004441, 14.99680997725065978 ) ) ;
#39377 = AXIS2_PLACEMENT_3D ( 'NONE', #32135, #78146, #70659 ) ;
#39378 = CARTESIAN_POINT ( 'NONE',  ( 14.92337183194729633, 52.67559781766745175, 8.527530157486181039 ) ) ;
#39379 = CARTESIAN_POINT ( 'NONE',  ( 1.472469842513823179, 36.42559781766745175, 4.923371831947296329 ) ) ;
#39380 = CARTESIAN_POINT ( 'NONE',  ( 24.16423886937410614, 19.30374883491397142, 8.672049930838204340E-16 ) ) ;
#39381 = CARTESIAN_POINT ( 'NONE',  ( 4.559911319644449179, 52.23035201082151247, -9.422509992056141925 ) ) ;
#39382 = CARTESIAN_POINT ( 'NONE',  ( 19.42250999205614548, 10.98035201082150358, -5.440088680355545492 ) ) ;
#39383 = EDGE_CURVE ( 'NONE', #48651, #47034, #89651, .T. ) ;
#39384 = CARTESIAN_POINT ( 'NONE',  ( 20.88017736071110519, 40.56368534415484106, 2.639326808657452039E-16 ) ) ;
#39385 = CARTESIAN_POINT ( 'NONE',  ( 12.91533473730993009, 36.60535201082151247, -10.88017736071109987 ) ) ;
#39386 = ORIENTED_EDGE ( 'NONE', *, *, #60523, .T. ) ;
#39387 = CARTESIAN_POINT ( 'NONE',  ( 10.00000000000000000, 32.87363466993042493, -12.81628187352647608 ) ) ;
#39388 = CARTESIAN_POINT ( 'NONE',  ( 0.5774900079438607392, 38.48035201082150536, 5.440088680355550821 ) ) ;
#39389 = ORIENTED_EDGE ( 'NONE', *, *, #52221, .T. ) ;
#39390 = CARTESIAN_POINT ( 'NONE',  ( 10.00000000000000000, 52.87363466993041783, -12.81628187352647608 ) ) ;
#39391 = AXIS2_PLACEMENT_3D ( 'NONE', #5262, #6238, #11761 ) ;
#39392 = CARTESIAN_POINT ( 'NONE',  ( 2.035157376598824452, 53.68868534415484817, 7.964842623401179544 ) ) ;
#39393 = ORIENTED_EDGE ( 'NONE', *, *, #29003, .F. ) ;
#39394 = AXIS2_PLACEMENT_3D ( 'NONE', #40422, #62902, #79388 ) ;
#39395 = CARTESIAN_POINT ( 'NONE',  ( 12.91533473730992121, 49.52201867748817676, 10.88017736071110164 ) ) ;
#39396 = CARTESIAN_POINT ( 'NONE',  ( 6.934035614042552531, -73.16521313705239038, 3.999999999998390177 ) ) ;
#39397 = FACE_OUTER_BOUND ( 'NONE', #26129, .T. ) ;
#39398 = CARTESIAN_POINT ( 'NONE',  ( -1.926860441876563801, 24.89664270246083788, 3.195792623639529761 ) ) ;
#39399 = CARTESIAN_POINT ( 'NONE',  ( -4.164238869374099927, 62.01208216824728936, 3.795296366450308767 ) ) ;
#39400 = CARTESIAN_POINT ( 'NONE',  ( -0.8801773607110991993, 62.85535201082150536, -2.915334737309923874 ) ) ;
#39401 = CARTESIAN_POINT ( 'NONE',  ( 6.204703633549690345, 5.762082168247301794, -14.16423886937410259 ) ) ;
#39402 = SURFACE_STYLE_FILL_AREA ( #38415 ) ;
#39403 = CARTESIAN_POINT ( 'NONE',  ( 17.96484262340118221, 4.938685344154837509, 7.964842623401181321 ) ) ;
#39404 = CARTESIAN_POINT ( 'NONE',  ( 10.00000000000000178, 27.25893115100078390, 9.846743663894594434 ) ) ;
#39405 = ORIENTED_EDGE ( 'NONE', *, *, #56154, .T. ) ;
#39406 = CARTESIAN_POINT ( 'NONE',  ( 1.472469842513823179, 30.59226448433411960, -4.923371831947296329 ) ) ;
#39407 = CARTESIAN_POINT ( 'NONE',  ( 7.084665262690076126, 42.02201867748816966, -10.88017736071110164 ) ) ;
#39408 = CARTESIAN_POINT ( 'NONE',  ( 19.84674366389459266, 33.71726448433410894, -2.638427012816827677 ) ) ;
#39409 = CARTESIAN_POINT ( 'NONE',  ( 13.43411237798106583, 17.66530133659708923, -12.81628187352647252 ) ) ;
#39410 = CARTESIAN_POINT ( 'NONE',  ( 10.00000000000000178, 64.31368534415483396, 10.88017736071110342 ) ) ;
#39411 = CARTESIAN_POINT ( 'NONE',  ( 17.96484262340118221, 41.18868534415484106, -7.964842623401177768 ) ) ;
#39412 = CARTESIAN_POINT ( 'NONE',  ( 20.36894250292379738, 59.92874883491397497, -10.36894250292379027 ) ) ;
#39413 = AXIS2_PLACEMENT_3D ( 'NONE', #25241, #33196, #55722 ) ;
#39414 = ADVANCED_FACE ( 'NONE', ( #40809 ), #48291, .T. ) ;
#39415 = CARTESIAN_POINT ( 'NONE',  ( 6.565887622018943937, 20.16530133659708213, 12.81628187352647430 ) ) ;
#39416 = EDGE_CURVE ( 'NONE', #98330, #69208, #9794, .T. ) ;
#39417 = VERTEX_POINT ( 'NONE', #1841 ) ;
#39418 = CARTESIAN_POINT ( 'NONE',  ( 10.00000000000000178, 25.37363466993041783, 12.81628187352647608 ) ) ;
#39419 = CARTESIAN_POINT ( 'NONE',  ( 10.00000000000000178, 24.31368534415484106, 10.88017736071110342 ) ) ;
#39420 = STYLED_ITEM ( 'NONE', ( #46022 ), #29361 ) ;
#39421 = ORIENTED_EDGE ( 'NONE', *, *, #74804, .T. ) ;
#39422 = CARTESIAN_POINT ( 'NONE',  ( 3.420591144908469161, 0.3639311400139680908, 14.60477854057961267 ) ) ;
#39423 = CARTESIAN_POINT ( 'NONE',  ( 5.076628168052703671, 1.842264484334118047, 8.527530157486179263 ) ) ;
#39424 = CARTESIAN_POINT ( 'NONE',  ( 17.20831665107776587, 42.88393115100077324, 7.208316651077764980 ) ) ;
#39425 = EDGE_CURVE ( 'NONE', #71988, #45674, #63288, .T. ) ;
#39426 = CARTESIAN_POINT ( 'NONE',  ( 2.791683348922240793, 36.63393115100078035, 7.208316651077764092 ) ) ;
#39427 = CARTESIAN_POINT ( 'NONE',  ( 10.14667048435145169, 15.00000000000000000, -10.35833375027041292 ) ) ;
#39428 = CARTESIAN_POINT ( 'NONE',  ( -2.816281873526473856, 64.33196800326376774, 3.434112377981055619 ) ) ;
#39429 = CARTESIAN_POINT ( 'NONE',  ( 19.84674366389459621, 28.50893115100078745, 7.409399052514197653E-17 ) ) ;
#39430 = DIRECTION ( 'NONE',  ( 0.000000000000000000, 0.000000000000000000, 1.000000000000000000 ) ) ;
#39431 = DIRECTION ( 'NONE',  ( 0.9975640502598257520, -0.06975647374410356982, 0.000000000000000000 ) ) ;
#39433 = FACE_OUTER_BOUND ( 'NONE', #21586, .T. ) ;
#39432 = CARTESIAN_POINT ( 'NONE',  ( 19.84674366389459266, 13.71726448433411782, -2.638427012816827677 ) ) ;
#39434 = FACE_OUTER_BOUND ( 'NONE', #94925, .T. ) ;
#39436 = VERTEX_POINT ( 'NONE', #17327 ) ;
#39435 = CARTESIAN_POINT ( 'NONE',  ( 14.92337183194729633, 42.67559781766745886, 8.527530157486181039 ) ) ;
#39437 =( BOUNDED_SURFACE ( )  B_SPLINE_SURFACE ( 3, 2, ( 
 ( #18150, #63138, #17663 ),
 ( #39679, #39181, #78149 ),
 ( #69670, #40155, #70170 ),
 ( #24178, #16674, #86642 ),
 ( #57969, #1686, #85165 ),
 ( #94624, #47146, #48624 ),
 ( #70661, #93640, #10156 ),
 ( #31657, #79128, #32139 ),
 ( #27476, #55654, #88475 ),
 ( #55140, #78650, #41154 ),
 ( #40651, #71150, #85654 ),
 ( #33612, #90430, #20981 ),
 ( #96993, #36963, #29932 ),
 ( #12966, #51966, #59940 ),
 ( #5974, #90930, #67954 ),
 ( #81462, #67458, #74950 ),
 ( #36467, #13973, #73461 ),
 ( #20481, #4989, #12477 ),
 ( #42981, #88973, #82450 ),
 ( #29435, #50968, #73962 ),
 ( #66962, #14464, #98477 ),
 ( #74447, #22458, #35470 ) ),
 .UNSPECIFIED., .F., .F., .F. ) 
 B_SPLINE_SURFACE_WITH_KNOTS ( ( 4, 2, 2, 2, 2, 2, 2, 2, 2, 2, 4 ),
 ( 3, 3 ),
 ( 0.000000000000000000, 0.002788823349942589833, 0.005577646699885179665, 0.01115529339977035933, 0.02231058679954071866, 0.03346588019931107799, 0.04462117359908143732, 0.06693176039862215598, 0.07808705379839250837, 0.08366470049827769151, 0.08924234719816287464 ),
 ( 0.000000000000000000, 1.000000000000000000 ),
 .UNSPECIFIED. ) 
 GEOMETRIC_REPRESENTATION_ITEM ( )  RATIONAL_B_SPLINE_SURFACE ( (
 ( 1.000000000000000000, 0.7071067811865475727, 1.000000000000000000),
 ( 1.000000000000000000, 0.7071067811865475727, 1.000000000000000000),
 ( 1.000000000000000000, 0.7071067811865482389, 1.000000000000000000),
 ( 1.000000000000000000, 0.7071067811865482389, 1.000000000000000000),
 ( 1.000000000000000000, 0.7071067811865482389, 1.000000000000000000),
 ( 1.000000000000000000, 0.7071067811865482389, 1.000000000000000000),
 ( 1.000000000000000000, 0.7071067811865487940, 1.000000000000000000),
 ( 1.000000000000000000, 0.7071067811865487940, 1.000000000000000000),
 ( 1.000000000000000000, 0.7071067811865477948, 1.000000000000000000),
 ( 1.000000000000000000, 0.7071067811865477948, 1.000000000000000000),
 ( 1.000000000000000000, 0.7071067811865493491, 1.000000000000000000),
 ( 1.000000000000000000, 0.7071067811865493491, 1.000000000000000000),
 ( 1.000000000000000000, 0.7071067811865473507, 1.000000000000000000),
 ( 1.000000000000000000, 0.7071067811865473507, 1.000000000000000000),
 ( 1.000000000000000000, 0.7071067811865482389, 1.000000000000000000),
 ( 1.000000000000000000, 0.7071067811865482389, 1.000000000000000000),
 ( 1.000000000000000000, 0.7071067811865482389, 1.000000000000000000),
 ( 1.000000000000000000, 0.7071067811865482389, 1.000000000000000000),
 ( 1.000000000000000000, 0.7071067811865482389, 1.000000000000000000),
 ( 1.000000000000000000, 0.7071067811865482389, 1.000000000000000000),
 ( 1.000000000000000000, 0.7071067811865482389, 1.000000000000000000),
 ( 1.000000000000000000, 0.7071067811865482389, 1.000000000000000000) ) ) 
 REPRESENTATION_ITEM ( '' )  SURFACE ( )  );
#39438 = CARTESIAN_POINT ( 'NONE',  ( 11.25000000000000178, 2.618033628982651351, -2.373340393710807175E-15 ) ) ;
#39439 = CARTESIAN_POINT ( 'NONE',  ( -2.816281873526471635, 13.91530133659708746, -3.434112377981056508 ) ) ;
#39440 = CARTESIAN_POINT ( 'NONE',  ( 20.88017736071110875, 50.77201867748817676, -2.915334737309920765 ) ) ;
#39441 = CIRCLE ( 'NONE', #21883, 2.500000000000002220 ) ;
#39442 = CARTESIAN_POINT ( 'NONE',  ( 13.79529636645031943, 40.34541550158063217, -14.16423886937409904 ) ) ;
#39443 =( BOUNDED_CURVE ( )  B_SPLINE_CURVE ( 3, ( #4742, #87726, #95225, #96237 ),
 .UNSPECIFIED., .F., .F. ) 
 B_SPLINE_CURVE_WITH_KNOTS ( ( 4, 4 ),
 ( 1.570796326794896558, 2.588785175020066109 ),
 .UNSPECIFIED. ) 
 CURVE ( )  GEOMETRIC_REPRESENTATION_ITEM ( )  RATIONAL_B_SPLINE_CURVE ( ( 1.000000000000000000, 0.9154899770527740177, 0.9154899770527740177, 1.000000000000000000 ) ) 
 REPRESENTATION_ITEM ( '' )  );
#39444 = FILL_AREA_STYLE ('',( #55917 ) ) ;
#39445 = CARTESIAN_POINT ( 'NONE',  ( -13.96552416078070102, 0.04962884865031235576, 4.756200848674986048 ) ) ;
#39446 = EDGE_CURVE ( 'NONE', #2953, #34081, #28901, .T. ) ;
#39447 = CARTESIAN_POINT ( 'NONE',  ( 24.16423886937410614, 44.51208216824730357, -3.795296366450302550 ) ) ;
#39448 = CARTESIAN_POINT ( 'NONE',  ( -4.164238869374099039, 61.80374883491397497, 8.674139862899312516E-16 ) ) ;
#39449 = CARTESIAN_POINT ( 'NONE',  ( 22.26659068614894466, 18.88708216824730002, 7.082119434687054849 ) ) ;
#39450 = CARTESIAN_POINT ( 'NONE',  ( 13.79529636645031943, 25.34541550158063572, -14.16423886937409904 ) ) ;
#39451 = CARTESIAN_POINT ( 'NONE',  ( -3.843542995449462651, 14.76984992749125780, -14.43777707752884787 ) ) ;
#39453 = CARTESIAN_POINT ( 'NONE',  ( 0.1532563361054082862, 41.21726448433411605, 2.638427012816831674 ) ) ;
#39452 = CARTESIAN_POINT ( 'NONE',  ( 4.919406150870956118, -13.80316667505430495, 2.750000000000000000 ) ) ;
#39454 = AXIS2_PLACEMENT_3D ( 'NONE', #79472, #10971, #41492 ) ;
#39455 = ORIENTED_EDGE ( 'NONE', *, *, #76596, .T. ) ;
#39456 = CARTESIAN_POINT ( 'NONE',  ( 10.00000000000000178, 39.31368534415484106, 10.88017736071110342 ) ) ;
#39457 = CARTESIAN_POINT ( 'NONE',  ( 0.000000000000000000, 14.49999999999999822, 0.000000000000000000 ) ) ;
#39458 = CARTESIAN_POINT ( 'NONE',  ( 19.65571488900283725, 92.22086433622595791, -5.360955758211049194 ) ) ;
#39459 = CARTESIAN_POINT ( 'NONE',  ( 5.076628168052704559, 45.17559781766745175, -8.527530157486179263 ) ) ;
#39461 = CARTESIAN_POINT ( 'NONE',  ( 22.81628187352647785, 61.62363466993041783, 6.195893100308588602E-16 ) ) ;
#39460 = VECTOR ( 'NONE', #75079, 1000.000000000000000 ) ;
#39462 = CARTESIAN_POINT ( 'NONE',  ( 10.36894250292378850, -5.071251165086031243, -10.36894250292379027 ) ) ;
#39463 = CARTESIAN_POINT ( 'NONE',  ( 10.00000000000000000, 44.75893115100078745, -9.846743663894594434 ) ) ;
#39464 = CARTESIAN_POINT ( 'NONE',  ( 7.361572987183169658, 59.96726448433410894, -9.846743663894592657 ) ) ;
#39465 = CARTESIAN_POINT ( 'NONE',  ( 6.204703633549690345, 42.84541550158063217, 14.16423886937410082 ) ) ;
#39466 = VERTEX_POINT ( 'NONE', #25804 ) ;
#39467 = CARTESIAN_POINT ( 'NONE',  ( -4.164238869374098151, 11.59541550158063217, -3.795296366450310543 ) ) ;
#39468 = DIRECTION ( 'NONE',  ( 0.000000000000000000, 0.000000000000000000, 1.000000000000000000 ) ) ;
#39470 = DIRECTION ( 'NONE',  ( 0.000000000000000000, 0.000000000000000000, 1.000000000000000000 ) ) ;
#39469 = CARTESIAN_POINT ( 'NONE',  ( 0.2751277870542871984, 68.21833443783938833, 6.499999999999984901 ) ) ;
#39471 = CARTESIAN_POINT ( 'NONE',  ( -0.8801773607110991993, 7.855352010821506248, -2.915334737309923874 ) ) ;
#39472 = CARTESIAN_POINT ( 'NONE',  ( 3.591859063236763294, 8.290301336597087456, -11.09922568453595026 ) ) ;
#39473 = PRESENTATION_STYLE_ASSIGNMENT (( #38977 ) ) ;
#39474 = CARTESIAN_POINT ( 'NONE',  ( -0.8801773607111008646, 68.27201867748817676, 2.915334737309923430 ) ) ;
#39475 = CARTESIAN_POINT ( 'NONE',  ( 4.630000000000001670, 1.019547802438464545, -4.000000000000000000 ) ) ;
#39476 = CARTESIAN_POINT ( 'NONE',  ( -46.94000000000001194, 103.2691844435154422, -6.361973263950303270 ) ) ;
#39477 = LINE ( 'NONE', #69967, #91810 ) ;
#39478 = CARTESIAN_POINT ( 'NONE',  ( 10.00000000000000178, 68.05374883491397497, 14.16423886937410082 ) ) ;
#39479 = CARTESIAN_POINT ( 'NONE',  ( -14.69266224296339729, 0.04962895675139352564, -1.335284760096340229 ) ) ;
#39480 = CARTESIAN_POINT ( 'NONE',  ( 7.084665262690076126, 32.02201867748816966, -10.88017736071110164 ) ) ;
#39481 = CARTESIAN_POINT ( 'NONE',  ( 10.00000000000000000, 26.81368534415484106, -10.88017736071110342 ) ) ;
#39482 = CARTESIAN_POINT ( 'NONE',  ( 10.00000000000000000, 2.873634669930420049, -12.81628187352647608 ) ) ;
#39483 = CARTESIAN_POINT ( 'NONE',  ( 17.20831665107776587, 49.13393115100078745, -7.208316651077762316 ) ) ;
#39484 = CARTESIAN_POINT ( 'NONE',  ( 13.43411237798106583, 62.66530133659708923, -12.81628187352647252 ) ) ;
#39485 = DIRECTION ( 'NONE',  ( 0.000000000000000000, 1.000000000000000000, 0.000000000000000000 ) ) ;
#39486 = EDGE_LOOP ( 'NONE', ( #66684, #17769, #78400, #83779, #88648, #46154 ) ) ;
#39487 = CARTESIAN_POINT ( 'NONE',  ( 4.559911319644449179, 27.23035201082150536, -9.422509992056141925 ) ) ;
#39488 = ADVANCED_FACE ( 'NONE', ( #78800 ), #22582, .T. ) ;
#39489 = CARTESIAN_POINT ( 'NONE',  ( 0.6178305044545838731, 34.74863466993042493, 9.382169495545420901 ) ) ;
#39490 = CARTESIAN_POINT ( 'NONE',  ( 18.52753015748618282, 63.92559781766745886, -4.923371831947291888 ) ) ;
#39491 = CARTESIAN_POINT ( 'NONE',  ( 4.559911319644449179, 48.89701867748817676, 9.422509992056141925 ) ) ;
#39492 = CARTESIAN_POINT ( 'NONE',  ( 0.1532563361054100626, 15.80059781766745353, -2.638427012816831230 ) ) ;
#39493 = VECTOR ( 'NONE', #53926, 1000.000000000000114 ) ;
#39494 = CARTESIAN_POINT ( 'NONE',  ( -2.816281873526473856, 19.12363466993042138, 9.499525473075851096E-16 ) ) ;
#39496 = CARTESIAN_POINT ( 'NONE',  ( 5.991992585808537441, 4.355491999677157623E-16, 13.20401548210299048 ) ) ;
#39495 = CARTESIAN_POINT ( 'NONE',  ( 7.084665262690076126, 64.10535201082150536, 10.88017736071109987 ) ) ;
#39497 = SURFACE_SIDE_STYLE ('',( #91989 ) ) ;
#39498 = VERTEX_POINT ( 'NONE', #78299 ) ;
#39499 = CARTESIAN_POINT ( 'NONE',  ( 3.843478602184446036, 0.2306972965111899754, 14.43834224996325410 ) ) ;
#39500 = CARTESIAN_POINT ( 'NONE',  ( -2.962741594152892510, -0.03417435944610275333, -13.93860331045676837 ) ) ;
#39501 = CARTESIAN_POINT ( 'NONE',  ( 7.084665262690076126, 44.10535201082151247, 10.88017736071109987 ) ) ;
#39503 = CARTESIAN_POINT ( 'NONE',  ( 24.16423886937410614, 9.303748834913967869, 8.672049930838204340E-16 ) ) ;
#39502 = CARTESIAN_POINT ( 'NONE',  ( 22.81628187352648496, 46.83196800326376064, -3.434112377981050290 ) ) ;
#39504 = CARTESIAN_POINT ( 'NONE',  ( 19.84674366389459266, 23.30059781766745530, 2.638427012816836559 ) ) ;
#39505 = CARTESIAN_POINT ( 'NONE',  ( 17.96484262340118221, 11.18868534415483929, -7.964842623401177768 ) ) ;
#39506 = CARTESIAN_POINT ( 'NONE',  ( 1.472469842513823179, 25.59226448433412315, -4.923371831947296329 ) ) ;
#39507 = CARTESIAN_POINT ( 'NONE',  ( 19.39235739573469885, 39.87576471608601025, 6.499999999999986677 ) ) ;
#39508 = CARTESIAN_POINT ( 'NONE',  ( 22.26659068614895176, 54.72041550158063217, -7.082119434687042414 ) ) ;
#39509 = ORIENTED_EDGE ( 'NONE', *, *, #89584, .F. ) ;
#39510 = CYLINDRICAL_SURFACE ( 'NONE', #56960, 0.5000000000000004441 ) ;
#39511 = CARTESIAN_POINT ( 'NONE',  ( 20.88017736071110519, 5.563685344154837509, 2.639326808657452039E-16 ) ) ;
#39512 = CARTESIAN_POINT ( 'NONE',  ( 1.472469842513823179, 15.59226448433411960, -4.923371831947296329 ) ) ;
#39513 = ORIENTED_EDGE ( 'NONE', *, *, #1773, .F. ) ;
#39514 = CARTESIAN_POINT ( 'NONE',  ( 15.44008868035555260, 9.730352010821505360, 9.422509992056143702 ) ) ;
#39515 = CARTESIAN_POINT ( 'NONE',  ( 20.88017736071110875, 5.772018677488170546, -2.915334737309920765 ) ) ;
#39516 = CARTESIAN_POINT ( 'NONE',  ( 19.84674366389459266, 43.71726448433410894, -2.638427012816827677 ) ) ;
#39517 = CARTESIAN_POINT ( 'NONE',  ( 6.565887622018943937, 43.08196800326374643, -12.81628187352647608 ) ) ;
#39518 = CARTESIAN_POINT ( 'NONE',  ( -9.705452947461466806, 12.49999999999999289, -5.689172442861226031 ) ) ;
#39520 = CARTESIAN_POINT ( 'NONE',  ( -0.3689425029237898834, 21.17874883491396432, -10.36894250292378850 ) ) ;
#39519 = DIRECTION ( 'NONE',  ( 1.000000000000000000, 0.000000000000000000, -0.000000000000000000 ) ) ;
#39521 = CARTESIAN_POINT ( 'NONE',  ( -0.8801773607111009756, 23.06368534415484106, 1.068504757029289695E-15 ) ) ;
#39522 = CARTESIAN_POINT ( 'NONE',  ( -0.3689425029237881626, 67.42874883491396076, 10.36894250292379027 ) ) ;
#39523 = CARTESIAN_POINT ( 'NONE',  ( 18.52753015748617571, 43.09226448433412315, 4.923371831947298993 ) ) ;
#39524 = CARTESIAN_POINT ( 'NONE',  ( 0.1034006766821432000, 15.00000000000000000, 14.49963131600458688 ) ) ;
#39525 = CARTESIAN_POINT ( 'NONE',  ( 10.00000000000000178, 42.25893115100078745, 9.846743663894594434 ) ) ;
#39526 = CARTESIAN_POINT ( 'NONE',  ( 9.065164099344512394, 14.49999999999999112, 11.95084933600776722 ) ) ;
#39527 = CARTESIAN_POINT ( 'NONE',  ( 7.208316651077762316, 29.13393115100079100, -7.208316651077764980 ) ) ;
#39528 = AXIS2_PLACEMENT_3D ( 'NONE', #36085, #50102, #85779 ) ;
#39529 = ORIENTED_EDGE ( 'NONE', *, *, #34736, .T. ) ;
#39530 = CARTESIAN_POINT ( 'NONE',  ( 20.88017736071110519, 5.563685344154837509, 2.639326808657452039E-16 ) ) ;
#39531 = CARTESIAN_POINT ( 'NONE',  ( 12.91533473730993009, 66.60535201082150536, -10.88017736071109987 ) ) ;
#39533 = CARTESIAN_POINT ( 'NONE',  ( 7.361572987183170547, 52.05059781766745175, 9.846743663894590881 ) ) ;
#39532 = CIRCLE ( 'NONE', #1295, 10.90000000000000036 ) ;
#39534 = CARTESIAN_POINT ( 'NONE',  ( 7.084665262690076126, 52.02201867748816255, -10.88017736071110164 ) ) ;
#39536 = CARTESIAN_POINT ( 'NONE',  ( 10.00000000000000178, 25.37363466993041783, 12.81628187352647608 ) ) ;
#39535 = CARTESIAN_POINT ( 'NONE',  ( 17.96484262340118221, 11.18868534415483929, -7.964842623401177768 ) ) ;
#39537 = CARTESIAN_POINT ( 'NONE',  ( 24.16423886937409904, 24.09541550158063927, 3.795296366450317205 ) ) ;
#39538 = TOROIDAL_SURFACE ( 'NONE', #47512, 14.49999999999999822, 0.5000000000000000000 ) ;
#39539 = CIRCLE ( 'NONE', #58638, 11.25000000000000178 ) ;
#39540 = ADVANCED_FACE ( 'NONE', ( #3798 ), #78450, .T. ) ;
#39541 = EDGE_CURVE ( 'NONE', #15515, #87018, #5012, .T. ) ;
#39542 = CARTESIAN_POINT ( 'NONE',  ( 10.00000000000000178, 45.37363466993041783, 12.81628187352647608 ) ) ;
#39543 = ADVANCED_FACE ( 'NONE', ( #85814 ), #24827, .T. ) ;
#39544 = ORIENTED_EDGE ( 'NONE', *, *, #83264, .T. ) ;
#39545 = CARTESIAN_POINT ( 'NONE',  ( 12.63842701281683922, 64.55059781766745175, -9.846743663894590881 ) ) ;
#39546 = CARTESIAN_POINT ( 'NONE',  ( 0.5774900079438590739, 17.64701867748817321, -5.440088680355550821 ) ) ;
#39547 = ORIENTED_EDGE ( 'NONE', *, *, #84118, .F. ) ;
#39548 = CARTESIAN_POINT ( 'NONE',  ( 15.44008868035555793, 31.39701867748817676, -9.422509992056140149 ) ) ;
#39549 = ORIENTED_EDGE ( 'NONE', *, *, #43152, .T. ) ;
#39550 = CARTESIAN_POINT ( 'NONE',  ( 2.035157376598822676, 62.43868534415483396, -7.964842623401177768 ) ) ;
#39551 = CARTESIAN_POINT ( 'NONE',  ( 20.88017736071110519, 65.56368534415483396, 2.639326808657452039E-16 ) ) ;
#39552 = CARTESIAN_POINT ( 'NONE',  ( 7.361572987183170547, 12.05059781766744997, 9.846743663894590881 ) ) ;
#39553 = EDGE_CURVE ( 'NONE', #35821, #36181, #18136, .T. ) ;
#39554 = CARTESIAN_POINT ( 'NONE',  ( 4.559911319644449179, 68.89701867748817676, 9.422509992056141925 ) ) ;
#39555 = CARTESIAN_POINT ( 'NONE',  ( 2.746530213673227803E-16, 21.83999999999999986, 0.000000000000000000 ) ) ;
#39557 = ORIENTED_EDGE ( 'NONE', *, *, #13597, .F. ) ;
#39556 = CARTESIAN_POINT ( 'NONE',  ( 12.63842701281683034, 12.46726448433411782, 9.846743663894596210 ) ) ;
#39558 = CARTESIAN_POINT ( 'NONE',  ( 12.63842701281683034, 37.46726448433411605, 9.846743663894596210 ) ) ;
#39559 = VERTEX_POINT ( 'NONE', #34254 ) ;
#39560 = EDGE_LOOP ( 'NONE', ( #74330, #22816, #62419 ) ) ;
#39561 = LINE ( 'NONE', #71538, #47432 ) ;
#39562 = CARTESIAN_POINT ( 'NONE',  ( -0.3689425029237881626, 2.428748834913967869, 10.36894250292379027 ) ) ;
#39563 = CARTESIAN_POINT ( 'NONE',  ( 6.565887622018943937, 58.08196800326376064, -12.81628187352647608 ) ) ;
#39564 = EDGE_CURVE ( 'NONE', #20729, #22610, #97609, .T. ) ;
#39565 = CARTESIAN_POINT ( 'NONE',  ( 20.36894250292379738, 9.928748834913966093, -10.36894250292379027 ) ) ;
#39566 = CARTESIAN_POINT ( 'NONE',  ( 2.917880565312948704, 17.63708216824730357, 12.26659068614894643 ) ) ;
#39567 = TOROIDAL_SURFACE ( 'NONE', #9226, 2.899999999999999467, 0.1000000000000000056 ) ;
#39568 = DIRECTION ( 'NONE',  ( 1.049065152435176504E-16, -1.000000000000000000, 0.000000000000000000 ) ) ;
#39570 = CARTESIAN_POINT ( 'NONE',  ( 0.5774900079438590739, 62.64701867748817676, -5.440088680355550821 ) ) ;
#39569 = CARTESIAN_POINT ( 'NONE',  ( 20.15039907845753220, 55.60158574516643171, -6.262539305110077947 ) ) ;
#39571 = CARTESIAN_POINT ( 'NONE',  ( 2.035157376598822676, 22.43868534415483396, -7.964842623401177768 ) ) ;
#39572 = CARTESIAN_POINT ( 'NONE',  ( 0.6081133539230402230, 68.33703382326399378, 6.499999999999953815 ) ) ;
#39573 = ORIENTED_EDGE ( 'NONE', *, *, #55589, .F. ) ;
#39574 = CARTESIAN_POINT ( 'NONE',  ( 17.20831665107776587, 9.133931151000787452, -7.208316651077762316 ) ) ;
#39575 = CARTESIAN_POINT ( 'NONE',  ( 19.84674366389459621, 8.508931151000785675, 7.409399052514197653E-17 ) ) ;
#39576 = CARTESIAN_POINT ( 'NONE',  ( 19.38216949554541557, 32.24863466993041783, -9.382169495545420901 ) ) ;
#39577 = CARTESIAN_POINT ( 'NONE',  ( 2.791683348922237240, 20.38393115100078745, -7.208316651077763204 ) ) ;
#39578 = CARTESIAN_POINT ( 'NONE',  ( 19.38216949554541202, 10.99863466993042138, 9.382169495545424454 ) ) ;
#39579 = EDGE_CURVE ( 'NONE', #88333, #243, #87276, .T. ) ;
#39580 = DIRECTION ( 'NONE',  ( 0.000000000000000000, 0.000000000000000000, 1.000000000000000000 ) ) ;
#39581 = CIRCLE ( 'NONE', #77883, 15.00000000000000000 ) ;
#39582 = CARTESIAN_POINT ( 'NONE',  ( 5.076628168052704559, 0.1755978176674514724, -8.527530157486179263 ) ) ;
#39583 = ORIENTED_EDGE ( 'NONE', *, *, #60064, .F. ) ;
#39584 = ORIENTED_EDGE ( 'NONE', *, *, #63126, .T. ) ;
#39585 = CARTESIAN_POINT ( 'NONE',  ( 0.5774900079438590739, 42.64701867748816966, -5.440088680355550821 ) ) ;
#39586 = CARTESIAN_POINT ( 'NONE',  ( -4.164238869374099039, 31.80374883491396432, 8.674139862899312516E-16 ) ) ;
#39587 = CARTESIAN_POINT ( 'NONE',  ( 7.361572987183169658, 39.96726448433411605, -9.846743663894592657 ) ) ;
#39588 = CARTESIAN_POINT ( 'NONE',  ( 2.791683348922240793, 1.633931151000784565, 7.208316651077764092 ) ) ;
#39590 = CARTESIAN_POINT ( 'NONE',  ( -7.081429851441987999, -84.79152421822192309, -3.750000000000000000 ) ) ;
#39589 = CARTESIAN_POINT ( 'NONE',  ( 0.6178305044545818747, 58.49863466993042493, -9.382169495545419124 ) ) ;
#39591 = CARTESIAN_POINT ( 'NONE',  ( 15.44008868035555260, 24.73035201082150891, 9.422509992056143702 ) ) ;
#39592 = LINE ( 'NONE', #47571, #80554 ) ;
#39593 = TOROIDAL_SURFACE ( 'NONE', #9250, 14.49999999999999822, 0.5000000000000000000 ) ;
#39594 = CARTESIAN_POINT ( 'NONE',  ( 3.591859063236761518, 19.95696800326375353, 11.09922568453594849 ) ) ;
#39595 = CARTESIAN_POINT ( 'NONE',  ( 19.38216949554541202, 10.99863466993042138, 9.382169495545424454 ) ) ;
#39596 = CARTESIAN_POINT ( 'NONE',  ( 10.00000000000000000, 39.75893115100078745, -9.846743663894594434 ) ) ;
#39597 = CARTESIAN_POINT ( 'NONE',  ( 7.964842623401181321, 4.938685344154837509, 7.964842623401174215 ) ) ;
#39598 = CARTESIAN_POINT ( 'NONE',  ( 6.565887622018943937, 55.16530133659709634, 12.81628187352647430 ) ) ;
#39599 = DIRECTION ( 'NONE',  ( -1.000000000000000000, -1.927470528863119542E-16, 0.000000000000000000 ) ) ;
#39601 = CARTESIAN_POINT ( 'NONE',  ( -13.34343830728408697, 14.49999999999999822, 6.852200678592504701 ) ) ;
#39600 = CARTESIAN_POINT ( 'NONE',  ( 17.96484262340118221, 59.93868534415484106, 7.964842623401181321 ) ) ;
#39602 = CIRCLE ( 'NONE', #15626, 0.4999999999999961142 ) ;
#39603 = CARTESIAN_POINT ( 'NONE',  ( -11.17376097835657411, -90.29818107662934779, 4.000000000000000888 ) ) ;
#39604 = FACE_OUTER_BOUND ( 'NONE', #26610, .T. ) ;
#39605 = AXIS2_PLACEMENT_3D ( 'NONE', #12191, #19699, #41243 ) ;
#39606 = CARTESIAN_POINT ( 'NONE',  ( 15.44008868035555793, 56.39701867748817676, -9.422509992056140149 ) ) ;
#39607 = CARTESIAN_POINT ( 'NONE',  ( 10.00000000000000178, 59.31368534415484106, 10.88017736071110342 ) ) ;
#39608 = CYLINDRICAL_SURFACE ( 'NONE', #44087, 15.00000000000000000 ) ;
#39609 = CARTESIAN_POINT ( 'NONE',  ( 17.96484262340118221, 9.938685344154839285, 7.964842623401181321 ) ) ;
#39610 = CARTESIAN_POINT ( 'NONE',  ( 0.1532563361054100626, 55.80059781766745175, -2.638427012816831230 ) ) ;
#39612 = CARTESIAN_POINT ( 'NONE',  ( 9.323033696085012423, 0.04962895454604582951, -11.43408728005512920 ) ) ;
#39611 = CARTESIAN_POINT ( 'NONE',  ( 15.44008868035555793, 16.39701867748817321, -9.422509992056140149 ) ) ;
#39613 = CARTESIAN_POINT ( 'NONE',  ( 22.81628187352647785, 31.62363466993042138, 6.195893100308588602E-16 ) ) ;
#39614 = VERTEX_POINT ( 'NONE', #16825 ) ;
#39615 = CARTESIAN_POINT ( 'NONE',  ( 10.00000000000000000, 41.81368534415484106, -10.88017736071110342 ) ) ;
#39617 = CARTESIAN_POINT ( 'NONE',  ( -5.999999999999994671, 79.82179676972448590, 6.250000000000000000 ) ) ;
#39616 = CARTESIAN_POINT ( 'NONE',  ( 19.38216949554541557, 12.24863466993041961, -9.382169495545420901 ) ) ;
#39618 = CARTESIAN_POINT ( 'NONE',  ( 0.5774900079438590739, 17.64701867748817321, -5.440088680355550821 ) ) ;
#39619 = CARTESIAN_POINT ( 'NONE',  ( 2.035157376598824452, 43.68868534415484106, 7.964842623401179544 ) ) ;
#39620 = CARTESIAN_POINT ( 'NONE',  ( -2.266590686148945544, 57.22041550158063217, 7.082119434687048631 ) ) ;
#39621 = CARTESIAN_POINT ( 'NONE',  ( 14.92337183194729988, 29.34226448433411960, -8.527530157486177487 ) ) ;
#39622 = CARTESIAN_POINT ( 'NONE',  ( 7.084665262690076126, 64.10535201082150536, 10.88017736071109987 ) ) ;
#39623 = CARTESIAN_POINT ( 'NONE',  ( 19.50000000000000711, 105.0000000000000000, -5.000000000000000000 ) ) ;
#39624 = CARTESIAN_POINT ( 'NONE',  ( -2.266590686148945544, 17.22041550158063572, 7.082119434687048631 ) ) ;
#39625 = EDGE_CURVE ( 'NONE', #81238, #86936, #77801, .T. ) ;
#39626 = CARTESIAN_POINT ( 'NONE',  ( -13.55255535720589322, -0.03417435944610275333, -4.403492169843143067 ) ) ;
#39627 = CARTESIAN_POINT ( 'NONE',  ( -3.750000000000000000, 10.25000000000000000, 4.000000000000000000 ) ) ;
#39628 = ORIENTED_EDGE ( 'NONE', *, *, #50484, .F. ) ;
#39629 = ORIENTED_EDGE ( 'NONE', *, *, #26216, .T. ) ;
#39630 = CARTESIAN_POINT ( 'NONE',  ( 10.00000000000000000, 40.55374883491397497, -14.16423886937410082 ) ) ;
#39631 = CARTESIAN_POINT ( 'NONE',  ( 17.08211943468705130, 38.47041550158063217, 12.26659068614894998 ) ) ;
#39632 = CARTESIAN_POINT ( 'NONE',  ( 10.00000000000000000, 66.81368534415484817, -10.88017736071110342 ) ) ;
#39633 = CARTESIAN_POINT ( 'NONE',  ( -2.816281873526473856, 9.123634669930421381, 9.499525473075851096E-16 ) ) ;
#39634 = CARTESIAN_POINT ( 'NONE',  ( 0.1532563361054083140, 66.00893115100079456, 1.131784320476157264E-15 ) ) ;
#39635 = CARTESIAN_POINT ( 'NONE',  ( 1.274849032794294290, 58.57228050351032778, 6.499999999999979572 ) ) ;
#39637 = CARTESIAN_POINT ( 'NONE',  ( 0.6178305044545818747, 23.49863466993041783, -9.382169495545419124 ) ) ;
#39636 = CARTESIAN_POINT ( 'NONE',  ( -0.8801773607111009756, 58.06368534415484106, 1.068504757029289695E-15 ) ) ;
#39638 = CARTESIAN_POINT ( 'NONE',  ( 24.16423886937410614, 34.51208216824731068, -3.795296366450302550 ) ) ;
#39639 = CARTESIAN_POINT ( 'NONE',  ( 20.88017736071110519, 30.56368534415484106, 2.639326808657452039E-16 ) ) ;
#39640 = CARTESIAN_POINT ( 'NONE',  ( 4.559911319644449179, 27.23035201082150536, -9.422509992056141925 ) ) ;
#39641 = DIRECTION ( 'NONE',  ( -0.000000000000000000, -1.000000000000000000, -0.000000000000000000 ) ) ;
#39642 = CARTESIAN_POINT ( 'NONE',  ( 10.00000000000000000, -0.2410688489992152128, -9.846743663894594434 ) ) ;
#39643 = CARTESIAN_POINT ( 'NONE',  ( -7.208316651077756099, -13.36606884899921077, 7.208316651077766757 ) ) ;
#39644 = ORIENTED_EDGE ( 'NONE', *, *, #67208, .F. ) ;
#39645 = CARTESIAN_POINT ( 'NONE',  ( 3.799999999999998934, 1.839999999999999636, 4.776122516674677286E-16 ) ) ;
#39646 =( BOUNDED_CURVE ( )  B_SPLINE_CURVE ( 2, ( #88916, #97922, #43890, #52878, #45378, #74890, #96934, #37410, #20918 ),
 .UNSPECIFIED., .F., .T. ) 
 B_SPLINE_CURVE_WITH_KNOTS ( ( 3, 2, 2, 2, 3 ),
 ( 0.5820003743640369542, 0.5833333333333333703, 0.5892857142857143016, 0.5952380952380952328, 0.5965710542073916489 ),
 .UNSPECIFIED. ) 
 CURVE ( )  GEOMETRIC_REPRESENTATION_ITEM ( )  RATIONAL_B_SPLINE_CURVE ( ( 0.9881565478350734510, 0.9923695281211492025, 1.000000000000000000, 0.9659258262890683122, 1.000000000000000000, 0.9659258262890683122, 1.000000000000000000, 0.9923695281211490915, 0.9881565478350733400 ) ) 
 REPRESENTATION_ITEM ( '' )  );
#39648 = ADVANCED_FACE ( 'NONE', ( #82237 ), #96777, .F. ) ;
#39647 = DIRECTION ( 'NONE',  ( -1.000000000000000000, 0.000000000000000000, 0.000000000000000000 ) ) ;
#39649 = VERTEX_POINT ( 'NONE', #43253 ) ;
#39650 =( LENGTH_UNIT ( ) NAMED_UNIT ( * ) SI_UNIT ( .MILLI., .METRE. ) );
#39652 = CARTESIAN_POINT ( 'NONE',  ( 4.559911319644449179, 13.89701867748817321, 9.422509992056141925 ) ) ;
#39651 = CARTESIAN_POINT ( 'NONE',  ( 22.26659068614894466, 63.88708216824730357, 7.082119434687054849 ) ) ;
#39654 = CARTESIAN_POINT ( 'NONE',  ( 19.84674366389459266, 58.30059781766745886, 2.638427012816836559 ) ) ;
#39653 = CARTESIAN_POINT ( 'NONE',  ( 17.20831665107776587, 39.13393115100079456, -7.208316651077762316 ) ) ;
#39655 = CARTESIAN_POINT ( 'NONE',  ( 19.72487221294571569, 42.80223176428830811, -6.499999999999990230 ) ) ;
#39656 = CARTESIAN_POINT ( 'NONE',  ( -5.999999999999994671, 43.00000000000000000, -6.500000000000000888 ) ) ;
#39657 = TOROIDAL_SURFACE ( 'NONE', #93955, 0.7500000000000008882, 0.2500000000000000000 ) ;
#39658 = EDGE_CURVE ( 'NONE', #7550, #88366, #51753, .T. ) ;
#39659 = CARTESIAN_POINT ( 'NONE',  ( -2.816281873526473856, -0.6680319967362464695, 3.434112377981055619 ) ) ;
#39660 = EDGE_CURVE ( 'NONE', #77584, #20106, #44965, .T. ) ;
#39661 = EDGE_LOOP ( 'NONE', ( #74566, #73146, #9991, #14686 ) ) ;
#39662 = CARTESIAN_POINT ( 'NONE',  ( -4.164238869374099927, 42.01208216824728936, 3.795296366450308767 ) ) ;
#39663 = ORIENTED_EDGE ( 'NONE', *, *, #6279, .F. ) ;
#39664 = CARTESIAN_POINT ( 'NONE',  ( 22.26659068614894466, 38.88708216824731068, 7.082119434687054849 ) ) ;
#39665 = ORIENTED_EDGE ( 'NONE', *, *, #96255, .F. ) ;
#39666 = CARTESIAN_POINT ( 'NONE',  ( 20.88017736071110519, 25.56368534415483751, 2.639326808657452039E-16 ) ) ;
#39667 = CARTESIAN_POINT ( 'NONE',  ( 0.000000000000000000, 15.00000000000000000, 0.000000000000000000 ) ) ;
#39668 = AXIS2_PLACEMENT_3D ( 'NONE', #80115, #72119, #93647 ) ;
#39669 = CARTESIAN_POINT ( 'NONE',  ( 2.035157376598824452, 43.68868534415484106, 7.964842623401179544 ) ) ;
#39670 = CARTESIAN_POINT ( 'NONE',  ( 7.361572987183169658, 54.96726448433413026, -9.846743663894592657 ) ) ;
#39671 = CARTESIAN_POINT ( 'NONE',  ( 19.42250999205614193, 35.14701867748816966, 5.440088680355555262 ) ) ;
#39672 = CARTESIAN_POINT ( 'NONE',  ( -6.581680125707233486, -88.31141629936868753, -3.750000000000000000 ) ) ;
#39673 = CARTESIAN_POINT ( 'NONE',  ( 0.5774900079438607392, 68.48035201082150536, 5.440088680355550821 ) ) ;
#39674 = CARTESIAN_POINT ( 'NONE',  ( 20.88017736071110519, 30.56368534415484106, 2.639326808657452039E-16 ) ) ;
#39675 = MECHANICAL_DESIGN_GEOMETRIC_PRESENTATION_REPRESENTATION (  '', ( #76419 ), #46026 ) ;
#39677 = VERTEX_POINT ( 'NONE', #80272 ) ;
#39676 = DIRECTION ( 'NONE',  ( 0.000000000000000000, 0.000000000000000000, 1.000000000000000000 ) ) ;
#39678 = CARTESIAN_POINT ( 'NONE',  ( 5.076628168052704559, 5.175597817667451750, -8.527530157486179263 ) ) ;
#39679 = CARTESIAN_POINT ( 'NONE',  ( -3.250000001579299802, 0.08818787376450962223, 2.500000000000000000 ) ) ;
#39680 = EDGE_LOOP ( 'NONE', ( #54516, #32006, #58031, #78017, #90534, #95708 ) ) ;
#39681 = SURFACE_STYLE_FILL_AREA ( #78151 ) ;
#39682 = CARTESIAN_POINT ( 'NONE',  ( 2.791683348922237240, 30.38393115100078390, -7.208316651077763204 ) ) ;
#39683 = CARTESIAN_POINT ( 'NONE',  ( -8.099999999999999645, 80.99999999999994316, 0.000000000000000000 ) ) ;
#39684 = CARTESIAN_POINT ( 'NONE',  ( -1.099225684535947600, 43.70696800326375353, -6.408140936763238038 ) ) ;
#39685 = FILL_AREA_STYLE_COLOUR ( '', #69146 ) ;
#39686 = EDGE_CURVE ( 'NONE', #85753, #53420, #264, .T. ) ;
#39687 = DIRECTION ( 'NONE',  ( -0.000000000000000000, -0.000000000000000000, 1.000000000000000000 ) ) ;
#39688 = CARTESIAN_POINT ( 'NONE',  ( 14.47650479471825236, 0.3639311865616660091, -3.928206833722031721 ) ) ;
#39689 = CARTESIAN_POINT ( 'NONE',  ( -42.50369195530268485, 107.9060299417078426, 4.999999999999996447 ) ) ;
#39690 = CARTESIAN_POINT ( 'NONE',  ( 19.84674366389459266, 48.71726448433413026, -2.638427012816827677 ) ) ;
#39691 = CARTESIAN_POINT ( 'NONE',  ( 2.917880565312950480, 45.97041550158063927, -12.26659068614894821 ) ) ;
#39692 = CARTESIAN_POINT ( 'NONE',  ( 17.20831665107776587, 64.13393115100079456, -7.208316651077762316 ) ) ;
#39693 = VERTEX_POINT ( 'NONE', #11773 ) ;
#39694 = CARTESIAN_POINT ( 'NONE',  ( -11.62719953690052144, 0.3640475087720991820, -9.476720473301961434 ) ) ;
#39695 = CARTESIAN_POINT ( 'NONE',  ( 12.63842701281683034, 22.46726448433411605, 9.846743663894596210 ) ) ;
#39696 = CARTESIAN_POINT ( 'NONE',  ( 22.81628187352648496, 51.83196800326376064, -3.434112377981050290 ) ) ;
#39697 = CARTESIAN_POINT ( 'NONE',  ( 1.472469842513823179, 61.42559781766745175, 4.923371831947296329 ) ) ;
#39698 = CARTESIAN_POINT ( 'NONE',  ( 17.96484262340118221, 59.93868534415484106, 7.964842623401181321 ) ) ;
#39699 = EDGE_CURVE ( 'NONE', #2288, #54272, #65249, .T. ) ;
#39700 = CARTESIAN_POINT ( 'NONE',  ( -11.92686044187656513, 7.662123368507814725, 3.903127820947815962E-15 ) ) ;
#39701 = ORIENTED_EDGE ( 'NONE', *, *, #57799, .F. ) ;
#39702 = CARTESIAN_POINT ( 'NONE',  ( 2.917880565312950480, 60.97041550158063927, -12.26659068614894821 ) ) ;
#39703 = CARTESIAN_POINT ( 'NONE',  ( 19.42250999205614548, 30.98035201082150536, -5.440088680355545492 ) ) ;
#39705 = CARTESIAN_POINT ( 'NONE',  ( -0.8801773607111009756, 63.06368534415484106, 1.068504757029289695E-15 ) ) ;
#39704 = CARTESIAN_POINT ( 'NONE',  ( -2.816281873526473856, 9.123634669930421381, 9.499525473075851096E-16 ) ) ;
#39706 = CARTESIAN_POINT ( 'NONE',  ( 14.11917416961168747, 14.76930270348881002, -4.887430353538946726 ) ) ;
#39707 = DIRECTION ( 'NONE',  ( 0.000000000000000000, 0.000000000000000000, -1.000000000000000000 ) ) ;
#39708 = CARTESIAN_POINT ( 'NONE',  ( 8.439016546559821919, 3.791394052158136007E-16, 11.79122553964979048 ) ) ;
#39710 = CARTESIAN_POINT ( 'NONE',  ( -4.000000000000000000, 10.00000000000000000, -3.750000000000000000 ) ) ;
#39709 = CARTESIAN_POINT ( 'NONE',  ( 2.035157376598824452, 58.68868534415482685, 7.964842623401179544 ) ) ;
#39711 = CARTESIAN_POINT ( 'NONE',  ( 12.63842701281683922, 39.55059781766744464, -9.846743663894590881 ) ) ;
#39712 = CARTESIAN_POINT ( 'NONE',  ( -10.36894250292379205, 31.17874883491396432, -10.36894250292378672 ) ) ;
#39713 = CARTESIAN_POINT ( 'NONE',  ( 21.09922568453594849, 6.206968003263753531, 6.408140936763242479 ) ) ;
#39715 = CARTESIAN_POINT ( 'NONE',  ( 0.09770025222076776650, 69.67742753483355500, -6.500000000000000000 ) ) ;
#39714 = CARTESIAN_POINT ( 'NONE',  ( 10.00000000000000000, 16.81368534415483751, -10.88017736071110342 ) ) ;
#39716 = CARTESIAN_POINT ( 'NONE',  ( -0.3998276802501956606, -0.03417435944610275333, -15.99117050944549234 ) ) ;
#39717 = CARTESIAN_POINT ( 'NONE',  ( 20.36894250292379738, 39.92874883491396787, -10.36894250292379027 ) ) ;
#39718 = CARTESIAN_POINT ( 'NONE',  ( 24.16423886937409904, 64.09541550158064638, 3.795296366450317205 ) ) ;
#39719 = CARTESIAN_POINT ( 'NONE',  ( 10.00000000000000000, 14.75893115100078568, -9.846743663894594434 ) ) ;
#39720 = CARTESIAN_POINT ( 'NONE',  ( 20.88017736071110875, 10.77201867748817143, -2.915334737309920765 ) ) ;
#39721 = EDGE_LOOP ( 'NONE', ( #24726, #11113, #94116, #16143, #86360, #56256 ) ) ;
#39722 = CARTESIAN_POINT ( 'NONE',  ( 7.361572987183169658, 39.96726448433411605, -9.846743663894592657 ) ) ;
#39723 = CARTESIAN_POINT ( 'NONE',  ( -0.8801773607111008646, 28.27201867748817321, 2.915334737309923430 ) ) ;
#39724 = CARTESIAN_POINT ( 'NONE',  ( 7.361572987183169658, 64.96726448433412315, -9.846743663894592657 ) ) ;
#39726 = CARTESIAN_POINT ( 'NONE',  ( -0.2838433074297238012, 13.12729635533385597, -10.00000000000000000 ) ) ;
#39725 = CARTESIAN_POINT ( 'NONE',  ( 20.36894250292379738, 14.92874883491396432, -10.36894250292379027 ) ) ;
#39727 = CARTESIAN_POINT ( 'NONE',  ( 0.8719017118913388043, 123.9374316453451286, -5.000000000000000000 ) ) ;
#39728 = CARTESIAN_POINT ( 'NONE',  ( 19.84674366389459266, 13.71726448433411782, -2.638427012816827677 ) ) ;
#39729 = CARTESIAN_POINT ( 'NONE',  ( 10.00000000000000000, 57.87363466993042493, -12.81628187352647608 ) ) ;
#39730 = CARTESIAN_POINT ( 'NONE',  ( 0.1532563361054082862, 51.21726448433412315, 2.638427012816831674 ) ) ;
#39731 = VERTEX_POINT ( 'NONE', #27257 ) ;
#39732 = CARTESIAN_POINT ( 'NONE',  ( 9.209312257346764952, -9.300771453421772250, -3.750000000000000000 ) ) ;
#39733 = CARTESIAN_POINT ( 'NONE',  ( -4.164238869374099039, 61.80374883491397497, 8.674139862899312516E-16 ) ) ;
#39734 = CIRCLE ( 'NONE', #52488, 15.00000000000000000 ) ;
#39735 = CARTESIAN_POINT ( 'NONE',  ( 20.36894250292379382, 13.67874883491396965, 10.36894250292379205 ) ) ;
#39736 = CARTESIAN_POINT ( 'NONE',  ( 10.00000000000000000, 61.81368534415484106, -10.88017736071110342 ) ) ;
#39737 = CARTESIAN_POINT ( 'NONE',  ( 1.472469842513823179, 40.59226448433411605, -4.923371831947296329 ) ) ;
#39738 = CARTESIAN_POINT ( 'NONE',  ( 0.5774900079438607392, 18.48035201082150536, 5.440088680355550821 ) ) ;
#39739 = DIRECTION ( 'NONE',  ( 0.000000000000000000, 0.000000000000000000, 1.000000000000000000 ) ) ;
#39740 = CARTESIAN_POINT ( 'NONE',  ( 12.63842701281683034, 62.46726448433410894, 9.846743663894596210 ) ) ;
#39741 = EDGE_CURVE ( 'NONE', #80524, #663, #49737, .T. ) ;
#39742 = AXIS2_PLACEMENT_3D ( 'NONE', #23172, #83163, #83660 ) ;
#39743 = LINE ( 'NONE', #1271, #5929 ) ;
#39744 = CIRCLE ( 'NONE', #50930, 15.00000000000000000 ) ;
#39745 = VERTEX_POINT ( 'NONE', #80767 ) ;
#39746 = EDGE_LOOP ( 'NONE', ( #62115, #67175, #49445, #17381 ) ) ;
#39747 = CARTESIAN_POINT ( 'NONE',  ( 17.39651004071843232, 17.93575266056828355, 6.499999999999984013 ) ) ;
#39748 = DIRECTION ( 'NONE',  ( 0.000000000000000000, 0.000000000000000000, 1.000000000000000000 ) ) ;
#39749 = CARTESIAN_POINT ( 'NONE',  ( 12.63842701281683922, 49.55059781766744464, -9.846743663894590881 ) ) ;
#39750 = CARTESIAN_POINT ( 'NONE',  ( 10.00000000000000178, 27.25893115100078390, 9.846743663894594434 ) ) ;
#39751 = CARTESIAN_POINT ( 'NONE',  ( 19.38216949554541202, 55.99863466993041072, 9.382169495545424454 ) ) ;
#39753 = CARTESIAN_POINT ( 'NONE',  ( 5.076628168052704559, 50.17559781766745886, -8.527530157486179263 ) ) ;
#39752 = CARTESIAN_POINT ( 'NONE',  ( 2.035157376598824452, 23.68868534415484461, 7.964842623401179544 ) ) ;
#39754 = CARTESIAN_POINT ( 'NONE',  ( 5.845017550302928022, -0.03417435944610275333, 14.89003580495037582 ) ) ;
#39755 = CARTESIAN_POINT ( 'NONE',  ( -4.164238869374099039, 56.80374883491397497, 8.674139862899312516E-16 ) ) ;
#39756 = DIRECTION ( 'NONE',  ( 0.000000000000000000, 0.000000000000000000, 1.000000000000000000 ) ) ;
#39757 = CARTESIAN_POINT ( 'NONE',  ( 20.88017736071110519, 55.56368534415484817, 2.639326808657452039E-16 ) ) ;
#39758 = CARTESIAN_POINT ( 'NONE',  ( 5.076628168052704559, 20.17559781766745175, -8.527530157486179263 ) ) ;
#39759 = DIRECTION ( 'NONE',  ( 8.673617379884027583E-16, 1.000000000000000000, -0.000000000000000000 ) ) ;
#39760 = ORIENTED_EDGE ( 'NONE', *, *, #41267, .T. ) ;
#39761 = CARTESIAN_POINT ( 'NONE',  ( 2.603489959281588995, 55.43575266056826933, -6.500000000000003553 ) ) ;
#39762 = ORIENTED_EDGE ( 'NONE', *, *, #69352, .T. ) ;
#39763 = CARTESIAN_POINT ( 'NONE',  ( 19.84674366389459266, 13.71726448433411782, -2.638427012816827677 ) ) ;
#39764 = VERTEX_POINT ( 'NONE', #89737 ) ;
#39765 = CARTESIAN_POINT ( 'NONE',  ( 6.204703633549690345, 17.84541550158063217, 14.16423886937410082 ) ) ;
#39766 = CARTESIAN_POINT ( 'NONE',  ( 0.1532563361054083140, 26.00893115100078745, 1.131784320476157264E-15 ) ) ;
#39767 = CARTESIAN_POINT ( 'NONE',  ( 0.5774900079438590739, 37.64701867748817676, -5.440088680355550821 ) ) ;
#39768 = STYLED_ITEM ( 'NONE', ( #47757 ), #26911 ) ;
#39769 = CARTESIAN_POINT ( 'NONE',  ( 14.49120296996857249, 0.04922511925147129985, 2.766068805437629674 ) ) ;
#39770 = ORIENTED_EDGE ( 'NONE', *, *, #62855, .T. ) ;
#39771 = CARTESIAN_POINT ( 'NONE',  ( 19.42250999205614193, 35.14701867748816966, 5.440088680355555262 ) ) ;
#39772 = EDGE_CURVE ( 'NONE', #86489, #44015, #4779, .T. ) ;
#39773 = CARTESIAN_POINT ( 'NONE',  ( 19.80427997160309417, 37.75733960839544778, -6.499999999999988454 ) ) ;
#39774 = CARTESIAN_POINT ( 'NONE',  ( 9.382169495545415572, -2.751365330069575510, -9.382169495545422677 ) ) ;
#39775 = EDGE_CURVE ( 'NONE', #22949, #77971, #14663, .T. ) ;
#39776 = VERTEX_POINT ( 'NONE', #59236 ) ;
#39777 = CARTESIAN_POINT ( 'NONE',  ( 22.26659068614895176, 9.720415501580633943, -7.082119434687042414 ) ) ;
#39778 = ORIENTED_EDGE ( 'NONE', *, *, #7858, .F. ) ;
#39779 = ORIENTED_EDGE ( 'NONE', *, *, #2152, .T. ) ;
#39780 = CARTESIAN_POINT ( 'NONE',  ( 3.591859063236761518, 29.95696800326375708, 11.09922568453594849 ) ) ;
#39781 = AXIS2_PLACEMENT_3D ( 'NONE', #32696, #2238, #10216 ) ;
#39782 = CARTESIAN_POINT ( 'NONE',  ( 12.63842701281683922, 9.550597817667449974, -9.846743663894590881 ) ) ;
#39783 = LINE ( 'NONE', #55258, #32287 ) ;
#39784 = CARTESIAN_POINT ( 'NONE',  ( -12.83294900548056994, 14.49999999999999112, -7.766300266068596692 ) ) ;
#39785 = CARTESIAN_POINT ( 'NONE',  ( 12.63842701281683034, 17.46726448433411250, 9.846743663894596210 ) ) ;
#39786 = CARTESIAN_POINT ( 'NONE',  ( 10.00000000000000178, 34.31368534415484106, 10.88017736071110342 ) ) ;
#39787 = VERTEX_POINT ( 'NONE', #35253 ) ;
#39788 = DIRECTION ( 'NONE',  ( 1.000000000000000000, 0.000000000000000000, 0.000000000000000000 ) ) ;
#39789 = CARTESIAN_POINT ( 'NONE',  ( 4.559911319644449179, 62.23035201082150536, -9.422509992056141925 ) ) ;
#39790 = CARTESIAN_POINT ( 'NONE',  ( 0.000000000000000000, 15.00000000000000000, 0.000000000000000000 ) ) ;
#39791 = DIRECTION ( 'NONE',  ( 0.000000000000000000, 0.000000000000000000, 1.000000000000000000 ) ) ;
#39792 = CARTESIAN_POINT ( 'NONE',  ( 10.00000000000000000, 56.81368534415484106, -10.88017736071110342 ) ) ;
#39793 = CARTESIAN_POINT ( 'NONE',  ( 16.40814093676324603, 7.456968003263754419, -11.09922568453594671 ) ) ;
#39794 = DIRECTION ( 'NONE',  ( 0.8320502943378436100, -0.5547001962252291474, 0.000000000000000000 ) ) ;
#39795 = AXIS2_PLACEMENT_3D ( 'NONE', #5203, #19209, #26701 ) ;
#39796 = CARTESIAN_POINT ( 'NONE',  ( 18.52753015748618282, 28.92559781766745175, -4.923371831947291888 ) ) ;
#39797 = CARTESIAN_POINT ( 'NONE',  ( 6.565887622018943937, 65.16530133659709634, 12.81628187352647430 ) ) ;
#39798 = CARTESIAN_POINT ( 'NONE',  ( -0.3689425029237898834, 1.178748834913967869, -10.36894250292378850 ) ) ;
#39799 = CARTESIAN_POINT ( 'NONE',  ( 5.076628168052704559, 15.17559781766745175, -8.527530157486179263 ) ) ;
#39800 = CARTESIAN_POINT ( 'NONE',  ( 6.565887622018943937, 23.08196800326375708, -12.81628187352647608 ) ) ;
#39801 = DIRECTION ( 'NONE',  ( -0.9887436111420608853, -0.1496197561345335991, 0.000000000000000000 ) ) ;
#39802 = CARTESIAN_POINT ( 'NONE',  ( 17.96484262340118221, 51.18868534415483396, -7.964842623401177768 ) ) ;
#39803 = CARTESIAN_POINT ( 'NONE',  ( 1.472469842513823179, 65.59226448433412315, -4.923371831947296329 ) ) ;
#39804 = CARTESIAN_POINT ( 'NONE',  ( 12.34597252984332272, 0.04962896562384134375, 8.076773567935909171 ) ) ;
#39806 = CARTESIAN_POINT ( 'NONE',  ( 12.63842701281683922, 34.55059781766745886, -9.846743663894590881 ) ) ;
#39805 = TOROIDAL_SURFACE ( 'NONE', #87673, 0.5000000000000000000, 0.2500000000000000000 ) ;
#39807 = CARTESIAN_POINT ( 'NONE',  ( 17.20831665107776587, 27.88393115100078390, 7.208316651077764980 ) ) ;
#39808 = CARTESIAN_POINT ( 'NONE',  ( 15.44008868035555793, 16.39701867748817321, -9.422509992056140149 ) ) ;
#39809 = CARTESIAN_POINT ( 'NONE',  ( 13.43411237798106583, 22.66530133659708923, -12.81628187352647252 ) ) ;
#39810 = CARTESIAN_POINT ( 'NONE',  ( 12.63842701281683922, 19.55059781766745175, -9.846743663894590881 ) ) ;
#39811 = CARTESIAN_POINT ( 'NONE',  ( -8.819573739049973327, 87.31373983715974418, 4.675023147224795395 ) ) ;
#39812 = CARTESIAN_POINT ( 'NONE',  ( 7.084665262690076126, 19.10535201082150181, 10.88017736071109987 ) ) ;
#39814 = CARTESIAN_POINT ( 'NONE',  ( 12.91533473730993009, 21.60535201082150536, -10.88017736071109987 ) ) ;
#39813 = CARTESIAN_POINT ( 'NONE',  ( 19.84674366389459266, 38.30059781766745175, 2.638427012816836559 ) ) ;
#39815 = CARTESIAN_POINT ( 'NONE',  ( 4.559911319644449179, 37.23035201082150536, -9.422509992056141925 ) ) ;
#39817 = CARTESIAN_POINT ( 'NONE',  ( 20.04068437667223890, 59.71974360917720048, 6.396802510829770583 ) ) ;
#39816 = CARTESIAN_POINT ( 'NONE',  ( 15.44008868035555260, 14.73035201082150536, 9.422509992056143702 ) ) ;
#39818 = CARTESIAN_POINT ( 'NONE',  ( 17.20831665107776587, 12.88393115100078390, 7.208316651077764980 ) ) ;
#39819 = CARTESIAN_POINT ( 'NONE',  ( 19.84674366389459266, 43.30059781766744464, 2.638427012816836559 ) ) ;
#39820 = DIRECTION ( 'NONE',  ( -1.257402221000611116E-16, 1.000000000000000000, 0.000000000000000000 ) ) ;
#39821 = DIRECTION ( 'NONE',  ( 0.9914448613738104932, 0.000000000000000000, -0.1305261922200514901 ) ) ;
#39822 = AXIS2_PLACEMENT_3D ( 'NONE', #19927, #4937, #12422 ) ;
#39823 = DIRECTION ( 'NONE',  ( 0.000000000000000000, 0.000000000000000000, 1.000000000000000000 ) ) ;
#39824 = CARTESIAN_POINT ( 'NONE',  ( 24.16423886937410614, 29.51208216824729647, -3.795296366450302550 ) ) ;
#39825 = CARTESIAN_POINT ( 'NONE',  ( 18.52753015748617571, 38.09226448433412315, 4.923371831947298993 ) ) ;
#39826 = FACE_OUTER_BOUND ( 'NONE', #57052, .T. ) ;
#39827 = CARTESIAN_POINT ( 'NONE',  ( -4.164238869374099927, 52.01208216824729647, 3.795296366450308767 ) ) ;
#39828 = CARTESIAN_POINT ( 'NONE',  ( 12.63842701281683034, 17.46726448433411250, 9.846743663894596210 ) ) ;
#39830 = CARTESIAN_POINT ( 'NONE',  ( -8.860528122731230027, 87.38741345285838236, -4.488970891313635470 ) ) ;
#39829 = LINE ( 'NONE', #31816, #69019 ) ;
#39831 = CARTESIAN_POINT ( 'NONE',  ( 0.5774900079438590739, 47.64701867748817676, -5.440088680355550821 ) ) ;
#39832 = CARTESIAN_POINT ( 'NONE',  ( 16.40814093676323893, 60.79030133659709634, 11.09922568453595026 ) ) ;
#39833 = CARTESIAN_POINT ( 'NONE',  ( 20.88017736071110519, 15.56368534415483751, 2.639326808657452039E-16 ) ) ;
#39834 = CARTESIAN_POINT ( 'NONE',  ( -2.816281873526473856, 54.33196800326376064, 3.434112377981055619 ) ) ;
#39835 = CARTESIAN_POINT ( 'NONE',  ( 6.565887622018943937, 8.081968003263751754, -12.81628187352647608 ) ) ;
#39836 = CARTESIAN_POINT ( 'NONE',  ( 19.84674366389459266, 18.30059781766745175, 2.638427012816836559 ) ) ;
#39837 = ORIENTED_EDGE ( 'NONE', *, *, #2973, .F. ) ;
#39838 = FILL_AREA_STYLE ('',( #9336 ) ) ;
#39839 = CARTESIAN_POINT ( 'NONE',  ( 0.2751277870542982451, 17.28217586085238011, -6.500000000000002665 ) ) ;
#39840 = CARTESIAN_POINT ( 'NONE',  ( 17.08211943468705130, 53.47041550158063217, 12.26659068614894998 ) ) ;
#39841 = CARTESIAN_POINT ( 'NONE',  ( 17.08211943468705130, 33.47041550158063927, 12.26659068614894998 ) ) ;
#39842 = CARTESIAN_POINT ( 'NONE',  ( 7.084665262690076126, 17.02201867748817676, -10.88017736071110164 ) ) ;
#39843 = CARTESIAN_POINT ( 'NONE',  ( 15.44008868035555793, 36.39701867748816966, -9.422509992056140149 ) ) ;
#39844 = PRESENTATION_STYLE_ASSIGNMENT (( #17833 ) ) ;
#39845 =( GEOMETRIC_REPRESENTATION_CONTEXT ( 3 ) GLOBAL_UNCERTAINTY_ASSIGNED_CONTEXT ( ( #28147 ) ) GLOBAL_UNIT_ASSIGNED_CONTEXT ( ( #33557, #26085, #87557 ) ) REPRESENTATION_CONTEXT ( 'NONE', 'WORKASPACE' ) );
#39846 = CARTESIAN_POINT ( 'NONE',  ( 2.035157376598824452, 68.68868534415484817, 7.964842623401179544 ) ) ;
#39847 = CARTESIAN_POINT ( 'NONE',  ( 8.629999999999995453, 40.74999999999999289, -4.250000000000000000 ) ) ;
#39848 = CARTESIAN_POINT ( 'NONE',  ( 10.00000000000000000, 24.75893115100078745, -9.846743663894594434 ) ) ;
#39849 = CARTESIAN_POINT ( 'NONE',  ( 17.62281668512004629, 18.28593319516823001, 6.499999999999968914 ) ) ;
#39850 = DIRECTION ( 'NONE',  ( 0.000000000000000000, 0.000000000000000000, -1.000000000000000000 ) ) ;
#39851 = CARTESIAN_POINT ( 'NONE',  ( 7.361572987183169658, 14.96726448433411960, -9.846743663894592657 ) ) ;
#39852 = CARTESIAN_POINT ( 'NONE',  ( 1.472469842513823179, 40.59226448433411605, -4.923371831947296329 ) ) ;
#39853 = CIRCLE ( 'NONE', #81373, 0.5000000000000000000 ) ;
#39854 = EDGE_CURVE ( 'NONE', #26202, #16435, #94438, .T. ) ;
#39855 = CARTESIAN_POINT ( 'NONE',  ( 10.00000000000000178, 9.313685344154839285, 10.88017736071110342 ) ) ;
#39856 = CARTESIAN_POINT ( 'NONE',  ( -2.816281873526473856, 29.12363466993041783, 9.499525473075851096E-16 ) ) ;
#39857 = CARTESIAN_POINT ( 'NONE',  ( 10.00000000000000000, 51.81368534415484106, -10.88017736071110342 ) ) ;
#39859 = CARTESIAN_POINT ( 'NONE',  ( 18.52753015748617571, 3.092264484334118269, 4.923371831947298993 ) ) ;
#39858 = CARTESIAN_POINT ( 'NONE',  ( -4.164238869374099927, 52.01208216824729647, 3.795296366450308767 ) ) ;
#39860 = CARTESIAN_POINT ( 'NONE',  ( -2.930023131210801157, 0.000000000000000000, 4.599215049682140233 ) ) ;
#39861 = CARTESIAN_POINT ( 'NONE',  ( 1.472469842513823179, 45.59226448433412315, -4.923371831947296329 ) ) ;
#39863 = CARTESIAN_POINT ( 'NONE',  ( 20.36894250292379382, 13.67874883491396965, 10.36894250292379205 ) ) ;
#39862 = CARTESIAN_POINT ( 'NONE',  ( 18.52753015748618282, 33.92559781766745886, -4.923371831947291888 ) ) ;
#39864 = CARTESIAN_POINT ( 'NONE',  ( 10.00000000000000178, 13.05374883491396787, 14.16423886937410082 ) ) ;
#39865 = CARTESIAN_POINT ( 'NONE',  ( 17.96484262340118221, 44.93868534415483396, 7.964842623401181321 ) ) ;
#39866 = CARTESIAN_POINT ( 'NONE',  ( 2.035157376598822676, 7.438685344154837509, -7.964842623401177768 ) ) ;
#39867 = CARTESIAN_POINT ( 'NONE',  ( 12.91533473730993009, 41.60535201082149825, -10.88017736071109987 ) ) ;
#39868 = CARTESIAN_POINT ( 'NONE',  ( 19.42250999205614548, 25.98035201082150891, -5.440088680355545492 ) ) ;
#39869 = ORIENTED_EDGE ( 'NONE', *, *, #60444, .F. ) ;
#39870 = CARTESIAN_POINT ( 'NONE',  ( 6.565887622018943937, 35.16530133659708923, 12.81628187352647430 ) ) ;
#39871 = CARTESIAN_POINT ( 'NONE',  ( 7.084665262690076126, 37.02201867748817676, -10.88017736071110164 ) ) ;
#39872 = ORIENTED_EDGE ( 'NONE', *, *, #94394, .T. ) ;
#39873 = CARTESIAN_POINT ( 'NONE',  ( -2.816281873526471635, 63.91530133659708923, -3.434112377981056508 ) ) ;
#39874 = CARTESIAN_POINT ( 'NONE',  ( 17.96484262340118221, 46.18868534415484106, -7.964842623401177768 ) ) ;
#39875 = ORIENTED_EDGE ( 'NONE', *, *, #44189, .F. ) ;
#39876 = CARTESIAN_POINT ( 'NONE',  ( 0.5774900079438607392, 48.48035201082150536, 5.440088680355550821 ) ) ;
#39877 = CARTESIAN_POINT ( 'NONE',  ( 20.88017736071110164, 5.355352010821502695, 2.915334737309930979 ) ) ;
#39878 = EDGE_CURVE ( 'NONE', #67069, #61160, #76711, .T. ) ;
#39879 = LINE ( 'NONE', #9881, #91511 ) ;
#39880 = CARTESIAN_POINT ( 'NONE',  ( 12.50465990577749409, 56.99999999999999289, 3.000000000000000000 ) ) ;
#39881 = CARTESIAN_POINT ( 'NONE',  ( -4.164238869374099039, 56.80374883491397497, 8.674139862899312516E-16 ) ) ;
#39882 = CARTESIAN_POINT ( 'NONE',  ( 19.42250999205614548, 60.98035201082151247, -5.440088680355545492 ) ) ;
#39883 = CARTESIAN_POINT ( 'NONE',  ( 13.79529636645030344, 3.262082168247301350, 14.16423886937410614 ) ) ;
#39884 = EDGE_CURVE ( 'NONE', #25163, #64978, #68732, .T. ) ;
#39885 = FACE_OUTER_BOUND ( 'NONE', #31002, .T. ) ;
#39886 = CARTESIAN_POINT ( 'NONE',  ( 19.42250999205614548, 15.98035201082150714, -5.440088680355545492 ) ) ;
#39887 = CARTESIAN_POINT ( 'NONE',  ( 17.20831665107776587, 42.88393115100077324, 7.208316651077764980 ) ) ;
#39888 = ORIENTED_EDGE ( 'NONE', *, *, #24777, .F. ) ;
#39889 = CIRCLE ( 'NONE', #68654, 15.00000000000000000 ) ;
#39890 = CARTESIAN_POINT ( 'NONE',  ( 18.52753015748617571, 43.09226448433412315, 4.923371831947298993 ) ) ;
#39891 = CARTESIAN_POINT ( 'NONE',  ( 2.035157376598824452, 63.68868534415484106, 7.964842623401179544 ) ) ;
#39892 = CARTESIAN_POINT ( 'NONE',  ( 20.88017736071110519, 40.56368534415484106, 2.639326808657452039E-16 ) ) ;
#39893 = CARTESIAN_POINT ( 'NONE',  ( 14.92337183194729633, 32.67559781766745175, 8.527530157486181039 ) ) ;
#39895 = CARTESIAN_POINT ( 'NONE',  ( 6.382347221874381304, 14.49999999999999112, 13.57444820018236520 ) ) ;
#39894 = CARTESIAN_POINT ( 'NONE',  ( -13.95749458852084146, 0.2306972965111889207, 5.331641351772924864 ) ) ;
#39896 = CARTESIAN_POINT ( 'NONE',  ( 4.559911319644449179, 52.23035201082151247, -9.422509992056141925 ) ) ;
#39897 = CARTESIAN_POINT ( 'NONE',  ( 2.917880565312948704, 62.63708216824730357, 12.26659068614894643 ) ) ;
#39898 = CARTESIAN_POINT ( 'NONE',  ( 16.40814093676324603, 22.45696800326375353, -11.09922568453594671 ) ) ;
#39899 = DIRECTION ( 'NONE',  ( 0.000000000000000000, 0.000000000000000000, 1.000000000000000000 ) ) ;
#39900 = ORIENTED_EDGE ( 'NONE', *, *, #44473, .T. ) ;
#39901 = CARTESIAN_POINT ( 'NONE',  ( 6.565887622018943937, 33.08196800326374643, -12.81628187352647608 ) ) ;
#39902 = CARTESIAN_POINT ( 'NONE',  ( 19.42250999205614193, 25.14701867748817321, 5.440088680355555262 ) ) ;
#39903 = ORIENTED_EDGE ( 'NONE', *, *, #9513, .T. ) ;
#39904 = CARTESIAN_POINT ( 'NONE',  ( 0.000000000000000000, 0.5000000000000004441, 0.000000000000000000 ) ) ;
#39905 = VECTOR ( 'NONE', #46331, 1000.000000000000000 ) ;
#39906 = EDGE_CURVE ( 'NONE', #89546, #71139, #49107, .T. ) ;
#39907 = CARTESIAN_POINT ( 'NONE',  ( 20.88017736071110164, 65.35535201082150536, 2.915334737309930979 ) ) ;
#39908 = CARTESIAN_POINT ( 'NONE',  ( 19.84674366389459266, 43.30059781766744464, 2.638427012816836559 ) ) ;
#39910 = CARTESIAN_POINT ( 'NONE',  ( 5.076628168052703671, 31.84226448433412315, 8.527530157486179263 ) ) ;
#39909 = CARTESIAN_POINT ( 'NONE',  ( 0.1532563361054082862, 6.217264484334118713, 2.638427012816831674 ) ) ;
#39911 = CARTESIAN_POINT ( 'NONE',  ( -10.91596227336299663, -97.59461837500816728, 3.749999999999999556 ) ) ;
#39912 = FACE_OUTER_BOUND ( 'NONE', #17732, .T. ) ;
#39913 = CARTESIAN_POINT ( 'NONE',  ( 12.63842701281683034, 27.46726448433411250, 9.846743663894596210 ) ) ;
#39914 = FACE_OUTER_BOUND ( 'NONE', #70242, .T. ) ;
#39915 = DIRECTION ( 'NONE',  ( -0.9537169507482258224, 0.000000000000000000, -0.3007057995042767273 ) ) ;
#39916 = ADVANCED_FACE ( 'NONE', ( #75729 ), #46702, .F. ) ;
#39917 = CARTESIAN_POINT ( 'NONE',  ( 17.20831665107776587, 27.88393115100078390, 7.208316651077764980 ) ) ;
#39918 = FACE_OUTER_BOUND ( 'NONE', #42936, .T. ) ;
#39920 = ORIENTED_EDGE ( 'NONE', *, *, #88957, .T. ) ;
#39919 = CARTESIAN_POINT ( 'NONE',  ( 0.1532563361054083140, 51.00893115100078745, 1.131784320476157264E-15 ) ) ;
#39921 = B_SPLINE_CURVE_WITH_KNOTS ( 'NONE', 3,
 ( #32091, #36551, #28547, #89048, #42087, #20054, #28046, #20559 ),
 .UNSPECIFIED., .F., .F.,
 ( 4, 2, 2, 4 ),
 ( 0.009612260643802141014, 0.01201872016511521847, 0.01442517968642829593, 0.01923809872905445084 ),
 .UNSPECIFIED. ) ;
#39922 = CARTESIAN_POINT ( 'NONE',  ( -0.9082943533638192513, 4.617951328659527895E-16, 14.47152380945584582 ) ) ;
#39923 = CARTESIAN_POINT ( 'NONE',  ( 6.565887622018943937, 28.08196800326375353, -12.81628187352647608 ) ) ;
#39924 = FACE_OUTER_BOUND ( 'NONE', #43386, .T. ) ;
#39925 = CARTESIAN_POINT ( 'NONE',  ( 17.08211943468705130, 48.47041550158063927, 12.26659068614894998 ) ) ;
#39926 = CARTESIAN_POINT ( 'NONE',  ( 10.00000000000000000, 24.75893115100078745, -9.846743663894594434 ) ) ;
#39927 = CARTESIAN_POINT ( 'NONE',  ( 10.00000000000000000, -0.2410688489992152128, -9.846743663894594434 ) ) ;
#39928 = CARTESIAN_POINT ( 'NONE',  ( 19.59242374975054446, 95.44328903796339603, 5.127491817726292034 ) ) ;
#39929 = CARTESIAN_POINT ( 'NONE',  ( 13.79529636645030344, 38.26208216824729647, 14.16423886937410614 ) ) ;
#39930 = CARTESIAN_POINT ( 'NONE',  ( 7.361572987183169658, 64.96726448433412315, -9.846743663894592657 ) ) ;
#39931 = CARTESIAN_POINT ( 'NONE',  ( 24.16423886937410614, 59.51208216824728936, -3.795296366450302550 ) ) ;
#39932 = CARTESIAN_POINT ( 'NONE',  ( -4.164238869374099039, 26.80374883491397142, 8.674139862899312516E-16 ) ) ;
#39933 = CARTESIAN_POINT ( 'NONE',  ( 22.26659068614894466, 23.88708216824730357, 7.082119434687054849 ) ) ;
#39934 = CARTESIAN_POINT ( 'NONE',  ( 13.48255862861920562, 15.00000000000000000, 5.335786055104250636 ) ) ;
#39936 = CARTESIAN_POINT ( 'NONE',  ( 2.791683348922240793, 61.63393115100079456, 7.208316651077764092 ) ) ;
#39935 = CARTESIAN_POINT ( 'NONE',  ( 20.00000000000000711, 105.0000000000000000, 5.000000000000000000 ) ) ;
#39937 = CARTESIAN_POINT ( 'NONE',  ( 12.91533473730993009, 31.60535201082150891, -10.88017736071109987 ) ) ;
#39938 = CYLINDRICAL_SURFACE ( 'NONE', #63420, 11.92686044187656513 ) ;
#39939 = CARTESIAN_POINT ( 'NONE',  ( 8.956109388601815269, -3.116898856182344080, 3.750000000000001332 ) ) ;
#39940 = CARTESIAN_POINT ( 'NONE',  ( 2.791683348922240793, 36.63393115100078035, 7.208316651077764092 ) ) ;
#39941 = CARTESIAN_POINT ( 'NONE',  ( 0.6178305044545838731, 49.74863466993041072, 9.382169495545420901 ) ) ;
#39942 = CARTESIAN_POINT ( 'NONE',  ( -14.16423886937410437, -3.404584498419356731, -3.795296366450299885 ) ) ;
#39943 = CARTESIAN_POINT ( 'NONE',  ( 19.84674366389459621, 48.50893115100078745, 7.409399052514197653E-17 ) ) ;
#39944 = CARTESIAN_POINT ( 'NONE',  ( -6.000000000000014211, 80.07179676972448590, -4.250000000000000000 ) ) ;
#39945 = ORIENTED_EDGE ( 'NONE', *, *, #31738, .T. ) ;
#39946 = CARTESIAN_POINT ( 'NONE',  ( -4.164238869374098151, 16.59541550158063927, -3.795296366450310543 ) ) ;
#39947 = CARTESIAN_POINT ( 'NONE',  ( -12.83294900548055573, 14.63606878838274206, -7.766300266068574487 ) ) ;
#39949 = LINE ( 'NONE', #24468, #15353 ) ;
#39948 = CARTESIAN_POINT ( 'NONE',  ( -0.7117905103455194338, 0.000000000000000000, 5.406585696355428183 ) ) ;
#39950 = CARTESIAN_POINT ( 'NONE',  ( 2.035157376598822676, 2.438685344154838397, -7.964842623401177768 ) ) ;
#39951 = CARTESIAN_POINT ( 'NONE',  ( 16.40814093676323893, 5.790301336597087456, 11.09922568453595026 ) ) ;
#39952 = CARTESIAN_POINT ( 'NONE',  ( 14.35840480524197282, 15.00000000000000000, 4.340070442838948495 ) ) ;
#39953 = CARTESIAN_POINT ( 'NONE',  ( 15.44008868035555793, 66.39701867748817676, -9.422509992056140149 ) ) ;
#39954 = DIRECTION ( 'NONE',  ( -0.000000000000000000, -0.000000000000000000, 1.000000000000000000 ) ) ;
#39955 = CIRCLE ( 'NONE', #22412, 1.500000000000001332 ) ;
#39956 = DIRECTION ( 'NONE',  ( 0.9890158633619168249, 0.000000000000000000, 0.1478094111296113511 ) ) ;
#39957 = CARTESIAN_POINT ( 'NONE',  ( 14.99999999999998046, 70.25000000000000000, -6.500000000000000888 ) ) ;
#39958 = CARTESIAN_POINT ( 'NONE',  ( -4.164238869374098151, 61.59541550158063217, -3.795296366450310543 ) ) ;
#39959 = DIRECTION ( 'NONE',  ( 0.000000000000000000, 0.000000000000000000, 1.000000000000000000 ) ) ;
#39960 = CARTESIAN_POINT ( 'NONE',  ( 0.5774900079438590739, 32.64701867748816966, -5.440088680355550821 ) ) ;
#39961 = CARTESIAN_POINT ( 'NONE',  ( 4.559911319644449179, 38.89701867748817676, 9.422509992056141925 ) ) ;
#39962 = CARTESIAN_POINT ( 'NONE',  ( -2.816281873526471635, 3.915301336597087456, -3.434112377981056508 ) ) ;
#39963 = CARTESIAN_POINT ( 'NONE',  ( 2.791683348922240793, 56.63393115100078035, 7.208316651077764092 ) ) ;
#39964 = CARTESIAN_POINT ( 'NONE',  ( 3.591859063236763294, 63.29030133659708923, -11.09922568453595026 ) ) ;
#39965 = CARTESIAN_POINT ( 'NONE',  ( 14.40939250469964961, 3.793246902777681429E-16, 1.618458416365853747 ) ) ;
#39967 = ORIENTED_EDGE ( 'NONE', *, *, #22255, .F. ) ;
#39966 = TOROIDAL_SURFACE ( 'NONE', #38401, 7.250000000000002665, 0.2500000000000000000 ) ;
#39968 = CARTESIAN_POINT ( 'NONE',  ( -0.8801773607111008646, 33.27201867748817676, 2.915334737309923430 ) ) ;
#39969 = EDGE_CURVE ( 'NONE', #34886, #71042, #40792, .T. ) ;
#39970 = CARTESIAN_POINT ( 'NONE',  ( 10.00000000000000000, 32.87363466993042493, -12.81628187352647608 ) ) ;
#39971 = CARTESIAN_POINT ( 'NONE',  ( 12.60874940350942985, 3.897725180921639224E-16, 7.160268045227119238 ) ) ;
#39972 = CARTESIAN_POINT ( 'NONE',  ( 5.076628168052704559, 65.17559781766745175, -8.527530157486179263 ) ) ;
#39973 = EDGE_CURVE ( 'NONE', #69208, #76544, #84716, .T. ) ;
#39974 = CARTESIAN_POINT ( 'NONE',  ( 12.91533473730993009, 46.60535201082150536, -10.88017736071109987 ) ) ;
#39975 = CARTESIAN_POINT ( 'NONE',  ( 12.63842701281683922, 14.55059781766744997, -9.846743663894590881 ) ) ;
#39976 = CARTESIAN_POINT ( 'NONE',  ( 16.40814093676324603, 37.45696800326376064, -11.09922568453594671 ) ) ;
#39978 = DIRECTION ( 'NONE',  ( 0.000000000000000000, 1.000000000000000000, 0.000000000000000000 ) ) ;
#39977 = CARTESIAN_POINT ( 'NONE',  ( 15.44008868035555793, 66.39701867748817676, -9.422509992056140149 ) ) ;
#39979 = FILL_AREA_STYLE ('',( #8980 ) ) ;
#39980 = CARTESIAN_POINT ( 'NONE',  ( 21.09922568453594849, 61.20696800326376064, 6.408140936763242479 ) ) ;
#39981 = VERTEX_POINT ( 'NONE', #29725 ) ;
#39982 = CARTESIAN_POINT ( 'NONE',  ( 3.836325488036083087, 0.5000000000000004441, 14.50112432709425114 ) ) ;
#39983 = SURFACE_SIDE_STYLE ('',( #17974 ) ) ;
#39984 = CARTESIAN_POINT ( 'NONE',  ( 17.96484262340118221, 11.18868534415483929, -7.964842623401177768 ) ) ;
#39986 = CARTESIAN_POINT ( 'NONE',  ( -2.266590686148945544, 11.38708216824730179, -7.082119434687050408 ) ) ;
#39985 = CARTESIAN_POINT ( 'NONE',  ( 3.591859063236761518, 49.95696800326375353, 11.09922568453594849 ) ) ;
#39987 = CARTESIAN_POINT ( 'NONE',  ( 18.52753015748618282, 23.92559781766745530, -4.923371831947291888 ) ) ;
#39988 = CARTESIAN_POINT ( 'NONE',  ( 17.20831665107776587, 17.88393115100078745, 7.208316651077764980 ) ) ;
#39989 = CARTESIAN_POINT ( 'NONE',  ( -4.164238869374099039, 56.80374883491397497, 8.674139862899312516E-16 ) ) ;
#39990 = VERTEX_POINT ( 'NONE', #68248 ) ;
#39991 = CARTESIAN_POINT ( 'NONE',  ( 12.91533473730993009, 21.60535201082150536, -10.88017736071109987 ) ) ;
#39992 = FACE_OUTER_BOUND ( 'NONE', #82147, .T. ) ;
#39993 = VERTEX_POINT ( 'NONE', #76232 ) ;
#39994 = ORIENTED_EDGE ( 'NONE', *, *, #15254, .F. ) ;
#39995 = CARTESIAN_POINT ( 'NONE',  ( 10.00000000000000000, 16.81368534415483751, -10.88017736071110342 ) ) ;
#39996 = CARTESIAN_POINT ( 'NONE',  ( 7.084665262690076126, 7.022018677488170546, -10.88017736071110164 ) ) ;
#39997 = CARTESIAN_POINT ( 'NONE',  ( 0.1532563361054100626, 55.80059781766745175, -2.638427012816831230 ) ) ;
#39998 = EDGE_CURVE ( 'NONE', #52968, #49408, #61244, .T. ) ;
#39999 = CARTESIAN_POINT ( 'NONE',  ( 16.40814093676323893, 55.79030133659708923, 11.09922568453595026 ) ) ;
#40000 = DIRECTION ( 'NONE',  ( 0.000000000000000000, 0.000000000000000000, -1.000000000000000000 ) ) ;
#40002 = CARTESIAN_POINT ( 'NONE',  ( -4.164238869374099927, 17.01208216824730357, 3.795296366450308767 ) ) ;
#40001 = CARTESIAN_POINT ( 'NONE',  ( -9.997910040112669705, 15.00000000000000000, 10.50199004140708325 ) ) ;
#40003 = CARTESIAN_POINT ( 'NONE',  ( 12.91533473730993009, 31.60535201082150891, -10.88017736071109987 ) ) ;
#40004 = CARTESIAN_POINT ( 'NONE',  ( 22.26659068614894466, 63.88708216824730357, 7.082119434687054849 ) ) ;
#40005 = CARTESIAN_POINT ( 'NONE',  ( 10.00000000000000178, 62.25893115100078745, 9.846743663894594434 ) ) ;
#40006 = CYLINDRICAL_SURFACE ( 'NONE', #58780, 4.000000000000003553 ) ;
#40007 = CARTESIAN_POINT ( 'NONE',  ( 0.1532563361054083140, 31.00893115100078390, 1.131784320476157264E-15 ) ) ;
#40008 = EDGE_CURVE ( 'NONE', #8159, #95321, #90230, .T. ) ;
#40009 = CARTESIAN_POINT ( 'NONE',  ( 1.472469842513823179, 6.425597817667451750, 4.923371831947296329 ) ) ;
#40010 = CARTESIAN_POINT ( 'NONE',  ( -12.81628187352647252, -40.66803199673623936, 3.434112377981066722 ) ) ;
#40011 = VERTEX_POINT ( 'NONE', #67248 ) ;
#40012 = CARTESIAN_POINT ( 'NONE',  ( 0.5774900079438607392, 3.480352010821504027, 5.440088680355550821 ) ) ;
#40013 = CARTESIAN_POINT ( 'NONE',  ( -0.8801773607110991993, 67.85535201082151957, -2.915334737309923874 ) ) ;
#40014 = CARTESIAN_POINT ( 'NONE',  ( 19.38216949554541557, 2.248634669930420049, -9.382169495545420901 ) ) ;
#40015 = CARTESIAN_POINT ( 'NONE',  ( 2.035157376598822676, 42.43868534415483396, -7.964842623401177768 ) ) ;
#40017 = CARTESIAN_POINT ( 'NONE',  ( -1.099225684535947600, 38.70696800326375353, -6.408140936763238038 ) ) ;
#40016 = CARTESIAN_POINT ( 'NONE',  ( 2.035157376598822676, 12.43868534415483751, -7.964842623401177768 ) ) ;
#40018 = CARTESIAN_POINT ( 'NONE',  ( 22.26659068614895176, 19.72041550158063572, -7.082119434687042414 ) ) ;
#40019 =( BOUNDED_SURFACE ( )  B_SPLINE_SURFACE ( 1, 2, ( 
 ( #89410, #74899, #83396, #59891, #6397, #36912, #97933, #52399, #75388, #20926, #6906, #37418, #14916, #45386, #75892, #38891, #901, #23404, #16380, #85363, #7900, #23894, #8383, #53888, #15893, #77355, #84394, #39866, #17374, #61372, #46379, #76385, #62350, #69379, #38395, #8866, #16875, #31363, #61863, #47844, #93350, #1397, #68897, #92854, #39382, #69877, #47351, #53378, #91882, #91380, #76867, #83888, #60880, #24382, #31852, #425, #92368, #54849, #55357, #77852, #62852, #54361, #70373, #30876, #22908, #9362, #1890, #84871, #78348, #46863, #32349, #24875, #85862, #37912, #68400, #98921, #30377, #15417, #45899, #25372, #41367, #2384, #40367, #64312, #48826, #41845, #94823, #78844, #3842, #88311, #26327, #3343, #10355, #71834, #19809, #70868, #40854, #71358, #33325, #86353, #42324, #11326, #17855, #56824, #57804, #57312, #50299, #86844, #18348, #80317, #18840, #34301, #32838, #2876, #63820, #94332, #9869, #63340, #26819, #10846, #25851, #72798, #79336, #64799, #95823, #65296, #93845, #55857, #33805, #48341, #95317, #87323, #49320, #79824, #4337, #56348, #72311, #87804, #19326, #49809, #34807, #11817, #27304, #73791, #50811, #22298, #96823, #60275, #6296, #27800, #82783, #51298, #44774, #28787, #81302, #13797, #74787, #36798, #90774, #36297, #20313, #90270, #66794, #12797, #59777, #75280, #58285, #65793, #58792, #67292, #21804, #80812, #42818, #43298, #5322, #35801, #88803, #14303, #82280, #66288, #97314, #29767, #29281, #12310, #89299, #20810, #52284, #89784, #97819, #73302, #28299, #81783, #13297, #4826, #35301, #6790, #43784, #74277, #37304, #5805, #67791, #98313, #96327, #59286, #21301, #51793, #44283, #39271, #84281, #15781, #61259, #85253, #76272, #91766, #98812, #23782, #1772, #47233, #14805, #54248, #45780, #22790, #93230, #68779, #32229, #77245, #30261, #54733, #23288, #16759, #791, #53267, #84760, #46749, #8752, #62729, #8273, #91265, #62237, #38770, #83773, #31742, #77737, #60764, #37793, #30752, #69760, #92744, #1288, #16268, #24268, #9248, #68291, #7789, #7293, #53766, #15297, #75772, #39757, #70257, #38284, #310, #52772, #83281, #45277, #46270, #76755, #69272, #31245, #61741, #92259, #3231, #40735, #57194, #56236, #79216, #94713, #93726, #10242, #33215, #86235, #49208, #72201, #32724, #9744, #2762, #85747, #55232, #25744, #71238, #71721, #86730, #63222, #33697, #95192, #18232, #63710, #25258, #94213, #10728, #55744, #64196, #48714, #41244, #26220, #56713, #70754, #87204, #34190, #18728, #79712, #11211, #41730, #3729, #64683, #24755, #26700, #47734, #17259, #78231, #40245, #2268, #17746, #48223, #78732 ),
 ( #15604, #621, #39582, #32548, #55046, #40062, #46569, #47560, #46089, #38108, #85566, #9069, #54067, #55561, #1097, #54553, #32043, #76574, #23602, #77068, #69088, #17078, #70562, #84090, #30574, #8580, #7615, #45588, #69578, #84581, #47054, #31560, #8094, #70073, #93546, #62056, #39084, #38590, #92558, #25078, #76085, #31067, #61567, #92077, #91589, #78058, #16579, #23103, #24085, #63049, #62545, #15111, #16082, #85070, #9560, #77552, #1593, #68597, #93051, #24585, #2088, #125, #61078, #53576, #72568, #19094, #64570, #43923, #4104, #59421, #18608, #18125, #28918, #5949, #87581, #34567, #13946, #94595, #67431, #34077, #48598, #25628, #95081, #56606, #66933, #79102, #3126, #11103, #11589, #79601, #42106, #64080, #26585, #26112, #65061, #74420, #49574, #80084, #6425, #82422, #89438, #87095, #81928, #20951, #10614, #95588, #27073, #86615, #44421, #33585, #41126, #56118, #89925, #71615, #49097, #58938, #51438, #36440, #41621, #72087, #3612, #13436, #21440, #74926, #57087, #97454, #51938, #36937, #54380, #97954, #38911, #84894, #39404, #7437, #53400, #69398, #90906, #61882, #15910, #23912, #92386, #29410, #920, #37439, #91900, #14440, #46883, #29906, #31382, #59915, #76890, #37933, #45917, #91404, #68422, #46400, #76405, #16404, #22435, #90404, #77375, #8402, #60903, #7921, #8888, #67930, #21945, #98945, #52422, #82922, #30399, #60412, #44910, #75416, #6931, #83418, #83909, #52906, #15438, #98450, #68916, #14938, #23425, #38418, #22932, #53904, #444, #45406, #30896, #75912, #84412, #61390, #2405, #25392, #40877, #86862, #11346, #48849, #1417, #55875, #94353, #71383, #70887, #32863, #55382, #48358, #18368, #39887, #86374, #40390, #85882, #47863, #10375, #17395, #71853, #49342, #93370, #78369, #9382, #25871, #9888, #63361, #24897, #41386, #94845, #70391, #85383, #93864, #62369, #31870, #17876, #78865, #2895, #33345, #1910, #63839, #79841, #56370, #79358, #32368, #10865, #69897, #92873, #62873, #3363, #33827, #47374, #64334, #26346, #77872, #56847, #18861, #87346, #24405, #54873, #16897, #13316, #50829, #35820, #34323, #11838, #72822, #42345, #82297, #41866, #58810, #89800, #65814, #42836, #35319, #96844, #28804, #97332, #21319, #72329, #73320, #57331, #28318, #4843, #96346, #50317, #74296, #65316, #80832, #87827, #12817, #51810, #36316, #3862, #43315, #34826, #4360, #64821, #57823, #95338, #66307, #19345, #43803, #12332, #5823, #88821, #95842, #73809, #89319, #20827, #26837, #27819, #80340, #51316, #58304, #27327, #81799, #66810, #49828, #88332, #19829, #59303, #20333, #81322, #5342, #15315, #91785, #29298, #67812, #67308 ) ),
 .UNSPECIFIED., .F., .F., .F. ) 
 B_SPLINE_SURFACE_WITH_KNOTS ( ( 2, 2 ),
 ( 3, 2, 2, 2, 2, 2, 2, 2, 2, 2, 2, 2, 2, 2, 2, 2, 2, 2, 2, 2, 2, 2, 2, 2, 2, 2, 2, 2, 2, 2, 2, 2, 2, 2, 2, 2, 2, 2, 2, 2, 2, 2, 2, 2, 2, 2, 2, 2, 2, 2, 2, 2, 2, 2, 2, 2, 2, 2, 2, 2, 2, 2, 2, 2, 2, 2, 2, 2, 2, 2, 2, 2, 2, 2, 2, 2, 2, 2, 2, 2, 2, 2, 2, 2, 2, 2, 2, 2, 2, 2, 2, 2, 2, 2, 2, 2, 2, 2, 2, 2, 2, 2, 2, 2, 2, 2, 2, 2, 2, 2, 2, 2, 2, 2, 2, 2, 2, 2, 2, 2, 2, 2, 2, 2, 2, 2, 2, 2, 2, 2, 2, 2, 2, 2, 2, 2, 2, 2, 2, 2, 2, 2, 2, 2, 2, 2, 2, 2, 2, 2, 2, 2, 2, 2, 2, 2, 2, 2, 2, 2, 2, 2, 3 ),
 ( 0.000000000000000000, 1.000000000000000000 ),
 ( 0.000000000000000000, 0.005952380952380952051, 0.01190476190476190410, 0.01785714285714285615, 0.02380952380952380820, 0.02976190476190476025, 0.03571428571428571230, 0.04166666666666666435, 0.04761904761904761640, 0.05357142857142856845, 0.05952380952380952051, 0.06547619047619047949, 0.07142857142857142461, 0.07738095238095238360, 0.08333333333333332871, 0.08928571428571428770, 0.09523809523809523281, 0.1011904761904761918, 0.1071428571428571369, 0.1130952380952380959, 0.1190476190476190410, 0.1250000000000000000, 0.1309523809523809590, 0.1369047619047619180, 0.1428571428571428492, 0.1488095238095238082, 0.1547619047619047672, 0.1607142857142857262, 0.1666666666666666574, 0.1726190476190476164, 0.1785714285714285754, 0.1845238095238095344, 0.1904761904761904656, 0.1964285714285714246, 0.2023809523809523836, 0.2083333333333333426, 0.2142857142857142738, 0.2202380952380952328, 0.2261904761904761918, 0.2321428571428571508, 0.2380952380952380820, 0.2440476190476190410, 0.2500000000000000000, 0.2559523809523809312, 0.2619047619047619180, 0.2678571428571428492, 0.2738095238095238360, 0.2797619047619047672, 0.2857142857142856984, 0.2916666666666666852, 0.2976190476190476164, 0.3035714285714285476, 0.3095238095238095344, 0.3154761904761904656, 0.3214285714285714524, 0.3273809523809523836, 0.3333333333333333148, 0.3392857142857143016, 0.3452380952380952328, 0.3511904761904761640, 0.3571428571428571508, 0.3630952380952380820, 0.3690476190476190688, 0.3750000000000000000, 0.3809523809523809312, 0.3869047619047619180, 0.3928571428571428492, 0.3988095238095238360, 0.4047619047619047672, 0.4107142857142856984, 0.4166666666666666852, 0.4226190476190476164, 0.4285714285714285476, 0.4345238095238095344, 0.4404761904761904656, 0.4464285714285714524, 0.4523809523809523836, 0.4583333333333333148, 0.4642857142857143016, 0.4702380952380952328, 0.4761904761904761640, 0.4821428571428571508, 0.4880952380952380820, 0.4940476190476190688, 0.5000000000000000000, 0.5059523809523809312, 0.5119047619047618625, 0.5178571428571429047, 0.5238095238095238360, 0.5297619047619047672, 0.5357142857142856984, 0.5416666666666666297, 0.5476190476190476719, 0.5535714285714286031, 0.5595238095238095344, 0.5654761904761904656, 0.5714285714285713969, 0.5773809523809523281, 0.5833333333333333703, 0.5892857142857143016, 0.5952380952380952328, 0.6011904761904761640, 0.6071428571428570953, 0.6130952380952381375, 0.6190476190476190688, 0.6250000000000000000, 0.6309523809523809312, 0.6369047619047618625, 0.6428571428571429047, 0.6488095238095238360, 0.6547619047619047672, 0.6607142857142856984, 0.6666666666666666297, 0.6726190476190476719, 0.6785714285714286031, 0.6845238095238095344, 0.6904761904761904656, 0.6964285714285713969, 0.7023809523809523281, 0.7083333333333333703, 0.7142857142857143016, 0.7202380952380952328, 0.7261904761904761640, 0.7321428571428570953, 0.7380952380952381375, 0.7440476190476190688, 0.7500000000000000000, 0.7559523809523809312, 0.7619047619047618625, 0.7678571428571429047, 0.7738095238095238360, 0.7797619047619047672, 0.7857142857142856984, 0.7916666666666666297, 0.7976190476190476719, 0.8035714285714286031, 0.8095238095238095344, 0.8154761904761904656, 0.8214285714285713969, 0.8273809523809523281, 0.8333333333333333703, 0.8392857142857143016, 0.8452380952380952328, 0.8511904761904761640, 0.8571428571428570953, 0.8630952380952381375, 0.8690476190476190688, 0.8750000000000000000, 0.8809523809523809312, 0.8869047619047618625, 0.8928571428571429047, 0.8988095238095238360, 0.9047619047619047672, 0.9107142857142856984, 0.9166666666666666297, 0.9226190476190476719, 0.9285714285714286031, 0.9345238095238095344, 0.9404761904761904656, 0.9464285714285713969, 0.9523809523809523281, 0.9583333333333333703, 0.9642857142857143016 ),
 .UNSPECIFIED. ) 
 GEOMETRIC_REPRESENTATION_ITEM ( )  RATIONAL_B_SPLINE_SURFACE ( (
 ( 1.000000000000000000, 0.9659258262890683122, 1.000000000000000000, 0.9659258262890683122, 1.000000000000000000, 0.9659258262890683122, 1.000000000000000000, 0.9659258262890683122, 1.000000000000000000, 0.9659258262890683122, 1.000000000000000000, 0.9659258262890683122, 1.000000000000000000, 0.9659258262890683122, 1.000000000000000000, 0.9659258262890683122, 1.000000000000000000, 0.9659258262890683122, 1.000000000000000000, 0.9659258262890683122, 1.000000000000000000, 0.9659258262890683122, 1.000000000000000000, 0.9659258262890683122, 1.000000000000000000, 0.9659258262890683122, 1.000000000000000000, 0.9659258262890683122, 1.000000000000000000, 0.9659258262890683122, 1.000000000000000000, 0.9659258262890683122, 1.000000000000000000, 0.9659258262890683122, 1.000000000000000000, 0.9659258262890683122, 1.000000000000000000, 0.9659258262890683122, 1.000000000000000000, 0.9659258262890683122, 1.000000000000000000, 0.9659258262890683122, 1.000000000000000000, 0.9659258262890683122, 1.000000000000000000, 0.9659258262890683122, 1.000000000000000000, 0.9659258262890683122, 1.000000000000000000, 0.9659258262890683122, 1.000000000000000000, 0.9659258262890683122, 1.000000000000000000, 0.9659258262890683122, 1.000000000000000000, 0.9659258262890683122, 1.000000000000000000, 0.9659258262890683122, 1.000000000000000000, 0.9659258262890683122, 1.000000000000000000, 0.9659258262890683122, 1.000000000000000000, 0.9659258262890683122, 1.000000000000000000, 0.9659258262890683122, 1.000000000000000000, 0.9659258262890683122, 1.000000000000000000, 0.9659258262890683122, 1.000000000000000000, 0.9659258262890683122, 1.000000000000000000, 0.9659258262890683122, 1.000000000000000000, 0.9659258262890683122, 1.000000000000000000, 0.9659258262890683122, 1.000000000000000000, 0.9659258262890683122, 1.000000000000000000, 0.9659258262890683122, 1.000000000000000000, 0.9659258262890683122, 1.000000000000000000, 0.9659258262890683122, 1.000000000000000000, 0.9659258262890683122, 1.000000000000000000, 0.9659258262890683122, 1.000000000000000000, 0.9659258262890683122, 1.000000000000000000, 0.9659258262890683122, 1.000000000000000000, 0.9659258262890683122, 1.000000000000000000, 0.9659258262890683122, 1.000000000000000000, 0.9659258262890683122, 1.000000000000000000, 0.9659258262890683122, 1.000000000000000000, 0.9659258262890683122, 1.000000000000000000, 0.9659258262890683122, 1.000000000000000000, 0.9659258262890683122, 1.000000000000000000, 0.9659258262890683122, 1.000000000000000000, 0.9659258262890683122, 1.000000000000000000, 0.9659258262890683122, 1.000000000000000000, 0.9659258262890683122, 1.000000000000000000, 0.9659258262890683122, 1.000000000000000000, 0.9659258262890683122, 1.000000000000000000, 0.9659258262890683122, 1.000000000000000000, 0.9659258262890683122, 1.000000000000000000, 0.9659258262890683122, 1.000000000000000000, 0.9659258262890683122, 1.000000000000000000, 0.9659258262890683122, 1.000000000000000000, 0.9659258262890683122, 1.000000000000000000, 0.9659258262890683122, 1.000000000000000000, 0.9659258262890683122, 1.000000000000000000, 0.9659258262890683122, 1.000000000000000000, 0.9659258262890683122, 1.000000000000000000, 0.9659258262890683122, 1.000000000000000000, 0.9659258262890683122, 1.000000000000000000, 0.9659258262890683122, 1.000000000000000000, 0.9659258262890683122, 1.000000000000000000, 0.9659258262890683122, 1.000000000000000000, 0.9659258262890683122, 1.000000000000000000, 0.9659258262890683122, 1.000000000000000000, 0.9659258262890683122, 1.000000000000000000, 0.9659258262890683122, 1.000000000000000000, 0.9659258262890683122, 1.000000000000000000, 0.9659258262890683122, 1.000000000000000000, 0.9659258262890683122, 1.000000000000000000, 0.9659258262890683122, 1.000000000000000000, 0.9659258262890683122, 1.000000000000000000, 0.9659258262890683122, 1.000000000000000000, 0.9659258262890683122, 1.000000000000000000, 0.9659258262890683122, 1.000000000000000000, 0.9659258262890683122, 1.000000000000000000, 0.9659258262890683122, 1.000000000000000000, 0.9659258262890683122, 1.000000000000000000, 0.9659258262890683122, 1.000000000000000000, 0.9659258262890683122, 1.000000000000000000, 0.9659258262890683122, 1.000000000000000000, 0.9659258262890683122, 1.000000000000000000, 0.9659258262890683122, 1.000000000000000000, 0.9659258262890683122, 1.000000000000000000, 0.9659258262890683122, 1.000000000000000000, 0.9659258262890683122, 1.000000000000000000, 0.9659258262890683122, 1.000000000000000000, 0.9659258262890683122, 1.000000000000000000, 0.9659258262890683122, 1.000000000000000000, 0.9659258262890683122, 1.000000000000000000, 0.9659258262890683122, 1.000000000000000000, 0.9659258262890683122, 1.000000000000000000, 0.9659258262890683122, 1.000000000000000000, 0.9659258262890683122, 1.000000000000000000, 0.9659258262890683122, 1.000000000000000000, 0.9659258262890683122, 1.000000000000000000, 0.9659258262890683122, 1.000000000000000000, 0.9659258262890683122, 1.000000000000000000, 0.9659258262890683122, 1.000000000000000000, 0.9659258262890683122, 1.000000000000000000, 0.9659258262890683122, 1.000000000000000000, 0.9659258262890683122, 1.000000000000000000, 0.9659258262890683122, 1.000000000000000000, 0.9659258262890683122, 1.000000000000000000, 0.9659258262890683122, 1.000000000000000000, 0.9659258262890683122, 1.000000000000000000, 0.9659258262890683122, 1.000000000000000000, 0.9659258262890683122, 1.000000000000000000, 0.9659258262890683122, 1.000000000000000000, 0.9659258262890683122, 1.000000000000000000, 0.9659258262890683122, 1.000000000000000000, 0.9659258262890683122, 1.000000000000000000, 0.9659258262890683122, 1.000000000000000000, 0.9659258262890683122, 1.000000000000000000, 0.9659258262890683122, 1.000000000000000000, 0.9659258262890683122, 1.000000000000000000, 0.9659258262890683122, 1.000000000000000000, 0.9659258262890683122, 1.000000000000000000, 0.9659258262890683122, 1.000000000000000000, 0.9659258262890683122, 1.000000000000000000, 0.9659258262890683122, 1.000000000000000000, 0.9659258262890683122, 1.000000000000000000, 0.9659258262890683122, 1.000000000000000000, 0.9659258262890683122, 1.000000000000000000, 0.9659258262890683122, 1.000000000000000000, 0.9659258262890683122, 1.000000000000000000, 0.9659258262890683122, 1.000000000000000000, 0.9659258262890683122, 1.000000000000000000, 0.9659258262890683122, 1.000000000000000000, 0.9659258262890683122, 1.000000000000000000, 0.9659258262890683122, 1.000000000000000000, 0.9659258262890683122, 1.000000000000000000, 0.9659258262890683122, 1.000000000000000000, 0.9659258262890683122, 1.000000000000000000, 0.9659258262890683122, 1.000000000000000000, 0.9659258262890683122, 1.000000000000000000, 0.9659258262890683122, 1.000000000000000000, 0.9659258262890683122, 1.000000000000000000, 0.9659258262890683122, 1.000000000000000000, 0.9659258262890683122, 1.000000000000000000, 0.9659258262890683122, 1.000000000000000000, 0.9659258262890683122, 1.000000000000000000, 0.9659258262890683122, 1.000000000000000000, 0.9659258262890683122, 1.000000000000000000, 0.9659258262890683122, 1.000000000000000000, 0.9659258262890683122, 1.000000000000000000, 0.9659258262890683122, 1.000000000000000000, 0.9659258262890683122, 1.000000000000000000, 0.9659258262890683122, 1.000000000000000000, 0.9659258262890683122, 1.000000000000000000),
 ( 1.000000000000000000, 0.9659258262890683122, 1.000000000000000000, 0.9659258262890683122, 1.000000000000000000, 0.9659258262890683122, 1.000000000000000000, 0.9659258262890683122, 1.000000000000000000, 0.9659258262890683122, 1.000000000000000000, 0.9659258262890683122, 1.000000000000000000, 0.9659258262890683122, 1.000000000000000000, 0.9659258262890683122, 1.000000000000000000, 0.9659258262890683122, 1.000000000000000000, 0.9659258262890683122, 1.000000000000000000, 0.9659258262890683122, 1.000000000000000000, 0.9659258262890683122, 1.000000000000000000, 0.9659258262890683122, 1.000000000000000000, 0.9659258262890683122, 1.000000000000000000, 0.9659258262890683122, 1.000000000000000000, 0.9659258262890683122, 1.000000000000000000, 0.9659258262890683122, 1.000000000000000000, 0.9659258262890683122, 1.000000000000000000, 0.9659258262890683122, 1.000000000000000000, 0.9659258262890683122, 1.000000000000000000, 0.9659258262890683122, 1.000000000000000000, 0.9659258262890683122, 1.000000000000000000, 0.9659258262890683122, 1.000000000000000000, 0.9659258262890683122, 1.000000000000000000, 0.9659258262890683122, 1.000000000000000000, 0.9659258262890683122, 1.000000000000000000, 0.9659258262890683122, 1.000000000000000000, 0.9659258262890683122, 1.000000000000000000, 0.9659258262890683122, 1.000000000000000000, 0.9659258262890683122, 1.000000000000000000, 0.9659258262890683122, 1.000000000000000000, 0.9659258262890683122, 1.000000000000000000, 0.9659258262890683122, 1.000000000000000000, 0.9659258262890683122, 1.000000000000000000, 0.9659258262890683122, 1.000000000000000000, 0.9659258262890683122, 1.000000000000000000, 0.9659258262890683122, 1.000000000000000000, 0.9659258262890683122, 1.000000000000000000, 0.9659258262890683122, 1.000000000000000000, 0.9659258262890683122, 1.000000000000000000, 0.9659258262890683122, 1.000000000000000000, 0.9659258262890683122, 1.000000000000000000, 0.9659258262890683122, 1.000000000000000000, 0.9659258262890683122, 1.000000000000000000, 0.9659258262890683122, 1.000000000000000000, 0.9659258262890683122, 1.000000000000000000, 0.9659258262890683122, 1.000000000000000000, 0.9659258262890683122, 1.000000000000000000, 0.9659258262890683122, 1.000000000000000000, 0.9659258262890683122, 1.000000000000000000, 0.9659258262890683122, 1.000000000000000000, 0.9659258262890683122, 1.000000000000000000, 0.9659258262890683122, 1.000000000000000000, 0.9659258262890683122, 1.000000000000000000, 0.9659258262890683122, 1.000000000000000000, 0.9659258262890683122, 1.000000000000000000, 0.9659258262890683122, 1.000000000000000000, 0.9659258262890683122, 1.000000000000000000, 0.9659258262890683122, 1.000000000000000000, 0.9659258262890683122, 1.000000000000000000, 0.9659258262890683122, 1.000000000000000000, 0.9659258262890683122, 1.000000000000000000, 0.9659258262890683122, 1.000000000000000000, 0.9659258262890683122, 1.000000000000000000, 0.9659258262890683122, 1.000000000000000000, 0.9659258262890683122, 1.000000000000000000, 0.9659258262890683122, 1.000000000000000000, 0.9659258262890683122, 1.000000000000000000, 0.9659258262890683122, 1.000000000000000000, 0.9659258262890683122, 1.000000000000000000, 0.9659258262890683122, 1.000000000000000000, 0.9659258262890683122, 1.000000000000000000, 0.9659258262890683122, 1.000000000000000000, 0.9659258262890683122, 1.000000000000000000, 0.9659258262890683122, 1.000000000000000000, 0.9659258262890683122, 1.000000000000000000, 0.9659258262890683122, 1.000000000000000000, 0.9659258262890683122, 1.000000000000000000, 0.9659258262890683122, 1.000000000000000000, 0.9659258262890683122, 1.000000000000000000, 0.9659258262890683122, 1.000000000000000000, 0.9659258262890683122, 1.000000000000000000, 0.9659258262890683122, 1.000000000000000000, 0.9659258262890683122, 1.000000000000000000, 0.9659258262890683122, 1.000000000000000000, 0.9659258262890683122, 1.000000000000000000, 0.9659258262890683122, 1.000000000000000000, 0.9659258262890683122, 1.000000000000000000, 0.9659258262890683122, 1.000000000000000000, 0.9659258262890683122, 1.000000000000000000, 0.9659258262890683122, 1.000000000000000000, 0.9659258262890683122, 1.000000000000000000, 0.9659258262890683122, 1.000000000000000000, 0.9659258262890683122, 1.000000000000000000, 0.9659258262890683122, 1.000000000000000000, 0.9659258262890683122, 1.000000000000000000, 0.9659258262890683122, 1.000000000000000000, 0.9659258262890683122, 1.000000000000000000, 0.9659258262890683122, 1.000000000000000000, 0.9659258262890683122, 1.000000000000000000, 0.9659258262890683122, 1.000000000000000000, 0.9659258262890683122, 1.000000000000000000, 0.9659258262890683122, 1.000000000000000000, 0.9659258262890683122, 1.000000000000000000, 0.9659258262890683122, 1.000000000000000000, 0.9659258262890683122, 1.000000000000000000, 0.9659258262890683122, 1.000000000000000000, 0.9659258262890683122, 1.000000000000000000, 0.9659258262890683122, 1.000000000000000000, 0.9659258262890683122, 1.000000000000000000, 0.9659258262890683122, 1.000000000000000000, 0.9659258262890683122, 1.000000000000000000, 0.9659258262890683122, 1.000000000000000000, 0.9659258262890683122, 1.000000000000000000, 0.9659258262890683122, 1.000000000000000000, 0.9659258262890683122, 1.000000000000000000, 0.9659258262890683122, 1.000000000000000000, 0.9659258262890683122, 1.000000000000000000, 0.9659258262890683122, 1.000000000000000000, 0.9659258262890683122, 1.000000000000000000, 0.9659258262890683122, 1.000000000000000000, 0.9659258262890683122, 1.000000000000000000, 0.9659258262890683122, 1.000000000000000000, 0.9659258262890683122, 1.000000000000000000, 0.9659258262890683122, 1.000000000000000000, 0.9659258262890683122, 1.000000000000000000, 0.9659258262890683122, 1.000000000000000000, 0.9659258262890683122, 1.000000000000000000, 0.9659258262890683122, 1.000000000000000000, 0.9659258262890683122, 1.000000000000000000, 0.9659258262890683122, 1.000000000000000000, 0.9659258262890683122, 1.000000000000000000, 0.9659258262890683122, 1.000000000000000000, 0.9659258262890683122, 1.000000000000000000, 0.9659258262890683122, 1.000000000000000000, 0.9659258262890683122, 1.000000000000000000, 0.9659258262890683122, 1.000000000000000000, 0.9659258262890683122, 1.000000000000000000, 0.9659258262890683122, 1.000000000000000000, 0.9659258262890683122, 1.000000000000000000, 0.9659258262890683122, 1.000000000000000000, 0.9659258262890683122, 1.000000000000000000, 0.9659258262890683122, 1.000000000000000000, 0.9659258262890683122, 1.000000000000000000, 0.9659258262890683122, 1.000000000000000000, 0.9659258262890683122, 1.000000000000000000, 0.9659258262890683122, 1.000000000000000000, 0.9659258262890683122, 1.000000000000000000, 0.9659258262890683122, 1.000000000000000000, 0.9659258262890683122, 1.000000000000000000, 0.9659258262890683122, 1.000000000000000000, 0.9659258262890683122, 1.000000000000000000, 0.9659258262890683122, 1.000000000000000000, 0.9659258262890683122, 1.000000000000000000, 0.9659258262890683122, 1.000000000000000000, 0.9659258262890683122, 1.000000000000000000, 0.9659258262890683122, 1.000000000000000000, 0.9659258262890683122, 1.000000000000000000, 0.9659258262890683122, 1.000000000000000000, 0.9659258262890683122, 1.000000000000000000, 0.9659258262890683122, 1.000000000000000000, 0.9659258262890683122, 1.000000000000000000) ) ) 
 REPRESENTATION_ITEM ( '' )  SURFACE ( )  );
#40020 = CARTESIAN_POINT ( 'NONE',  ( 22.81628187352647785, 41.62363466993042493, 6.195893100308588602E-16 ) ) ;
#40021 = ORIENTED_EDGE ( 'NONE', *, *, #38922, .F. ) ;
#40022 =( BOUNDED_SURFACE ( )  B_SPLINE_SURFACE ( 1, 2, ( 
 ( #23551, #17022, #98577, #9010, #46041, #77017, #8531, #69526, #31504, #40512, #11470, #64455, #26464, #49459, #9507, #18486, #56000, #47987, #2035, #64942, #94963, #18002, #55508, #62994, #41002, #47499, #71009, #2531, #56964, #25992, #79965, #32985, #40009, #41988, #87466, #10491, #56487, #34450, #17520, #87953, #86504, #70511, #78002, #48482, #78497, #18981, #32496, #25023, #41503, #10982, #95469, #86008, #93498, #63488, #3983, #10011, #33464, #71502, #71971, #3015, #93991, #94474, #26960, #3494, #78984, #63961, #86975, #57460, #72452, #25514, #48974, #79482, #33952, #42467, #59424, #13438, #58433, #59917, #5467, #58940, #36442, #80954, #27941, #50946, #73439, #89927, #44423, #88452, #34945, #81440, #11963, #49960, #73939, #88948, #51441, #35939, #19953, #43925, #97956, #66435, #12942, #50447, #43438, #29412, #80464, #12452, #42958, #4965, #95968, #51940, #20953, #27452, #96970, #67435, #66935, #19469, #97456, #28442, #20455, #72950, #4478, #65444, #74928, #57945, #89440, #81930, #74423, #5951, #28921, #35446, #65942, #21442, #82424, #6427, #36939, #96469, #13949, #91407, #6934, #76892, #22934, #53402, #98947, #23914, #14940, #30402, #37441, #61392, #39406, #84896, #52425, #91902, #60905, #82924, #45919, #8890, #77377, #90909, #52908, #23427, #83911, #54382, #38420, #22437, #53906, #84414, #46402, #1419, #76407, #29908, #922, #7923, #83421, #69400, #16407, #67932, #15912, #14442, #45409, #60414, #8406, #38913, #31384, #61884, #98452, #75914, #44912, #68424, #75419, #7438, #92389, #15439, #37935, #68919, #46886, #447, #69899, #31872, #30898, #90405, #21947, #24409, #18863, #70393, #54875, #62371, #26348, #92875, #39890, #33347, #71385, #79360, #1912, #24900, #55384, #17878, #64336, #49344, #47866, #32865, #86376, #78867, #79845, #85386, #3367, #11348, #3864, #70889, #48361, #33829, #85884, #56849, #10867, #41389, #94847, #16899, #63842, #2407, #62875, #47376, #41868, #71856, #63364, #32370, #77874, #55878, #9385, #17397, #78371, #87348, #40879, #72331, #9890, #93372, #40393, #93866, #25393, #2898, #10377, #94355, #25873, #56373, #86864, #18370, #48851, #65319, #74299, #87830, #11840, #28321, #96846, #51812, #72824, #19348, #19832, #89802, #49830, #20335, #27821, #58812, #96350, #42347, #81324, #82299, #89321, #65816, #58307, #88823, #5345, #51318, #74805, #13319, #64823, #43317, #21322, #50831, #59305, #12819, #50319, #73811, #81801, #4362, #35823, #4846, #80834, #66309, #26839, #20829, #12334, #13821, #57826, #42838, #34828, #43805, #35321, #95844, #5825, #36319, #66812, #97334, #44302, #34326, #28807, #95340, #57333 ),
 ( #27329, #88334, #80342, #73322, #70641, #54628, #8171, #39659, #1669, #62617, #17648, #62127, #46167, #17156, #92636, #38663, #85638, #2167, #84175, #70151, #197, #690, #76651, #32122, #77626, #9142, #47637, #23181, #61634, #61155, #84652, #30647, #69166, #78132, #16160, #31144, #92154, #93126, #25158, #9641, #32624, #39162, #40140, #23679, #91664, #63122, #24652, #46642, #48118, #24160, #47128, #55122, #54143, #77141, #69652, #8650, #93625, #55634, #1177, #53658, #31635, #15682, #36818, #85147, #16654, #86135, #6311, #67310, #72581, #58072, #64581, #72097, #48610, #41631, #88576, #40636, #79113, #10627, #3134, #56132, #12092, #80094, #86624, #95090, #27579, #27083, #20085, #57585, #26598, #79611, #10141, #71134, #2662, #4610, #18137, #57095, #19101, #11597, #49582, #4113, #25640, #63607, #87591, #34578, #65571, #35071, #78631, #33112, #11112, #94113, #65072, #3622, #34090, #87104, #42595, #33595, #42117, #41138, #95597, #26123, #71625, #64093, #94606, #56615, #88082, #19592, #18619, #50090, #80595, #73074, #96098, #49109, #7071, #14080, #20587, #6564, #44560, #35579, #44058, #52072, #12582, #37573, #58573, #43081, #50587, #14579, #81079, #28075, #21582, #59563, #67573, #89074, #13073, #43566, #6079, #52554, #68065, #36073, #21080, #74565, #67067, #98593, #73566, #90549, #30042, #91042, #59064, #36580, #22079, #74062, #45047, #98085, #29543, #83058, #5091, #82566, #89569, #51074, #66069, #60551, #60049, #51576, #81566, #96597, #97595, #5594, #66575, #97102, #75557, #29057, #28573, #82065, #13573, #90058, #75058, #37076, #1055, #9520, #91548, #63007, #31027, #15079, #22570, #92035, #53536, #62506, #76048, #89, #16543, #85029, #40020, #61036, #7578, #8054, #78015, #38066, #8544, #16041, #47017, #84542, #30536, #69539, #70524, #77509, #54032, #46529, #77032, #92519, #39542, #53041, #1555, #83557, #31522, #2047, #39044, #47515, #62018, #38553, #24044, #70031, #23067, #54515, #23564, #69048, #32509, #17036, #45550, #9026, #61526, #68557, #32002, #84050, #15570, #46051, #76538, #93011, #24546, #85523, #55006, #582, #26479, #87480, #49471, #4492, #48988, #33001, #3999, #79496, #25525, #72466, #87965, #71021, #56975, #86018, #86515, #63502, #18994, #64469, #94976, #34463, #10023, #48495, #47999, #71518, #17532, #94002, #64955, #3028, #56015, #78997, #79978, #11976, #95482, #19479, #26005, #26973, #18013, #78508, #57471, #11481, #33477, #34957, #10995, #33965, #42001, #10502, #63973, #56499, #41016, #49971, #80477, #94486, #40523, #86990, #2544, #25036, #41515, #18497, #42478, #71982, #3506, #72961, #93510, #55521, #58951 ) ),
 .UNSPECIFIED., .F., .F., .F. ) 
 B_SPLINE_SURFACE_WITH_KNOTS ( ( 2, 2 ),
 ( 3, 2, 2, 2, 2, 2, 2, 2, 2, 2, 2, 2, 2, 2, 2, 2, 2, 2, 2, 2, 2, 2, 2, 2, 2, 2, 2, 2, 2, 2, 2, 2, 2, 2, 2, 2, 2, 2, 2, 2, 2, 2, 2, 2, 2, 2, 2, 2, 2, 2, 2, 2, 2, 2, 2, 2, 2, 2, 2, 2, 2, 2, 2, 2, 2, 2, 2, 2, 2, 2, 2, 2, 2, 2, 2, 2, 2, 2, 2, 2, 2, 2, 2, 2, 2, 2, 2, 2, 2, 2, 2, 2, 2, 2, 2, 2, 2, 2, 2, 2, 2, 2, 2, 2, 2, 2, 2, 2, 2, 2, 2, 2, 2, 2, 2, 2, 2, 2, 2, 2, 2, 2, 2, 2, 2, 2, 2, 2, 2, 2, 2, 2, 2, 2, 2, 2, 2, 2, 2, 2, 2, 2, 2, 2, 2, 2, 2, 2, 2, 2, 2, 2, 2, 2, 2, 2, 2, 2, 2, 2, 2, 2, 3 ),
 ( 0.000000000000000000, 1.000000000000000000 ),
 ( 0.000000000000000000, 0.005952380952380952051, 0.01190476190476190410, 0.01785714285714285615, 0.02380952380952380820, 0.02976190476190476025, 0.03571428571428571230, 0.04166666666666666435, 0.04761904761904761640, 0.05357142857142856845, 0.05952380952380952051, 0.06547619047619047949, 0.07142857142857142461, 0.07738095238095238360, 0.08333333333333332871, 0.08928571428571428770, 0.09523809523809523281, 0.1011904761904761918, 0.1071428571428571369, 0.1130952380952380959, 0.1190476190476190410, 0.1250000000000000000, 0.1309523809523809590, 0.1369047619047619180, 0.1428571428571428492, 0.1488095238095238082, 0.1547619047619047672, 0.1607142857142857262, 0.1666666666666666574, 0.1726190476190476164, 0.1785714285714285754, 0.1845238095238095344, 0.1904761904761904656, 0.1964285714285714246, 0.2023809523809523836, 0.2083333333333333426, 0.2142857142857142738, 0.2202380952380952328, 0.2261904761904761918, 0.2321428571428571508, 0.2380952380952380820, 0.2440476190476190410, 0.2500000000000000000, 0.2559523809523809312, 0.2619047619047619180, 0.2678571428571428492, 0.2738095238095238360, 0.2797619047619047672, 0.2857142857142856984, 0.2916666666666666852, 0.2976190476190476164, 0.3035714285714285476, 0.3095238095238095344, 0.3154761904761904656, 0.3214285714285714524, 0.3273809523809523836, 0.3333333333333333148, 0.3392857142857143016, 0.3452380952380952328, 0.3511904761904761640, 0.3571428571428571508, 0.3630952380952380820, 0.3690476190476190688, 0.3750000000000000000, 0.3809523809523809312, 0.3869047619047619180, 0.3928571428571428492, 0.3988095238095238360, 0.4047619047619047672, 0.4107142857142856984, 0.4166666666666666852, 0.4226190476190476164, 0.4285714285714285476, 0.4345238095238095344, 0.4404761904761904656, 0.4464285714285714524, 0.4523809523809523836, 0.4583333333333333148, 0.4642857142857143016, 0.4702380952380952328, 0.4761904761904761640, 0.4821428571428571508, 0.4880952380952380820, 0.4940476190476190688, 0.5000000000000000000, 0.5059523809523809312, 0.5119047619047618625, 0.5178571428571429047, 0.5238095238095238360, 0.5297619047619047672, 0.5357142857142856984, 0.5416666666666666297, 0.5476190476190476719, 0.5535714285714286031, 0.5595238095238095344, 0.5654761904761904656, 0.5714285714285713969, 0.5773809523809523281, 0.5833333333333333703, 0.5892857142857143016, 0.5952380952380952328, 0.6011904761904761640, 0.6071428571428570953, 0.6130952380952381375, 0.6190476190476190688, 0.6250000000000000000, 0.6309523809523809312, 0.6369047619047618625, 0.6428571428571429047, 0.6488095238095238360, 0.6547619047619047672, 0.6607142857142856984, 0.6666666666666666297, 0.6726190476190476719, 0.6785714285714286031, 0.6845238095238095344, 0.6904761904761904656, 0.6964285714285713969, 0.7023809523809523281, 0.7083333333333333703, 0.7142857142857143016, 0.7202380952380952328, 0.7261904761904761640, 0.7321428571428570953, 0.7380952380952381375, 0.7440476190476190688, 0.7500000000000000000, 0.7559523809523809312, 0.7619047619047618625, 0.7678571428571429047, 0.7738095238095238360, 0.7797619047619047672, 0.7857142857142856984, 0.7916666666666666297, 0.7976190476190476719, 0.8035714285714286031, 0.8095238095238095344, 0.8154761904761904656, 0.8214285714285713969, 0.8273809523809523281, 0.8333333333333333703, 0.8392857142857143016, 0.8452380952380952328, 0.8511904761904761640, 0.8571428571428570953, 0.8630952380952381375, 0.8690476190476190688, 0.8750000000000000000, 0.8809523809523809312, 0.8869047619047618625, 0.8928571428571429047, 0.8988095238095238360, 0.9047619047619047672, 0.9107142857142856984, 0.9166666666666666297, 0.9226190476190476719, 0.9285714285714286031, 0.9345238095238095344, 0.9404761904761904656, 0.9464285714285713969, 0.9523809523809523281, 0.9583333333333333703, 0.9642857142857143016 ),
 .UNSPECIFIED. ) 
 GEOMETRIC_REPRESENTATION_ITEM ( )  RATIONAL_B_SPLINE_SURFACE ( (
 ( 1.000000000000000000, 0.9659258262890683122, 1.000000000000000000, 0.9659258262890683122, 1.000000000000000000, 0.9659258262890683122, 1.000000000000000000, 0.9659258262890683122, 1.000000000000000000, 0.9659258262890683122, 1.000000000000000000, 0.9659258262890683122, 1.000000000000000000, 0.9659258262890683122, 1.000000000000000000, 0.9659258262890683122, 1.000000000000000000, 0.9659258262890683122, 1.000000000000000000, 0.9659258262890683122, 1.000000000000000000, 0.9659258262890683122, 1.000000000000000000, 0.9659258262890683122, 1.000000000000000000, 0.9659258262890683122, 1.000000000000000000, 0.9659258262890683122, 1.000000000000000000, 0.9659258262890683122, 1.000000000000000000, 0.9659258262890683122, 1.000000000000000000, 0.9659258262890683122, 1.000000000000000000, 0.9659258262890683122, 1.000000000000000000, 0.9659258262890683122, 1.000000000000000000, 0.9659258262890683122, 1.000000000000000000, 0.9659258262890683122, 1.000000000000000000, 0.9659258262890683122, 1.000000000000000000, 0.9659258262890683122, 1.000000000000000000, 0.9659258262890683122, 1.000000000000000000, 0.9659258262890683122, 1.000000000000000000, 0.9659258262890683122, 1.000000000000000000, 0.9659258262890683122, 1.000000000000000000, 0.9659258262890683122, 1.000000000000000000, 0.9659258262890683122, 1.000000000000000000, 0.9659258262890683122, 1.000000000000000000, 0.9659258262890683122, 1.000000000000000000, 0.9659258262890683122, 1.000000000000000000, 0.9659258262890683122, 1.000000000000000000, 0.9659258262890683122, 1.000000000000000000, 0.9659258262890683122, 1.000000000000000000, 0.9659258262890683122, 1.000000000000000000, 0.9659258262890683122, 1.000000000000000000, 0.9659258262890683122, 1.000000000000000000, 0.9659258262890683122, 1.000000000000000000, 0.9659258262890683122, 1.000000000000000000, 0.9659258262890683122, 1.000000000000000000, 0.9659258262890683122, 1.000000000000000000, 0.9659258262890683122, 1.000000000000000000, 0.9659258262890683122, 1.000000000000000000, 0.9659258262890683122, 1.000000000000000000, 0.9659258262890683122, 1.000000000000000000, 0.9659258262890683122, 1.000000000000000000, 0.9659258262890683122, 1.000000000000000000, 0.9659258262890683122, 1.000000000000000000, 0.9659258262890683122, 1.000000000000000000, 0.9659258262890683122, 1.000000000000000000, 0.9659258262890683122, 1.000000000000000000, 0.9659258262890683122, 1.000000000000000000, 0.9659258262890683122, 1.000000000000000000, 0.9659258262890683122, 1.000000000000000000, 0.9659258262890683122, 1.000000000000000000, 0.9659258262890683122, 1.000000000000000000, 0.9659258262890683122, 1.000000000000000000, 0.9659258262890683122, 1.000000000000000000, 0.9659258262890683122, 1.000000000000000000, 0.9659258262890683122, 1.000000000000000000, 0.9659258262890683122, 1.000000000000000000, 0.9659258262890683122, 1.000000000000000000, 0.9659258262890683122, 1.000000000000000000, 0.9659258262890683122, 1.000000000000000000, 0.9659258262890683122, 1.000000000000000000, 0.9659258262890683122, 1.000000000000000000, 0.9659258262890683122, 1.000000000000000000, 0.9659258262890683122, 1.000000000000000000, 0.9659258262890683122, 1.000000000000000000, 0.9659258262890683122, 1.000000000000000000, 0.9659258262890683122, 1.000000000000000000, 0.9659258262890683122, 1.000000000000000000, 0.9659258262890683122, 1.000000000000000000, 0.9659258262890683122, 1.000000000000000000, 0.9659258262890683122, 1.000000000000000000, 0.9659258262890683122, 1.000000000000000000, 0.9659258262890683122, 1.000000000000000000, 0.9659258262890683122, 1.000000000000000000, 0.9659258262890683122, 1.000000000000000000, 0.9659258262890683122, 1.000000000000000000, 0.9659258262890683122, 1.000000000000000000, 0.9659258262890683122, 1.000000000000000000, 0.9659258262890683122, 1.000000000000000000, 0.9659258262890683122, 1.000000000000000000, 0.9659258262890683122, 1.000000000000000000, 0.9659258262890683122, 1.000000000000000000, 0.9659258262890683122, 1.000000000000000000, 0.9659258262890683122, 1.000000000000000000, 0.9659258262890683122, 1.000000000000000000, 0.9659258262890683122, 1.000000000000000000, 0.9659258262890683122, 1.000000000000000000, 0.9659258262890683122, 1.000000000000000000, 0.9659258262890683122, 1.000000000000000000, 0.9659258262890683122, 1.000000000000000000, 0.9659258262890683122, 1.000000000000000000, 0.9659258262890683122, 1.000000000000000000, 0.9659258262890683122, 1.000000000000000000, 0.9659258262890683122, 1.000000000000000000, 0.9659258262890683122, 1.000000000000000000, 0.9659258262890683122, 1.000000000000000000, 0.9659258262890683122, 1.000000000000000000, 0.9659258262890683122, 1.000000000000000000, 0.9659258262890683122, 1.000000000000000000, 0.9659258262890683122, 1.000000000000000000, 0.9659258262890683122, 1.000000000000000000, 0.9659258262890683122, 1.000000000000000000, 0.9659258262890683122, 1.000000000000000000, 0.9659258262890683122, 1.000000000000000000, 0.9659258262890683122, 1.000000000000000000, 0.9659258262890683122, 1.000000000000000000, 0.9659258262890683122, 1.000000000000000000, 0.9659258262890683122, 1.000000000000000000, 0.9659258262890683122, 1.000000000000000000, 0.9659258262890683122, 1.000000000000000000, 0.9659258262890683122, 1.000000000000000000, 0.9659258262890683122, 1.000000000000000000, 0.9659258262890683122, 1.000000000000000000, 0.9659258262890683122, 1.000000000000000000, 0.9659258262890683122, 1.000000000000000000, 0.9659258262890683122, 1.000000000000000000, 0.9659258262890683122, 1.000000000000000000, 0.9659258262890683122, 1.000000000000000000, 0.9659258262890683122, 1.000000000000000000, 0.9659258262890683122, 1.000000000000000000, 0.9659258262890683122, 1.000000000000000000, 0.9659258262890683122, 1.000000000000000000, 0.9659258262890683122, 1.000000000000000000, 0.9659258262890683122, 1.000000000000000000, 0.9659258262890683122, 1.000000000000000000, 0.9659258262890683122, 1.000000000000000000, 0.9659258262890683122, 1.000000000000000000, 0.9659258262890683122, 1.000000000000000000, 0.9659258262890683122, 1.000000000000000000, 0.9659258262890683122, 1.000000000000000000, 0.9659258262890683122, 1.000000000000000000, 0.9659258262890683122, 1.000000000000000000, 0.9659258262890683122, 1.000000000000000000, 0.9659258262890683122, 1.000000000000000000, 0.9659258262890683122, 1.000000000000000000, 0.9659258262890683122, 1.000000000000000000, 0.9659258262890683122, 1.000000000000000000, 0.9659258262890683122, 1.000000000000000000, 0.9659258262890683122, 1.000000000000000000, 0.9659258262890683122, 1.000000000000000000, 0.9659258262890683122, 1.000000000000000000, 0.9659258262890683122, 1.000000000000000000, 0.9659258262890683122, 1.000000000000000000, 0.9659258262890683122, 1.000000000000000000, 0.9659258262890683122, 1.000000000000000000, 0.9659258262890683122, 1.000000000000000000, 0.9659258262890683122, 1.000000000000000000, 0.9659258262890683122, 1.000000000000000000, 0.9659258262890683122, 1.000000000000000000, 0.9659258262890683122, 1.000000000000000000, 0.9659258262890683122, 1.000000000000000000, 0.9659258262890683122, 1.000000000000000000, 0.9659258262890683122, 1.000000000000000000, 0.9659258262890683122, 1.000000000000000000, 0.9659258262890683122, 1.000000000000000000, 0.9659258262890683122, 1.000000000000000000, 0.9659258262890683122, 1.000000000000000000),
 ( 1.000000000000000000, 0.9659258262890683122, 1.000000000000000000, 0.9659258262890683122, 1.000000000000000000, 0.9659258262890683122, 1.000000000000000000, 0.9659258262890683122, 1.000000000000000000, 0.9659258262890683122, 1.000000000000000000, 0.9659258262890683122, 1.000000000000000000, 0.9659258262890683122, 1.000000000000000000, 0.9659258262890683122, 1.000000000000000000, 0.9659258262890683122, 1.000000000000000000, 0.9659258262890683122, 1.000000000000000000, 0.9659258262890683122, 1.000000000000000000, 0.9659258262890683122, 1.000000000000000000, 0.9659258262890683122, 1.000000000000000000, 0.9659258262890683122, 1.000000000000000000, 0.9659258262890683122, 1.000000000000000000, 0.9659258262890683122, 1.000000000000000000, 0.9659258262890683122, 1.000000000000000000, 0.9659258262890683122, 1.000000000000000000, 0.9659258262890683122, 1.000000000000000000, 0.9659258262890683122, 1.000000000000000000, 0.9659258262890683122, 1.000000000000000000, 0.9659258262890683122, 1.000000000000000000, 0.9659258262890683122, 1.000000000000000000, 0.9659258262890683122, 1.000000000000000000, 0.9659258262890683122, 1.000000000000000000, 0.9659258262890683122, 1.000000000000000000, 0.9659258262890683122, 1.000000000000000000, 0.9659258262890683122, 1.000000000000000000, 0.9659258262890683122, 1.000000000000000000, 0.9659258262890683122, 1.000000000000000000, 0.9659258262890683122, 1.000000000000000000, 0.9659258262890683122, 1.000000000000000000, 0.9659258262890683122, 1.000000000000000000, 0.9659258262890683122, 1.000000000000000000, 0.9659258262890683122, 1.000000000000000000, 0.9659258262890683122, 1.000000000000000000, 0.9659258262890683122, 1.000000000000000000, 0.9659258262890683122, 1.000000000000000000, 0.9659258262890683122, 1.000000000000000000, 0.9659258262890683122, 1.000000000000000000, 0.9659258262890683122, 1.000000000000000000, 0.9659258262890683122, 1.000000000000000000, 0.9659258262890683122, 1.000000000000000000, 0.9659258262890683122, 1.000000000000000000, 0.9659258262890683122, 1.000000000000000000, 0.9659258262890683122, 1.000000000000000000, 0.9659258262890683122, 1.000000000000000000, 0.9659258262890683122, 1.000000000000000000, 0.9659258262890683122, 1.000000000000000000, 0.9659258262890683122, 1.000000000000000000, 0.9659258262890683122, 1.000000000000000000, 0.9659258262890683122, 1.000000000000000000, 0.9659258262890683122, 1.000000000000000000, 0.9659258262890683122, 1.000000000000000000, 0.9659258262890683122, 1.000000000000000000, 0.9659258262890683122, 1.000000000000000000, 0.9659258262890683122, 1.000000000000000000, 0.9659258262890683122, 1.000000000000000000, 0.9659258262890683122, 1.000000000000000000, 0.9659258262890683122, 1.000000000000000000, 0.9659258262890683122, 1.000000000000000000, 0.9659258262890683122, 1.000000000000000000, 0.9659258262890683122, 1.000000000000000000, 0.9659258262890683122, 1.000000000000000000, 0.9659258262890683122, 1.000000000000000000, 0.9659258262890683122, 1.000000000000000000, 0.9659258262890683122, 1.000000000000000000, 0.9659258262890683122, 1.000000000000000000, 0.9659258262890683122, 1.000000000000000000, 0.9659258262890683122, 1.000000000000000000, 0.9659258262890683122, 1.000000000000000000, 0.9659258262890683122, 1.000000000000000000, 0.9659258262890683122, 1.000000000000000000, 0.9659258262890683122, 1.000000000000000000, 0.9659258262890683122, 1.000000000000000000, 0.9659258262890683122, 1.000000000000000000, 0.9659258262890683122, 1.000000000000000000, 0.9659258262890683122, 1.000000000000000000, 0.9659258262890683122, 1.000000000000000000, 0.9659258262890683122, 1.000000000000000000, 0.9659258262890683122, 1.000000000000000000, 0.9659258262890683122, 1.000000000000000000, 0.9659258262890683122, 1.000000000000000000, 0.9659258262890683122, 1.000000000000000000, 0.9659258262890683122, 1.000000000000000000, 0.9659258262890683122, 1.000000000000000000, 0.9659258262890683122, 1.000000000000000000, 0.9659258262890683122, 1.000000000000000000, 0.9659258262890683122, 1.000000000000000000, 0.9659258262890683122, 1.000000000000000000, 0.9659258262890683122, 1.000000000000000000, 0.9659258262890683122, 1.000000000000000000, 0.9659258262890683122, 1.000000000000000000, 0.9659258262890683122, 1.000000000000000000, 0.9659258262890683122, 1.000000000000000000, 0.9659258262890683122, 1.000000000000000000, 0.9659258262890683122, 1.000000000000000000, 0.9659258262890683122, 1.000000000000000000, 0.9659258262890683122, 1.000000000000000000, 0.9659258262890683122, 1.000000000000000000, 0.9659258262890683122, 1.000000000000000000, 0.9659258262890683122, 1.000000000000000000, 0.9659258262890683122, 1.000000000000000000, 0.9659258262890683122, 1.000000000000000000, 0.9659258262890683122, 1.000000000000000000, 0.9659258262890683122, 1.000000000000000000, 0.9659258262890683122, 1.000000000000000000, 0.9659258262890683122, 1.000000000000000000, 0.9659258262890683122, 1.000000000000000000, 0.9659258262890683122, 1.000000000000000000, 0.9659258262890683122, 1.000000000000000000, 0.9659258262890683122, 1.000000000000000000, 0.9659258262890683122, 1.000000000000000000, 0.9659258262890683122, 1.000000000000000000, 0.9659258262890683122, 1.000000000000000000, 0.9659258262890683122, 1.000000000000000000, 0.9659258262890683122, 1.000000000000000000, 0.9659258262890683122, 1.000000000000000000, 0.9659258262890683122, 1.000000000000000000, 0.9659258262890683122, 1.000000000000000000, 0.9659258262890683122, 1.000000000000000000, 0.9659258262890683122, 1.000000000000000000, 0.9659258262890683122, 1.000000000000000000, 0.9659258262890683122, 1.000000000000000000, 0.9659258262890683122, 1.000000000000000000, 0.9659258262890683122, 1.000000000000000000, 0.9659258262890683122, 1.000000000000000000, 0.9659258262890683122, 1.000000000000000000, 0.9659258262890683122, 1.000000000000000000, 0.9659258262890683122, 1.000000000000000000, 0.9659258262890683122, 1.000000000000000000, 0.9659258262890683122, 1.000000000000000000, 0.9659258262890683122, 1.000000000000000000, 0.9659258262890683122, 1.000000000000000000, 0.9659258262890683122, 1.000000000000000000, 0.9659258262890683122, 1.000000000000000000, 0.9659258262890683122, 1.000000000000000000, 0.9659258262890683122, 1.000000000000000000, 0.9659258262890683122, 1.000000000000000000, 0.9659258262890683122, 1.000000000000000000, 0.9659258262890683122, 1.000000000000000000, 0.9659258262890683122, 1.000000000000000000, 0.9659258262890683122, 1.000000000000000000, 0.9659258262890683122, 1.000000000000000000, 0.9659258262890683122, 1.000000000000000000, 0.9659258262890683122, 1.000000000000000000, 0.9659258262890683122, 1.000000000000000000, 0.9659258262890683122, 1.000000000000000000, 0.9659258262890683122, 1.000000000000000000, 0.9659258262890683122, 1.000000000000000000, 0.9659258262890683122, 1.000000000000000000, 0.9659258262890683122, 1.000000000000000000, 0.9659258262890683122, 1.000000000000000000, 0.9659258262890683122, 1.000000000000000000, 0.9659258262890683122, 1.000000000000000000, 0.9659258262890683122, 1.000000000000000000, 0.9659258262890683122, 1.000000000000000000, 0.9659258262890683122, 1.000000000000000000, 0.9659258262890683122, 1.000000000000000000, 0.9659258262890683122, 1.000000000000000000, 0.9659258262890683122, 1.000000000000000000, 0.9659258262890683122, 1.000000000000000000) ) ) 
 REPRESENTATION_ITEM ( '' )  SURFACE ( )  );
#40023 = CARTESIAN_POINT ( 'NONE',  ( 10.00000000000000000, 54.75893115100078745, -9.846743663894594434 ) ) ;
#40024 = CARTESIAN_POINT ( 'NONE',  ( 17.96484262340118221, 14.93868534415484106, 7.964842623401181321 ) ) ;
#40025 = VECTOR ( 'NONE', #18442, 1000.000000000000000 ) ;
#40026 = CARTESIAN_POINT ( 'NONE',  ( -0.8801773607111008646, 28.27201867748817321, 2.915334737309923430 ) ) ;
#40027 = ORIENTED_EDGE ( 'NONE', *, *, #7823, .T. ) ;
#40028 = CARTESIAN_POINT ( 'NONE',  ( 12.63842701281683922, 9.550597817667449974, -9.846743663894590881 ) ) ;
#40029 = AXIS2_PLACEMENT_3D ( 'NONE', #8496, #38999, #69986 ) ;
#40030 = CARTESIAN_POINT ( 'NONE',  ( 12.91533473730993009, 66.60535201082150536, -10.88017736071109987 ) ) ;
#40031 = CARTESIAN_POINT ( 'NONE',  ( 0.000000000000000000, 0.5000000000000004441, 0.000000000000000000 ) ) ;
#40032 = CARTESIAN_POINT ( 'NONE',  ( 0.1532563361054083140, 6.008931151000784787, 1.131784320476157264E-15 ) ) ;
#40033 = CARTESIAN_POINT ( 'NONE',  ( 7.361572987183169658, -0.03273551566588185635, -9.846743663894592657 ) ) ;
#40034 = AXIS2_PLACEMENT_3D ( 'NONE', #42227, #29173, #58180 ) ;
#40035 = EDGE_CURVE ( 'NONE', #9509, #75439, #52636, .T. ) ;
#40037 = CARTESIAN_POINT ( 'NONE',  ( -8.124115902427741176, 75.04369783535875627, 3.000000000000000000 ) ) ;
#40036 = CARTESIAN_POINT ( 'NONE',  ( 10.00000000000000000, 51.81368534415484106, -10.88017736071110342 ) ) ;
#40038 = CARTESIAN_POINT ( 'NONE',  ( 0.5774900079438590739, 67.64701867748817676, -5.440088680355550821 ) ) ;
#40040 = ORIENTED_EDGE ( 'NONE', *, *, #82692, .F. ) ;
#40039 = CARTESIAN_POINT ( 'NONE',  ( 7.361572987183169658, -0.03273551566588185635, -9.846743663894592657 ) ) ;
#40041 = CARTESIAN_POINT ( 'NONE',  ( 1.472469842513823179, 61.42559781766745175, 4.923371831947296329 ) ) ;
#40042 = ORIENTED_EDGE ( 'NONE', *, *, #87703, .T. ) ;
#40043 = VERTEX_POINT ( 'NONE', #15742 ) ;
#40044 = CARTESIAN_POINT ( 'NONE',  ( -7.750000000000000000, 79.82179676972448590, 6.250000000000000000 ) ) ;
#40045 = CARTESIAN_POINT ( 'NONE',  ( 20.36894250292379738, 9.928748834913966093, -10.36894250292379027 ) ) ;
#40046 = CARTESIAN_POINT ( 'NONE',  ( 0.6178305044545838731, 54.74863466993042493, 9.382169495545420901 ) ) ;
#40047 = CARTESIAN_POINT ( 'NONE',  ( -2.266590686148945544, 22.22041550158063572, 7.082119434687048631 ) ) ;
#40048 = DIRECTION ( 'NONE',  ( -0.000000000000000000, -1.000000000000000000, -0.000000000000000000 ) ) ;
#40049 = LINE ( 'NONE', #2077, #94477 ) ;
#40050 = CARTESIAN_POINT ( 'NONE',  ( 0.5774900079438590739, 17.64701867748817321, -5.440088680355550821 ) ) ;
#40051 = DIRECTION ( 'NONE',  ( -1.000000000000000000, 0.000000000000000000, 0.000000000000000000 ) ) ;
#40052 = ORIENTED_EDGE ( 'NONE', *, *, #92212, .T. ) ;
#40053 = PRESENTATION_STYLE_ASSIGNMENT (( #25067 ) ) ;
#40054 = CARTESIAN_POINT ( 'NONE',  ( 10.00000000000000000, -0.2410688489992152128, -9.846743663894594434 ) ) ;
#40055 = CARTESIAN_POINT ( 'NONE',  ( 19.38216949554541557, 27.24863466993041783, -9.382169495545420901 ) ) ;
#40056 = CARTESIAN_POINT ( 'NONE',  ( 19.84674366389459266, 43.30059781766744464, 2.638427012816836559 ) ) ;
#40057 = CARTESIAN_POINT ( 'NONE',  ( 7.684764310694891520, 14.49999999999999112, -12.88194075009941564 ) ) ;
#40058 = CARTESIAN_POINT ( 'NONE',  ( 10.00000000000000000, 17.87363466993041783, -12.81628187352647608 ) ) ;
#40059 = DIRECTION ( 'NONE',  ( 1.000000000000000000, 0.000000000000000000, 0.000000000000000000 ) ) ;
#40060 = CARTESIAN_POINT ( 'NONE',  ( 10.00000000000000000, 29.75893115100078745, -9.846743663894594434 ) ) ;
#40061 = CIRCLE ( 'NONE', #17661, 14.49999999999999822 ) ;
#40062 = CARTESIAN_POINT ( 'NONE',  ( 0.1532563361054100626, 0.8005978176674514168, -2.638427012816831230 ) ) ;
#40063 = VERTEX_POINT ( 'NONE', #45731 ) ;
#40064 = ORIENTED_EDGE ( 'NONE', *, *, #8840, .T. ) ;
#40065 = CARTESIAN_POINT ( 'NONE',  ( 17.96484262340118221, 31.18868534415483751, -7.964842623401177768 ) ) ;
#40066 = CARTESIAN_POINT ( 'NONE',  ( 6.204703633549690345, 27.84541550158063217, 14.16423886937410082 ) ) ;
#40067 = CARTESIAN_POINT ( 'NONE',  ( 7.361572987183169658, 44.96726448433412315, -9.846743663894592657 ) ) ;
#40068 = EDGE_CURVE ( 'NONE', #85555, #59552, #82009, .T. ) ;
#40069 = CARTESIAN_POINT ( 'NONE',  ( 14.92337183194729633, 17.67559781766745175, 8.527530157486181039 ) ) ;
#40071 = DIRECTION ( 'NONE',  ( 1.000000000000000000, 0.000000000000000000, 0.000000000000000000 ) ) ;
#40070 = CARTESIAN_POINT ( 'NONE',  ( 3.591859063236761518, 54.95696800326376064, 11.09922568453594849 ) ) ;
#40072 = CARTESIAN_POINT ( 'NONE',  ( 20.88017736071110875, 30.77201867748816966, -2.915334737309920765 ) ) ;
#40073 = DIRECTION ( 'NONE',  ( -0.000000000000000000, -0.000000000000000000, 1.000000000000000000 ) ) ;
#40074 = CARTESIAN_POINT ( 'NONE',  ( 0.6178305044545838731, 19.74863466993042138, 9.382169495545420901 ) ) ;
#40075 = CARTESIAN_POINT ( 'NONE',  ( 14.92337183194729988, 34.34226448433411605, -8.527530157486177487 ) ) ;
#40076 = CARTESIAN_POINT ( 'NONE',  ( 7.964842623401177768, 1.188685344154840395, -7.964842623401181321 ) ) ;
#40077 = CARTESIAN_POINT ( 'NONE',  ( 19.38216949554541557, 42.24863466993041783, -9.382169495545420901 ) ) ;
#40078 = CARTESIAN_POINT ( 'NONE',  ( 4.856044144387705153, 15.00000000000000888, -13.79699902221158858 ) ) ;
#40080 = DIRECTION ( 'NONE',  ( -0.9975640502598243087, 0.06975647374412545509, 0.000000000000000000 ) ) ;
#40079 = CARTESIAN_POINT ( 'NONE',  ( 0.5774900079438607392, 58.48035201082151247, 5.440088680355550821 ) ) ;
#40081 = FACE_OUTER_BOUND ( 'NONE', #81467, .T. ) ;
#40082 = ADVANCED_FACE ( 'NONE', ( #61219, #29237, #61696, #91722 ), #23243, .T. ) ;
#40083 = PLANE ( 'NONE',  #20886 ) ;
#40084 = CARTESIAN_POINT ( 'NONE',  ( 20.88017736071110875, 50.77201867748817676, -2.915334737309920765 ) ) ;
#40085 = CARTESIAN_POINT ( 'NONE',  ( 10.00000000000000178, 64.31368534415483396, 10.88017736071110342 ) ) ;
#40086 = DIRECTION ( 'NONE',  ( 0.000000000000000000, 0.000000000000000000, 1.000000000000000000 ) ) ;
#40087 = DIRECTION ( 'NONE',  ( 1.000000000000000000, -1.257568779154408793E-17, 0.000000000000000000 ) ) ;
#40088 = ADVANCED_FACE ( 'NONE', ( #71190 ), #33167, .F. ) ;
#40089 = ADVANCED_FACE ( 'NONE', ( #56665 ), #86742, .T. ) ;
#40090 = CARTESIAN_POINT ( 'NONE',  ( 0.5774900079438607392, 13.48035201082150358, 5.440088680355550821 ) ) ;
#40091 = CARTESIAN_POINT ( 'NONE',  ( 19.84674366389459266, 58.30059781766745886, 2.638427012816836559 ) ) ;
#40093 = CARTESIAN_POINT ( 'NONE',  ( 20.15039907845753220, 44.72266099184918176, 6.262539305110078836 ) ) ;
#40092 = CARTESIAN_POINT ( 'NONE',  ( 20.88017736071110519, 15.56368534415483751, 2.639326808657452039E-16 ) ) ;
#40094 = CIRCLE ( 'NONE', #12886, 1.249999999999987121 ) ;
#40095 = CARTESIAN_POINT ( 'NONE',  ( 22.81628187352647785, 26.41530133659708923, 3.434112377981063169 ) ) ;
#40096 = ORIENTED_EDGE ( 'NONE', *, *, #39564, .F. ) ;
#40097 = CARTESIAN_POINT ( 'NONE',  ( 0.5774900079438590739, 52.64701867748817676, -5.440088680355550821 ) ) ;
#40098 = CARTESIAN_POINT ( 'NONE',  ( 5.076628168052703671, 36.84226448433412315, 8.527530157486179263 ) ) ;
#40099 = CARTESIAN_POINT ( 'NONE',  ( 3.591859063236763294, 13.29030133659708746, -11.09922568453595026 ) ) ;
#40100 = CARTESIAN_POINT ( 'NONE',  ( -0.8801773607110991993, 17.85535201082150536, -2.915334737309923874 ) ) ;
#40101 = CARTESIAN_POINT ( 'NONE',  ( 12.91533473730993009, 36.60535201082151247, -10.88017736071109987 ) ) ;
#40102 = CARTESIAN_POINT ( 'NONE',  ( 2.917880565312950480, 55.97041550158063217, -12.26659068614894821 ) ) ;
#40103 = CARTESIAN_POINT ( 'NONE',  ( 2.791683348922237240, 40.38393115100078035, -7.208316651077763204 ) ) ;
#40104 = CARTESIAN_POINT ( 'NONE',  ( 12.91533473730993009, 66.60535201082150536, -10.88017736071109987 ) ) ;
#40105 = SURFACE_STYLE_FILL_AREA ( #47605 ) ;
#40106 = CARTESIAN_POINT ( 'NONE',  ( 6.204703633549690345, 10.76208216824729824, -14.16423886937410259 ) ) ;
#40107 =( NAMED_UNIT ( * ) SI_UNIT ( $, .STERADIAN. ) SOLID_ANGLE_UNIT ( ) );
#40108 = CARTESIAN_POINT ( 'NONE',  ( -10.20000000000000107, 43.92361346574197256, -2.900000000000000799 ) ) ;
#40109 = EDGE_LOOP ( 'NONE', ( #88204, #55291, #54929, #24946 ) ) ;
#40110 = ORIENTED_EDGE ( 'NONE', *, *, #17867, .T. ) ;
#40111 = CARTESIAN_POINT ( 'NONE',  ( 13.79529636645031943, 30.34541550158063927, -14.16423886937409904 ) ) ;
#40112 = CARTESIAN_POINT ( 'NONE',  ( 24.16423886937409904, 34.09541550158064638, 3.795296366450317205 ) ) ;
#40113 = CARTESIAN_POINT ( 'NONE',  ( 12.63842701281683922, 9.550597817667449974, -9.846743663894590881 ) ) ;
#40114 = EDGE_CURVE ( 'NONE', #60118, #74806, #85161, .T. ) ;
#40115 = CARTESIAN_POINT ( 'NONE',  ( 16.40814093676323893, 20.79030133659708923, 11.09922568453595026 ) ) ;
#40116 = CARTESIAN_POINT ( 'NONE',  ( 18.52753015748618282, 58.92559781766745886, -4.923371831947291888 ) ) ;
#40117 = CARTESIAN_POINT ( 'NONE',  ( -18.89999999999999503, 98.99999999999998579, 8.000000000000000000 ) ) ;
#40119 = CARTESIAN_POINT ( 'NONE',  ( 13.43411237798106583, 37.66530133659708923, -12.81628187352647252 ) ) ;
#40118 = CARTESIAN_POINT ( 'NONE',  ( 15.44008868035555260, 54.73035201082150536, 9.422509992056143702 ) ) ;
#40120 = CARTESIAN_POINT ( 'NONE',  ( 10.00000000000000000, 25.55374883491396787, -14.16423886937410082 ) ) ;
#40121 = CARTESIAN_POINT ( 'NONE',  ( 20.88017736071110875, 20.77201867748816611, -2.915334737309920765 ) ) ;
#40122 = CARTESIAN_POINT ( 'NONE',  ( -8.839000071697160621, 14.95037109469996395, 11.81225584161635211 ) ) ;
#40123 = CARTESIAN_POINT ( 'NONE',  ( 17.96484262340118221, 66.18868534415483396, -7.964842623401177768 ) ) ;
#40124 = EDGE_CURVE ( 'NONE', #14317, #18642, #48389, .T. ) ;
#40125 = CARTESIAN_POINT ( 'NONE',  ( -9.846743663894596210, -9.199402182332550026, -2.638427012816824124 ) ) ;
#40126 = CARTESIAN_POINT ( 'NONE',  ( 17.20831665107776587, 7.883931151000784787, 7.208316651077764980 ) ) ;
#40127 = EDGE_LOOP ( 'NONE', ( #11691, #79511, #19012, #66138, #14959, #94767 ) ) ;
#40128 = PLANE ( 'NONE',  #85838 ) ;
#40129 = CARTESIAN_POINT ( 'NONE',  ( 1.983216688680936812, -0.03417435944610275333, -14.11131997956737649 ) ) ;
#40130 = ORIENTED_EDGE ( 'NONE', *, *, #80819, .F. ) ;
#40131 = CIRCLE ( 'NONE', #96014, 11.92686044187656513 ) ;
#40132 = CARTESIAN_POINT ( 'NONE',  ( 17.08211943468705130, 3.470415501580634388, 12.26659068614894998 ) ) ;
#40134 = CARTESIAN_POINT ( 'NONE',  ( -0.8801773607111008646, 13.27201867748817321, 2.915334737309923430 ) ) ;
#40133 = CARTESIAN_POINT ( 'NONE',  ( 15.44008868035555260, 9.730352010821505360, 9.422509992056143702 ) ) ;
#40136 = CARTESIAN_POINT ( 'NONE',  ( 3.591859063236763294, 3.290301336597087012, -11.09922568453595026 ) ) ;
#40135 = CARTESIAN_POINT ( 'NONE',  ( 12.63842701281683034, 42.46726448433412315, 9.846743663894596210 ) ) ;
#40137 = DIRECTION ( 'NONE',  ( 0.000000000000000000, 1.000000000000000000, 0.000000000000000000 ) ) ;
#40138 = DIRECTION ( 'NONE',  ( 6.938893903907222067E-15, -1.000000000000000000, 0.000000000000000000 ) ) ;
#40139 = TOROIDAL_SURFACE ( 'NONE', #19359, 14.49999999999999822, 0.5000000000000000000 ) ;
#40140 = CARTESIAN_POINT ( 'NONE',  ( 22.81628187352647785, 6.623634669930420493, 6.195893100308588602E-16 ) ) ;
#40141 = ORIENTED_EDGE ( 'NONE', *, *, #16476, .F. ) ;
#40142 = CARTESIAN_POINT ( 'NONE',  ( 20.36894250292379382, 48.67874883491396076, 10.36894250292379205 ) ) ;
#40143 = ORIENTED_EDGE ( 'NONE', *, *, #88343, .T. ) ;
#40144 = CARTESIAN_POINT ( 'NONE',  ( 10.00000000000000178, 63.05374883491396076, 14.16423886937410082 ) ) ;
#40145 = ORIENTED_EDGE ( 'NONE', *, *, #81064, .T. ) ;
#40146 = CARTESIAN_POINT ( 'NONE',  ( 15.44008868035555260, 39.73035201082150536, 9.422509992056143702 ) ) ;
#40147 = CARTESIAN_POINT ( 'NONE',  ( 0.5774900079438607392, 43.48035201082151247, 5.440088680355550821 ) ) ;
#40148 = CARTESIAN_POINT ( 'NONE',  ( 5.076628168052704559, 60.17559781766745175, -8.527530157486179263 ) ) ;
#40149 = CARTESIAN_POINT ( 'NONE',  ( 10.00000000000000178, 34.31368534415484106, 10.88017736071110342 ) ) ;
#40150 = CARTESIAN_POINT ( 'NONE',  ( 7.084665262690076126, 69.10535201082151957, 10.88017736071109987 ) ) ;
#40151 = CARTESIAN_POINT ( 'NONE',  ( 19.42250999205614193, 25.14701867748817321, 5.440088680355555262 ) ) ;
#40153 = STYLED_ITEM ( 'NONE', ( #81626 ), #63320 ) ;
#40152 = CARTESIAN_POINT ( 'NONE',  ( 1.354709868695545216, 14.49999999999999112, 14.93870011653158336 ) ) ;
#40154 =( LENGTH_UNIT ( ) NAMED_UNIT ( * ) SI_UNIT ( .MILLI., .METRE. ) );
#40155 = CARTESIAN_POINT ( 'NONE',  ( -3.521809514228321003, -0.8352226969044395100, 2.499999999999597655 ) ) ;
#40156 = ORIENTED_EDGE ( 'NONE', *, *, #82857, .F. ) ;
#40157 = DIRECTION ( 'NONE',  ( 0.9975640502598257520, -0.06975647374410356982, 0.000000000000000000 ) ) ;
#40158 = CARTESIAN_POINT ( 'NONE',  ( 7.361572987183169658, 39.96726448433411605, -9.846743663894592657 ) ) ;
#40159 = CARTESIAN_POINT ( 'NONE',  ( -11.48952521350012113, 4.018634162980579609E-16, -8.845383562533903898 ) ) ;
#40160 = CARTESIAN_POINT ( 'NONE',  ( 10.00000000000000178, 45.37363466993041783, 12.81628187352647608 ) ) ;
#40161 = AXIS2_PLACEMENT_3D ( 'NONE', #1011, #77969, #84498 ) ;
#40162 = B_SPLINE_CURVE_WITH_KNOTS ( 'NONE', 3,
 ( #22357, #30321, #35859, #53323 ),
 .UNSPECIFIED., .F., .F.,
 ( 4, 4 ),
 ( 1.854451039242195167E-16, 0.001060528352561992006 ),
 .UNSPECIFIED. ) ;
#40163 = CARTESIAN_POINT ( 'NONE',  ( -1.761054936948036165, 12.86682408883346440, -10.00000000000000000 ) ) ;
#40164 = DIRECTION ( 'NONE',  ( 1.000000000000000000, 1.189524669241238632E-14, 0.000000000000000000 ) ) ;
#40165 = CARTESIAN_POINT ( 'NONE',  ( -45.73459272351794169, 104.7119485869564528, 5.163735687858058476 ) ) ;
#40166 = CARTESIAN_POINT ( 'NONE',  ( 7.361572987183169658, 54.96726448433413026, -9.846743663894592657 ) ) ;
#40167 = CARTESIAN_POINT ( 'NONE',  ( 20.36894250292379382, 43.67874883491397497, 10.36894250292379205 ) ) ;
#40168 = CARTESIAN_POINT ( 'NONE',  ( 5.076628168052703671, 56.84226448433412315, 8.527530157486179263 ) ) ;
#40169 = VERTEX_POINT ( 'NONE', #87154 ) ;
#40171 = VECTOR ( 'NONE', #66151, 1000.000000000000000 ) ;
#40170 = CARTESIAN_POINT ( 'NONE',  ( 19.72487221294570858, 41.86607318730076344, 6.500000000000000888 ) ) ;
#40172 = CARTESIAN_POINT ( 'NONE',  ( 17.20831665107776587, 22.88393115100078745, 7.208316651077764980 ) ) ;
#40173 = CARTESIAN_POINT ( 'NONE',  ( 6.565887622018943937, 58.08196800326376064, -12.81628187352647608 ) ) ;
#40174 = CARTESIAN_POINT ( 'NONE',  ( 17.20831665107776587, 64.13393115100079456, -7.208316651077762316 ) ) ;
#40175 = CARTESIAN_POINT ( 'NONE',  ( 12.91533473730992121, 64.52201867748817676, 10.88017736071110164 ) ) ;
#40176 = DIRECTION ( 'NONE',  ( 0.000000000000000000, 0.000000000000000000, -1.000000000000000000 ) ) ;
#40177 = ORIENTED_EDGE ( 'NONE', *, *, #37160, .T. ) ;
#40178 = CARTESIAN_POINT ( 'NONE',  ( 17.08211943468705840, 60.13708216824729647, -12.26659068614894466 ) ) ;
#40179 = SURFACE_SIDE_STYLE ('',( #9188 ) ) ;
#40180 = CARTESIAN_POINT ( 'NONE',  ( 20.88017736071110164, 30.35535201082151247, 2.915334737309930979 ) ) ;
#40182 = CARTESIAN_POINT ( 'NONE',  ( 12.91533473730992121, 54.52201867748816255, 10.88017736071110164 ) ) ;
#40181 = CARTESIAN_POINT ( 'NONE',  ( 6.565887622018943937, 18.08196800326375708, -12.81628187352647608 ) ) ;
#40183 = CARTESIAN_POINT ( 'NONE',  ( -4.880290883660339141, 0.000000000000000000, -2.433223276543861502 ) ) ;
#40184 = DIRECTION ( 'NONE',  ( -1.000000000000000000, 0.000000000000000000, 0.000000000000000000 ) ) ;
#40185 = CARTESIAN_POINT ( 'NONE',  ( -0.1503990784575275907, 58.10158574516644592, 6.262539305110076171 ) ) ;
#40186 = CARTESIAN_POINT ( 'NONE',  ( -5.991992585808713301, 15.00000000000000000, 13.20401548210291054 ) ) ;
#40187 = CARTESIAN_POINT ( 'NONE',  ( 17.20831665107776587, 54.13393115100079456, -7.208316651077762316 ) ) ;
#40188 = CARTESIAN_POINT ( 'NONE',  ( -10.88017736071109987, -36.72798132251182324, 2.915334737309934532 ) ) ;
#40189 = CARTESIAN_POINT ( 'NONE',  ( 0.6178305044545818747, 8.498634669930421381, -9.382169495545419124 ) ) ;
#40190 = ADVANCED_FACE ( 'NONE', ( #49164 ), #5307, .T. ) ;
#40192 = CARTESIAN_POINT ( 'NONE',  ( 1.821708436314967372, 66.66792564121897158, -6.500000000000079048 ) ) ;
#40191 = CARTESIAN_POINT ( 'NONE',  ( 4.559911319644449179, 8.897018677488173211, 9.422509992056141925 ) ) ;
#40193 = DIRECTION ( 'NONE',  ( 0.000000000000000000, -1.000000000000000000, 0.000000000000000000 ) ) ;
#40194 = CARTESIAN_POINT ( 'NONE',  ( -4.164238869374099039, 31.80374883491396432, 8.674139862899312516E-16 ) ) ;
#40195 = CARTESIAN_POINT ( 'NONE',  ( 22.26659068614894466, 23.88708216824730357, 7.082119434687054849 ) ) ;
#40196 = CARTESIAN_POINT ( 'NONE',  ( -0.8801773607111009756, 3.063685344154838397, 1.068504757029289695E-15 ) ) ;
#40197 = CARTESIAN_POINT ( 'NONE',  ( 0.1532563361054082862, 36.21726448433410894, 2.638427012816831674 ) ) ;
#40198 = CARTESIAN_POINT ( 'NONE',  ( 12.63842701281683922, 14.55059781766744997, -9.846743663894590881 ) ) ;
#40199 = CARTESIAN_POINT ( 'NONE',  ( 20.88017736071110164, 20.35535201082150891, 2.915334737309930979 ) ) ;
#40200 = EDGE_CURVE ( 'NONE', #56195, #36584, #49968, .T. ) ;
#40201 = AXIS2_PLACEMENT_3D ( 'NONE', #36277, #3824, #12780 ) ;
#40202 = EDGE_LOOP ( 'NONE', ( #14821, #79860, #78718, #59081 ) ) ;
#40203 = CARTESIAN_POINT ( 'NONE',  ( 10.00000000000000000, 44.75893115100078745, -9.846743663894594434 ) ) ;
#40204 = CARTESIAN_POINT ( 'NONE',  ( 20.88017736071110875, 45.77201867748816966, -2.915334737309920765 ) ) ;
#40205 = CARTESIAN_POINT ( 'NONE',  ( 17.20831665107776587, 59.13393115100078745, -7.208316651077762316 ) ) ;
#40207 = CARTESIAN_POINT ( 'NONE',  ( -1.926860441876562247, 17.45379003517447458, -3.195792623639530650 ) ) ;
#40206 = CARTESIAN_POINT ( 'NONE',  ( -4.164238869374098151, 16.59541550158063927, -3.795296366450310543 ) ) ;
#40208 = DIRECTION ( 'NONE',  ( -0.000000000000000000, -1.000000000000000000, -0.000000000000000000 ) ) ;
#40209 = ADVANCED_FACE ( 'NONE', ( #31694 ), #48172, .F. ) ;
#40210 = UNCERTAINTY_MEASURE_WITH_UNIT (LENGTH_MEASURE( 1.000000000000000082E-05 ), #97851, 'distance_accuracy_value', 'NONE');
#40211 = CARTESIAN_POINT ( 'NONE',  ( 0.1532563361054082862, 16.21726448433411960, 2.638427012816831674 ) ) ;
#40212 = CARTESIAN_POINT ( 'NONE',  ( -2.816281873526473856, 49.33196800326374643, 3.434112377981055619 ) ) ;
#40213 = CARTESIAN_POINT ( 'NONE',  ( 5.076628168052703671, 51.84226448433412315, 8.527530157486179263 ) ) ;
#40214 = ORIENTED_EDGE ( 'NONE', *, *, #68885, .F. ) ;
#40215 = DIRECTION ( 'NONE',  ( 0.000000000000000000, 0.000000000000000000, -1.000000000000000000 ) ) ;
#40216 = CARTESIAN_POINT ( 'NONE',  ( 2.035157376598822676, 7.438685344154837509, -7.964842623401177768 ) ) ;
#40217 = CARTESIAN_POINT ( 'NONE',  ( 10.00000000000000000, 56.81368534415484106, -10.88017736071110342 ) ) ;
#40218 = CARTESIAN_POINT ( 'NONE',  ( -4.164238869374099039, 6.803748834913967869, 8.674139862899312516E-16 ) ) ;
#40219 = CARTESIAN_POINT ( 'NONE',  ( 5.076628168052703671, 1.842264484334118047, 8.527530157486179263 ) ) ;
#40220 = CARTESIAN_POINT ( 'NONE',  ( 1.472469842513823179, 55.59226448433412315, -4.923371831947296329 ) ) ;
#40221 = CARTESIAN_POINT ( 'NONE',  ( 19.42250999205614193, 20.14701867748817321, 5.440088680355555262 ) ) ;
#40222 = CARTESIAN_POINT ( 'NONE',  ( 20.15039907845753930, 11.74884699246888964, 6.262539305110064625 ) ) ;
#40223 = CARTESIAN_POINT ( 'NONE',  ( 12.63842701281683922, 59.55059781766744464, -9.846743663894590881 ) ) ;
#40224 = CARTESIAN_POINT ( 'NONE',  ( 7.361572987183169658, 4.967264484334119601, -9.846743663894592657 ) ) ;
#40225 = AXIS2_PLACEMENT_3D ( 'NONE', #17591, #77573, #16598 ) ;
#40226 = CARTESIAN_POINT ( 'NONE',  ( -1.099225684535947600, 63.70696800326376774, -6.408140936763238038 ) ) ;
#40227 = ORIENTED_EDGE ( 'NONE', *, *, #56131, .T. ) ;
#40228 = AXIS2_PLACEMENT_3D ( 'NONE', #84324, #32272, #31783 ) ;
#40229 = ORIENTED_EDGE ( 'NONE', *, *, #59300, .T. ) ;
#40230 = CYLINDRICAL_SURFACE ( 'NONE', #11806, 0.5000000000000004441 ) ;
#40231 = CARTESIAN_POINT ( 'NONE',  ( 18.72515096720573879, 35.05509018479936145, 6.499999999999937828 ) ) ;
#40232 = SURFACE_STYLE_FILL_AREA ( #48701 ) ;
#40233 = CARTESIAN_POINT ( 'NONE',  ( -0.3689425029237881626, 37.42874883491396787, 10.36894250292379027 ) ) ;
#40234 = CARTESIAN_POINT ( 'NONE',  ( 0.1532563361054100626, 50.80059781766745175, -2.638427012816831230 ) ) ;
#40235 = CARTESIAN_POINT ( 'NONE',  ( 0.1532563361054083140, 16.00893115100078390, 1.131784320476157264E-15 ) ) ;
#40236 = CARTESIAN_POINT ( 'NONE',  ( 0.2751277870542911952, 38.21833443783937412, 6.499999999999992006 ) ) ;
#40238 = CARTESIAN_POINT ( 'NONE',  ( 0.1532563361054083140, 66.00893115100079456, 1.131784320476157264E-15 ) ) ;
#40237 = CARTESIAN_POINT ( 'NONE',  ( 2.035157376598824452, 13.68868534415483751, 7.964842623401179544 ) ) ;
#40239 = CARTESIAN_POINT ( 'NONE',  ( -0.1503990784575328643, 35.12777174578612716, 6.262539305110068177 ) ) ;
#40240 = CARTESIAN_POINT ( 'NONE',  ( 20.36894250292379382, 38.67874883491396076, 10.36894250292379205 ) ) ;
#40241 = CARTESIAN_POINT ( 'NONE',  ( -0.3689425029237898834, 61.17874883491396076, -10.36894250292378850 ) ) ;
#40242 = CARTESIAN_POINT ( 'NONE',  ( 10.00000000000000178, 67.25893115100079456, 9.846743663894594434 ) ) ;
#40243 = COLOUR_RGB ( '', 0.31764706, 0.68627451, 0.89019608) ;
#40244 = CARTESIAN_POINT ( 'NONE',  ( 18.00000000000000000, 77.07179676972447169, 4.250000000000000000 ) ) ;
#40245 = CARTESIAN_POINT ( 'NONE',  ( 0.5774900079438607392, 68.48035201082150536, 5.440088680355550821 ) ) ;
#40246 = ADVANCED_FACE ( 'NONE', ( #63661 ), #18185, .T. ) ;
#40247 = CARTESIAN_POINT ( 'NONE',  ( 2.791683348922240793, 11.63393115100078568, 7.208316651077764092 ) ) ;
#40248 = CARTESIAN_POINT ( 'NONE',  ( -7.124934413272103306, -78.83349193436582425, 4.000000000000000888 ) ) ;
#40249 = ORIENTED_EDGE ( 'NONE', *, *, #68460, .F. ) ;
#40250 = CARTESIAN_POINT ( 'NONE',  ( -27.43587634952537968, 0.5000000000000038858, 10.00000000000000000 ) ) ;
#40251 = CIRCLE ( 'NONE', #11473, 14.49999999999999822 ) ;
#40252 = ORIENTED_EDGE ( 'NONE', *, *, #86646, .T. ) ;
#40253 = CARTESIAN_POINT ( 'NONE',  ( 0.1532563361054083140, 21.00893115100078745, 1.131784320476157264E-15 ) ) ;
#40254 = ORIENTED_EDGE ( 'NONE', *, *, #60958, .T. ) ;
#40255 = CARTESIAN_POINT ( 'NONE',  ( 24.16423886937410614, 29.51208216824729647, -3.795296366450302550 ) ) ;
#40256 = CARTESIAN_POINT ( 'NONE',  ( 19.84674366389459266, 23.71726448433412315, -2.638427012816827677 ) ) ;
#40257 = CARTESIAN_POINT ( 'NONE',  ( 10.00000000000000000, 41.81368534415484106, -10.88017736071110342 ) ) ;
#40258 = LINE ( 'NONE', #18739, #74532 ) ;
#40260 = EDGE_CURVE ( 'NONE', #76878, #1436, #60483, .T. ) ;
#40259 = VERTEX_POINT ( 'NONE', #47185 ) ;
#40261 = CARTESIAN_POINT ( 'NONE',  ( 12.91533473730992121, 39.52201867748817676, 10.88017736071110164 ) ) ;
#40262 = CARTESIAN_POINT ( 'NONE',  ( -9.382169495545422677, -11.50136533006958217, -9.382169495545417348 ) ) ;
#40263 = ORIENTED_EDGE ( 'NONE', *, *, #48530, .F. ) ;
#40264 = CARTESIAN_POINT ( 'NONE',  ( 6.204703633549690345, 0.7620821682473009062, -14.16423886937410259 ) ) ;
#40265 = ORIENTED_EDGE ( 'NONE', *, *, #92002, .F. ) ;
#40266 = CARTESIAN_POINT ( 'NONE',  ( -1.099225684535947600, 29.54030133659708923, 6.408140936763237150 ) ) ;
#40267 = B_SPLINE_CURVE_WITH_KNOTS ( 'NONE', 3,
 ( #3762, #85284, #55268, #85781 ),
 .UNSPECIFIED., .F., .F.,
 ( 4, 4 ),
 ( 0.000000000000000000, 0.002392975128318458600 ),
 .UNSPECIFIED. ) ;
#40268 = CARTESIAN_POINT ( 'NONE',  ( 17.20831665107776587, 7.883931151000784787, 7.208316651077764980 ) ) ;
#40269 = DIRECTION ( 'NONE',  ( -0.7716245833877234395, 0.000000000000000000, 0.6360782202777597316 ) ) ;
#40270 = CARTESIAN_POINT ( 'NONE',  ( 0.6178305044545838731, 44.74863466993042493, 9.382169495545420901 ) ) ;
#40271 = CARTESIAN_POINT ( 'NONE',  ( 0.1532563361054083140, 26.00893115100078745, 1.131784320476157264E-15 ) ) ;
#40272 = B_SPLINE_CURVE_WITH_KNOTS ( 'NONE', 3,
 ( #5581, #91024, #89059, #7053, #20574, #81547 ),
 .UNSPECIFIED., .F., .F.,
 ( 4, 2, 4 ),
 ( 0.0002800421825936756258, 0.0006862478247299506375, 0.001092453466866225758 ),
 .UNSPECIFIED. ) ;
#40273 = AXIS2_PLACEMENT_3D ( 'NONE', #62495, #24533, #75541 ) ;
#40274 = ORIENTED_EDGE ( 'NONE', *, *, #33964, .T. ) ;
#40275 = CARTESIAN_POINT ( 'NONE',  ( 1.932340009482123699, 46.49127512925448968, -6.499999999999926281 ) ) ;
#40276 = CARTESIAN_POINT ( 'NONE',  ( -0.8801773607110991993, 52.85535201082151247, -2.915334737309923874 ) ) ;
#40277 = CYLINDRICAL_SURFACE ( 'NONE', #61101, 15.00000000000000000 ) ;
#40278 = LINE ( 'NONE', #38805, #34933 ) ;
#40279 = CARTESIAN_POINT ( 'NONE',  ( 18.52753015748617571, 3.092264484334118269, 4.923371831947298993 ) ) ;
#40280 = CARTESIAN_POINT ( 'NONE',  ( -2.816281873526473856, 9.123634669930421381, 9.499525473075851096E-16 ) ) ;
#40281 = CARTESIAN_POINT ( 'NONE',  ( 11.61621867929611973, 15.00000000000000000, -10.99731149103385874 ) ) ;
#40282 = EDGE_CURVE ( 'NONE', #43677, #63872, #24513, .T. ) ;
#40283 = CARTESIAN_POINT ( 'NONE',  ( 17.20831665107776587, 29.13393115100078390, -7.208316651077762316 ) ) ;
#40284 = CARTESIAN_POINT ( 'NONE',  ( 6.565887622018943937, 63.08196800326376064, -12.81628187352647608 ) ) ;
#40285 = CARTESIAN_POINT ( 'NONE',  ( 22.26659068614894466, 13.88708216824730179, 7.082119434687054849 ) ) ;
#40286 = CARTESIAN_POINT ( 'NONE',  ( 7.361572987183170547, 22.05059781766745530, 9.846743663894590881 ) ) ;
#40287 = CARTESIAN_POINT ( 'NONE',  ( -2.816281873526473856, 39.12363466993041783, 9.499525473075851096E-16 ) ) ;
#40289 = CARTESIAN_POINT ( 'NONE',  ( 9.879999999999988347, 26.99999999999999645, 3.000000000000000000 ) ) ;
#40288 = DIRECTION ( 'NONE',  ( 1.000000000000000000, 0.000000000000000000, 0.000000000000000000 ) ) ;
#40290 = CARTESIAN_POINT ( 'NONE',  ( -0.8801773607111009756, 43.06368534415484106, 1.068504757029289695E-15 ) ) ;
#40291 = CARTESIAN_POINT ( 'NONE',  ( 16.40814093676324603, 2.456968003263753531, -11.09922568453594671 ) ) ;
#40292 = CARTESIAN_POINT ( 'NONE',  ( 34.56412365047463453, 26.99999999999999645, -9.500000000000000000 ) ) ;
#40293 = ADVANCED_FACE ( 'NONE', ( #27639 ), #96156, .F. ) ;
#40294 = CARTESIAN_POINT ( 'NONE',  ( 10.00000000000000000, 29.75893115100078745, -9.846743663894594434 ) ) ;
#40295 = CARTESIAN_POINT ( 'NONE',  ( 0.1532563361054082862, 26.21726448433411605, 2.638427012816831674 ) ) ;
#40296 = CARTESIAN_POINT ( 'NONE',  ( 20.88017736071110164, 20.35535201082150891, 2.915334737309930979 ) ) ;
#40297 = CARTESIAN_POINT ( 'NONE',  ( 3.591859063236761518, 14.95696800326375531, 11.09922568453594849 ) ) ;
#40298 = AXIS2_PLACEMENT_3D ( 'NONE', #74192, #36717, #75191 ) ;
#40299 = CARTESIAN_POINT ( 'NONE',  ( 5.076628168052703671, 21.84226448433411960, 8.527530157486179263 ) ) ;
#40300 = DIRECTION ( 'NONE',  ( 0.000000000000000000, -1.000000000000000000, 0.000000000000000000 ) ) ;
#40301 = CARTESIAN_POINT ( 'NONE',  ( 12.91533473730993009, 16.60535201082150891, -10.88017736071109987 ) ) ;
#40302 = AXIS2_PLACEMENT_3D ( 'NONE', #8308, #67831, #7332 ) ;
#40303 = VERTEX_POINT ( 'NONE', #81625 ) ;
#40304 = AXIS2_PLACEMENT_3D ( 'NONE', #68091, #27609, #66096 ) ;
#40305 = CARTESIAN_POINT ( 'NONE',  ( 19.42250999205614548, 60.98035201082151247, -5.440088680355545492 ) ) ;
#40306 = CARTESIAN_POINT ( 'NONE',  ( 69.60148758828985649, 0.4999999999999935052, 9.500000000000000000 ) ) ;
#40308 = CARTESIAN_POINT ( 'NONE',  ( 19.42250999205614193, 15.14701867748817143, 5.440088680355555262 ) ) ;
#40307 = CARTESIAN_POINT ( 'NONE',  ( 12.63842701281683922, 49.55059781766744464, -9.846743663894590881 ) ) ;
#40309 =( NAMED_UNIT ( * ) SI_UNIT ( $, .STERADIAN. ) SOLID_ANGLE_UNIT ( ) );
#40310 = AXIS2_PLACEMENT_3D ( 'NONE', #55616, #94096, #18597 ) ;
#40311 = CARTESIAN_POINT ( 'NONE',  ( 0.5774900079438590739, 42.64701867748816966, -5.440088680355550821 ) ) ;
#40313 = CARTESIAN_POINT ( 'NONE',  ( -0.3289641300568005855, 20.10497603579417358, 5.963430220938281678 ) ) ;
#40312 = CARTESIAN_POINT ( 'NONE',  ( 15.44008868035555793, 16.39701867748817321, -9.422509992056140149 ) ) ;
#40314 = CARTESIAN_POINT ( 'NONE',  ( 19.84674366389459266, 13.30059781766745353, 2.638427012816836559 ) ) ;
#40315 = CIRCLE ( 'NONE', #67437, 0.2500000000000002220 ) ;
#40316 = CARTESIAN_POINT ( 'NONE',  ( 14.92337183194729633, 37.67559781766745175, 8.527530157486181039 ) ) ;
#40317 = DIRECTION ( 'NONE',  ( 0.9588197348681964938, 0.000000000000000000, -0.2840153447039108214 ) ) ;
#40318 = CARTESIAN_POINT ( 'NONE',  ( 6.000000000000000000, 11.00000000000000000, -5.000000000000000000 ) ) ;
#40319 = CARTESIAN_POINT ( 'NONE',  ( -2.816281873526471635, -1.084698663402913210, -3.434112377981056508 ) ) ;
#40320 = LINE ( 'NONE', #64757, #44209 ) ;
#40322 = CIRCLE ( 'NONE', #33861, 15.00000000000000000 ) ;
#40321 = CARTESIAN_POINT ( 'NONE',  ( 22.26659068614895176, 19.72041550158063572, -7.082119434687042414 ) ) ;
#40323 = CARTESIAN_POINT ( 'NONE',  ( 19.84674366389459621, 38.50893115100078745, 7.409399052514197653E-17 ) ) ;
#40324 = EDGE_CURVE ( 'NONE', #29627, #88696, #32396, .T. ) ;
#40325 = DIRECTION ( 'NONE',  ( -0.02177529129954166101, -0.9997628902338895340, -5.564908543122672015E-14 ) ) ;
#40326 = CARTESIAN_POINT ( 'NONE',  ( 17.96484262340118221, 6.188685344154837509, -7.964842623401177768 ) ) ;
#40327 = CARTESIAN_POINT ( 'NONE',  ( 18.52753015748618282, 23.92559781766745530, -4.923371831947291888 ) ) ;
#40329 = FACE_OUTER_BOUND ( 'NONE', #77218, .T. ) ;
#40328 = LINE ( 'NONE', #34262, #77061 ) ;
#40330 = CARTESIAN_POINT ( 'NONE',  ( 19.42250999205614193, 40.14701867748817676, 5.440088680355555262 ) ) ;
#40331 = CARTESIAN_POINT ( 'NONE',  ( 10.00000000000000178, 60.37363466993041783, 12.81628187352647608 ) ) ;
#40332 = EDGE_CURVE ( 'NONE', #79587, #9323, #35132, .T. ) ;
#40333 = CARTESIAN_POINT ( 'NONE',  ( 19.42250999205614548, 15.98035201082150714, -5.440088680355545492 ) ) ;
#40334 = CARTESIAN_POINT ( 'NONE',  ( 13.43411237798105340, 45.58196800326374643, 12.81628187352647963 ) ) ;
#40335 = CARTESIAN_POINT ( 'NONE',  ( 21.09922568453594849, 11.20696800326375531, 6.408140936763242479 ) ) ;
#40336 = CARTESIAN_POINT ( 'NONE',  ( 12.63842701281683922, 19.55059781766745175, -9.846743663894590881 ) ) ;
#40337 = ORIENTED_EDGE ( 'NONE', *, *, #56390, .T. ) ;
#40338 = CARTESIAN_POINT ( 'NONE',  ( 0.000000000000000000, 0.5000000000000004441, 0.000000000000000000 ) ) ;
#40339 = FACE_OUTER_BOUND ( 'NONE', #39301, .T. ) ;
#40340 = CARTESIAN_POINT ( 'NONE',  ( -0.3689425029237898834, 51.17874883491397497, -10.36894250292378850 ) ) ;
#40341 = CARTESIAN_POINT ( 'NONE',  ( -4.164238869374098151, 26.59541550158063217, -3.795296366450310543 ) ) ;
#40342 = CARTESIAN_POINT ( 'NONE',  ( 2.035157376598824452, 23.68868534415484461, 7.964842623401179544 ) ) ;
#40344 = DIRECTION ( 'NONE',  ( 0.000000000000000000, -1.000000000000000000, 0.000000000000000000 ) ) ;
#40343 = CARTESIAN_POINT ( 'NONE',  ( 20.88017736071110875, 55.77201867748816966, -2.915334737309920765 ) ) ;
#40345 = DIRECTION ( 'NONE',  ( -0.8320502943378437211, 0.5547001962252290364, 0.000000000000000000 ) ) ;
#40346 = DIRECTION ( 'NONE',  ( -1.000000000000000000, 0.000000000000000000, 0.000000000000000000 ) ) ;
#40347 = CARTESIAN_POINT ( 'NONE',  ( 17.96484262340118221, 61.18868534415482685, -7.964842623401177768 ) ) ;
#40348 = CARTESIAN_POINT ( 'NONE',  ( 10.00000000000000178, 17.25893115100078745, 9.846743663894594434 ) ) ;
#40349 = FACE_OUTER_BOUND ( 'NONE', #14260, .T. ) ;
#40350 = PRESENTATION_STYLE_ASSIGNMENT (( #54346 ) ) ;
#40351 = CARTESIAN_POINT ( 'NONE',  ( 17.20831665107776587, 22.88393115100078745, 7.208316651077764980 ) ) ;
#40352 = CARTESIAN_POINT ( 'NONE',  ( 14.92337183194729988, 49.34226448433411605, -8.527530157486177487 ) ) ;
#40353 = CARTESIAN_POINT ( 'NONE',  ( 10.00000000000000178, 19.31368534415484106, 10.88017736071110342 ) ) ;
#40354 = AXIS2_PLACEMENT_3D ( 'NONE', #87361, #41401, #71867 ) ;
#40355 = CARTESIAN_POINT ( 'NONE',  ( 0.6178305044545818747, 33.49863466993042493, -9.382169495545419124 ) ) ;
#40356 = CARTESIAN_POINT ( 'NONE',  ( 15.44008868035555793, 51.39701867748816966, -9.422509992056140149 ) ) ;
#40357 = CARTESIAN_POINT ( 'NONE',  ( 7.361572987183169658, 29.96726448433411960, -9.846743663894592657 ) ) ;
#40359 = CARTESIAN_POINT ( 'NONE',  ( 5.076628168052703671, 26.84226448433411960, 8.527530157486179263 ) ) ;
#40358 = CARTESIAN_POINT ( 'NONE',  ( 22.26659068614894466, 48.88708216824730357, 7.082119434687054849 ) ) ;
#40360 = CARTESIAN_POINT ( 'NONE',  ( -14.43100913236846061, 15.00000000000000000, -1.412789942453363423 ) ) ;
#40361 = CARTESIAN_POINT ( 'NONE',  ( 0.1532563361054083140, 51.00893115100078745, 1.131784320476157264E-15 ) ) ;
#40363 = CARTESIAN_POINT ( 'NONE',  ( 24.16423886937409904, 14.09541550158063217, 3.795296366450317205 ) ) ;
#40362 = CARTESIAN_POINT ( 'NONE',  ( 0.1532563361054083140, 26.00893115100078745, 1.131784320476157264E-15 ) ) ;
#40364 = CARTESIAN_POINT ( 'NONE',  ( 20.36894250292379738, 24.92874883491396787, -10.36894250292379027 ) ) ;
#40365 = CARTESIAN_POINT ( 'NONE',  ( 0.1532563361054082862, 36.21726448433410894, 2.638427012816831674 ) ) ;
#40366 = CARTESIAN_POINT ( 'NONE',  ( 20.88017736071110519, 40.56368534415484106, 2.639326808657452039E-16 ) ) ;
#40367 = CARTESIAN_POINT ( 'NONE',  ( 4.559911319644449179, 18.89701867748817321, 9.422509992056141925 ) ) ;
#40368 = ADVANCED_FACE ( 'NONE', ( #80148 ), #59591, .F. ) ;
#40369 = CARTESIAN_POINT ( 'NONE',  ( 7.084665262690076126, 42.02201867748816966, -10.88017736071110164 ) ) ;
#40370 = CARTESIAN_POINT ( 'NONE',  ( 19.42250999205614193, 30.14701867748817321, 5.440088680355555262 ) ) ;
#40371 = ORIENTED_EDGE ( 'NONE', *, *, #13791, .F. ) ;
#40372 = CARTESIAN_POINT ( 'NONE',  ( 19.38216949554541202, 35.99863466993041072, 9.382169495545424454 ) ) ;
#40373 = CARTESIAN_POINT ( 'NONE',  ( 17.96484262340118221, 34.93868534415482685, 7.964842623401181321 ) ) ;
#40374 = EDGE_LOOP ( 'NONE', ( #9493, #92712, #63225, #59372 ) ) ;
#40375 = CARTESIAN_POINT ( 'NONE',  ( 16.40814093676323893, 55.79030133659708923, 11.09922568453595026 ) ) ;
#40376 = CARTESIAN_POINT ( 'NONE',  ( -0.8801773607110991993, 67.85535201082151957, -2.915334737309923874 ) ) ;
#40377 = AXIS2_PLACEMENT_3D ( 'NONE', #58899, #66393, #35404 ) ;
#40378 = EDGE_LOOP ( 'NONE', ( #92142, #67753, #68262, #47193 ) ) ;
#40379 = CARTESIAN_POINT ( 'NONE',  ( 4.559911319644449179, 57.23035201082150536, -9.422509992056141925 ) ) ;
#40380 = CARTESIAN_POINT ( 'NONE',  ( -0.8801773607110991993, 7.855352010821504471, -2.915334737309923874 ) ) ;
#40381 = CARTESIAN_POINT ( 'NONE',  ( 3.115783986955557694, 15.00000000000000000, -14.16128137375397955 ) ) ;
#40382 = CARTESIAN_POINT ( 'NONE',  ( -0.1503990784575328643, 69.92552686551195507, 6.262539305110068177 ) ) ;
#40383 = CARTESIAN_POINT ( 'NONE',  ( 13.79529636645031943, 65.34541550158063217, -14.16423886937409904 ) ) ;
#40384 = CARTESIAN_POINT ( 'NONE',  ( 1.472469842513823179, 11.42559781766745175, 4.923371831947296329 ) ) ;
#40385 = CARTESIAN_POINT ( 'NONE',  ( -2.266590686148945544, 11.38708216824730179, -7.082119434687050408 ) ) ;
#40386 = AXIS2_PLACEMENT_3D ( 'NONE', #35721, #41282, #87241 ) ;
#40387 = CARTESIAN_POINT ( 'NONE',  ( 14.92337183194729633, 2.675597817667451750, 8.527530157486181039 ) ) ;
#40388 = AXIS2_PLACEMENT_3D ( 'NONE', #74971, #12498, #80995 ) ;
#40389 = CARTESIAN_POINT ( 'NONE',  ( 12.91533473730992121, 9.522018677488171434, 10.88017736071110164 ) ) ;
#40390 = CARTESIAN_POINT ( 'NONE',  ( 19.84674366389459266, 43.30059781766744464, 2.638427012816836559 ) ) ;
#40391 = ORIENTED_EDGE ( 'NONE', *, *, #33254, .T. ) ;
#40392 = PRESENTATION_LAYER_ASSIGNMENT (  '', '', ( #5267 ) ) ;
#40393 = CARTESIAN_POINT ( 'NONE',  ( 14.92337183194729633, 52.67559781766745175, 8.527530157486181039 ) ) ;
#40394 = CARTESIAN_POINT ( 'NONE',  ( -14.49440716394874151, 15.00000000000000000, 0.4026921475165272657 ) ) ;
#40395 = AXIS2_PLACEMENT_3D ( 'NONE', #13759, #43261, #82745 ) ;
#40396 = CARTESIAN_POINT ( 'NONE',  ( 19.42250999205614548, 45.98035201082150536, -5.440088680355545492 ) ) ;
#40397 = CARTESIAN_POINT ( 'NONE',  ( 10.00000000000000178, 47.25893115100078745, 9.846743663894594434 ) ) ;
#40398 = CARTESIAN_POINT ( 'NONE',  ( -2.816281873526473856, 29.12363466993041783, 9.499525473075851096E-16 ) ) ;
#40400 = DIRECTION ( 'NONE',  ( 0.000000000000000000, 1.000000000000000000, -0.000000000000000000 ) ) ;
#40399 = CYLINDRICAL_SURFACE ( 'NONE', #25965, 1.500000000000001332 ) ;
#40401 = CARTESIAN_POINT ( 'NONE',  ( 17.96484262340118221, 49.93868534415484106, 7.964842623401181321 ) ) ;
#40402 = CARTESIAN_POINT ( 'NONE',  ( 19.42250999205614548, 5.980352010821504471, -5.440088680355545492 ) ) ;
#40403 = CARTESIAN_POINT ( 'NONE',  ( 10.00000000000000178, 35.37363466993042493, 12.81628187352647608 ) ) ;
#40404 = DIRECTION ( 'NONE',  ( 0.000000000000000000, 1.000000000000000000, 0.000000000000000000 ) ) ;
#40405 = VERTEX_POINT ( 'NONE', #19652 ) ;
#40406 = CARTESIAN_POINT ( 'NONE',  ( -2.816281873526471635, 33.91530133659708213, -3.434112377981056508 ) ) ;
#40407 = CARTESIAN_POINT ( 'NONE',  ( 0.5774900079438590739, 37.64701867748817676, -5.440088680355550821 ) ) ;
#40408 = ORIENTED_EDGE ( 'NONE', *, *, #27082, .T. ) ;
#40409 = MECHANICAL_DESIGN_GEOMETRIC_PRESENTATION_REPRESENTATION (  '', ( #61161 ), #30822 ) ;
#40410 = PLANE ( 'NONE',  #35648 ) ;
#40411 = CARTESIAN_POINT ( 'NONE',  ( 1.472469842513823179, 50.59226448433411605, -4.923371831947296329 ) ) ;
#40413 = CARTESIAN_POINT ( 'NONE',  ( 1.472469842513823179, 35.59226448433412315, -4.923371831947296329 ) ) ;
#40412 = CARTESIAN_POINT ( 'NONE',  ( 17.20831665107776587, 19.13393115100078035, -7.208316651077762316 ) ) ;
#40414 = CARTESIAN_POINT ( 'NONE',  ( -11.60534915929947708, -82.02544043777214711, 3.750000000000000444 ) ) ;
#40415 = CARTESIAN_POINT ( 'NONE',  ( 18.52753015748618282, 28.92559781766745175, -4.923371831947291888 ) ) ;
#40416 = DIRECTION ( 'NONE',  ( 8.881784197001252323E-16, 0.000000000000000000, 1.000000000000000000 ) ) ;
#40417 = DIRECTION ( 'NONE',  ( -0.000000000000000000, 1.000000000000000000, 0.000000000000000000 ) ) ;
#40418 = AXIS2_PLACEMENT_3D ( 'NONE', #48665, #86680, #33652 ) ;
#40419 = EDGE_CURVE ( 'NONE', #58682, #91405, #57954, .T. ) ;
#40421 = CARTESIAN_POINT ( 'NONE',  ( 12.63842701281683034, 2.467264484334118269, 9.846743663894596210 ) ) ;
#40420 = CARTESIAN_POINT ( 'NONE',  ( 5.076628168052703671, 26.84226448433411960, 8.527530157486179263 ) ) ;
#40422 = CARTESIAN_POINT ( 'NONE',  ( 0.000000000000000000, 14.49999999999999822, 0.000000000000000000 ) ) ;
#40424 = VERTEX_POINT ( 'NONE', #87648 ) ;
#40423 = CARTESIAN_POINT ( 'NONE',  ( 18.52753015748617571, 48.09226448433412315, 4.923371831947298993 ) ) ;
#40425 = FILL_AREA_STYLE ('',( #26379 ) ) ;
#40426 = CARTESIAN_POINT ( 'NONE',  ( 10.00000000000000178, 25.37363466993041783, 12.81628187352647608 ) ) ;
#40427 = CARTESIAN_POINT ( 'NONE',  ( -1.847237859018534323, 14.95037103927854538, -14.63711110085123757 ) ) ;
#40428 = CARTESIAN_POINT ( 'NONE',  ( 24.16423886937410614, 44.51208216824730357, -3.795296366450302550 ) ) ;
#40429 = CARTESIAN_POINT ( 'NONE',  ( 7.361572987183170547, 17.05059781766745530, 9.846743663894590881 ) ) ;
#40430 = DIRECTION ( 'NONE',  ( 0.000000000000000000, 0.000000000000000000, 1.000000000000000000 ) ) ;
#40431 = DIRECTION ( 'NONE',  ( 2.569960705150826877E-16, -1.000000000000000000, -0.000000000000000000 ) ) ;
#40432 = CARTESIAN_POINT ( 'NONE',  ( 24.16423886937410614, 39.51208216824731068, -3.795296366450302550 ) ) ;
#40433 = CARTESIAN_POINT ( 'NONE',  ( 0.1532563361054083140, 66.00893115100079456, 1.131784320476157264E-15 ) ) ;
#40434 = CARTESIAN_POINT ( 'NONE',  ( -0.8801773607110991993, 7.855352010821506248, -2.915334737309923874 ) ) ;
#40435 = CARTESIAN_POINT ( 'NONE',  ( 22.26659068614895176, 24.72041550158063572, -7.082119434687042414 ) ) ;
#40436 = CARTESIAN_POINT ( 'NONE',  ( -4.164238869374099039, 36.80374883491396787, 8.674139862899312516E-16 ) ) ;
#40437 = CARTESIAN_POINT ( 'NONE',  ( 12.60589901313228189, 14.49999999999999112, -8.129656208642064286 ) ) ;
#40439 = CARTESIAN_POINT ( 'NONE',  ( 10.00000000000000000, 49.75893115100078745, -9.846743663894594434 ) ) ;
#40438 = CARTESIAN_POINT ( 'NONE',  ( -3.420591144908647241, 0.5000000000000004441, 14.60477854057953451 ) ) ;
#40440 = CARTESIAN_POINT ( 'NONE',  ( 19.42250999205614548, 35.98035201082151247, -5.440088680355545492 ) ) ;
#40441 = DIRECTION ( 'NONE',  ( 0.000000000000000000, 0.000000000000000000, 1.000000000000000000 ) ) ;
#40442 = CARTESIAN_POINT ( 'NONE',  ( 19.54746220608152640, 97.02070453147715057, -5.000000000000000000 ) ) ;
#40443 = CARTESIAN_POINT ( 'NONE',  ( 0.1532563361054100626, 35.80059781766745175, -2.638427012816831230 ) ) ;
#40444 = CARTESIAN_POINT ( 'NONE',  ( 13.75801628063878645, 15.00000000000000000, 4.578972376164554881 ) ) ;
#40445 = CARTESIAN_POINT ( 'NONE',  ( -12.26659068614894110, -2.779584498419355842, 7.082119434687058401 ) ) ;
#40446 = CARTESIAN_POINT ( 'NONE',  ( 7.361572987183169658, 39.96726448433411605, -9.846743663894592657 ) ) ;
#40447 = CARTESIAN_POINT ( 'NONE',  ( 19.84674366389459266, 63.71726448433412315, -2.638427012816827677 ) ) ;
#40448 = ADVANCED_FACE ( 'NONE', ( #80653 ), #80370, .T. ) ;
#40449 = VERTEX_POINT ( 'NONE', #72636 ) ;
#40450 = CARTESIAN_POINT ( 'NONE',  ( 6.204703633549690345, 12.84541550158063572, 14.16423886937410082 ) ) ;
#40451 = CARTESIAN_POINT ( 'NONE',  ( -12.79413655343686784, 14.76984915707685531, -7.715718893783058974 ) ) ;
#40453 = CARTESIAN_POINT ( 'NONE',  ( 20.88017736071110164, 45.35535201082149825, 2.915334737309930979 ) ) ;
#40452 = CARTESIAN_POINT ( 'NONE',  ( -4.010449548136814535, -13.83555390988818523, -2.500000000000000888 ) ) ;
#40454 = CARTESIAN_POINT ( 'NONE',  ( 7.084665262690076126, 2.022018677488171434, -10.88017736071110164 ) ) ;
#40455 = CARTESIAN_POINT ( 'NONE',  ( 21.09922568453595559, 22.04030133659708923, -6.408140936763230044 ) ) ;
#40456 = EDGE_CURVE ( 'NONE', #53389, #33104, #43135, .T. ) ;
#40457 =( NAMED_UNIT ( * ) PLANE_ANGLE_UNIT ( ) SI_UNIT ( $, .RADIAN. ) );
#40458 = CARTESIAN_POINT ( 'NONE',  ( 5.076628168052704559, 0.1755978176674514724, -8.527530157486179263 ) ) ;
#40459 = CARTESIAN_POINT ( 'NONE',  ( 4.630000001262032150, 0.09071174558778491437, -4.000000000000000000 ) ) ;
#40460 = SURFACE_STYLE_USAGE ( .BOTH. , #47934 ) ;
#40461 = CARTESIAN_POINT ( 'NONE',  ( 14.26295192185810201, 0.04922511925148844586, 3.770186020345128952 ) ) ;
#40462 = CARTESIAN_POINT ( 'NONE',  ( 4.559911319644449179, 7.230352010821505360, -9.422509992056141925 ) ) ;
#40463 = LINE ( 'NONE', #1982, #38393 ) ;
#40464 = CARTESIAN_POINT ( 'NONE',  ( -0.8801773607111009756, 23.06368534415484106, 1.068504757029289695E-15 ) ) ;
#40466 = AXIS2_PLACEMENT_3D ( 'NONE', #65342, #57358, #74322 ) ;
#40465 = CARTESIAN_POINT ( 'NONE',  ( -0.8801773607111008646, 38.27201867748816255, 2.915334737309923430 ) ) ;
#40467 = CARTESIAN_POINT ( 'NONE',  ( 1.472469842513823179, 65.59226448433412315, -4.923371831947296329 ) ) ;
#40468 = CARTESIAN_POINT ( 'NONE',  ( 0.1532563361054083140, 56.00893115100078745, 1.131784320476157264E-15 ) ) ;
#40469 = CARTESIAN_POINT ( 'NONE',  ( -44.44142132516394383, 105.4794309841216347, -5.302661541405906398 ) ) ;
#40470 = CARTESIAN_POINT ( 'NONE',  ( 0.1532563361054082862, 11.21726448433411605, 2.638427012816831674 ) ) ;
#40471 = ORIENTED_EDGE ( 'NONE', *, *, #97594, .F. ) ;
#40472 = CARTESIAN_POINT ( 'NONE',  ( 19.42250999205614193, 35.14701867748816966, 5.440088680355555262 ) ) ;
#40473 = CARTESIAN_POINT ( 'NONE',  ( 3.591859063236763294, 33.29030133659708213, -11.09922568453595026 ) ) ;
#40474 = CARTESIAN_POINT ( 'NONE',  ( 18.00000000000001776, 4.625929269271493211E-15, 3.750000000000000000 ) ) ;
#40475 = UNCERTAINTY_MEASURE_WITH_UNIT (LENGTH_MEASURE( 1.000000000000000082E-05 ), #19141, 'distance_accuracy_value', 'NONE');
#40476 = CARTESIAN_POINT ( 'NONE',  ( 2.791683348922237240, 60.38393115100078745, -7.208316651077763204 ) ) ;
#40477 = CARTESIAN_POINT ( 'NONE',  ( -0.8801773607111009756, 53.06368534415484106, 1.068504757029289695E-15 ) ) ;
#40478 = CARTESIAN_POINT ( 'NONE',  ( 19.84674366389459266, 13.30059781766745353, 2.638427012816836559 ) ) ;
#40479 = CARTESIAN_POINT ( 'NONE',  ( 22.81628187352647785, 41.41530133659708923, 3.434112377981063169 ) ) ;
#40481 = CARTESIAN_POINT ( 'NONE',  ( -5.806616290881239095, 15.00000000000000533, -13.42355087257370272 ) ) ;
#40480 = CARTESIAN_POINT ( 'NONE',  ( -0.8801773607111008646, 58.27201867748816966, 2.915334737309923430 ) ) ;
#40482 = LINE ( 'NONE', #8498, #308 ) ;
#40483 = ORIENTED_EDGE ( 'NONE', *, *, #79080, .T. ) ;
#40484 = DIRECTION ( 'NONE',  ( 1.049065152435176504E-16, -1.000000000000000000, 0.000000000000000000 ) ) ;
#40485 = CARTESIAN_POINT ( 'NONE',  ( 4.559911319644449179, 2.230352010821504471, -9.422509992056141925 ) ) ;
#40487 = CARTESIAN_POINT ( 'NONE',  ( -4.164238869374098151, 11.59541550158063217, -3.795296366450310543 ) ) ;
#40486 = CARTESIAN_POINT ( 'NONE',  ( 21.09922568453594849, 46.20696800326376064, 6.408140936763242479 ) ) ;
#40488 = CARTESIAN_POINT ( 'NONE',  ( 7.361572987183170547, 12.05059781766744997, 9.846743663894590881 ) ) ;
#40489 =( LENGTH_UNIT ( ) NAMED_UNIT ( * ) SI_UNIT ( .MILLI., .METRE. ) );
#40490 = CARTESIAN_POINT ( 'NONE',  ( 14.92337183194729633, 17.67559781766745175, 8.527530157486181039 ) ) ;
#40491 = CARTESIAN_POINT ( 'NONE',  ( 17.08211943468705840, 60.13708216824729647, -12.26659068614894466 ) ) ;
#40492 = ORIENTED_EDGE ( 'NONE', *, *, #37056, .T. ) ;
#40493 = CARTESIAN_POINT ( 'NONE',  ( 19.42250999205614193, 5.147018677488171434, 5.440088680355555262 ) ) ;
#40494 = STYLED_ITEM ( 'NONE', ( #69711 ), #40089 ) ;
#40495 = EDGE_CURVE ( 'NONE', #79187, #40528, #56398, .T. ) ;
#40496 = CARTESIAN_POINT ( 'NONE',  ( 20.88017736071110875, 15.77201867748817143, -2.915334737309920765 ) ) ;
#40497 = CARTESIAN_POINT ( 'NONE',  ( 3.840373378095567336, 13.17686044187654559, -11.29165764256138260 ) ) ;
#40498 = ORIENTED_EDGE ( 'NONE', *, *, #42578, .F. ) ;
#40499 = VERTEX_POINT ( 'NONE', #65632 ) ;
#40500 = CIRCLE ( 'NONE', #19711, 0.2500000000000002220 ) ;
#40501 = CARTESIAN_POINT ( 'NONE',  ( 15.44008868035555793, 11.39701867748817143, -9.422509992056140149 ) ) ;
#40502 = CARTESIAN_POINT ( 'NONE',  ( 17.20831665107776587, 52.88393115100078035, 7.208316651077764980 ) ) ;
#40503 = CARTESIAN_POINT ( 'NONE',  ( 1.274849032794292736, 67.55509018479936856, -6.499999999999977796 ) ) ;
#40505 = CARTESIAN_POINT ( 'NONE',  ( 24.16423886937409904, 19.09541550158063927, 3.795296366450317205 ) ) ;
#40504 = FACE_OUTER_BOUND ( 'NONE', #9768, .T. ) ;
#40506 = CARTESIAN_POINT ( 'NONE',  ( 10.00000000000000000, 41.81368534415484106, -10.88017736071110342 ) ) ;
#40507 = CARTESIAN_POINT ( 'NONE',  ( 20.88017736071110875, 20.77201867748816611, -2.915334737309920765 ) ) ;
#40508 = CARTESIAN_POINT ( 'NONE',  ( 0.1532563361054083140, 56.00893115100078745, 1.131784320476157264E-15 ) ) ;
#40509 = CARTESIAN_POINT ( 'NONE',  ( -8.469613711665671119, -9.365740742666716301, -3.750000000000000444 ) ) ;
#40510 = CARTESIAN_POINT ( 'NONE',  ( 2.791683348922237240, 30.38393115100078390, -7.208316651077763204 ) ) ;
#40511 = DIRECTION ( 'NONE',  ( -5.818595309480553908E-17, -1.000000000000000000, -0.000000000000000000 ) ) ;
#40512 = CARTESIAN_POINT ( 'NONE',  ( 2.791683348922240793, 1.633931151000784565, 7.208316651077764092 ) ) ;
#40513 = CARTESIAN_POINT ( 'NONE',  ( 4.923371831947301658, 27.67559781766745886, 8.527530157486175710 ) ) ;
#40514 = VERTEX_POINT ( 'NONE', #66636 ) ;
#40515 = CARTESIAN_POINT ( 'NONE',  ( 5.795997163830165277, -0.03417435944610275333, -13.01802277140705932 ) ) ;
#40516 = CARTESIAN_POINT ( 'NONE',  ( 5.076628168052703671, 16.84226448433411960, 8.527530157486179263 ) ) ;
#40517 = CARTESIAN_POINT ( 'NONE',  ( 6.565887622018943937, 5.165301336597086568, 12.81628187352647430 ) ) ;
#40518 = CARTESIAN_POINT ( 'NONE',  ( 12.91533473730993009, 51.60535201082149825, -10.88017736071109987 ) ) ;
#40520 = CARTESIAN_POINT ( 'NONE',  ( -2.816281873526473856, 49.12363466993042493, 9.499525473075851096E-16 ) ) ;
#40519 = CARTESIAN_POINT ( 'NONE',  ( -0.8801773607111008646, 8.272018677488171434, 2.915334737309923430 ) ) ;
#40521 = CARTESIAN_POINT ( 'NONE',  ( 6.204703633549690345, 20.76208216824730357, -14.16423886937410259 ) ) ;
#40522 =( GEOMETRIC_REPRESENTATION_CONTEXT ( 3 ) GLOBAL_UNCERTAINTY_ASSIGNED_CONTEXT ( ( #57495 ) ) GLOBAL_UNIT_ASSIGNED_CONTEXT ( ( #94795, #87780, #3815 ) ) REPRESENTATION_CONTEXT ( 'NONE', 'WORKASPACE' ) );
#40523 = CARTESIAN_POINT ( 'NONE',  ( 10.00000000000000000, 62.87363466993042493, -12.81628187352647608 ) ) ;
#40524 = VERTEX_POINT ( 'NONE', #64635 ) ;
#40525 = CARTESIAN_POINT ( 'NONE',  ( 14.92337183194729988, 54.34226448433412315, -8.527530157486177487 ) ) ;
#40526 = CARTESIAN_POINT ( 'NONE',  ( 7.084665262690076126, 24.10535201082150181, 10.88017736071109987 ) ) ;
#40527 = TOROIDAL_SURFACE ( 'NONE', #72401, 14.49999999999999822, 0.5000000000000000000 ) ;
#40528 = VERTEX_POINT ( 'NONE', #4169 ) ;
#40529 = CARTESIAN_POINT ( 'NONE',  ( 19.84674366389459266, 3.717264484334118713, -2.638427012816827677 ) ) ;
#40530 = CARTESIAN_POINT ( 'NONE',  ( 10.69820648722788015, 1.823139558123380688, 5.272416709312279792 ) ) ;
#40531 = CARTESIAN_POINT ( 'NONE',  ( 5.076628168052704559, 10.17559781766745175, -8.527530157486179263 ) ) ;
#40532 = CARTESIAN_POINT ( 'NONE',  ( 10.00000000000000178, 69.31368534415484817, 10.88017736071110342 ) ) ;
#40533 = CARTESIAN_POINT ( 'NONE',  ( -9.997910040112461871, 4.266261872180168263E-16, -10.50199004140731773 ) ) ;
#40534 = EDGE_CURVE ( 'NONE', #10816, #87399, #93139, .T. ) ;
#40536 = DIRECTION ( 'NONE',  ( 0.000000000000000000, 0.000000000000000000, 1.000000000000000000 ) ) ;
#40535 = CARTESIAN_POINT ( 'NONE',  ( 17.96484262340118221, 54.93868534415484106, 7.964842623401181321 ) ) ;
#40537 = CARTESIAN_POINT ( 'NONE',  ( 2.035157376598824452, 58.68868534415482685, 7.964842623401179544 ) ) ;
#40539 = ORIENTED_EDGE ( 'NONE', *, *, #60292, .F. ) ;
#40538 = CARTESIAN_POINT ( 'NONE',  ( 0.1532563361054083140, 1.008931151000784787, 1.131784320476157264E-15 ) ) ;
#40540 = CARTESIAN_POINT ( 'NONE',  ( 0.2751277870542986892, 7.282175860852375671, -6.500000000000003553 ) ) ;
#40541 = CARTESIAN_POINT ( 'NONE',  ( 1.472469842513823179, 50.59226448433411605, -4.923371831947296329 ) ) ;
#40542 = ORIENTED_EDGE ( 'NONE', *, *, #65751, .F. ) ;
#40543 = VERTEX_POINT ( 'NONE', #50646 ) ;
#40544 = CARTESIAN_POINT ( 'NONE',  ( 24.16423886937410614, 4.303748834913967869, 8.672049930838204340E-16 ) ) ;
#40545 = CARTESIAN_POINT ( 'NONE',  ( 22.81628187352647785, 56.41530133659708213, 3.434112377981063169 ) ) ;
#40546 = CARTESIAN_POINT ( 'NONE',  ( 22.26659068614895176, 4.720415501580633943, -7.082119434687042414 ) ) ;
#40547 = CARTESIAN_POINT ( 'NONE',  ( 24.16423886937409904, 24.09541550158063927, 3.795296366450317205 ) ) ;
#40548 = CARTESIAN_POINT ( 'NONE',  ( 10.00000000000000178, 3.053748834913967425, 14.16423886937410082 ) ) ;
#40549 = CARTESIAN_POINT ( 'NONE',  ( 20.88017736071110519, 25.56368534415483751, 2.639326808657452039E-16 ) ) ;
#40550 = DIRECTION ( 'NONE',  ( 0.000000000000000000, 1.000000000000000000, 0.000000000000000000 ) ) ;
#40551 = ORIENTED_EDGE ( 'NONE', *, *, #1167, .F. ) ;
#40552 = CARTESIAN_POINT ( 'NONE',  ( 1.472469842513823179, 5.592264484334118713, -4.923371831947296329 ) ) ;
#40553 = CARTESIAN_POINT ( 'NONE',  ( 2.791683348922237240, 10.38393115100078390, -7.208316651077763204 ) ) ;
#40554 = CARTESIAN_POINT ( 'NONE',  ( 19.38216949554541202, 30.99863466993042138, 9.382169495545424454 ) ) ;
#40555 = CARTESIAN_POINT ( 'NONE',  ( 19.84674366389459266, 43.71726448433410894, -2.638427012816827677 ) ) ;
#40556 = DIRECTION ( 'NONE',  ( 0.000000000000000000, -0.000000000000000000, -1.000000000000000000 ) ) ;
#40557 = CARTESIAN_POINT ( 'NONE',  ( -2.816281873526473856, 24.33196800326375353, 3.434112377981055619 ) ) ;
#40558 = CARTESIAN_POINT ( 'NONE',  ( 8.979999999999991545, 27.03929484861771826, -3.000000000000000000 ) ) ;
#40559 = CARTESIAN_POINT ( 'NONE',  ( 19.84674366389459266, 23.30059781766745530, 2.638427012816836559 ) ) ;
#40560 = CARTESIAN_POINT ( 'NONE',  ( 24.16423886937409904, 19.09541550158063927, 3.795296366450317205 ) ) ;
#40561 = EDGE_CURVE ( 'NONE', #94977, #77859, #23550, .T. ) ;
#40562 = ORIENTED_EDGE ( 'NONE', *, *, #25859, .T. ) ;
#40563 = B_SPLINE_CURVE_WITH_KNOTS ( 'NONE', 3,
 ( #81867, #27390, #80896, #58368, #34391, #49896 ),
 .UNSPECIFIED., .F., .F.,
 ( 4, 2, 4 ),
 ( 3.409110551494655498E-05, 0.0004400426677367912337, 0.0008459942299586359869 ),
 .UNSPECIFIED. ) ;
#40564 = CARTESIAN_POINT ( 'NONE',  ( 15.44008868035555793, 31.39701867748817676, -9.422509992056140149 ) ) ;
#40565 = CARTESIAN_POINT ( 'NONE',  ( 13.79529636645031943, 30.34541550158063927, -14.16423886937409904 ) ) ;
#40566 = CARTESIAN_POINT ( 'NONE',  ( 0.1532563361054083140, 51.00893115100078745, 1.131784320476157264E-15 ) ) ;
#40567 = CARTESIAN_POINT ( 'NONE',  ( 2.791683348922237240, 15.38393115100078212, -7.208316651077763204 ) ) ;
#40569 = CARTESIAN_POINT ( 'NONE',  ( -7.804338076140435732, 84.96756567522902515, 4.038273117401847578 ) ) ;
#40568 = CARTESIAN_POINT ( 'NONE',  ( -2.816281873526471635, 48.91530133659708213, -3.434112377981056508 ) ) ;
#40570 = CARTESIAN_POINT ( 'NONE',  ( 10.00000000000000000, 26.81368534415484106, -10.88017736071110342 ) ) ;
#40571 = EDGE_CURVE ( 'NONE', #51581, #78512, #5151, .T. ) ;
#40572 = LINE ( 'NONE', #2100, #50203 ) ;
#40573 = CARTESIAN_POINT ( 'NONE',  ( -2.816281873526473856, 19.33196800326375708, 3.434112377981055619 ) ) ;
#40574 = CARTESIAN_POINT ( 'NONE',  ( 19.38216949554541202, 20.99863466993042138, 9.382169495545424454 ) ) ;
#40575 = CARTESIAN_POINT ( 'NONE',  ( 19.84674366389459266, 43.71726448433410894, -2.638427012816827677 ) ) ;
#40576 = CARTESIAN_POINT ( 'NONE',  ( -5.440088680355558814, 2.230352010821508468, -9.422509992056136596 ) ) ;
#40577 = CARTESIAN_POINT ( 'NONE',  ( 0.6178305044545838731, 44.74863466993042493, 9.382169495545420901 ) ) ;
#40578 = FACE_OUTER_BOUND ( 'NONE', #66407, .T. ) ;
#40580 = CARTESIAN_POINT ( 'NONE',  ( 19.89220837332774749, 9.740628644642393752, 6.478736007405950126 ) ) ;
#40579 = CARTESIAN_POINT ( 'NONE',  ( -0.8801773607110991993, 47.85535201082150536, -2.915334737309923874 ) ) ;
#40581 = CARTESIAN_POINT ( 'NONE',  ( -9.543970587329795308, -28.01866822101010612, 3.999999999999999112 ) ) ;
#40582 = LINE ( 'NONE', #72046, #67203 ) ;
#40583 = CARTESIAN_POINT ( 'NONE',  ( 4.559911319644449179, 58.89701867748817676, 9.422509992056141925 ) ) ;
#40584 = CARTESIAN_POINT ( 'NONE',  ( 17.96484262340118221, 56.18868534415484817, -7.964842623401177768 ) ) ;
#40585 = DIRECTION ( 'NONE',  ( 0.000000000000000000, 0.000000000000000000, 1.000000000000000000 ) ) ;
#40586 = CARTESIAN_POINT ( 'NONE',  ( 8.731067818237031375, 12.81330936912750929, -8.731067818237036704 ) ) ;
#40587 = PRESENTATION_LAYER_ASSIGNMENT (  '', '', ( #40649 ) ) ;
#40588 = CARTESIAN_POINT ( 'NONE',  ( 20.88017736071110519, 5.563685344154838397, 2.639326808657452039E-16 ) ) ;
#40589 = CARTESIAN_POINT ( 'NONE',  ( 0.6178305044545838731, -0.2513653300695798953, 9.382169495545420901 ) ) ;
#40591 = DIRECTION ( 'NONE',  ( 0.000000000000000000, 0.000000000000000000, 1.000000000000000000 ) ) ;
#40590 = CARTESIAN_POINT ( 'NONE',  ( 12.91533473730992121, 24.52201867748816966, 10.88017736071110164 ) ) ;
#40592 = CARTESIAN_POINT ( 'NONE',  ( 22.81628187352647785, 21.62363466993041783, 6.195893100308588602E-16 ) ) ;
#40593 = ORIENTED_EDGE ( 'NONE', *, *, #76902, .T. ) ;
#40594 = CARTESIAN_POINT ( 'NONE',  ( 4.559911319644449179, 47.23035201082150536, -9.422509992056141925 ) ) ;
#40595 = CARTESIAN_POINT ( 'NONE',  ( 5.076628168052704559, 35.17559781766745175, -8.527530157486179263 ) ) ;
#40597 = CARTESIAN_POINT ( 'NONE',  ( -12.50534872682737664, 4.247830340245585198E-16, 7.339363270777436554 ) ) ;
#40596 = CARTESIAN_POINT ( 'NONE',  ( 3.591859063236761518, 9.956968003263753531, 11.09922568453594849 ) ) ;
#40598 = CARTESIAN_POINT ( 'NONE',  ( 0.5774900079438607392, 23.48035201082150536, 5.440088680355550821 ) ) ;
#40599 = CARTESIAN_POINT ( 'NONE',  ( 17.96484262340118221, 39.93868534415484106, 7.964842623401181321 ) ) ;
#40600 = CARTESIAN_POINT ( 'NONE',  ( 6.204703633549690345, 52.84541550158062506, 14.16423886937410082 ) ) ;
#40601 = CARTESIAN_POINT ( 'NONE',  ( 14.92337183194729988, 34.34226448433411605, -8.527530157486177487 ) ) ;
#40602 = CARTESIAN_POINT ( 'NONE',  ( 15.44008868035555793, 61.39701867748817676, -9.422509992056140149 ) ) ;
#40603 = CARTESIAN_POINT ( 'NONE',  ( 13.30156849913886496, 14.76930270348881002, -6.804875469488061768 ) ) ;
#40604 = CARTESIAN_POINT ( 'NONE',  ( 10.00000000000000000, 15.55374883491396787, -14.16423886937410082 ) ) ;
#40605 = EDGE_CURVE ( 'NONE', #21360, #45156, #65136, .T. ) ;
#40606 = DIRECTION ( 'NONE',  ( -0.02177529129959714441, -0.9997628902338883128, 0.000000000000000000 ) ) ;
#40607 = FACE_OUTER_BOUND ( 'NONE', #71151, .T. ) ;
#40608 = ORIENTED_EDGE ( 'NONE', *, *, #33056, .T. ) ;
#40609 = EDGE_LOOP ( 'NONE', ( #47739, #10701, #71314, #90062, #1073, #91666 ) ) ;
#40610 = CARTESIAN_POINT ( 'NONE',  ( 20.36894250292379738, 54.92874883491396076, -10.36894250292379027 ) ) ;
#40611 = CARTESIAN_POINT ( 'NONE',  ( 13.79529636645031943, 35.34541550158063927, -14.16423886937409904 ) ) ;
#40612 = CARTESIAN_POINT ( 'NONE',  ( 5.076628168052703671, 21.84226448433411960, 8.527530157486179263 ) ) ;
#40613 = CARTESIAN_POINT ( 'NONE',  ( 0.1532563361054083140, 61.00893115100078745, 1.131784320476157264E-15 ) ) ;
#40614 = CYLINDRICAL_SURFACE ( 'NONE', #83420, 0.5000000000000004441 ) ;
#40616 = CARTESIAN_POINT ( 'NONE',  ( -2.816281873526471635, 28.91530133659708213, -3.434112377981056508 ) ) ;
#40615 = CARTESIAN_POINT ( 'NONE',  ( 0.5774900079438607392, 53.48035201082151247, 5.440088680355550821 ) ) ;
#40617 = CARTESIAN_POINT ( 'NONE',  ( -2.266590686148945544, 41.38708216824729647, -7.082119434687050408 ) ) ;
#40618 = CARTESIAN_POINT ( 'NONE',  ( 20.88017736071110519, 25.56368534415483751, 2.639326808657452039E-16 ) ) ;
#40619 = CARTESIAN_POINT ( 'NONE',  ( 12.60589901313221439, 0.5000000000000004441, -8.129656208642048298 ) ) ;
#40620 = CARTESIAN_POINT ( 'NONE',  ( 4.559911319644449179, 63.89701867748817676, 9.422509992056141925 ) ) ;
#40621 = EDGE_CURVE ( 'NONE', #19964, #46091, #13281, .T. ) ;
#40622 = CARTESIAN_POINT ( 'NONE',  ( 7.208316651077764980, -7.116068848999210772, 7.208316651077762316 ) ) ;
#40623 = CARTESIAN_POINT ( 'NONE',  ( 7.361572987183170547, 7.050597817667451750, 9.846743663894590881 ) ) ;
#40624 = EDGE_LOOP ( 'NONE', ( #49673, #9060, #27507, #82572 ) ) ;
#40625 = CARTESIAN_POINT ( 'NONE',  ( -2.962741594153171842, 15.00000000000000000, 13.93860331045670975 ) ) ;
#40626 = ORIENTED_EDGE ( 'NONE', *, *, #55843, .T. ) ;
#40627 = DIRECTION ( 'NONE',  ( 0.2503800040544389427, 0.000000000000000000, 0.9681476403781082984 ) ) ;
#40628 = ORIENTED_EDGE ( 'NONE', *, *, #40896, .F. ) ;
#40630 = CARTESIAN_POINT ( 'NONE',  ( 0.5774900079438590739, 12.64701867748817321, -5.440088680355550821 ) ) ;
#40629 = CARTESIAN_POINT ( 'NONE',  ( 17.96484262340118221, 9.938685344154839285, 7.964842623401181321 ) ) ;
#40632 = CARTESIAN_POINT ( 'NONE',  ( 13.43411237798106583, 7.665301336597086568, -12.81628187352647252 ) ) ;
#40631 = CARTESIAN_POINT ( 'NONE',  ( 1.472469842513823179, 35.59226448433412315, -4.923371831947296329 ) ) ;
#40633 = CARTESIAN_POINT ( 'NONE',  ( -13.61464873478159454, 14.63595249122789177, -6.296136897218026718 ) ) ;
#40634 = CIRCLE ( 'NONE', #69603, 3.000000000000002665 ) ;
#40635 = LINE ( 'NONE', #87101, #73339 ) ;
#40636 = CARTESIAN_POINT ( 'NONE',  ( 0.6178305044545818747, 13.49863466993041783, -9.382169495545419124 ) ) ;
#40637 = ORIENTED_EDGE ( 'NONE', *, *, #25771, .T. ) ;
#40638 = CARTESIAN_POINT ( 'NONE',  ( 2.917880565312948704, 52.63708216824730357, 12.26659068614894643 ) ) ;
#40639 = VERTEX_POINT ( 'NONE', #43630 ) ;
#40640 = CARTESIAN_POINT ( 'NONE',  ( -0.3689425029237881626, 52.42874883491396076, 10.36894250292379027 ) ) ;
#40641 = ORIENTED_EDGE ( 'NONE', *, *, #32120, .F. ) ;
#40642 = CARTESIAN_POINT ( 'NONE',  ( 10.00000000000000178, 34.31368534415484106, 10.88017736071110342 ) ) ;
#40643 = CARTESIAN_POINT ( 'NONE',  ( 10.00000000000000178, 39.31368534415484106, 10.88017736071110342 ) ) ;
#40644 = CARTESIAN_POINT ( 'NONE',  ( 2.035157376598824452, 38.68868534415483396, 7.964842623401179544 ) ) ;
#40645 = CARTESIAN_POINT ( 'NONE',  ( -0.8801773607111009756, 63.06368534415484106, 1.068504757029289695E-15 ) ) ;
#40646 = CARTESIAN_POINT ( 'NONE',  ( 0.5774900079438590739, 27.64701867748817676, -5.440088680355550821 ) ) ;
#40647 = EDGE_CURVE ( 'NONE', #10095, #93630, #47347, .T. ) ;
#40648 = LINE ( 'NONE', #64103, #45650 ) ;
#40649 = STYLED_ITEM ( 'NONE', ( #56878 ), #98724 ) ;
#40650 = CARTESIAN_POINT ( 'NONE',  ( 10.00000000000000178, 12.25893115100078568, 9.846743663894594434 ) ) ;
#40651 = CARTESIAN_POINT ( 'NONE',  ( -5.079065453169564037, -28.67168118942975497, 2.500000000000000888 ) ) ;
#40652 = ORIENTED_EDGE ( 'NONE', *, *, #48337, .F. ) ;
#40653 = EDGE_CURVE ( 'NONE', #37189, #51203, #69181, .T. ) ;
#40654 = SURFACE_STYLE_USAGE ( .BOTH. , #9662 ) ;
#40655 = CARTESIAN_POINT ( 'NONE',  ( 5.076628168052703671, 41.84226448433411605, 8.527530157486179263 ) ) ;
#40656 = ADVANCED_FACE ( 'NONE', ( #91481 ), #45480, .T. ) ;
#40657 = CIRCLE ( 'NONE', #24751, 0.2500000000000002220 ) ;
#40658 = CARTESIAN_POINT ( 'NONE',  ( 64.56412365047461321, 29.00000000000000355, 7.000000000000000000 ) ) ;
#40659 = CARTESIAN_POINT ( 'NONE',  ( -3.635384400432159158, -3.854802480546752896, 2.750000000000000000 ) ) ;
#40660 = LINE ( 'NONE', #56157, #93884 ) ;
#40661 = CARTESIAN_POINT ( 'NONE',  ( -2.815433093577223378, 15.00000000000000000, 14.73340885523747978 ) ) ;
#40662 = CARTESIAN_POINT ( 'NONE',  ( 19.84674366389459621, 48.50893115100078745, 7.409399052514197653E-17 ) ) ;
#40663 = CARTESIAN_POINT ( 'NONE',  ( 6.204703633549690345, 42.84541550158063217, 14.16423886937410082 ) ) ;
#40664 = CARTESIAN_POINT ( 'NONE',  ( -22.44000000000001194, 93.50000000000000000, -10.09898361729590199 ) ) ;
#40665 = VERTEX_POINT ( 'NONE', #76476 ) ;
#40666 = CARTESIAN_POINT ( 'NONE',  ( -7.684764310694718326, 14.49999999999999112, -12.88194075009952222 ) ) ;
#40667 = CARTESIAN_POINT ( 'NONE',  ( 10.00000000000000178, 22.25893115100078745, 9.846743663894594434 ) ) ;
#40668 = ADVANCED_FACE ( 'NONE', ( #83492 ), #50035, .T. ) ;
#40669 = CARTESIAN_POINT ( 'NONE',  ( 0.6178305044545838731, 64.74863466993043914, 9.382169495545420901 ) ) ;
#40670 = CARTESIAN_POINT ( 'NONE',  ( 0.1532563361054082862, 56.21726448433411605, 2.638427012816831674 ) ) ;
#40671 = CARTESIAN_POINT ( 'NONE',  ( 17.96484262340118221, 66.18868534415483396, -7.964842623401177768 ) ) ;
#40672 = CARTESIAN_POINT ( 'NONE',  ( 0.1532563361054100626, 45.80059781766745886, -2.638427012816831230 ) ) ;
#40673 = CARTESIAN_POINT ( 'NONE',  ( 4.573260519721095818, -6.401749983321133541, -2.750000000000000000 ) ) ;
#40674 = EDGE_LOOP ( 'NONE', ( #42479, #58820, #25025, #34596, #28286, #40265 ) ) ;
#40675 = CARTESIAN_POINT ( 'NONE',  ( -4.164238869374099039, 61.80374883491397497, 8.674139862899312516E-16 ) ) ;
#40676 = CARTESIAN_POINT ( 'NONE',  ( 17.85999999999999588, 37.99999999999997868, 10.00000000000000000 ) ) ;
#40677 = CARTESIAN_POINT ( 'NONE',  ( 12.91533473730993009, 36.60535201082151247, -10.88017736071109987 ) ) ;
#40679 = CARTESIAN_POINT ( 'NONE',  ( 12.91533473730993009, 66.60535201082150536, -10.88017736071109987 ) ) ;
#40678 = CARTESIAN_POINT ( 'NONE',  ( 19.38216949554541202, 10.99863466993042138, 9.382169495545424454 ) ) ;
#40680 = CARTESIAN_POINT ( 'NONE',  ( -0.2418659066527703572, 63.09014588040356841, 6.114288769123046308 ) ) ;
#40681 = EDGE_CURVE ( 'NONE', #11914, #97132, #8474, .T. ) ;
#40682 = CARTESIAN_POINT ( 'NONE',  ( 19.89103541497709315, 45.66234555792569694, -6.479102184480826310 ) ) ;
#40683 = CARTESIAN_POINT ( 'NONE',  ( 0.000000000000000000, 0.5000000000000004441, 0.000000000000000000 ) ) ;
#40684 = CARTESIAN_POINT ( 'NONE',  ( 18.52753015748617571, 53.09226448433412315, 4.923371831947298993 ) ) ;
#40685 = CARTESIAN_POINT ( 'NONE',  ( 2.915334737309921209, -33.39464798917849464, -10.88017736071110164 ) ) ;
#40686 = CARTESIAN_POINT ( 'NONE',  ( 6.565887622018943937, 5.165301336597086568, 12.81628187352647430 ) ) ;
#40688 = DIRECTION ( 'NONE',  ( 0.000000000000000000, 1.000000000000000000, -0.000000000000000000 ) ) ;
#40687 = CARTESIAN_POINT ( 'NONE',  ( -0.8801773607111009756, 18.06368534415484106, 1.068504757029289695E-15 ) ) ;
#40689 = DIRECTION ( 'NONE',  ( 0.000000000000000000, 0.000000000000000000, -1.000000000000000000 ) ) ;
#40690 = AXIS2_PLACEMENT_3D ( 'NONE', #2658, #33110, #24649 ) ;
#40691 = CARTESIAN_POINT ( 'NONE',  ( 20.36894250292379738, 29.92874883491396432, -10.36894250292379027 ) ) ;
#40692 = CARTESIAN_POINT ( 'NONE',  ( -2.266590686148945544, 31.38708216824730002, -7.082119434687050408 ) ) ;
#40693 = CARTESIAN_POINT ( 'NONE',  ( 6.204703633549690345, 57.84541550158063927, 14.16423886937410082 ) ) ;
#40694 = CARTESIAN_POINT ( 'NONE',  ( 16.40814093676324603, 42.45696800326375353, -11.09922568453594671 ) ) ;
#40695 = CARTESIAN_POINT ( 'NONE',  ( 4.559911319644449179, 17.23035201082150536, -9.422509992056141925 ) ) ;
#40696 = ORIENTED_EDGE ( 'NONE', *, *, #49054, .F. ) ;
#40697 = CARTESIAN_POINT ( 'NONE',  ( 18.52753015748617571, 43.09226448433412315, 4.923371831947298993 ) ) ;
#40698 = CARTESIAN_POINT ( 'NONE',  ( 19.42250999205614548, 35.98035201082151247, -5.440088680355545492 ) ) ;
#40699 = CARTESIAN_POINT ( 'NONE',  ( 12.63842701281683922, 64.55059781766745175, -9.846743663894590881 ) ) ;
#40701 = CARTESIAN_POINT ( 'NONE',  ( 1.816707512666842605, 45.10290668512025292, -6.499999999999958256 ) ) ;
#40700 = CARTESIAN_POINT ( 'NONE',  ( -4.164238869374098151, 26.59541550158063217, -3.795296366450310543 ) ) ;
#40702 = CARTESIAN_POINT ( 'NONE',  ( -13.40508947812791796, 15.00000000000000000, -5.527528931052510863 ) ) ;
#40703 = CARTESIAN_POINT ( 'NONE',  ( 19.84674366389459621, 18.50893115100078745, 7.409399052514197653E-17 ) ) ;
#40704 = CARTESIAN_POINT ( 'NONE',  ( 0.6178305044545838731, 54.74863466993042493, 9.382169495545420901 ) ) ;
#40705 = CARTESIAN_POINT ( 'NONE',  ( 1.472469842513823179, 50.59226448433411605, -4.923371831947296329 ) ) ;
#40706 = VERTEX_POINT ( 'NONE', #7991 ) ;
#40707 = CARTESIAN_POINT ( 'NONE',  ( 2.603489959281613420, 35.43575266056827644, -6.500000000000031086 ) ) ;
#40708 = CARTESIAN_POINT ( 'NONE',  ( -0.8801773607111009756, 3.063685344154838397, 1.068504757029289695E-15 ) ) ;
#40709 = CARTESIAN_POINT ( 'NONE',  ( 10.00000000000000000, 15.55374883491396787, -14.16423886937410082 ) ) ;
#40710 = CARTESIAN_POINT ( 'NONE',  ( 19.84674366389459266, 3.717264484334118713, -2.638427012816827677 ) ) ;
#40711 = CARTESIAN_POINT ( 'NONE',  ( 5.076628168052704559, 55.17559781766745175, -8.527530157486179263 ) ) ;
#40712 = CARTESIAN_POINT ( 'NONE',  ( 19.42250999205614548, 25.98035201082150891, -5.440088680355545492 ) ) ;
#40713 = DIRECTION ( 'NONE',  ( -0.8038568606172203923, 0.000000000000000000, 0.5948227867513371514 ) ) ;
#40714 = CARTESIAN_POINT ( 'NONE',  ( 1.472469842513823179, 61.42559781766745175, 4.923371831947296329 ) ) ;
#40715 = VECTOR ( 'NONE', #19907, 1000.000000000000000 ) ;
#40716 = EDGE_CURVE ( 'NONE', #63612, #56374, #31827, .T. ) ;
#40717 = CARTESIAN_POINT ( 'NONE',  ( 2.791683348922237240, 0.3839311510007847872, -7.208316651077763204 ) ) ;
#40718 = CARTESIAN_POINT ( 'NONE',  ( 0.2751277870542967463, 70.00000000000000000, 6.000000000000000000 ) ) ;
#40719 = ORIENTED_EDGE ( 'NONE', *, *, #18796, .T. ) ;
#40720 = VERTEX_POINT ( 'NONE', #92454 ) ;
#40721 = CARTESIAN_POINT ( 'NONE',  ( 2.550000000000003819, 99.99999999999998579, -8.525133428036873795 ) ) ;
#40722 = CARTESIAN_POINT ( 'NONE',  ( -0.3689425029237898834, 11.17874883491396787, -10.36894250292378850 ) ) ;
#40723 =( GEOMETRIC_REPRESENTATION_CONTEXT ( 3 ) GLOBAL_UNCERTAINTY_ASSIGNED_CONTEXT ( ( #44461 ) ) GLOBAL_UNIT_ASSIGNED_CONTEXT ( ( #75827, #90318, #7840 ) ) REPRESENTATION_CONTEXT ( 'NONE', 'WORKASPACE' ) );
#40724 = CARTESIAN_POINT ( 'NONE',  ( 20.36894250292379382, 38.67874883491396076, 10.36894250292379205 ) ) ;
#40725 = CARTESIAN_POINT ( 'NONE',  ( 18.52753015748618282, 53.92559781766745175, -4.923371831947291888 ) ) ;
#40726 = CARTESIAN_POINT ( 'NONE',  ( 12.63842701281683034, 17.46726448433411250, 9.846743663894596210 ) ) ;
#40727 = SURFACE_STYLE_FILL_AREA ( #26692 ) ;
#40729 = CARTESIAN_POINT ( 'NONE',  ( 14.92337183194729988, 64.34226448433412315, -8.527530157486177487 ) ) ;
#40728 = CARTESIAN_POINT ( 'NONE',  ( 7.084665262690076126, 17.02201867748817676, -10.88017736071110164 ) ) ;
#40730 = CARTESIAN_POINT ( 'NONE',  ( 10.00000000000000000, 40.55374883491397497, -14.16423886937410082 ) ) ;
#40731 = AXIS2_PLACEMENT_3D ( 'NONE', #64849, #42376, #4387 ) ;
#40732 = CARTESIAN_POINT ( 'NONE',  ( -0.8801773607111008646, 3.272018677488171434, 2.915334737309923430 ) ) ;
#40733 = CARTESIAN_POINT ( 'NONE',  ( 10.84451454130507209, 4.631809541732465460E-16, -9.625305416630832056 ) ) ;
#40734 = DIRECTION ( 'NONE',  ( -4.174438572590589223E-14, 0.000000000000000000, 1.000000000000000000 ) ) ;
#40735 = CARTESIAN_POINT ( 'NONE',  ( 0.5774900079438607392, 58.48035201082151247, 5.440088680355550821 ) ) ;
#40736 = CARTESIAN_POINT ( 'NONE',  ( 0.1532563361054083140, 16.00893115100078390, 1.131784320476157264E-15 ) ) ;
#40737 = CARTESIAN_POINT ( 'NONE',  ( -6.031993939728320875, -39.82530731229964260, 3.999999999998387068 ) ) ;
#40738 = ORIENTED_EDGE ( 'NONE', *, *, #67752, .T. ) ;
#40739 = CARTESIAN_POINT ( 'NONE',  ( 10.00000000000000178, 65.37363466993042493, 12.81628187352647608 ) ) ;
#40740 = ORIENTED_EDGE ( 'NONE', *, *, #61171, .T. ) ;
#40741 = CARTESIAN_POINT ( 'NONE',  ( 18.52753015748618282, 23.92559781766745530, -4.923371831947291888 ) ) ;
#40742 = ORIENTED_EDGE ( 'NONE', *, *, #63487, .F. ) ;
#40743 = CARTESIAN_POINT ( 'NONE',  ( -4.164238869374099927, 32.01208216824730357, 3.795296366450308767 ) ) ;
#40744 = CARTESIAN_POINT ( 'NONE',  ( 1.472469842513823179, 30.59226448433411960, -4.923371831947296329 ) ) ;
#40745 = CARTESIAN_POINT ( 'NONE',  ( 0.5774900079438607392, 38.48035201082150536, 5.440088680355550821 ) ) ;
#40746 = DIRECTION ( 'NONE',  ( -1.000000000000000000, 0.000000000000000000, 0.000000000000000000 ) ) ;
#40747 = VERTEX_POINT ( 'NONE', #54452 ) ;
#40748 = CARTESIAN_POINT ( 'NONE',  ( 7.084665262690076126, 37.02201867748817676, -10.88017736071110164 ) ) ;
#40749 = CARTESIAN_POINT ( 'NONE',  ( 19.88565890683628368, 37.71691075486301514, -6.480892540919849232 ) ) ;
#40750 =( GEOMETRIC_REPRESENTATION_CONTEXT ( 3 ) GLOBAL_UNCERTAINTY_ASSIGNED_CONTEXT ( ( #3201 ) ) GLOBAL_UNIT_ASSIGNED_CONTEXT ( ( #69237, #61228, #53236 ) ) REPRESENTATION_CONTEXT ( 'NONE', 'WORKASPACE' ) );
#40751 = CARTESIAN_POINT ( 'NONE',  ( -12.81628187352647608, -10.87636533006957507, 3.903127820947815962E-15 ) ) ;
#40752 = ORIENTED_EDGE ( 'NONE', *, *, #41663, .T. ) ;
#40753 = CARTESIAN_POINT ( 'NONE',  ( -0.8801773607110991993, 42.85535201082150536, -2.915334737309923874 ) ) ;
#40754 = CARTESIAN_POINT ( 'NONE',  ( 6.204703633549690345, 10.76208216824729824, -14.16423886937410259 ) ) ;
#40755 = ORIENTED_EDGE ( 'NONE', *, *, #71397, .F. ) ;
#40756 = ORIENTED_EDGE ( 'NONE', *, *, #88215, .T. ) ;
#40757 = CARTESIAN_POINT ( 'NONE',  ( 21.09922568453595559, 37.04030133659708923, -6.408140936763230044 ) ) ;
#40758 = SURFACE_STYLE_FILL_AREA ( #64218 ) ;
#40759 = CARTESIAN_POINT ( 'NONE',  ( 0.1532563361054082862, 21.21726448433412315, 2.638427012816831674 ) ) ;
#40760 =( NAMED_UNIT ( * ) PLANE_ANGLE_UNIT ( ) SI_UNIT ( $, .RADIAN. ) );
#40761 = ADVANCED_FACE ( 'NONE', ( #85455 ), #10458, .T. ) ;
#40762 = CARTESIAN_POINT ( 'NONE',  ( 14.92337183194729988, 34.34226448433411605, -8.527530157486177487 ) ) ;
#40763 = AXIS2_PLACEMENT_3D ( 'NONE', #61319, #22359, #29829 ) ;
#40764 = CARTESIAN_POINT ( 'NONE',  ( 10.00000000000000178, 59.31368534415484106, 10.88017736071110342 ) ) ;
#40765 = ADVANCED_FACE ( 'NONE', ( #94915 ), #3443, .F. ) ;
#40766 = DIRECTION ( 'NONE',  ( 0.000000000000000000, 0.000000000000000000, 1.000000000000000000 ) ) ;
#40767 = VECTOR ( 'NONE', #68257, 1000.000000000000000 ) ;
#40768 = SURFACE_SIDE_STYLE ('',( #49719 ) ) ;
#40769 = CARTESIAN_POINT ( 'NONE',  ( 20.88017736071110164, 65.35535201082150536, 2.915334737309930979 ) ) ;
#40770 = CARTESIAN_POINT ( 'NONE',  ( 18.72515096720583827, 30.05509018479937566, 6.499999999999810818 ) ) ;
#40771 = ADVANCED_FACE ( 'NONE', ( #86448 ), #75521, .T. ) ;
#40772 = FACE_OUTER_BOUND ( 'NONE', #63293, .T. ) ;
#40773 = CARTESIAN_POINT ( 'NONE',  ( 0.1532563361054100626, 5.800597817667452638, -2.638427012816831230 ) ) ;
#40774 = EDGE_CURVE ( 'NONE', #24283, #70171, #73618, .T. ) ;
#40775 = CARTESIAN_POINT ( 'NONE',  ( 10.00000000000000178, 15.37363466993042138, 12.81628187352647608 ) ) ;
#40776 = DIRECTION ( 'NONE',  ( 0.000000000000000000, -1.000000000000000000, 0.000000000000000000 ) ) ;
#40777 =( GEOMETRIC_REPRESENTATION_CONTEXT ( 3 ) GLOBAL_UNCERTAINTY_ASSIGNED_CONTEXT ( ( #21147 ) ) GLOBAL_UNIT_ASSIGNED_CONTEXT ( ( #21090, #51589, #22089 ) ) REPRESENTATION_CONTEXT ( 'NONE', 'WORKASPACE' ) );
#40778 = CARTESIAN_POINT ( 'NONE',  ( 0.1532563361054100626, 50.80059781766745175, -2.638427012816831230 ) ) ;
#40779 = CARTESIAN_POINT ( 'NONE',  ( 19.42250999205614548, 35.98035201082151247, -5.440088680355545492 ) ) ;
#40780 = CARTESIAN_POINT ( 'NONE',  ( 24.16423886937410614, 4.512082168247300906, -3.795296366450302550 ) ) ;
#40781 = CARTESIAN_POINT ( 'NONE',  ( 18.52753015748617571, 28.09226448433411960, 4.923371831947298993 ) ) ;
#40782 = CARTESIAN_POINT ( 'NONE',  ( -2.816281873526473856, 34.33196800326376064, 3.434112377981055619 ) ) ;
#40784 = CYLINDRICAL_SURFACE ( 'NONE', #75263, 7.000000000000002665 ) ;
#40783 =( NAMED_UNIT ( * ) SI_UNIT ( $, .STERADIAN. ) SOLID_ANGLE_UNIT ( ) );
#40785 = CARTESIAN_POINT ( 'NONE',  ( 7.084665262690076126, 49.10535201082149825, 10.88017736071109987 ) ) ;
#40786 = CARTESIAN_POINT ( 'NONE',  ( 22.81628187352647785, 1.623634669930420271, 6.195893100308588602E-16 ) ) ;
#40787 = CARTESIAN_POINT ( 'NONE',  ( 13.95692576442265853, 14.76984994696949727, -5.331646315825722127 ) ) ;
#40788 = CARTESIAN_POINT ( 'NONE',  ( 5.076628168052704559, 15.17559781766745175, -8.527530157486179263 ) ) ;
#40789 = CARTESIAN_POINT ( 'NONE',  ( 17.96484262340118221, 24.93868534415484461, 7.964842623401181321 ) ) ;
#40790 = CARTESIAN_POINT ( 'NONE',  ( 0.6178305044545818747, 23.49863466993041783, -9.382169495545419124 ) ) ;
#40791 = AXIS2_PLACEMENT_3D ( 'NONE', #92004, #23533, #46500 ) ;
#40792 = B_SPLINE_CURVE_WITH_KNOTS ( 'NONE', 3,
 ( #53715, #75233, #38724, #30216, #91216, #30707 ),
 .UNSPECIFIED., .F., .F.,
 ( 4, 2, 4 ),
 ( 0.000000000000000000, 0.0002701661927229225967, 0.0005403323854458451933 ),
 .UNSPECIFIED. ) ;
#40793 = CARTESIAN_POINT ( 'NONE',  ( -9.483770294663347755, 88.32858231846624619, 5.216041430090285758 ) ) ;
#40794 = AXIS2_PLACEMENT_3D ( 'NONE', #35233, #64737, #19750 ) ;
#40796 = B_SPLINE_CURVE_WITH_KNOTS ( 'NONE', 3,
 ( #90114, #76105, #22628, #66635, #89627, #14135 ),
 .UNSPECIFIED., .F., .F.,
 ( 4, 2, 4 ),
 ( 3.409110551496111039E-05, 0.0004400426677367849995, 0.0008459942299586088819 ),
 .UNSPECIFIED. ) ;
#40795 = CARTESIAN_POINT ( 'NONE',  ( 20.88017736071110164, 15.35535201082150358, 2.915334737309930979 ) ) ;
#40797 = AXIS2_PLACEMENT_3D ( 'NONE', #67224, #42747, #88235 ) ;
#40798 = CARTESIAN_POINT ( 'NONE',  ( 0.5774900079438590739, 67.64701867748817676, -5.440088680355550821 ) ) ;
#40800 = CARTESIAN_POINT ( 'NONE',  ( 17.96484262340118221, 36.18868534415484106, -7.964842623401177768 ) ) ;
#40799 = CARTESIAN_POINT ( 'NONE',  ( 5.076628168052704559, 45.17559781766745175, -8.527530157486179263 ) ) ;
#40801 = CARTESIAN_POINT ( 'NONE',  ( 14.99999999999997868, 79.82179676972448590, -6.250000000000000000 ) ) ;
#40802 = EDGE_CURVE ( 'NONE', #83218, #14105, #20671, .T. ) ;
#40803 = CARTESIAN_POINT ( 'NONE',  ( 0.5774900079438590739, 52.64701867748817676, -5.440088680355550821 ) ) ;
#40805 = LINE ( 'NONE', #26273, #63799 ) ;
#40804 = CARTESIAN_POINT ( 'NONE',  ( 7.084665262690076126, 9.105352010821503583, 10.88017736071109987 ) ) ;
#40806 = DIRECTION ( 'NONE',  ( 0.000000000000000000, 0.000000000000000000, -1.000000000000000000 ) ) ;
#40807 = CARTESIAN_POINT ( 'NONE',  ( 1.472469842513823179, 36.42559781766745175, 4.923371831947296329 ) ) ;
#40808 = DIRECTION ( 'NONE',  ( -0.000000000000000000, -1.000000000000000000, -0.000000000000000000 ) ) ;
#40809 = FACE_OUTER_BOUND ( 'NONE', #89386, .T. ) ;
#40810 = CARTESIAN_POINT ( 'NONE',  ( 16.40814093676324603, 2.456968003263753531, -11.09922568453594671 ) ) ;
#40811 = CARTESIAN_POINT ( 'NONE',  ( 20.15039907845753575, 50.60158574516642460, -6.262539305110073506 ) ) ;
#40812 = EDGE_CURVE ( 'NONE', #67453, #15068, #26066, .T. ) ;
#40813 = CARTESIAN_POINT ( 'NONE',  ( 10.00000000000000178, 28.05374883491396787, 14.16423886937410082 ) ) ;
#40814 = DIRECTION ( 'NONE',  ( -0.000000000000000000, -0.000000000000000000, -1.000000000000000000 ) ) ;
#40815 = ORIENTED_EDGE ( 'NONE', *, *, #73229, .T. ) ;
#40816 = CARTESIAN_POINT ( 'NONE',  ( 10.00000000000000000, 60.55374883491397497, -14.16423886937410082 ) ) ;
#40817 = CARTESIAN_POINT ( 'NONE',  ( 2.791683348922240793, 21.63393115100078745, 7.208316651077764092 ) ) ;
#40819 = CARTESIAN_POINT ( 'NONE',  ( -13.14228782657345107, 15.00000000000000000, 7.230509711182143917 ) ) ;
#40818 = LINE ( 'NONE', #41808, #85061 ) ;
#40820 = CARTESIAN_POINT ( 'NONE',  ( 15.44008868035555260, 54.73035201082150536, 9.422509992056143702 ) ) ;
#40821 = CARTESIAN_POINT ( 'NONE',  ( 0.6178305044545838731, 59.74863466993041783, 9.382169495545420901 ) ) ;
#40822 = CARTESIAN_POINT ( 'NONE',  ( 0.5774900079438607392, 28.48035201082150891, 5.440088680355550821 ) ) ;
#40823 = CARTESIAN_POINT ( 'NONE',  ( 16.40814093676324603, 62.45696800326376064, -11.09922568453594671 ) ) ;
#40824 = CARTESIAN_POINT ( 'NONE',  ( 16.40814093676323893, 5.790301336597087456, 11.09922568453595026 ) ) ;
#40825 = CARTESIAN_POINT ( 'NONE',  ( 12.63842701281683922, 9.550597817667449974, -9.846743663894590881 ) ) ;
#40826 = ORIENTED_EDGE ( 'NONE', *, *, #27524, .F. ) ;
#40827 = CARTESIAN_POINT ( 'NONE',  ( 14.99999999999997868, 80.07179676972448590, -4.250000000000000000 ) ) ;
#40828 = CARTESIAN_POINT ( 'NONE',  ( 22.26659068614894466, 58.88708216824729647, 7.082119434687054849 ) ) ;
#40829 = CARTESIAN_POINT ( 'NONE',  ( 2.917880565312950480, 30.97041550158063572, -12.26659068614894821 ) ) ;
#40830 = CARTESIAN_POINT ( 'NONE',  ( 17.96484262340118221, 14.93868534415483751, 7.964842623401181321 ) ) ;
#40831 = CARTESIAN_POINT ( 'NONE',  ( 19.42250999205614193, 50.14701867748817676, 5.440088680355555262 ) ) ;
#40832 = CARTESIAN_POINT ( 'NONE',  ( 10.47193227288532569, -40.28585825680447385, -3.999999999999999112 ) ) ;
#40833 = CARTESIAN_POINT ( 'NONE',  ( 0.1532563361054083140, 11.00893115100078568, 1.131784320476157264E-15 ) ) ;
#40834 =( LENGTH_UNIT ( ) NAMED_UNIT ( * ) SI_UNIT ( .MILLI., .METRE. ) );
#40835 = CARTESIAN_POINT ( 'NONE',  ( 5.076628168052703671, 16.84226448433411960, 8.527530157486179263 ) ) ;
#40836 = SURFACE_STYLE_USAGE ( .BOTH. , #41827 ) ;
#40837 = DIRECTION ( 'NONE',  ( 0.000000000000000000, -1.000000000000000000, 0.000000000000000000 ) ) ;
#40838 = CARTESIAN_POINT ( 'NONE',  ( 5.076628168052704559, 20.17559781766745175, -8.527530157486179263 ) ) ;
#40839 = CARTESIAN_POINT ( 'NONE',  ( 0.1532563361054083140, 51.00893115100078745, 1.131784320476157264E-15 ) ) ;
#40840 = VECTOR ( 'NONE', #43241, 1000.000000000000114 ) ;
#40841 = CARTESIAN_POINT ( 'NONE',  ( 0.5774900079438590739, 27.64701867748817676, -5.440088680355550821 ) ) ;
#40842 = CARTESIAN_POINT ( 'NONE',  ( 16.40814093676324603, 37.45696800326376064, -11.09922568453594671 ) ) ;
#40843 = AXIS2_PLACEMENT_3D ( 'NONE', #5316, #95310, #42812 ) ;
#40844 = CARTESIAN_POINT ( 'NONE',  ( -0.8801773607111009756, 58.06368534415484106, 1.068504757029289695E-15 ) ) ;
#40845 = CARTESIAN_POINT ( 'NONE',  ( 17.20831665107776587, 27.88393115100078390, 7.208316651077764980 ) ) ;
#40847 = CARTESIAN_POINT ( 'NONE',  ( 1.472469842513823179, 16.42559781766745175, 4.923371831947296329 ) ) ;
#40846 = CARTESIAN_POINT ( 'NONE',  ( -4.164238869374099927, 47.01208216824729647, 3.795296366450308767 ) ) ;
#40848 = DIRECTION ( 'NONE',  ( -0.9975640502598257520, 0.06975647374410356982, 0.000000000000000000 ) ) ;
#40849 = CARTESIAN_POINT ( 'NONE',  ( 5.076628168052703671, 56.84226448433412315, 8.527530157486179263 ) ) ;
#40850 = CARTESIAN_POINT ( 'NONE',  ( 18.52753015748617571, 48.09226448433412315, 4.923371831947298993 ) ) ;
#40851 = CARTESIAN_POINT ( 'NONE',  ( 20.36894250292379738, 29.92874883491396432, -10.36894250292379027 ) ) ;
#40852 = CARTESIAN_POINT ( 'NONE',  ( 19.84674366389459266, 28.30059781766745886, 2.638427012816836559 ) ) ;
#40853 = CARTESIAN_POINT ( 'NONE',  ( 15.44008868035555793, 46.39701867748817676, -9.422509992056140149 ) ) ;
#40854 = CARTESIAN_POINT ( 'NONE',  ( 10.00000000000000000, 21.81368534415484106, -10.88017736071110342 ) ) ;
#40855 = CARTESIAN_POINT ( 'NONE',  ( -0.8801773607111009756, 48.06368534415484817, 1.068504757029289695E-15 ) ) ;
#40856 = CARTESIAN_POINT ( 'NONE',  ( 17.96484262340118221, 26.18868534415483396, -7.964842623401177768 ) ) ;
#40857 = ORIENTED_EDGE ( 'NONE', *, *, #24949, .F. ) ;
#40858 = CARTESIAN_POINT ( 'NONE',  ( 16.40814093676323893, 30.79030133659708923, 11.09922568453595026 ) ) ;
#40859 = CARTESIAN_POINT ( 'NONE',  ( 10.00000000000000178, 59.31368534415484106, 10.88017736071110342 ) ) ;
#40860 = ORIENTED_EDGE ( 'NONE', *, *, #16221, .F. ) ;
#40861 = ADVANCED_FACE ( 'NONE', ( #49411 ), #6861, .T. ) ;
#40862 = LINE ( 'NONE', #25858, #31429 ) ;
#40863 = CARTESIAN_POINT ( 'NONE',  ( 4.559911319644449179, 67.23035201082150536, -9.422509992056141925 ) ) ;
#40864 = AXIS2_PLACEMENT_3D ( 'NONE', #30506, #8027, #23036 ) ;
#40865 = ORIENTED_EDGE ( 'NONE', *, *, #63561, .F. ) ;
#40866 = VECTOR ( 'NONE', #17869, 1000.000000000000000 ) ;
#40867 = CARTESIAN_POINT ( 'NONE',  ( 0.5774900079438590739, 62.64701867748817676, -5.440088680355550821 ) ) ;
#40868 =( NAMED_UNIT ( * ) SI_UNIT ( $, .STERADIAN. ) SOLID_ANGLE_UNIT ( ) );
#40869 = VECTOR ( 'NONE', #68346, 1000.000000000000000 ) ;
#40870 = CARTESIAN_POINT ( 'NONE',  ( 2.377183314879983911, 25.78593319516823001, -6.500000000000031974 ) ) ;
#40871 = CARTESIAN_POINT ( 'NONE',  ( 13.07751017357383994, 15.00000000000000000, -6.263284095430508458 ) ) ;
#40872 = CARTESIAN_POINT ( 'NONE',  ( -0.3689425029237898834, 56.17874883491396076, -10.36894250292378850 ) ) ;
#40873 = CARTESIAN_POINT ( 'NONE',  ( 10.00000000000000000, 14.75893115100078568, -9.846743663894594434 ) ) ;
#40874 = CARTESIAN_POINT ( 'NONE',  ( -0.3689425029237898834, 6.178748834913968757, -10.36894250292378850 ) ) ;
#40875 = CARTESIAN_POINT ( 'NONE',  ( 1.472469842513823179, 1.425597817667451528, 4.923371831947296329 ) ) ;
#40876 = CARTESIAN_POINT ( 'NONE',  ( 15.44008868035555260, 4.730352010821504471, 9.422509992056143702 ) ) ;
#40877 = CARTESIAN_POINT ( 'NONE',  ( 5.076628168052704559, 40.17559781766745175, -8.527530157486179263 ) ) ;
#40878 = ORIENTED_EDGE ( 'NONE', *, *, #32567, .F. ) ;
#40879 = CARTESIAN_POINT ( 'NONE',  ( 5.076628168052703671, 51.84226448433412315, 8.527530157486179263 ) ) ;
#40880 = ORIENTED_EDGE ( 'NONE', *, *, #60401, .F. ) ;
#40881 = DIRECTION ( 'NONE',  ( 0.000000000000000000, 0.000000000000000000, -1.000000000000000000 ) ) ;
#40882 = CARTESIAN_POINT ( 'NONE',  ( 10.00000000000000178, 59.31368534415484106, 10.88017736071110342 ) ) ;
#40883 = CARTESIAN_POINT ( 'NONE',  ( 1.472469842513823179, 55.59226448433412315, -4.923371831947296329 ) ) ;
#40884 = CARTESIAN_POINT ( 'NONE',  ( 10.00000000000000000, 27.87363466993042138, -12.81628187352647608 ) ) ;
#40886 = DIRECTION ( 'NONE',  ( 0.6087614290087296487, 0.000000000000000000, -0.7933533402912281707 ) ) ;
#40885 =( LENGTH_UNIT ( ) NAMED_UNIT ( * ) SI_UNIT ( .MILLI., .METRE. ) );
#40887 = CARTESIAN_POINT ( 'NONE',  ( 12.91533473730992121, 54.52201867748816255, 10.88017736071110164 ) ) ;
#40888 = CARTESIAN_POINT ( 'NONE',  ( 2.035157376598824452, 8.688685344154839285, 7.964842623401179544 ) ) ;
#40889 = EDGE_CURVE ( 'NONE', #64701, #12669, #30887, .T. ) ;
#40890 = AXIS2_PLACEMENT_3D ( 'NONE', #2957, #95407, #48425 ) ;
#40891 = CARTESIAN_POINT ( 'NONE',  ( 22.81628187352647785, 36.41530133659707502, 3.434112377981063169 ) ) ;
#40892 = CARTESIAN_POINT ( 'NONE',  ( -0.1503990784575328643, 10.12777174578612716, 6.262539305110068177 ) ) ;
#40893 = VERTEX_POINT ( 'NONE', #25938 ) ;
#40894 = CARTESIAN_POINT ( 'NONE',  ( 0.6178305044545818747, 33.49863466993042493, -9.382169495545419124 ) ) ;
#40895 = CARTESIAN_POINT ( 'NONE',  ( 0.5774900079438590739, 32.64701867748816966, -5.440088680355550821 ) ) ;
#40896 = EDGE_CURVE ( 'NONE', #6556, #4006, #87901, .T. ) ;
#40897 = EDGE_LOOP ( 'NONE', ( #64418, #76512, #21833, #9770, #54586, #90671, #22560, #6840, #37117, #73950 ) ) ;
#40898 = CARTESIAN_POINT ( 'NONE',  ( -1.099225684535947600, -1.293031996736246469, -6.408140936763238038 ) ) ;
#40900 = CARTESIAN_POINT ( 'NONE',  ( 0.1532563361054083140, 56.00893115100078745, 1.131784320476157264E-15 ) ) ;
#40899 = CARTESIAN_POINT ( 'NONE',  ( 12.63842701281683922, 9.550597817667449974, -9.846743663894590881 ) ) ;
#40901 = CARTESIAN_POINT ( 'NONE',  ( -10.07519558535470239, -32.17712024071101951, 3.750000000000001332 ) ) ;
#40902 = CARTESIAN_POINT ( 'NONE',  ( -1.780824192092595792, 0.3639308653492316359, 14.89391369643515617 ) ) ;
#40903 = CARTESIAN_POINT ( 'NONE',  ( 17.20831665107776587, 42.88393115100077324, 7.208316651077764980 ) ) ;
#40904 = CARTESIAN_POINT ( 'NONE',  ( -0.1503990784575247319, 52.22266099184918176, -6.262539305110083276 ) ) ;
#40905 = VECTOR ( 'NONE', #16919, 1000.000000000000114 ) ;
#40906 = CIRCLE ( 'NONE', #74433, 0.09999999999999982514 ) ;
#40907 = CARTESIAN_POINT ( 'NONE',  ( -3.499999999999998668, 1.019547802438465434, 2.500000000000000000 ) ) ;
#40909 = FILL_AREA_STYLE_COLOUR ( '', #78655 ) ;
#40908 = CARTESIAN_POINT ( 'NONE',  ( 17.20831665107776587, 24.13393115100078035, -7.208316651077762316 ) ) ;
#40910 = CARTESIAN_POINT ( 'NONE',  ( 4.096035146093440993, 4.852245006323173772E-16, 13.90943910019262120 ) ) ;
#40912 = ORIENTED_EDGE ( 'NONE', *, *, #21359, .T. ) ;
#40911 = CARTESIAN_POINT ( 'NONE',  ( 7.361572987183170547, 62.05059781766745886, 9.846743663894590881 ) ) ;
#40913 = CARTESIAN_POINT ( 'NONE',  ( 1.548803529117991573, 0.000000000000000000, 5.228673087012104759 ) ) ;
#40914 = CARTESIAN_POINT ( 'NONE',  ( 10.00000000000000000, 22.87363466993042138, -12.81628187352647608 ) ) ;
#40915 = CARTESIAN_POINT ( 'NONE',  ( 1.472469842513823179, 50.59226448433411605, -4.923371831947296329 ) ) ;
#40916 = EDGE_CURVE ( 'NONE', #3878, #43714, #18072, .T. ) ;
#40917 = CARTESIAN_POINT ( 'NONE',  ( 22.17874357816322117, 89.00000000000000000, -12.00000000000000000 ) ) ;
#40918 = CARTESIAN_POINT ( 'NONE',  ( 24.16423886937410614, 49.30374883491396787, 8.672049930838204340E-16 ) ) ;
#40919 = CARTESIAN_POINT ( 'NONE',  ( 14.92337183194729988, 14.34226448433411782, -8.527530157486177487 ) ) ;
#40920 = CIRCLE ( 'NONE', #37790, 3.799999999999998934 ) ;
#40921 = DIRECTION ( 'NONE',  ( 0.000000000000000000, 1.000000000000000000, 0.000000000000000000 ) ) ;
#40922 = DIRECTION ( 'NONE',  ( -0.000000000000000000, 1.000000000000000000, -0.000000000000000000 ) ) ;
#40923 = CARTESIAN_POINT ( 'NONE',  ( -0.3689425029237881626, 42.42874883491396787, 10.36894250292379027 ) ) ;
#40924 = CARTESIAN_POINT ( 'NONE',  ( 5.076628168052704559, 60.17559781766745175, -8.527530157486179263 ) ) ;
#40925 = EDGE_CURVE ( 'NONE', #23291, #66530, #79912, .T. ) ;
#40926 = CARTESIAN_POINT ( 'NONE',  ( -0.8801773607110991993, 12.85535201082150358, -2.915334737309923874 ) ) ;
#40927 = CARTESIAN_POINT ( 'NONE',  ( 13.79529636645030344, 28.26208216824729647, 14.16423886937410614 ) ) ;
#40928 = CARTESIAN_POINT ( 'NONE',  ( 13.79529636645031943, 35.34541550158063927, -14.16423886937409904 ) ) ;
#40929 = FILL_AREA_STYLE_COLOUR ( '', #94679 ) ;
#40931 = CARTESIAN_POINT ( 'NONE',  ( 14.92337183194729988, 49.34226448433411605, -8.527530157486177487 ) ) ;
#40930 = CARTESIAN_POINT ( 'NONE',  ( 0.5774900079438590739, 27.64701867748817676, -5.440088680355550821 ) ) ;
#40932 = ORIENTED_EDGE ( 'NONE', *, *, #10178, .F. ) ;
#40933 = CARTESIAN_POINT ( 'NONE',  ( 20.88017736071110164, 40.35535201082150536, 2.915334737309930979 ) ) ;
#40934 = CARTESIAN_POINT ( 'NONE',  ( 19.88565890683628012, 22.71691075486302580, -6.480892540919844791 ) ) ;
#40935 = DIRECTION ( 'NONE',  ( 0.000000000000000000, 1.000000000000000000, 0.000000000000000000 ) ) ;
#40936 = CARTESIAN_POINT ( 'NONE',  ( -1.983216688681034068, 0.000000000000000000, 14.11131997956736406 ) ) ;
#40938 = VECTOR ( 'NONE', #74335, 1000.000000000000227 ) ;
#40937 = CARTESIAN_POINT ( 'NONE',  ( -5.204170427930421283E-15, 5.553748834913975863, -14.16423886937410082 ) ) ;
#40939 = CARTESIAN_POINT ( 'NONE',  ( 2.791683348922237240, 50.38393115100078035, -7.208316651077763204 ) ) ;
#40940 = CARTESIAN_POINT ( 'NONE',  ( 1.472469842513823179, 61.42559781766745175, 4.923371831947296329 ) ) ;
#40941 = ORIENTED_EDGE ( 'NONE', *, *, #14836, .F. ) ;
#40942 = CARTESIAN_POINT ( 'NONE',  ( 10.00000000000000178, 33.05374883491396787, 14.16423886937410082 ) ) ;
#40943 = CIRCLE ( 'NONE', #96841, 2.250000000000000444 ) ;
#40944 = CARTESIAN_POINT ( 'NONE',  ( -3.250000000000000444, 1.019547802438465656, -2.500000000000000000 ) ) ;
#40945 = DIRECTION ( 'NONE',  ( 0.000000000000000000, -1.000000000000000000, 0.000000000000000000 ) ) ;
#40946 = CARTESIAN_POINT ( 'NONE',  ( 12.91533473730993009, 6.605352010821504471, -10.88017736071109987 ) ) ;
#40947 = CARTESIAN_POINT ( 'NONE',  ( 13.43411237798105340, 25.58196800326374998, 12.81628187352647963 ) ) ;
#40948 = CARTESIAN_POINT ( 'NONE',  ( 3.469446951953614189E-15, 10.93830936912750573, 11.92686044187656513 ) ) ;
#40949 = CARTESIAN_POINT ( 'NONE',  ( 1.472469842513823179, 11.42559781766745175, 4.923371831947296329 ) ) ;
#40950 = FACE_OUTER_BOUND ( 'NONE', #76925, .T. ) ;
#40951 = B_SPLINE_CURVE_WITH_KNOTS ( 'NONE', 3,
 ( #58592, #89094, #20609, #19613, #83079, #38089 ),
 .UNSPECIFIED., .F., .F.,
 ( 4, 2, 4 ),
 ( 6.705420115022808671E-18, 0.0002626113303185853608, 0.0005252226606371639996 ),
 .UNSPECIFIED. ) ;
#40952 = CARTESIAN_POINT ( 'NONE',  ( -0.2418659066527783508, 9.260286857231744051, -6.114288769123032985 ) ) ;
#40953 = MANIFOLD_SOLID_BREP ( 'Fillet11', #60156 ) ;
#40954 = CARTESIAN_POINT ( 'NONE',  ( 19.42250999205614193, 5.147018677488171434, 5.440088680355555262 ) ) ;
#40955 = CARTESIAN_POINT ( 'NONE',  ( -7.750000000000000000, 43.00000000000000000, 6.250000000000000000 ) ) ;
#40956 = CARTESIAN_POINT ( 'NONE',  ( 17.96484262340118221, 34.93868534415482685, 7.964842623401181321 ) ) ;
#40957 = CARTESIAN_POINT ( 'NONE',  ( 12.91533473730992121, 34.52201867748817676, 10.88017736071110164 ) ) ;
#40958 = CARTESIAN_POINT ( 'NONE',  ( 0.6178305044545838731, 4.748634669930420493, 9.382169495545420901 ) ) ;
#40959 = CARTESIAN_POINT ( 'NONE',  ( 5.076628168052703671, 61.84226448433412315, 8.527530157486179263 ) ) ;
#40960 = CARTESIAN_POINT ( 'NONE',  ( 19.38216949554541202, 60.99863466993042493, 9.382169495545424454 ) ) ;
#40961 = CARTESIAN_POINT ( 'NONE',  ( 19.84674366389459621, 13.50893115100078568, 7.409399052514197653E-17 ) ) ;
#40962 = EDGE_LOOP ( 'NONE', ( #6797, #2517, #90317, #81222 ) ) ;
#40963 = CARTESIAN_POINT ( 'NONE',  ( 7.084665262690076126, 37.02201867748817676, -10.88017736071110164 ) ) ;
#40964 = CARTESIAN_POINT ( 'NONE',  ( 22.81628187352647785, 36.41530133659707502, 3.434112377981063169 ) ) ;
#40965 = VECTOR ( 'NONE', #12249, 1000.000000000000000 ) ;
#40966 = CARTESIAN_POINT ( 'NONE',  ( -0.3289641300568005855, 54.27164270246084499, -5.963430220938281678 ) ) ;
#40967 = AXIS2_PLACEMENT_3D ( 'NONE', #87377, #70421, #10894 ) ;
#40968 = TOROIDAL_SURFACE ( 'NONE', #56929, 14.49999999999999822, 0.5000000000000000000 ) ;
#40969 = CARTESIAN_POINT ( 'NONE',  ( 19.84674366389459621, 63.50893115100078745, 7.409399052514197653E-17 ) ) ;
#40970 = CARTESIAN_POINT ( 'NONE',  ( 0.5774900079438590739, 67.64701867748817676, -5.440088680355550821 ) ) ;
#40971 = CARTESIAN_POINT ( 'NONE',  ( 14.92337183194729633, 17.67559781766745175, 8.527530157486181039 ) ) ;
#40972 = CARTESIAN_POINT ( 'NONE',  ( 3.591859063236763294, 33.29030133659708213, -11.09922568453595026 ) ) ;
#40973 = CARTESIAN_POINT ( 'NONE',  ( 20.88017736071110875, 55.77201867748816966, -2.915334737309920765 ) ) ;
#40974 = ORIENTED_EDGE ( 'NONE', *, *, #32559, .F. ) ;
#40975 = DIRECTION ( 'NONE',  ( -1.257568779154408793E-17, -1.000000000000000000, 0.000000000000000000 ) ) ;
#40976 = CARTESIAN_POINT ( 'NONE',  ( 2.035157376598824452, 8.688685344154839285, 7.964842623401179544 ) ) ;
#40978 = CARTESIAN_POINT ( 'NONE',  ( -2.266590686148945544, 26.38708216824730357, -7.082119434687050408 ) ) ;
#40977 = CARTESIAN_POINT ( 'NONE',  ( 10.00000000000000178, 65.37363466993042493, 12.81628187352647608 ) ) ;
#40979 = CARTESIAN_POINT ( 'NONE',  ( 12.63842701281683034, 22.46726448433411605, 9.846743663894596210 ) ) ;
#40980 = SURFACE_STYLE_USAGE ( .BOTH. , #98554 ) ;
#40981 = CARTESIAN_POINT ( 'NONE',  ( 0.1532563361054083140, 16.00893115100078390, 1.131784320476157264E-15 ) ) ;
#40982 = CARTESIAN_POINT ( 'NONE',  ( 22.26659068614895176, 59.72041550158063927, -7.082119434687042414 ) ) ;
#40983 = ORIENTED_EDGE ( 'NONE', *, *, #61474, .T. ) ;
#40984 = AXIS2_PLACEMENT_3D ( 'NONE', #80968, #73452, #4002 ) ;
#40985 = CARTESIAN_POINT ( 'NONE',  ( 19.42250999205614548, 15.98035201082150714, -5.440088680355545492 ) ) ;
#40986 = ADVANCED_FACE ( 'NONE', ( #51890 ), #37333, .T. ) ;
#40987 = CARTESIAN_POINT ( 'NONE',  ( 17.96484262340118221, 14.93868534415483751, 7.964842623401181321 ) ) ;
#40988 = CARTESIAN_POINT ( 'NONE',  ( 20.10384461210892226, 46.74302437010791778, 6.337995344473753789 ) ) ;
#40989 = VERTEX_POINT ( 'NONE', #93635 ) ;
#40991 = VERTEX_POINT ( 'NONE', #86145 ) ;
#40990 = AXIS2_PLACEMENT_3D ( 'NONE', #73576, #20094, #34589 ) ;
#40992 = CARTESIAN_POINT ( 'NONE',  ( 12.91533473730993009, 21.60535201082150536, -10.88017736071109987 ) ) ;
#40993 = CARTESIAN_POINT ( 'NONE',  ( 7.361572987183170547, 52.05059781766745175, 9.846743663894590881 ) ) ;
#40994 = CARTESIAN_POINT ( 'NONE',  ( 3.591859063236761518, 49.95696800326375353, 11.09922568453594849 ) ) ;
#40995 = CARTESIAN_POINT ( 'NONE',  ( -0.8801773607111009756, 68.06368534415484817, 1.068504757029289695E-15 ) ) ;
#40996 = CARTESIAN_POINT ( 'NONE',  ( 10.00000000000000178, 18.05374883491396787, 14.16423886937410082 ) ) ;
#40997 = CARTESIAN_POINT ( 'NONE',  ( -0.8801773607111009756, 33.06368534415484106, 1.068504757029289695E-15 ) ) ;
#40998 = CARTESIAN_POINT ( 'NONE',  ( 0.5774900079438590739, 22.64701867748817321, -5.440088680355550821 ) ) ;
#40999 = CARTESIAN_POINT ( 'NONE',  ( 7.361572987183169658, 54.96726448433413026, -9.846743663894592657 ) ) ;
#41000 = CARTESIAN_POINT ( 'NONE',  ( -11.30269888132237810, -57.08933895092661004, -3.749999999999999556 ) ) ;
#41001 = CARTESIAN_POINT ( 'NONE',  ( 18.52753015748618282, 38.92559781766745175, -4.923371831947291888 ) ) ;
#41002 = CARTESIAN_POINT ( 'NONE',  ( 10.00000000000000000, 4.758931151000784787, -9.846743663894594434 ) ) ;
#41003 = CARTESIAN_POINT ( 'NONE',  ( -11.09922568453594316, -25.45969866340290721, 6.408140936763246920 ) ) ;
#41004 = ORIENTED_EDGE ( 'NONE', *, *, #46732, .T. ) ;
#41005 = CARTESIAN_POINT ( 'NONE',  ( 4.559911319644449179, 2.230352010821504471, -9.422509992056141925 ) ) ;
#41006 = CARTESIAN_POINT ( 'NONE',  ( 0.1532563361054083140, 11.00893115100078568, 1.131784320476157264E-15 ) ) ;
#41007 = CARTESIAN_POINT ( 'NONE',  ( 0.6178305044545838731, -0.2513653300695798953, 9.382169495545420901 ) ) ;
#41009 = CARTESIAN_POINT ( 'NONE',  ( 20.88017736071110164, 45.35535201082149115, 2.915334737309930979 ) ) ;
#41008 = CARTESIAN_POINT ( 'NONE',  ( 17.96484262340118221, 49.93868534415484106, 7.964842623401181321 ) ) ;
#41011 = CARTESIAN_POINT ( 'NONE',  ( 16.40814093676324603, 42.45696800326375353, -11.09922568453594671 ) ) ;
#41010 = CARTESIAN_POINT ( 'NONE',  ( 20.88017736071110875, 15.77201867748817143, -2.915334737309920765 ) ) ;
#41012 = CARTESIAN_POINT ( 'NONE',  ( 2.917880565312950480, 25.97041550158063572, -12.26659068614894821 ) ) ;
#41013 = LINE ( 'NONE', #26478, #93754 ) ;
#41014 = EDGE_CURVE ( 'NONE', #47240, #39693, #23692, .T. ) ;
#41016 = CARTESIAN_POINT ( 'NONE',  ( 21.09922568453595559, 62.04030133659709634, -6.408140936763230044 ) ) ;
#41015 = CIRCLE ( 'NONE', #90527, 0.2500000000000002220 ) ;
#41017 = ORIENTED_EDGE ( 'NONE', *, *, #75348, .T. ) ;
#41018 = CARTESIAN_POINT ( 'NONE',  ( 14.92337183194729988, 59.34226448433412315, -8.527530157486177487 ) ) ;
#41019 = EDGE_CURVE ( 'NONE', #12064, #40893, #86637, .T. ) ;
#41020 = CARTESIAN_POINT ( 'NONE',  ( 15.44008868035555260, 39.73035201082150536, 9.422509992056143702 ) ) ;
#41021 = ORIENTED_EDGE ( 'NONE', *, *, #87262, .F. ) ;
#41022 = CARTESIAN_POINT ( 'NONE',  ( 1.472469842513823179, 1.425597817667451528, 4.923371831947296329 ) ) ;
#41023 = DIRECTION ( 'NONE',  ( 0.000000000000000000, -1.000000000000000000, 0.000000000000000000 ) ) ;
#41024 = CARTESIAN_POINT ( 'NONE',  ( 5.076628168052703671, 26.84226448433411960, 8.527530157486179263 ) ) ;
#41025 = CARTESIAN_POINT ( 'NONE',  ( 7.084665262690076126, 67.02201867748817676, -10.88017736071110164 ) ) ;
#41026 = CARTESIAN_POINT ( 'NONE',  ( 7.361572987183170547, 2.050597817667451750, 9.846743663894590881 ) ) ;
#41028 = CARTESIAN_POINT ( 'NONE',  ( -4.841308736149794179, 0.2301500557980292461, 14.13449535775529675 ) ) ;
#41027 = CARTESIAN_POINT ( 'NONE',  ( 7.084665262690076126, 62.02201867748816966, -10.88017736071110164 ) ) ;
#41029 = CARTESIAN_POINT ( 'NONE',  ( 12.91533473730992121, 59.52201867748816966, 10.88017736071110164 ) ) ;
#41031 = ORIENTED_EDGE ( 'NONE', *, *, #21354, .F. ) ;
#41030 = CARTESIAN_POINT ( 'NONE',  ( 0.1532563361054082862, 11.21726448433411605, 2.638427012816831674 ) ) ;
#41032 = MECHANICAL_DESIGN_GEOMETRIC_PRESENTATION_REPRESENTATION (  '', ( #95329 ), #92123 ) ;
#41033 = LINE ( 'NONE', #26023, #98119 ) ;
#41034 = CIRCLE ( 'NONE', #66574, 0.2499999999999997780 ) ;
#41035 = CARTESIAN_POINT ( 'NONE',  ( 19.84674366389459621, 53.50893115100078745, 7.409399052514197653E-17 ) ) ;
#41036 = ORIENTED_EDGE ( 'NONE', *, *, #56910, .F. ) ;
#41037 = VERTEX_POINT ( 'NONE', #77153 ) ;
#41038 = DIRECTION ( 'NONE',  ( 0.000000000000000000, 0.000000000000000000, -1.000000000000000000 ) ) ;
#41039 = CARTESIAN_POINT ( 'NONE',  ( -4.164238869374099039, 6.803748834913967869, 8.674139862899312516E-16 ) ) ;
#41040 = CARTESIAN_POINT ( 'NONE',  ( 6.565887622018943937, 55.16530133659709634, 12.81628187352647430 ) ) ;
#41041 = CARTESIAN_POINT ( 'NONE',  ( -0.3689425029237881626, 7.428748834913967869, 10.36894250292379027 ) ) ;
#41042 = CARTESIAN_POINT ( 'NONE',  ( 2.917880565312948704, 32.63708216824730357, 12.26659068614894643 ) ) ;
#41043 =( NAMED_UNIT ( * ) PLANE_ANGLE_UNIT ( ) SI_UNIT ( $, .RADIAN. ) );
#41044 = CARTESIAN_POINT ( 'NONE',  ( 24.16423886937409904, 4.095415501580634832, 3.795296366450317205 ) ) ;
#41045 = CARTESIAN_POINT ( 'NONE',  ( -0.8801773607111008646, 23.27201867748817676, 2.915334737309923430 ) ) ;
#41046 =( NAMED_UNIT ( * ) PLANE_ANGLE_UNIT ( ) SI_UNIT ( $, .RADIAN. ) );
#41047 = ORIENTED_EDGE ( 'NONE', *, *, #9761, .F. ) ;
#41048 = CARTESIAN_POINT ( 'NONE',  ( 18.52753015748617571, 23.09226448433411960, 4.923371831947298993 ) ) ;
#41049 = CARTESIAN_POINT ( 'NONE',  ( 14.92337183194729633, 17.67559781766745175, 8.527530157486181039 ) ) ;
#41050 = CARTESIAN_POINT ( 'NONE',  ( 3.591859063236761518, 49.95696800326375353, 11.09922568453594849 ) ) ;
#41051 = CARTESIAN_POINT ( 'NONE',  ( 12.63842701281683922, 34.55059781766745886, -9.846743663894590881 ) ) ;
#41052 = CARTESIAN_POINT ( 'NONE',  ( 0.000000000000000000, -97.00000000000000000, -3.750000000000000000 ) ) ;
#41053 = CARTESIAN_POINT ( 'NONE',  ( 12.91533473730993009, 56.60535201082151247, -10.88017736071109987 ) ) ;
#41054 = CARTESIAN_POINT ( 'NONE',  ( 0.6178305044545818747, 33.49863466993042493, -9.382169495545419124 ) ) ;
#41055 = CARTESIAN_POINT ( 'NONE',  ( -3.795296366450300773, -27.15458449841936428, 14.16423886937410437 ) ) ;
#41056 = COLOUR_RGB ( '', 0.40784314, 0.44705882, 0.49803922) ;
#41057 = CARTESIAN_POINT ( 'NONE',  ( 10.00000000000000178, 27.25893115100078390, 9.846743663894594434 ) ) ;
#41058 = CARTESIAN_POINT ( 'NONE',  ( -2.266590686148945544, 11.38708216824730179, -7.082119434687050408 ) ) ;
#41059 = ORIENTED_EDGE ( 'NONE', *, *, #61660, .T. ) ;
#41060 = CIRCLE ( 'NONE', #77733, 15.00000000000000000 ) ;
#41061 = CARTESIAN_POINT ( 'NONE',  ( 20.88017736071110875, 30.77201867748816966, -2.915334737309920765 ) ) ;
#41062 = CARTESIAN_POINT ( 'NONE',  ( 2.917880565312948704, 27.63708216824730357, 12.26659068614894643 ) ) ;
#41063 = CARTESIAN_POINT ( 'NONE',  ( 18.52753015748617571, 48.09226448433412315, 4.923371831947298993 ) ) ;
#41064 = CARTESIAN_POINT ( 'NONE',  ( 1.472469842513823179, 10.59226448433411782, -4.923371831947296329 ) ) ;
#41066 = DIRECTION ( 'NONE',  ( 0.000000000000000000, -1.000000000000000000, 0.000000000000000000 ) ) ;
#41065 = CARTESIAN_POINT ( 'NONE',  ( 13.43411237798106583, 47.66530133659709634, -12.81628187352647252 ) ) ;
#41067 = CARTESIAN_POINT ( 'NONE',  ( 17.96484262340118221, 34.93868534415482685, 7.964842623401181321 ) ) ;
#41068 = CARTESIAN_POINT ( 'NONE',  ( -10.70613742633244669, 4.850979303660538556E-16, -9.778988772285387654 ) ) ;
#41069 = CARTESIAN_POINT ( 'NONE',  ( 3.591859063236763294, 18.29030133659708568, -11.09922568453595026 ) ) ;
#41070 = CARTESIAN_POINT ( 'NONE',  ( 13.43411237798106583, 17.66530133659708923, -12.81628187352647252 ) ) ;
#41071 = CARTESIAN_POINT ( 'NONE',  ( 2.791683348922240793, 36.63393115100078035, 7.208316651077764092 ) ) ;
#41072 = CARTESIAN_POINT ( 'NONE',  ( -10.88017736071109987, 3.272018677488170990, 2.915334737309934532 ) ) ;
#41073 = FILL_AREA_STYLE_COLOUR ( '', #10124 ) ;
#41075 = CARTESIAN_POINT ( 'NONE',  ( 0.000000000000000000, 0.5000000000000004441, 0.000000000000000000 ) ) ;
#41074 = LINE ( 'NONE', #79051, #66324 ) ;
#41076 = CARTESIAN_POINT ( 'NONE',  ( -7.750000000000000000, 1.019547802438458550, 4.000000000000000000 ) ) ;
#41077 = CARTESIAN_POINT ( 'NONE',  ( 10.00000000000000178, 70.00000000000000000, 0.000000000000000000 ) ) ;
#41078 = CARTESIAN_POINT ( 'NONE',  ( 19.42250999205614193, 50.14701867748817676, 5.440088680355555262 ) ) ;
#41079 = CARTESIAN_POINT ( 'NONE',  ( 10.00000000000000000, 61.81368534415484106, -10.88017736071110342 ) ) ;
#41080 = DIRECTION ( 'NONE',  ( -0.000000000000000000, -0.000000000000000000, -1.000000000000000000 ) ) ;
#41081 =( LENGTH_UNIT ( ) NAMED_UNIT ( * ) SI_UNIT ( .MILLI., .METRE. ) );
#41082 = CARTESIAN_POINT ( 'NONE',  ( 1.472469842513823179, 21.42559781766745175, 4.923371831947296329 ) ) ;
#41083 = MECHANICAL_DESIGN_GEOMETRIC_PRESENTATION_REPRESENTATION (  '', ( #79397 ), #92175 ) ;
#41084 = CARTESIAN_POINT ( 'NONE',  ( 10.00000000000000000, 26.81368534415484106, -10.88017736071110342 ) ) ;
#41085 = CARTESIAN_POINT ( 'NONE',  ( 13.43411237798105340, 0.5819680032637533085, 12.81628187352647963 ) ) ;
#41087 = FACE_OUTER_BOUND ( 'NONE', #69987, .T. ) ;
#41086 = CARTESIAN_POINT ( 'NONE',  ( 17.96484262340118221, 26.18868534415483396, -7.964842623401177768 ) ) ;
#41088 = CYLINDRICAL_SURFACE ( 'NONE', #80051, 0.2500000000000002220 ) ;
#41089 = CARTESIAN_POINT ( 'NONE',  ( 22.81628187352647785, 21.41530133659708923, 3.434112377981063169 ) ) ;
#41090 = EDGE_LOOP ( 'NONE', ( #34111, #18473, #12602, #45200 ) ) ;
#41091 = CARTESIAN_POINT ( 'NONE',  ( 7.084665262690076126, 52.02201867748816255, -10.88017736071110164 ) ) ;
#41092 = CARTESIAN_POINT ( 'NONE',  ( 10.00000000000000178, 37.25893115100078745, 9.846743663894594434 ) ) ;
#41094 = DIRECTION ( 'NONE',  ( -0.000000000000000000, -1.000000000000000000, -0.000000000000000000 ) ) ;
#41093 = CARTESIAN_POINT ( 'NONE',  ( 22.81628187352647785, 16.62363466993042138, 6.195893100308588602E-16 ) ) ;
#41095 = CARTESIAN_POINT ( 'NONE',  ( 0.5774900079438590739, 27.64701867748817676, -5.440088680355550821 ) ) ;
#41096 = CARTESIAN_POINT ( 'NONE',  ( 17.96484262340118221, 34.93868534415482685, 7.964842623401181321 ) ) ;
#41097 = CARTESIAN_POINT ( 'NONE',  ( 17.08211943468705840, 50.13708216824730357, -12.26659068614894466 ) ) ;
#41098 = AXIS2_PLACEMENT_3D ( 'NONE', #97115, #60062, #83572 ) ;
#41099 = CARTESIAN_POINT ( 'NONE',  ( 5.076628168052703671, 41.84226448433411605, 8.527530157486179263 ) ) ;
#41100 = CARTESIAN_POINT ( 'NONE',  ( 10.00000000000000000, 61.81368534415484106, -10.88017736071110342 ) ) ;
#41101 = CARTESIAN_POINT ( 'NONE',  ( 2.035157376598824452, 43.68868534415484106, 7.964842623401179544 ) ) ;
#41102 = DIRECTION ( 'NONE',  ( -0.000000000000000000, 1.000000000000000000, -0.000000000000000000 ) ) ;
#41103 = CARTESIAN_POINT ( 'NONE',  ( 6.204703633549690345, 12.84541550158063572, 14.16423886937410082 ) ) ;
#41104 = AXIS2_PLACEMENT_3D ( 'NONE', #24952, #33397, #3916 ) ;
#41105 = ADVANCED_FACE ( 'NONE', ( #84665 ), #8662, .T. ) ;
#41106 = CIRCLE ( 'NONE', #9182, 0.2500000000000002220 ) ;
#41107 = FILL_AREA_STYLE ('',( #10593 ) ) ;
#41108 = CARTESIAN_POINT ( 'NONE',  ( 0.000000000000000000, 0.5000000000000004441, 0.000000000000000000 ) ) ;
#41109 = AXIS2_PLACEMENT_3D ( 'NONE', #54001, #8508, #84993 ) ;
#41110 = ORIENTED_EDGE ( 'NONE', *, *, #16039, .T. ) ;
#41111 = ORIENTED_EDGE ( 'NONE', *, *, #72012, .T. ) ;
#41112 = CARTESIAN_POINT ( 'NONE',  ( -4.164238869374098151, 51.59541550158063217, -3.795296366450310543 ) ) ;
#41113 = CARTESIAN_POINT ( 'NONE',  ( 2.917880565312950480, 50.97041550158064638, -12.26659068614894821 ) ) ;
#41114 = CARTESIAN_POINT ( 'NONE',  ( 2.791683348922237240, 10.38393115100078390, -7.208316651077763204 ) ) ;
#41115 = CARTESIAN_POINT ( 'NONE',  ( 10.00000000000000000, 12.87363466993042138, -12.81628187352647608 ) ) ;
#41116 = CARTESIAN_POINT ( 'NONE',  ( 12.24319267753454099, 54.01141590572476048, 0.000000000000000000 ) ) ;
#41117 = CARTESIAN_POINT ( 'NONE',  ( 19.72487221294570858, 70.00000000000000000, -6.000000000000000000 ) ) ;
#41119 = CARTESIAN_POINT ( 'NONE',  ( -2.816281873526471635, 33.91530133659708213, -3.434112377981056508 ) ) ;
#41118 = CARTESIAN_POINT ( 'NONE',  ( 4.559911319644449179, 2.230352010821504471, -9.422509992056141925 ) ) ;
#41120 = CARTESIAN_POINT ( 'NONE',  ( -0.3689425029237881626, 42.42874883491396787, 10.36894250292379027 ) ) ;
#41121 = SURFACE_SIDE_STYLE ('',( #33580 ) ) ;
#41122 = FILL_AREA_STYLE_COLOUR ( '', #9063 ) ;
#41123 = CARTESIAN_POINT ( 'NONE',  ( 8.527530157486175710, 8.925597817667455303, -4.923371831947298993 ) ) ;
#41124 = EDGE_LOOP ( 'NONE', ( #75625, #92174, #16979, #41619 ) ) ;
#41125 = FACE_OUTER_BOUND ( 'NONE', #14831, .T. ) ;
#41126 = CARTESIAN_POINT ( 'NONE',  ( 14.92337183194729633, 22.67559781766745175, 8.527530157486181039 ) ) ;
#41127 = DIRECTION ( 'NONE',  ( 0.000000000000000000, 1.000000000000000000, 0.000000000000000000 ) ) ;
#41128 = ORIENTED_EDGE ( 'NONE', *, *, #47526, .F. ) ;
#41129 = CARTESIAN_POINT ( 'NONE',  ( -2.266590686148945544, 12.22041550158063394, 7.082119434687048631 ) ) ;
#41131 = CARTESIAN_POINT ( 'NONE',  ( 15.44008868035555260, 14.73035201082150536, 9.422509992056143702 ) ) ;
#41130 = CARTESIAN_POINT ( 'NONE',  ( 12.91533473730993009, 11.60535201082150714, -10.88017736071109987 ) ) ;
#41133 = CARTESIAN_POINT ( 'NONE',  ( 10.00000000000000000, -2.126365330069579951, -12.81628187352647608 ) ) ;
#41132 = CARTESIAN_POINT ( 'NONE',  ( 5.076628168052703671, 36.84226448433412315, 8.527530157486179263 ) ) ;
#41134 = LINE ( 'NONE', #57582, #37570 ) ;
#41135 = CARTESIAN_POINT ( 'NONE',  ( 12.25993886608605443, 15.00000000000000000, -8.642563219313617040 ) ) ;
#41136 =( BOUNDED_SURFACE ( )  B_SPLINE_SURFACE ( 1, 2, ( 
 ( #45561, #90561, #83070, #60060, #8066, #61047, #66586, #91560, #97113, #89579, #13585, #14089, #44572, #75069, #67586, #16553, #1564, #46541, #92527, #71029, #8555, #77042, #78516, #55530, #47027, #32013, #1067, #84553, #62516, #31531, #40032, #93021, #31037, #70534, #85040, #94010, #86522, #17046, #39056, #48008, #62027, #69550, #24055, #18020, #54524, #77519, #10030, #47525, #9035, #48502, #40531, #2056, #23574, #24557, #32518, #63016, #78028, #79005, #2552, #39552, #70042, #56024, #38562, #55016, #85533, #33009, #9530, #93517, #86026, #25532, #61538, #25044, #17541, #63508, #69058, #596, #92046, #54043, #16053, #87977, #57966, #34967, #49481, #65464, #96490, #27473, #88970, #19488, #87491, #26984, #88470, #71991, #19005, #42011, #34472, #19972, #49981, #94984, #72971, #27961, #79989, #80975, #64965, #11491, #42489, #95491, #4502, #57482, #20479, #3036, #56984, #95991, #72477, #63984, #71526, #79505, #41523, #33974, #94495, #11007, #3515, #65963, #35467, #50470, #4010, #80488, #11986, #12474, #50965, #64477, #41024, #33486, #58454, #48996, #42978, #26490, #73458, #4986, #10508, #18506, #26014, #56509, #87000, #67949, #98969, #22455, #13463, #59936, #43945, #35959, #28467, #74443, #98473, #66454, #13970, #90426, #21967, #52930, #74947, #89460, #68448, #5970, #36464, #21464, #81951, #44445, #66959, #96990, #29927, #97477, #51461, #52446, #73959, #58964, #20978, #82946, #12962, #75442, #60433, #75934, #28943, #59445, #37955, #83441, #89946, #14461, #6449, #44935, #51962, #82446, #7457, #6954, #36960, #67455, #30423, #43457, #60924, #97976, #90926, #29432, #37462, #14962, #45432, #91429, #22956, #81459, #5488, #39424, #16426, #39908, #77395, #8908, #84915, #9909, #32388, #2426, #1931, #32883, #85406, #9406, #15458, #16916, #30915, #46902, #31403, #69918, #61414, #8425, #85903, #23447, #91922, #93392, #70411, #61904, #1439, #15931, #467, #31891, #46422, #54891, #62388, #45939, #47392, #941, #40411, #63382, #92896, #53924, #62893, #76915, #84434, #38932, #93886, #69421, #92410, #24917, #24427, #23934, #53422, #55402, #77893, #38440, #17417, #47886, #78388, #70906, #83929, #76429, #7944, #68937, #54403, #11862, #95360, #34350, #42370, #63859, #27351, #87367, #49363, #87851, #41408, #64357, #49854, #25892, #41891, #80854, #25414, #65341, #4380, #19850, #17898, #73341, #26860, #72350, #33849, #57357, #55898, #95869, #19369, #18388, #94866, #56391, #78883, #42858, #26367, #65839, #86395, #94373, #11369, #56866, #57844, #48381, #86878, #88354, #18882, #79865, #64841, #3883, #80363, #50343, #72844, #48867, #34845, #4868, #10394 ),
 ( #12351, #79379, #35345, #10884, #40898, #71399, #71872, #3384, #2915, #33365, #50850, #35843, #74824, #27841, #90309, #44812, #90812, #28342, #74321, #52814, #98354, #58832, #67328, #21343, #5364, #5847, #14847, #75815, #43825, #36338, #67835, #82321, #89339, #75318, #83321, #20354, #66330, #6831, #66832, #45318, #22340, #97354, #28823, #89826, #6328, #37345, #21845, #59323, #52326, #7337, #14339, #37838, #36840, #51834, #13841, #29812, #20849, #44323, #97854, #29317, #60321, #59813, #81825, #82819, #96368, #58329, #88846, #81343, #12839, #43339, #73836, #96866, #51340, #13341, #60805, #15823, #54779, #831, #22833, #30303, #38326, #353, #91809, #53308, #68820, #30801, #24801, #93278, #77778, #38817, #39313, #92299, #69309, #78274, #23331, #98849, #91305, #55278, #7830, #1329, #53811, #61300, #70301, #84322, #76312, #9291, #46793, #31290, #46310, #76797, #85788, #1815, #8313, #69806, #23823, #61789, #54286, #17301, #47776, #84801, #16310, #39800, #77286, #8796, #16801, #9788, #83816, #31781, #47277, #62276, #68329, #15342, #92782, #24313, #85294, #32270, #62779, #45825, #79262, #64725, #27232, #57238, #19739, #49255, #18275, #56753, #87736, #2804, #48754, #71762, #64237, #19248, #18772, #25783, #3775, #57727, #10773, #11747, #94755, #41288, #72241, #26256, #34228, #87246, #50224, #32767, #86773, #26743, #3272, #93771, #2312, #10282, #71282, #63750, #25297, #40782, #33259, #95748, #65221, #49732, #33736, #11252, #79754, #41770, #80738, #94255, #70795, #63262, #88230, #78777, #95235, #56277, #80239, #42255, #72725, #48263, #4259, #34730, #40287, #55784, #86279, #17788, #43222, #89711, #73717, #65721, #58207, #5249, #29206, #96247, #43719, #21225, #51729, #82708, #5737, #20235, #98233, #35727, #66215, #51225, #12727, #74203, #96746, #27727, #59705, #28222, #81228, #82211, #4751, #88724, #50739, #13721, #42742, #6225, #90202, #6715, #58720, #29694, #81709, #52703, #12233, #89225, #97248, #20734, #52214, #35222, #13223, #75205, #36223, #44205, #66724, #28717, #37232, #74715, #59208, #36729, #60203, #73223, #90698, #67220, #21732, #97743, #14226, #44705, #67721, #22227, #55544, #62038, #32533, #70546, #47542, #71045, #9542, #40046, #17060, #41040, #63521, #33502, #33024, #64000, #17555, #40545, #45206, #48021, #92538, #78040, #62529, #2072, #24068, #39563, #18039, #54536, #85051, #25548, #2568, #93035, #63031, #47038, #31543, #93529, #77534, #86043, #25060, #75705, #78533, #32025, #71540, #94511, #10046, #16564, #94025, #9052, #70053, #1576, #26031, #24569, #55029, #56039, #86534, #85548, #83208, #48516, #79019, #68219, #10530 ) ),
 .UNSPECIFIED., .F., .F., .T. ) 
 B_SPLINE_SURFACE_WITH_KNOTS ( ( 2, 2 ),
 ( 3, 2, 2, 2, 2, 2, 2, 2, 2, 2, 2, 2, 2, 2, 2, 2, 2, 2, 2, 2, 2, 2, 2, 2, 2, 2, 2, 2, 2, 2, 2, 2, 2, 2, 2, 2, 2, 2, 2, 2, 2, 2, 2, 2, 2, 2, 2, 2, 2, 2, 2, 2, 2, 2, 2, 2, 2, 2, 2, 2, 2, 2, 2, 2, 2, 2, 2, 2, 2, 2, 2, 2, 2, 2, 2, 2, 2, 2, 2, 2, 2, 2, 2, 2, 2, 2, 2, 2, 2, 2, 2, 2, 2, 2, 2, 2, 2, 2, 2, 2, 2, 2, 2, 2, 2, 2, 2, 2, 2, 2, 2, 2, 2, 2, 2, 2, 2, 2, 2, 2, 2, 2, 2, 2, 2, 2, 2, 2, 2, 2, 2, 2, 2, 2, 2, 2, 2, 2, 2, 2, 2, 2, 2, 2, 2, 2, 2, 2, 2, 2, 2, 2, 2, 2, 2, 2, 2, 2, 2, 2, 2, 2, 3 ),
 ( 0.000000000000000000, 1.000000000000000000 ),
 ( 0.000000000000000000, 0.005952380952380952051, 0.01190476190476190410, 0.01785714285714285615, 0.02380952380952380820, 0.02976190476190476025, 0.03571428571428571230, 0.04166666666666666435, 0.04761904761904761640, 0.05357142857142856845, 0.05952380952380952051, 0.06547619047619047949, 0.07142857142857142461, 0.07738095238095238360, 0.08333333333333332871, 0.08928571428571428770, 0.09523809523809523281, 0.1011904761904761918, 0.1071428571428571369, 0.1130952380952380959, 0.1190476190476190410, 0.1250000000000000000, 0.1309523809523809590, 0.1369047619047619180, 0.1428571428571428492, 0.1488095238095238082, 0.1547619047619047672, 0.1607142857142857262, 0.1666666666666666574, 0.1726190476190476164, 0.1785714285714285754, 0.1845238095238095344, 0.1904761904761904656, 0.1964285714285714246, 0.2023809523809523836, 0.2083333333333333426, 0.2142857142857142738, 0.2202380952380952328, 0.2261904761904761918, 0.2321428571428571508, 0.2380952380952380820, 0.2440476190476190410, 0.2500000000000000000, 0.2559523809523809312, 0.2619047619047619180, 0.2678571428571428492, 0.2738095238095238360, 0.2797619047619047672, 0.2857142857142856984, 0.2916666666666666852, 0.2976190476190476164, 0.3035714285714285476, 0.3095238095238095344, 0.3154761904761904656, 0.3214285714285714524, 0.3273809523809523836, 0.3333333333333333148, 0.3392857142857143016, 0.3452380952380952328, 0.3511904761904761640, 0.3571428571428571508, 0.3630952380952380820, 0.3690476190476190688, 0.3750000000000000000, 0.3809523809523809312, 0.3869047619047619180, 0.3928571428571428492, 0.3988095238095238360, 0.4047619047619047672, 0.4107142857142856984, 0.4166666666666666852, 0.4226190476190476164, 0.4285714285714285476, 0.4345238095238095344, 0.4404761904761904656, 0.4464285714285714524, 0.4523809523809523836, 0.4583333333333333148, 0.4642857142857143016, 0.4702380952380952328, 0.4761904761904761640, 0.4821428571428571508, 0.4880952380952380820, 0.4940476190476190688, 0.5000000000000000000, 0.5059523809523809312, 0.5119047619047618625, 0.5178571428571429047, 0.5238095238095238360, 0.5297619047619047672, 0.5357142857142856984, 0.5416666666666666297, 0.5476190476190476719, 0.5535714285714286031, 0.5595238095238095344, 0.5654761904761904656, 0.5714285714285713969, 0.5773809523809523281, 0.5833333333333333703, 0.5892857142857143016, 0.5952380952380952328, 0.6011904761904761640, 0.6071428571428570953, 0.6130952380952381375, 0.6190476190476190688, 0.6250000000000000000, 0.6309523809523809312, 0.6369047619047618625, 0.6428571428571429047, 0.6488095238095238360, 0.6547619047619047672, 0.6607142857142856984, 0.6666666666666666297, 0.6726190476190476719, 0.6785714285714286031, 0.6845238095238095344, 0.6904761904761904656, 0.6964285714285713969, 0.7023809523809523281, 0.7083333333333333703, 0.7142857142857143016, 0.7202380952380952328, 0.7261904761904761640, 0.7321428571428570953, 0.7380952380952381375, 0.7440476190476190688, 0.7500000000000000000, 0.7559523809523809312, 0.7619047619047618625, 0.7678571428571429047, 0.7738095238095238360, 0.7797619047619047672, 0.7857142857142856984, 0.7916666666666666297, 0.7976190476190476719, 0.8035714285714286031, 0.8095238095238095344, 0.8154761904761904656, 0.8214285714285713969, 0.8273809523809523281, 0.8333333333333333703, 0.8392857142857143016, 0.8452380952380952328, 0.8511904761904761640, 0.8571428571428570953, 0.8630952380952381375, 0.8690476190476190688, 0.8750000000000000000, 0.8809523809523809312, 0.8869047619047618625, 0.8928571428571429047, 0.8988095238095238360, 0.9047619047619047672, 0.9107142857142856984, 0.9166666666666666297, 0.9226190476190476719, 0.9285714285714286031, 0.9345238095238095344, 0.9404761904761904656, 0.9464285714285713969, 0.9523809523809523281, 0.9583333333333333703, 0.9642857142857143016 ),
 .UNSPECIFIED. ) 
 GEOMETRIC_REPRESENTATION_ITEM ( )  RATIONAL_B_SPLINE_SURFACE ( (
 ( 1.000000000000000000, 0.9659258262890683122, 1.000000000000000000, 0.9659258262890683122, 1.000000000000000000, 0.9659258262890683122, 1.000000000000000000, 0.9659258262890683122, 1.000000000000000000, 0.9659258262890683122, 1.000000000000000000, 0.9659258262890683122, 1.000000000000000000, 0.9659258262890683122, 1.000000000000000000, 0.9659258262890683122, 1.000000000000000000, 0.9659258262890683122, 1.000000000000000000, 0.9659258262890683122, 1.000000000000000000, 0.9659258262890683122, 1.000000000000000000, 0.9659258262890683122, 1.000000000000000000, 0.9659258262890683122, 1.000000000000000000, 0.9659258262890683122, 1.000000000000000000, 0.9659258262890683122, 1.000000000000000000, 0.9659258262890683122, 1.000000000000000000, 0.9659258262890683122, 1.000000000000000000, 0.9659258262890683122, 1.000000000000000000, 0.9659258262890683122, 1.000000000000000000, 0.9659258262890683122, 1.000000000000000000, 0.9659258262890683122, 1.000000000000000000, 0.9659258262890683122, 1.000000000000000000, 0.9659258262890683122, 1.000000000000000000, 0.9659258262890683122, 1.000000000000000000, 0.9659258262890683122, 1.000000000000000000, 0.9659258262890683122, 1.000000000000000000, 0.9659258262890683122, 1.000000000000000000, 0.9659258262890683122, 1.000000000000000000, 0.9659258262890683122, 1.000000000000000000, 0.9659258262890683122, 1.000000000000000000, 0.9659258262890683122, 1.000000000000000000, 0.9659258262890683122, 1.000000000000000000, 0.9659258262890683122, 1.000000000000000000, 0.9659258262890683122, 1.000000000000000000, 0.9659258262890683122, 1.000000000000000000, 0.9659258262890683122, 1.000000000000000000, 0.9659258262890683122, 1.000000000000000000, 0.9659258262890683122, 1.000000000000000000, 0.9659258262890683122, 1.000000000000000000, 0.9659258262890683122, 1.000000000000000000, 0.9659258262890683122, 1.000000000000000000, 0.9659258262890683122, 1.000000000000000000, 0.9659258262890683122, 1.000000000000000000, 0.9659258262890683122, 1.000000000000000000, 0.9659258262890683122, 1.000000000000000000, 0.9659258262890683122, 1.000000000000000000, 0.9659258262890683122, 1.000000000000000000, 0.9659258262890683122, 1.000000000000000000, 0.9659258262890683122, 1.000000000000000000, 0.9659258262890683122, 1.000000000000000000, 0.9659258262890683122, 1.000000000000000000, 0.9659258262890683122, 1.000000000000000000, 0.9659258262890683122, 1.000000000000000000, 0.9659258262890683122, 1.000000000000000000, 0.9659258262890683122, 1.000000000000000000, 0.9659258262890683122, 1.000000000000000000, 0.9659258262890683122, 1.000000000000000000, 0.9659258262890683122, 1.000000000000000000, 0.9659258262890683122, 1.000000000000000000, 0.9659258262890683122, 1.000000000000000000, 0.9659258262890683122, 1.000000000000000000, 0.9659258262890683122, 1.000000000000000000, 0.9659258262890683122, 1.000000000000000000, 0.9659258262890683122, 1.000000000000000000, 0.9659258262890683122, 1.000000000000000000, 0.9659258262890683122, 1.000000000000000000, 0.9659258262890683122, 1.000000000000000000, 0.9659258262890683122, 1.000000000000000000, 0.9659258262890683122, 1.000000000000000000, 0.9659258262890683122, 1.000000000000000000, 0.9659258262890683122, 1.000000000000000000, 0.9659258262890683122, 1.000000000000000000, 0.9659258262890683122, 1.000000000000000000, 0.9659258262890683122, 1.000000000000000000, 0.9659258262890683122, 1.000000000000000000, 0.9659258262890683122, 1.000000000000000000, 0.9659258262890683122, 1.000000000000000000, 0.9659258262890683122, 1.000000000000000000, 0.9659258262890683122, 1.000000000000000000, 0.9659258262890683122, 1.000000000000000000, 0.9659258262890683122, 1.000000000000000000, 0.9659258262890683122, 1.000000000000000000, 0.9659258262890683122, 1.000000000000000000, 0.9659258262890683122, 1.000000000000000000, 0.9659258262890683122, 1.000000000000000000, 0.9659258262890683122, 1.000000000000000000, 0.9659258262890683122, 1.000000000000000000, 0.9659258262890683122, 1.000000000000000000, 0.9659258262890683122, 1.000000000000000000, 0.9659258262890683122, 1.000000000000000000, 0.9659258262890683122, 1.000000000000000000, 0.9659258262890683122, 1.000000000000000000, 0.9659258262890683122, 1.000000000000000000, 0.9659258262890683122, 1.000000000000000000, 0.9659258262890683122, 1.000000000000000000, 0.9659258262890683122, 1.000000000000000000, 0.9659258262890683122, 1.000000000000000000, 0.9659258262890683122, 1.000000000000000000, 0.9659258262890683122, 1.000000000000000000, 0.9659258262890683122, 1.000000000000000000, 0.9659258262890683122, 1.000000000000000000, 0.9659258262890683122, 1.000000000000000000, 0.9659258262890683122, 1.000000000000000000, 0.9659258262890683122, 1.000000000000000000, 0.9659258262890683122, 1.000000000000000000, 0.9659258262890683122, 1.000000000000000000, 0.9659258262890683122, 1.000000000000000000, 0.9659258262890683122, 1.000000000000000000, 0.9659258262890683122, 1.000000000000000000, 0.9659258262890683122, 1.000000000000000000, 0.9659258262890683122, 1.000000000000000000, 0.9659258262890683122, 1.000000000000000000, 0.9659258262890683122, 1.000000000000000000, 0.9659258262890683122, 1.000000000000000000, 0.9659258262890683122, 1.000000000000000000, 0.9659258262890683122, 1.000000000000000000, 0.9659258262890683122, 1.000000000000000000, 0.9659258262890683122, 1.000000000000000000, 0.9659258262890683122, 1.000000000000000000, 0.9659258262890683122, 1.000000000000000000, 0.9659258262890683122, 1.000000000000000000, 0.9659258262890683122, 1.000000000000000000, 0.9659258262890683122, 1.000000000000000000, 0.9659258262890683122, 1.000000000000000000, 0.9659258262890683122, 1.000000000000000000, 0.9659258262890683122, 1.000000000000000000, 0.9659258262890683122, 1.000000000000000000, 0.9659258262890683122, 1.000000000000000000, 0.9659258262890683122, 1.000000000000000000, 0.9659258262890683122, 1.000000000000000000, 0.9659258262890683122, 1.000000000000000000, 0.9659258262890683122, 1.000000000000000000, 0.9659258262890683122, 1.000000000000000000, 0.9659258262890683122, 1.000000000000000000, 0.9659258262890683122, 1.000000000000000000, 0.9659258262890683122, 1.000000000000000000, 0.9659258262890683122, 1.000000000000000000, 0.9659258262890683122, 1.000000000000000000, 0.9659258262890683122, 1.000000000000000000, 0.9659258262890683122, 1.000000000000000000, 0.9659258262890683122, 1.000000000000000000, 0.9659258262890683122, 1.000000000000000000, 0.9659258262890683122, 1.000000000000000000, 0.9659258262890683122, 1.000000000000000000, 0.9659258262890683122, 1.000000000000000000, 0.9659258262890683122, 1.000000000000000000, 0.9659258262890683122, 1.000000000000000000, 0.9659258262890683122, 1.000000000000000000, 0.9659258262890683122, 1.000000000000000000, 0.9659258262890683122, 1.000000000000000000, 0.9659258262890683122, 1.000000000000000000, 0.9659258262890683122, 1.000000000000000000, 0.9659258262890683122, 1.000000000000000000, 0.9659258262890683122, 1.000000000000000000, 0.9659258262890683122, 1.000000000000000000, 0.9659258262890683122, 1.000000000000000000, 0.9659258262890683122, 1.000000000000000000, 0.9659258262890683122, 1.000000000000000000, 0.9659258262890683122, 1.000000000000000000, 0.9659258262890683122, 1.000000000000000000, 0.9659258262890683122, 1.000000000000000000, 0.9659258262890683122, 1.000000000000000000),
 ( 1.000000000000000000, 0.9659258262890683122, 1.000000000000000000, 0.9659258262890683122, 1.000000000000000000, 0.9659258262890683122, 1.000000000000000000, 0.9659258262890683122, 1.000000000000000000, 0.9659258262890683122, 1.000000000000000000, 0.9659258262890683122, 1.000000000000000000, 0.9659258262890683122, 1.000000000000000000, 0.9659258262890683122, 1.000000000000000000, 0.9659258262890683122, 1.000000000000000000, 0.9659258262890683122, 1.000000000000000000, 0.9659258262890683122, 1.000000000000000000, 0.9659258262890683122, 1.000000000000000000, 0.9659258262890683122, 1.000000000000000000, 0.9659258262890683122, 1.000000000000000000, 0.9659258262890683122, 1.000000000000000000, 0.9659258262890683122, 1.000000000000000000, 0.9659258262890683122, 1.000000000000000000, 0.9659258262890683122, 1.000000000000000000, 0.9659258262890683122, 1.000000000000000000, 0.9659258262890683122, 1.000000000000000000, 0.9659258262890683122, 1.000000000000000000, 0.9659258262890683122, 1.000000000000000000, 0.9659258262890683122, 1.000000000000000000, 0.9659258262890683122, 1.000000000000000000, 0.9659258262890683122, 1.000000000000000000, 0.9659258262890683122, 1.000000000000000000, 0.9659258262890683122, 1.000000000000000000, 0.9659258262890683122, 1.000000000000000000, 0.9659258262890683122, 1.000000000000000000, 0.9659258262890683122, 1.000000000000000000, 0.9659258262890683122, 1.000000000000000000, 0.9659258262890683122, 1.000000000000000000, 0.9659258262890683122, 1.000000000000000000, 0.9659258262890683122, 1.000000000000000000, 0.9659258262890683122, 1.000000000000000000, 0.9659258262890683122, 1.000000000000000000, 0.9659258262890683122, 1.000000000000000000, 0.9659258262890683122, 1.000000000000000000, 0.9659258262890683122, 1.000000000000000000, 0.9659258262890683122, 1.000000000000000000, 0.9659258262890683122, 1.000000000000000000, 0.9659258262890683122, 1.000000000000000000, 0.9659258262890683122, 1.000000000000000000, 0.9659258262890683122, 1.000000000000000000, 0.9659258262890683122, 1.000000000000000000, 0.9659258262890683122, 1.000000000000000000, 0.9659258262890683122, 1.000000000000000000, 0.9659258262890683122, 1.000000000000000000, 0.9659258262890683122, 1.000000000000000000, 0.9659258262890683122, 1.000000000000000000, 0.9659258262890683122, 1.000000000000000000, 0.9659258262890683122, 1.000000000000000000, 0.9659258262890683122, 1.000000000000000000, 0.9659258262890683122, 1.000000000000000000, 0.9659258262890683122, 1.000000000000000000, 0.9659258262890683122, 1.000000000000000000, 0.9659258262890683122, 1.000000000000000000, 0.9659258262890683122, 1.000000000000000000, 0.9659258262890683122, 1.000000000000000000, 0.9659258262890683122, 1.000000000000000000, 0.9659258262890683122, 1.000000000000000000, 0.9659258262890683122, 1.000000000000000000, 0.9659258262890683122, 1.000000000000000000, 0.9659258262890683122, 1.000000000000000000, 0.9659258262890683122, 1.000000000000000000, 0.9659258262890683122, 1.000000000000000000, 0.9659258262890683122, 1.000000000000000000, 0.9659258262890683122, 1.000000000000000000, 0.9659258262890683122, 1.000000000000000000, 0.9659258262890683122, 1.000000000000000000, 0.9659258262890683122, 1.000000000000000000, 0.9659258262890683122, 1.000000000000000000, 0.9659258262890683122, 1.000000000000000000, 0.9659258262890683122, 1.000000000000000000, 0.9659258262890683122, 1.000000000000000000, 0.9659258262890683122, 1.000000000000000000, 0.9659258262890683122, 1.000000000000000000, 0.9659258262890683122, 1.000000000000000000, 0.9659258262890683122, 1.000000000000000000, 0.9659258262890683122, 1.000000000000000000, 0.9659258262890683122, 1.000000000000000000, 0.9659258262890683122, 1.000000000000000000, 0.9659258262890683122, 1.000000000000000000, 0.9659258262890683122, 1.000000000000000000, 0.9659258262890683122, 1.000000000000000000, 0.9659258262890683122, 1.000000000000000000, 0.9659258262890683122, 1.000000000000000000, 0.9659258262890683122, 1.000000000000000000, 0.9659258262890683122, 1.000000000000000000, 0.9659258262890683122, 1.000000000000000000, 0.9659258262890683122, 1.000000000000000000, 0.9659258262890683122, 1.000000000000000000, 0.9659258262890683122, 1.000000000000000000, 0.9659258262890683122, 1.000000000000000000, 0.9659258262890683122, 1.000000000000000000, 0.9659258262890683122, 1.000000000000000000, 0.9659258262890683122, 1.000000000000000000, 0.9659258262890683122, 1.000000000000000000, 0.9659258262890683122, 1.000000000000000000, 0.9659258262890683122, 1.000000000000000000, 0.9659258262890683122, 1.000000000000000000, 0.9659258262890683122, 1.000000000000000000, 0.9659258262890683122, 1.000000000000000000, 0.9659258262890683122, 1.000000000000000000, 0.9659258262890683122, 1.000000000000000000, 0.9659258262890683122, 1.000000000000000000, 0.9659258262890683122, 1.000000000000000000, 0.9659258262890683122, 1.000000000000000000, 0.9659258262890683122, 1.000000000000000000, 0.9659258262890683122, 1.000000000000000000, 0.9659258262890683122, 1.000000000000000000, 0.9659258262890683122, 1.000000000000000000, 0.9659258262890683122, 1.000000000000000000, 0.9659258262890683122, 1.000000000000000000, 0.9659258262890683122, 1.000000000000000000, 0.9659258262890683122, 1.000000000000000000, 0.9659258262890683122, 1.000000000000000000, 0.9659258262890683122, 1.000000000000000000, 0.9659258262890683122, 1.000000000000000000, 0.9659258262890683122, 1.000000000000000000, 0.9659258262890683122, 1.000000000000000000, 0.9659258262890683122, 1.000000000000000000, 0.9659258262890683122, 1.000000000000000000, 0.9659258262890683122, 1.000000000000000000, 0.9659258262890683122, 1.000000000000000000, 0.9659258262890683122, 1.000000000000000000, 0.9659258262890683122, 1.000000000000000000, 0.9659258262890683122, 1.000000000000000000, 0.9659258262890683122, 1.000000000000000000, 0.9659258262890683122, 1.000000000000000000, 0.9659258262890683122, 1.000000000000000000, 0.9659258262890683122, 1.000000000000000000, 0.9659258262890683122, 1.000000000000000000, 0.9659258262890683122, 1.000000000000000000, 0.9659258262890683122, 1.000000000000000000, 0.9659258262890683122, 1.000000000000000000, 0.9659258262890683122, 1.000000000000000000, 0.9659258262890683122, 1.000000000000000000, 0.9659258262890683122, 1.000000000000000000, 0.9659258262890683122, 1.000000000000000000, 0.9659258262890683122, 1.000000000000000000, 0.9659258262890683122, 1.000000000000000000, 0.9659258262890683122, 1.000000000000000000, 0.9659258262890683122, 1.000000000000000000, 0.9659258262890683122, 1.000000000000000000, 0.9659258262890683122, 1.000000000000000000, 0.9659258262890683122, 1.000000000000000000, 0.9659258262890683122, 1.000000000000000000, 0.9659258262890683122, 1.000000000000000000, 0.9659258262890683122, 1.000000000000000000, 0.9659258262890683122, 1.000000000000000000, 0.9659258262890683122, 1.000000000000000000, 0.9659258262890683122, 1.000000000000000000, 0.9659258262890683122, 1.000000000000000000, 0.9659258262890683122, 1.000000000000000000, 0.9659258262890683122, 1.000000000000000000, 0.9659258262890683122, 1.000000000000000000, 0.9659258262890683122, 1.000000000000000000, 0.9659258262890683122, 1.000000000000000000, 0.9659258262890683122, 1.000000000000000000, 0.9659258262890683122, 1.000000000000000000, 0.9659258262890683122, 1.000000000000000000) ) ) 
 REPRESENTATION_ITEM ( '' )  SURFACE ( )  );
#41137 = EDGE_CURVE ( 'NONE', #35809, #93854, #66521, .T. ) ;
#41138 = CARTESIAN_POINT ( 'NONE',  ( 19.38216949554541557, 22.24863466993041428, -9.382169495545420901 ) ) ;
#41139 = CARTESIAN_POINT ( 'NONE',  ( -11.09922568453594316, 29.54030133659710344, 6.408140936763246920 ) ) ;
#41140 = ORIENTED_EDGE ( 'NONE', *, *, #55529, .T. ) ;
#41141 = CARTESIAN_POINT ( 'NONE',  ( -4.164238869374098151, 46.59541550158063927, -3.795296366450310543 ) ) ;
#41142 = EDGE_LOOP ( 'NONE', ( #2634, #56059, #28458, #20230 ) ) ;
#41143 = CARTESIAN_POINT ( 'NONE',  ( 24.16423886937410614, 54.51208216824730357, -3.795296366450302550 ) ) ;
#41144 = ORIENTED_EDGE ( 'NONE', *, *, #18998, .F. ) ;
#41145 = CARTESIAN_POINT ( 'NONE',  ( 15.44008868035555260, 34.73035201082151247, 9.422509992056143702 ) ) ;
#41146 = CARTESIAN_POINT ( 'NONE',  ( 12.91533473730993009, 36.60535201082151247, -10.88017736071109987 ) ) ;
#41147 = CARTESIAN_POINT ( 'NONE',  ( 20.88017736071110875, 60.77201867748817676, -2.915334737309920765 ) ) ;
#41148 = CARTESIAN_POINT ( 'NONE',  ( 0.5774900079438590739, 22.64701867748817321, -5.440088680355550821 ) ) ;
#41149 = AXIS2_PLACEMENT_3D ( 'NONE', #18659, #41666, #11147 ) ;
#41152 = ORIENTED_EDGE ( 'NONE', *, *, #69551, .T. ) ;
#41151 = AXIS2_PLACEMENT_3D ( 'NONE', #27064, #56109, #35051 ) ;
#41150 = CARTESIAN_POINT ( 'NONE',  ( 0.000000000000000000, 35.00000000000000000, 0.000000000000000000 ) ) ;
#41153 = CARTESIAN_POINT ( 'NONE',  ( 0.1532563361054083140, 21.00893115100078745, 1.131784320476157264E-15 ) ) ;
#41154 = CARTESIAN_POINT ( 'NONE',  ( -5.068142462348440347, -24.94450071860939033, 2.749999999999193978 ) ) ;
#41155 = VERTEX_POINT ( 'NONE', #57595 ) ;
#41156 = CARTESIAN_POINT ( 'NONE',  ( 11.18123354730910002, -92.99280210684537451, 4.000000000000002665 ) ) ;
#41157 = CARTESIAN_POINT ( 'NONE',  ( 7.361572987183170547, 42.05059781766745886, 9.846743663894590881 ) ) ;
#41158 = CARTESIAN_POINT ( 'NONE',  ( 0.000000000000000000, 14.49999999999999822, 0.000000000000000000 ) ) ;
#41159 = CARTESIAN_POINT ( 'NONE',  ( 13.43411237798106583, 47.66530133659709634, -12.81628187352647252 ) ) ;
#41160 = CARTESIAN_POINT ( 'NONE',  ( -7.127794346849581686, -80.93619716733995517, 3.750000000000000444 ) ) ;
#41161 = VECTOR ( 'NONE', #75659, 1000.000000000000000 ) ;
#41162 = EDGE_CURVE ( 'NONE', #59403, #26337, #89085, .T. ) ;
#41163 = CARTESIAN_POINT ( 'NONE',  ( -46.34323875807881166, 103.6109741468810483, 6.190393423093142999 ) ) ;
#41164 = CARTESIAN_POINT ( 'NONE',  ( -45.36990007558824800, 104.5810639163623676, 5.619481386446134152 ) ) ;
#41165 = DIRECTION ( 'NONE',  ( 1.483861936729427615E-16, -1.000000000000000000, 0.000000000000000000 ) ) ;
#41166 = CARTESIAN_POINT ( 'NONE',  ( 2.917880565312950480, 50.97041550158064638, -12.26659068614894821 ) ) ;
#41167 = DIRECTION ( 'NONE',  ( 0.000000000000000000, 0.000000000000000000, 1.000000000000000000 ) ) ;
#41168 = EDGE_LOOP ( 'NONE', ( #38272, #79485, #5621, #47385 ) ) ;
#41169 =( LENGTH_UNIT ( ) NAMED_UNIT ( * ) SI_UNIT ( .MILLI., .METRE. ) );
#41170 = CARTESIAN_POINT ( 'NONE',  ( 18.52753015748618282, 38.92559781766745175, -4.923371831947291888 ) ) ;
#41171 =( LENGTH_UNIT ( ) NAMED_UNIT ( * ) SI_UNIT ( .MILLI., .METRE. ) );
#41172 = CARTESIAN_POINT ( 'NONE',  ( 0.6178305044545838731, 9.748634669930416052, 9.382169495545420901 ) ) ;
#41174 = ADVANCED_FACE ( 'NONE', ( #34100 ), #27593, .T. ) ;
#41173 = CARTESIAN_POINT ( 'NONE',  ( 18.52753015748618282, 3.925597817667451306, -4.923371831947291888 ) ) ;
#41175 = VECTOR ( 'NONE', #37144, 1000.000000000000000 ) ;
#41176 = CARTESIAN_POINT ( 'NONE',  ( -2.283843307429720415, 13.12729635533385597, -9.500000000000000000 ) ) ;
#41177 = CARTESIAN_POINT ( 'NONE',  ( 10.00000000000000178, 57.25893115100078745, 9.846743663894594434 ) ) ;
#41178 = LINE ( 'NONE', #72134, #28106 ) ;
#41179 = ORIENTED_EDGE ( 'NONE', *, *, #213, .T. ) ;
#41180 = CARTESIAN_POINT ( 'NONE',  ( 2.917880565312948704, 57.63708216824731068, 12.26659068614894643 ) ) ;
#41181 = FACE_OUTER_BOUND ( 'NONE', #19102, .T. ) ;
#41182 = CARTESIAN_POINT ( 'NONE',  ( -0.8801773607110991993, 37.85535201082151247, -2.915334737309923874 ) ) ;
#41184 = FACE_OUTER_BOUND ( 'NONE', #8677, .T. ) ;
#41183 = CARTESIAN_POINT ( 'NONE',  ( -1.099225684535947600, 18.70696800326375353, -6.408140936763238038 ) ) ;
#41185 = CARTESIAN_POINT ( 'NONE',  ( 0.000000000000000000, 84.07179676972448590, -4.000000000000000000 ) ) ;
#41186 = ADVANCED_FACE ( 'NONE', ( #66080 ), #96108, .T. ) ;
#41187 = CARTESIAN_POINT ( 'NONE',  ( 2.174473938468991285, 0.000000000000000000, -5.000947681547184942 ) ) ;
#41188 = DIRECTION ( 'NONE',  ( 0.000000000000000000, 0.000000000000000000, 1.000000000000000000 ) ) ;
#41189 = CARTESIAN_POINT ( 'NONE',  ( 14.92337183194729633, 47.67559781766745175, 8.527530157486181039 ) ) ;
#41190 = CARTESIAN_POINT ( 'NONE',  ( 2.791683348922240793, 1.633931151000784565, 7.208316651077764092 ) ) ;
#41191 = CARTESIAN_POINT ( 'NONE',  ( 10.36894250292378850, 29.92874883491397853, -10.36894250292379027 ) ) ;
#41192 = CARTESIAN_POINT ( 'NONE',  ( 16.40814093676323893, 5.790301336597087456, 11.09922568453595026 ) ) ;
#41193 = CARTESIAN_POINT ( 'NONE',  ( -11.30180206635974116, -57.06075279890724516, -4.000000000003605116 ) ) ;
#41195 = DIRECTION ( 'NONE',  ( 1.000000000000000000, -1.355252715606880851E-17, 0.000000000000000000 ) ) ;
#41194 = CARTESIAN_POINT ( 'NONE',  ( 19.42250999205614193, 25.14701867748817321, 5.440088680355555262 ) ) ;
#41196 = DIRECTION ( 'NONE',  ( 1.000000000000000000, 1.927470528863119542E-16, -0.000000000000000000 ) ) ;
#41197 = CARTESIAN_POINT ( 'NONE',  ( -2.266590686148945544, 32.22041550158063927, 7.082119434687048631 ) ) ;
#41198 = CARTESIAN_POINT ( 'NONE',  ( -4.164238869374099039, 26.80374883491397142, 8.674139862899312516E-16 ) ) ;
#41199 = CARTESIAN_POINT ( 'NONE',  ( -0.8801773607110991993, 12.85535201082150358, -2.915334737309923874 ) ) ;
#41200 = CARTESIAN_POINT ( 'NONE',  ( 19.84674366389459266, 43.30059781766744464, 2.638427012816836559 ) ) ;
#41201 = CARTESIAN_POINT ( 'NONE',  ( 16.40814093676324603, 37.45696800326376064, -11.09922568453594671 ) ) ;
#41202 = CARTESIAN_POINT ( 'NONE',  ( 19.42250999205614193, 15.14701867748817143, 5.440088680355555262 ) ) ;
#41203 = ORIENTED_EDGE ( 'NONE', *, *, #7259, .T. ) ;
#41204 = CARTESIAN_POINT ( 'NONE',  ( 19.84674366389459266, 38.30059781766745175, 2.638427012816836559 ) ) ;
#41205 = CARTESIAN_POINT ( 'NONE',  ( 15.44008868035555260, 34.73035201082151247, 9.422509992056143702 ) ) ;
#41206 = CARTESIAN_POINT ( 'NONE',  ( 13.43411237798106583, 2.665301336597086568, -12.81628187352647252 ) ) ;
#41208 = CARTESIAN_POINT ( 'NONE',  ( -0.3289641300568009741, 17.24545670184113888, -5.963430220938281678 ) ) ;
#41207 = CARTESIAN_POINT ( 'NONE',  ( -0.3689425029237881626, 22.42874883491397142, 10.36894250292379027 ) ) ;
#41209 = FACE_OUTER_BOUND ( 'NONE', #34197, .T. ) ;
#41210 = UNCERTAINTY_MEASURE_WITH_UNIT (LENGTH_MEASURE( 1.000000000000000082E-05 ), #45625, 'distance_accuracy_value', 'NONE');
#41211 =( BOUNDED_SURFACE ( )  B_SPLINE_SURFACE ( 3, 2, ( 
 ( #78927, #49897, #2471 ),
 ( #72393, #11411, #95912 ),
 ( #93934, #33407, #57883 ),
 ( #33893, #3434, #3922 ),
 ( #25458, #94907, #88397 ),
 ( #10924, #64398, #26406 ),
 ( #80406, #56906, #95406 ),
 ( #87409, #42410, #40452 ),
 ( #18926, #63905, #49402 ),
 ( #71442, #86440, #34392 ),
 ( #26903, #17940, #57399 ),
 ( #72889, #48424, #47926 ),
 ( #78432, #9949, #2956 ),
 ( #94416, #86920, #18431 ),
 ( #48914, #60354, #28385 ),
 ( #90347, #12880, #82868 ),
 ( #97899, #21885, #80897 ),
 ( #58877, #20399, #73380 ),
 ( #89379, #19894, #50387 ),
 ( #13381, #12393, #43378 ),
 ( #36880, #97393, #52363 ),
 ( #42898, #20892, #35387 ) ),
 .UNSPECIFIED., .F., .F., .F. ) 
 B_SPLINE_SURFACE_WITH_KNOTS ( ( 4, 2, 2, 2, 2, 2, 2, 2, 2, 2, 4 ),
 ( 3, 3 ),
 ( -1.040834085586084257E-17, 0.002788823349942579858, 0.005577646699885170124, 0.01115529339977035066, 0.02231058679954071172, 0.03346588019931107105, 0.04462117359908143038, 0.06693176039862215598, 0.07808705379839250837, 0.08366470049827769151, 0.08924234719816287464 ),
 ( 0.000000000000000000, 1.000000000000000000 ),
 .UNSPECIFIED. ) 
 GEOMETRIC_REPRESENTATION_ITEM ( )  RATIONAL_B_SPLINE_SURFACE ( (
 ( 1.000000000000000000, 0.7071067811865475727, 1.000000000000000000),
 ( 1.000000000000000000, 0.7071067811865475727, 1.000000000000000000),
 ( 1.000000000000000000, 0.7071067811865469066, 1.000000000000000000),
 ( 1.000000000000000000, 0.7071067811865469066, 1.000000000000000000),
 ( 1.000000000000000000, 0.7071067811865482389, 1.000000000000000000),
 ( 1.000000000000000000, 0.7071067811865482389, 1.000000000000000000),
 ( 1.000000000000000000, 0.7071067811865487940, 1.000000000000000000),
 ( 1.000000000000000000, 0.7071067811865487940, 1.000000000000000000),
 ( 1.000000000000000000, 0.7071067811865482389, 1.000000000000000000),
 ( 1.000000000000000000, 0.7071067811865482389, 1.000000000000000000),
 ( 1.000000000000000000, 0.7071067811865493491, 1.000000000000000000),
 ( 1.000000000000000000, 0.7071067811865493491, 1.000000000000000000),
 ( 1.000000000000000000, 0.7071067811865473507, 1.000000000000000000),
 ( 1.000000000000000000, 0.7071067811865473507, 1.000000000000000000),
 ( 1.000000000000000000, 0.7071067811865482389, 1.000000000000000000),
 ( 1.000000000000000000, 0.7071067811865482389, 1.000000000000000000),
 ( 1.000000000000000000, 0.7071067811865482389, 1.000000000000000000),
 ( 1.000000000000000000, 0.7071067811865482389, 1.000000000000000000),
 ( 1.000000000000000000, 0.7071067811865482389, 1.000000000000000000),
 ( 1.000000000000000000, 0.7071067811865482389, 1.000000000000000000),
 ( 1.000000000000000000, 0.7071067811865482389, 1.000000000000000000),
 ( 1.000000000000000000, 0.7071067811865482389, 1.000000000000000000) ) ) 
 REPRESENTATION_ITEM ( '' )  SURFACE ( )  );
#41212 = CARTESIAN_POINT ( 'NONE',  ( 19.84674366389459266, 23.30059781766745530, 2.638427012816836559 ) ) ;
#41213 = CARTESIAN_POINT ( 'NONE',  ( 19.38216949554541557, 57.24863466993042493, -9.382169495545420901 ) ) ;
#41214 = CARTESIAN_POINT ( 'NONE',  ( 19.84674366389459621, 53.50893115100078745, 7.409399052514197653E-17 ) ) ;
#41215 = ORIENTED_EDGE ( 'NONE', *, *, #84673, .T. ) ;
#41216 = CARTESIAN_POINT ( 'NONE',  ( 8.955816604300867567, -3.107613341155669229, -4.000000000000000000 ) ) ;
#41217 = SURFACE_STYLE_USAGE ( .BOTH. , #63681 ) ;
#41218 = CARTESIAN_POINT ( 'NONE',  ( 22.26659068614894466, 63.88708216824730357, 7.082119434687054849 ) ) ;
#41219 = CARTESIAN_POINT ( 'NONE',  ( 24.16423886937410614, 9.303748834913967869, 8.672049930838204340E-16 ) ) ;
#41220 = CARTESIAN_POINT ( 'NONE',  ( 14.92337183194729633, 2.675597817667451750, 8.527530157486181039 ) ) ;
#41221 = CARTESIAN_POINT ( 'NONE',  ( 19.84674366389459621, 48.50893115100078745, 7.409399052514197653E-17 ) ) ;
#41222 = CARTESIAN_POINT ( 'NONE',  ( 4.559911319644449179, 18.89701867748817321, 9.422509992056141925 ) ) ;
#41223 = CARTESIAN_POINT ( 'NONE',  ( 19.72487221294571569, 39.78217586085237656, 6.499999999999986677 ) ) ;
#41224 = CARTESIAN_POINT ( 'NONE',  ( 19.10478245763068372, 25.10160829253888792, 5.990408912944043429 ) ) ;
#41225 = EDGE_CURVE ( 'NONE', #50127, #70139, #96608, .T. ) ;
#41226 = ORIENTED_EDGE ( 'NONE', *, *, #5652, .T. ) ;
#41227 = DIRECTION ( 'NONE',  ( -0.000000000000000000, 0.000000000000000000, 1.000000000000000000 ) ) ;
#41228 = ORIENTED_EDGE ( 'NONE', *, *, #39383, .F. ) ;
#41229 = ORIENTED_EDGE ( 'NONE', *, *, #76441, .F. ) ;
#41230 = DIRECTION ( 'NONE',  ( 0.000000000000000000, 0.000000000000000000, 1.000000000000000000 ) ) ;
#41231 = CARTESIAN_POINT ( 'NONE',  ( 20.36894250292379738, 4.928748834913967869, -10.36894250292379027 ) ) ;
#41232 = CARTESIAN_POINT ( 'NONE',  ( -11.81797300553251162, -43.76346696326814367, 3.750000000000000000 ) ) ;
#41233 = CARTESIAN_POINT ( 'NONE',  ( 17.08211943468705130, 43.47041550158063927, 12.26659068614894998 ) ) ;
#41234 = CARTESIAN_POINT ( 'NONE',  ( 12.63842701281683922, 59.55059781766744464, -9.846743663894590881 ) ) ;
#41235 = CARTESIAN_POINT ( 'NONE',  ( 14.92337183194729988, 34.34226448433411605, -8.527530157486177487 ) ) ;
#41237 = CARTESIAN_POINT ( 'NONE',  ( 0.1532563361054083140, 61.00893115100078745, 1.131784320476157264E-15 ) ) ;
#41236 = CARTESIAN_POINT ( 'NONE',  ( -0.8801773607110991993, 37.85535201082151247, -2.915334737309923874 ) ) ;
#41238 = CARTESIAN_POINT ( 'NONE',  ( 17.08211943468705840, 10.13708216824730179, -12.26659068614894466 ) ) ;
#41239 = EDGE_CURVE ( 'NONE', #22085, #74593, #84089, .T. ) ;
#41240 = CARTESIAN_POINT ( 'NONE',  ( 13.79529636645031943, 40.34541550158063217, -14.16423886937409904 ) ) ;
#41241 = CARTESIAN_POINT ( 'NONE',  ( -0.8801773607110991993, 7.855352010821506248, -2.915334737309923874 ) ) ;
#41242 = DIRECTION ( 'NONE',  ( -0.000000000000000000, -1.000000000000000000, -0.000000000000000000 ) ) ;
#41243 = DIRECTION ( 'NONE',  ( 1.000000000000000000, -5.551115123125777653E-14, 0.000000000000000000 ) ) ;
#41244 = CARTESIAN_POINT ( 'NONE',  ( 17.96484262340118221, 64.93868534415483396, 7.964842623401181321 ) ) ;
#41245 = B_SPLINE_CURVE_WITH_KNOTS ( 'NONE', 3,
 ( #86929, #56918, #42912, #49912, #56443, #72407 ),
 .UNSPECIFIED., .F., .F.,
 ( 4, 2, 4 ),
 ( 0.0002800267093156154179, 0.0006862322000234324405, 0.001092437690731249463 ),
 .UNSPECIFIED. ) ;
#41246 = CARTESIAN_POINT ( 'NONE',  ( 14.92337183194729633, 32.67559781766745175, 8.527530157486181039 ) ) ;
#41247 =( GEOMETRIC_REPRESENTATION_CONTEXT ( 3 ) GLOBAL_UNCERTAINTY_ASSIGNED_CONTEXT ( ( #43145 ) ) GLOBAL_UNIT_ASSIGNED_CONTEXT ( ( #7920, #75415, #91899 ) ) REPRESENTATION_CONTEXT ( 'NONE', 'WORKASPACE' ) );
#41248 = CARTESIAN_POINT ( 'NONE',  ( -7.124934413296625912, -78.83349193436581004, 3.750000000000000888 ) ) ;
#41249 = ORIENTED_EDGE ( 'NONE', *, *, #24332, .F. ) ;
#41250 = DIRECTION ( 'NONE',  ( 0.8788171126619646056, 0.000000000000000000, 0.4771587602596096267 ) ) ;
#41251 = ORIENTED_EDGE ( 'NONE', *, *, #20881, .T. ) ;
#41252 = EDGE_CURVE ( 'NONE', #95502, #59148, #26611, .T. ) ;
#41253 = CARTESIAN_POINT ( 'NONE',  ( 12.63842701281683922, 24.55059781766745175, -9.846743663894590881 ) ) ;
#41254 = EDGE_LOOP ( 'NONE', ( #1198, #44048, #67777, #97189, #98826, #29550 ) ) ;
#41255 = CARTESIAN_POINT ( 'NONE',  ( -2.266590686148945544, 27.22041550158063572, 7.082119434687048631 ) ) ;
#41256 = CARTESIAN_POINT ( 'NONE',  ( 19.84674366389459266, 28.30059781766745886, 2.638427012816836559 ) ) ;
#41257 = CARTESIAN_POINT ( 'NONE',  ( 20.88017736071110164, 60.35535201082151957, 2.915334737309930979 ) ) ;
#41258 = VECTOR ( 'NONE', #27788, 1000.000000000000000 ) ;
#41259 = CIRCLE ( 'NONE', #4554, 4.190000000000001279 ) ;
#41260 = CARTESIAN_POINT ( 'NONE',  ( 20.88017736071110875, 40.77201867748818387, -2.915334737309920765 ) ) ;
#41261 = CARTESIAN_POINT ( 'NONE',  ( 14.99847009497948136, 0.3639309181704115104, 0.2142307401081242346 ) ) ;
#41262 = EDGE_CURVE ( 'NONE', #72885, #27580, #39120, .T. ) ;
#41263 = CARTESIAN_POINT ( 'NONE',  ( 9.382169495545419124, -4.001365330069578619, 9.382169495545417348 ) ) ;
#41264 = EDGE_LOOP ( 'NONE', ( #94006, #38084, #43309, #26838, #18515, #15798, #17928, #36163, #17384, #33030 ) ) ;
#41265 = CARTESIAN_POINT ( 'NONE',  ( 19.42250999205614548, 45.98035201082150536, -5.440088680355545492 ) ) ;
#41266 = CARTESIAN_POINT ( 'NONE',  ( 10.00000000000000000, 5.553748834913967869, -14.16423886937410082 ) ) ;
#41267 = EDGE_CURVE ( 'NONE', #30783, #98547, #29528, .T. ) ;
#41268 = ORIENTED_EDGE ( 'NONE', *, *, #48609, .F. ) ;
#41269 = CARTESIAN_POINT ( 'NONE',  ( 7.361572987183170547, 2.050597817667451750, 9.846743663894590881 ) ) ;
#41270 = CARTESIAN_POINT ( 'NONE',  ( -1.099225684535947600, 33.70696800326375353, -6.408140936763238038 ) ) ;
#41271 = CARTESIAN_POINT ( 'NONE',  ( 12.63842701281683034, 22.46726448433411605, 9.846743663894596210 ) ) ;
#41272 = CARTESIAN_POINT ( 'NONE',  ( 10.00000000000000178, 4.313685344154837509, 10.88017736071110342 ) ) ;
#41273 = FACE_OUTER_BOUND ( 'NONE', #11336, .T. ) ;
#41274 = CARTESIAN_POINT ( 'NONE',  ( 7.361572987183169658, 24.96726448433412315, -9.846743663894592657 ) ) ;
#41275 = CARTESIAN_POINT ( 'NONE',  ( 0.5774900079438590739, 62.64701867748817676, -5.440088680355550821 ) ) ;
#41276 = CARTESIAN_POINT ( 'NONE',  ( -8.209432707284950226, 15.00000000000000000, 12.55409154915480485 ) ) ;
#41277 = CARTESIAN_POINT ( 'NONE',  ( 10.00000000000000178, 64.31368534415483396, 10.88017736071110342 ) ) ;
#41278 = CARTESIAN_POINT ( 'NONE',  ( -1.499999999999998890, 21.83999999999999986, 0.000000000000000000 ) ) ;
#41279 = DIRECTION ( 'NONE',  ( 0.000000000000000000, 0.000000000000000000, -1.000000000000000000 ) ) ;
#41280 = CARTESIAN_POINT ( 'NONE',  ( 1.472469842513823179, 1.425597817667451528, 4.923371831947296329 ) ) ;
#41281 = CARTESIAN_POINT ( 'NONE',  ( 6.565887622018943937, 15.16530133659708568, 12.81628187352647430 ) ) ;
#41282 = DIRECTION ( 'NONE',  ( -0.5372996083468249973, 0.000000000000000000, 0.8433914458128849434 ) ) ;
#41283 = MANIFOLD_SOLID_BREP ( 'Fillet3', #34588 ) ;
#41284 = CARTESIAN_POINT ( 'NONE',  ( 18.52753015748618282, 48.92559781766745886, -4.923371831947291888 ) ) ;
#41285 = CARTESIAN_POINT ( 'NONE',  ( 14.02068044289375415, 15.00000000000000000, 5.331089937175756965 ) ) ;
#41286 = CARTESIAN_POINT ( 'NONE',  ( 6.204703633549690345, 10.76208216824729824, -14.16423886937410259 ) ) ;
#41287 = CARTESIAN_POINT ( 'NONE',  ( 12.63842701281683034, 27.46726448433411250, 9.846743663894596210 ) ) ;
#41288 = CARTESIAN_POINT ( 'NONE',  ( 19.38216949554541202, 30.99863466993042138, 9.382169495545424454 ) ) ;
#41290 = CYLINDRICAL_SURFACE ( 'NONE', #3328, 0.5000000000000004441 ) ;
#41289 = DIRECTION ( 'NONE',  ( 0.000000000000000000, 1.000000000000000000, 0.000000000000000000 ) ) ;
#41291 = CARTESIAN_POINT ( 'NONE',  ( 15.44008868035555260, 49.73035201082150536, 9.422509992056143702 ) ) ;
#41292 = CARTESIAN_POINT ( 'NONE',  ( 22.81628187352647785, 6.415301336597088344, 3.434112377981063169 ) ) ;
#41293 = CARTESIAN_POINT ( 'NONE',  ( 9.876730923139305673, 0.3640475087720985714, -11.28938378619063343 ) ) ;
#41294 = CARTESIAN_POINT ( 'NONE',  ( 1.472469842513823179, 20.59226448433411960, -4.923371831947296329 ) ) ;
#41296 = EDGE_CURVE ( 'NONE', #61288, #52968, #93447, .T. ) ;
#41295 = CARTESIAN_POINT ( 'NONE',  ( 19.42250999205614548, 25.98035201082150891, -5.440088680355545492 ) ) ;
#41297 = CARTESIAN_POINT ( 'NONE',  ( 0.6178305044545818747, 28.49863466993041783, -9.382169495545419124 ) ) ;
#41298 = AXIS2_PLACEMENT_3D ( 'NONE', #30392, #15905, #76883 ) ;
#41299 = CARTESIAN_POINT ( 'NONE',  ( 12.63842701281683034, 17.46726448433411250, 9.846743663894596210 ) ) ;
#41300 = SURFACE_STYLE_USAGE ( .BOTH. , #48274 ) ;
#41301 = CARTESIAN_POINT ( 'NONE',  ( -8.443706647342963834, 87.03308080853030049, 4.556631258847859911 ) ) ;
#41302 = CARTESIAN_POINT ( 'NONE',  ( 20.88017736071110875, 30.77201867748816966, -2.915334737309920765 ) ) ;
#41303 = ORIENTED_EDGE ( 'NONE', *, *, #16597, .T. ) ;
#41304 = CARTESIAN_POINT ( 'NONE',  ( 17.96484262340118221, 54.93868534415484106, 7.964842623401181321 ) ) ;
#41305 = CARTESIAN_POINT ( 'NONE',  ( 7.084665262690076126, 2.022018677488170990, -10.88017736071110164 ) ) ;
#41307 = CARTESIAN_POINT ( 'NONE',  ( -0.8801773607111008646, 28.27201867748817321, 2.915334737309923430 ) ) ;
#41306 = CARTESIAN_POINT ( 'NONE',  ( 17.20831665107776587, 44.13393115100078745, -7.208316651077762316 ) ) ;
#41308 = SURFACE_STYLE_FILL_AREA ( #25318 ) ;
#41309 = CARTESIAN_POINT ( 'NONE',  ( -0.8801773607110991993, 47.85535201082150536, -2.915334737309923874 ) ) ;
#41310 = COLOUR_RGB ( '', 0.72549020, 0.75294118, 0.79215686) ;
#41312 = CARTESIAN_POINT ( 'NONE',  ( -1.926860441876563801, 19.89664270246084143, 3.195792623639529761 ) ) ;
#41311 = CARTESIAN_POINT ( 'NONE',  ( 20.88017736071110875, 10.77201867748817143, -2.915334737309920765 ) ) ;
#41313 = CARTESIAN_POINT ( 'NONE',  ( 1.683889348827612823E-15, 15.00000000000000000, -13.75000000000001776 ) ) ;
#41314 = CARTESIAN_POINT ( 'NONE',  ( 1.472469842513823179, 41.42559781766745886, 4.923371831947296329 ) ) ;
#41316 = CARTESIAN_POINT ( 'NONE',  ( 1.707155281725170060, 47.90189080397283306, 6.499999999999919176 ) ) ;
#41315 = CARTESIAN_POINT ( 'NONE',  ( 24.16423886937409904, 44.09541550158063927, 3.795296366450317205 ) ) ;
#41317 = CARTESIAN_POINT ( 'NONE',  ( 2.377183314879974585, 5.785933195168225573, -6.499999999999999112 ) ) ;
#41319 = DIRECTION ( 'NONE',  ( -0.000000000000000000, -0.000000000000000000, -1.000000000000000000 ) ) ;
#41318 =( GEOMETRIC_REPRESENTATION_CONTEXT ( 3 ) GLOBAL_UNCERTAINTY_ASSIGNED_CONTEXT ( ( #95302 ) ) GLOBAL_UNIT_ASSIGNED_CONTEXT ( ( #16146, #93116, #9631 ) ) REPRESENTATION_CONTEXT ( 'NONE', 'WORKASPACE' ) );
#41320 = VECTOR ( 'NONE', #50941, 1000.000000000000000 ) ;
#41321 = CARTESIAN_POINT ( 'NONE',  ( 6.204703633549690345, 30.76208216824730357, -14.16423886937410259 ) ) ;
#41322 = DIRECTION ( 'NONE',  ( -0.000000000000000000, -1.000000000000000000, -0.000000000000000000 ) ) ;
#41323 = ORIENTED_EDGE ( 'NONE', *, *, #39775, .F. ) ;
#41324 = CARTESIAN_POINT ( 'NONE',  ( 6.204703633549690345, 67.84541550158060375, 14.16423886937410082 ) ) ;
#41325 = CARTESIAN_POINT ( 'NONE',  ( 2.791683348922237240, 40.38393115100078035, -7.208316651077763204 ) ) ;
#41327 = CARTESIAN_POINT ( 'NONE',  ( -9.093709202272499681, 88.10000367580643399, -5.077063215882387404 ) ) ;
#41326 = DIRECTION ( 'NONE',  ( 0.6038238647437471629, -0.7971177707001175783, -1.734723475976782837E-15 ) ) ;
#41328 = CARTESIAN_POINT ( 'NONE',  ( 20.88017736071110519, 60.56368534415484106, 2.639326808657452039E-16 ) ) ;
#41329 = CARTESIAN_POINT ( 'NONE',  ( 3.591859063236763294, 63.29030133659708923, -11.09922568453595026 ) ) ;
#41330 = CARTESIAN_POINT ( 'NONE',  ( 0.5774900079438590739, 32.64701867748816966, -5.440088680355550821 ) ) ;
#41331 = ADVANCED_FACE ( 'NONE', ( #67079 ), #45058, .T. ) ;
#41332 = CARTESIAN_POINT ( 'NONE',  ( 19.38216949554541557, 57.24863466993042493, -9.382169495545420901 ) ) ;
#41333 = CARTESIAN_POINT ( 'NONE',  ( 3.591859063236763294, 8.290301336597087456, -11.09922568453595026 ) ) ;
#41334 = CARTESIAN_POINT ( 'NONE',  ( 19.84674366389459621, 18.50893115100078745, 7.409399052514197653E-17 ) ) ;
#41335 = ORIENTED_EDGE ( 'NONE', *, *, #12845, .T. ) ;
#41336 = SURFACE_STYLE_USAGE ( .BOTH. , #4794 ) ;
#41337 = CARTESIAN_POINT ( 'NONE',  ( 0.1957200283969102450, 20.25733960839543712, 6.499999999999992006 ) ) ;
#41338 = CARTESIAN_POINT ( 'NONE',  ( 15.44008868035555260, 4.730352010821505360, 9.422509992056143702 ) ) ;
#41339 = CARTESIAN_POINT ( 'NONE',  ( -4.164238869374099039, 31.80374883491396432, 8.674139862899312516E-16 ) ) ;
#41340 = CARTESIAN_POINT ( 'NONE',  ( 12.91533473730992121, 29.52201867748817321, 10.88017736071110164 ) ) ;
#41341 = CARTESIAN_POINT ( 'NONE',  ( 7.084665262690076126, 49.10535201082149825, 10.88017736071109987 ) ) ;
#41342 = CARTESIAN_POINT ( 'NONE',  ( -12.87890026492945239, 0.04922511925147124434, 7.195834080858260151 ) ) ;
#41343 = CARTESIAN_POINT ( 'NONE',  ( -7.618485323809105481, 1.609362599783170644E-16, -12.48587314215772892 ) ) ;
#41344 = AXIS2_PLACEMENT_3D ( 'NONE', #52688, #66203, #83192 ) ;
#41345 = CARTESIAN_POINT ( 'NONE',  ( 12.63842701281683922, 4.550597817667451750, -9.846743663894590881 ) ) ;
#41346 = FACE_OUTER_BOUND ( 'NONE', #26858, .T. ) ;
#41347 = CARTESIAN_POINT ( 'NONE',  ( 0.1532563361054082862, 26.21726448433411605, 2.638427012816831674 ) ) ;
#41348 = CARTESIAN_POINT ( 'NONE',  ( 20.15039907845753220, 64.72266099184918176, 6.262539305110077947 ) ) ;
#41349 = DIRECTION ( 'NONE',  ( -0.000000000000000000, -1.000000000000000000, -0.000000000000000000 ) ) ;
#41350 = CARTESIAN_POINT ( 'NONE',  ( 0.1532563361054100626, 25.80059781766744820, -2.638427012816831230 ) ) ;
#41351 = CARTESIAN_POINT ( 'NONE',  ( 18.52753015748617571, 53.09226448433412315, 4.923371831947298993 ) ) ;
#41352 = CARTESIAN_POINT ( 'NONE',  ( -0.8801773607111009756, 23.06368534415484106, 1.068504757029289695E-15 ) ) ;
#41353 = UNCERTAINTY_MEASURE_WITH_UNIT (LENGTH_MEASURE( 1.000000000000000082E-05 ), #84750, 'distance_accuracy_value', 'NONE');
#41354 = CARTESIAN_POINT ( 'NONE',  ( 21.09922568453595559, 42.04030133659708213, -6.408140936763230044 ) ) ;
#41355 = CARTESIAN_POINT ( 'NONE',  ( 20.88017736071110164, 50.35535201082151247, 2.915334737309930979 ) ) ;
#41356 = CARTESIAN_POINT ( 'NONE',  ( 10.00000000000000000, 24.75893115100078745, -9.846743663894594434 ) ) ;
#41358 = CARTESIAN_POINT ( 'NONE',  ( 10.00000000000000178, 22.25893115100078745, 9.846743663894594434 ) ) ;
#41357 = CARTESIAN_POINT ( 'NONE',  ( 24.16423886937410614, 39.51208216824731068, -3.795296366450302550 ) ) ;
#41360 = ADVANCED_FACE ( 'NONE', ( #6090 ), #82074, .F. ) ;
#41359 = CARTESIAN_POINT ( 'NONE',  ( -0.1503990784575242878, 44.24884699246889852, -6.262539305110083276 ) ) ;
#41361 = ADVANCED_FACE ( 'NONE', ( #37087 ), #66311, .T. ) ;
#41362 = CARTESIAN_POINT ( 'NONE',  ( -42.94000000000001194, 92.00000000000000000, -8.999999999999998224 ) ) ;
#41363 = CARTESIAN_POINT ( 'NONE',  ( 24.16423886937410614, 9.512082168247301794, -3.795296366450302550 ) ) ;
#41364 = CARTESIAN_POINT ( 'NONE',  ( 20.36894250292379382, 33.67874883491396076, 10.36894250292379205 ) ) ;
#41365 = CARTESIAN_POINT ( 'NONE',  ( 7.361572987183169658, 29.96726448433411960, -9.846743663894592657 ) ) ;
#41366 = DIRECTION ( 'NONE',  ( 0.000000000000000000, 0.000000000000000000, -1.000000000000000000 ) ) ;
#41367 = CARTESIAN_POINT ( 'NONE',  ( 0.5774900079438607392, 18.48035201082150536, 5.440088680355550821 ) ) ;
#41368 = CARTESIAN_POINT ( 'NONE',  ( 12.91533473730993009, 46.60535201082150536, -10.88017736071109987 ) ) ;
#41369 = CARTESIAN_POINT ( 'NONE',  ( 10.00000000000000000, 41.81368534415484106, -10.88017736071110342 ) ) ;
#41370 = ORIENTED_EDGE ( 'NONE', *, *, #84035, .F. ) ;
#41371 = CARTESIAN_POINT ( 'NONE',  ( 22.81628187352648496, 31.83196800326375353, -3.434112377981050290 ) ) ;
#41372 = CARTESIAN_POINT ( 'NONE',  ( 17.96484262340118221, 59.93868534415484106, 7.964842623401181321 ) ) ;
#41373 = ORIENTED_EDGE ( 'NONE', *, *, #82010, .T. ) ;
#41374 = CARTESIAN_POINT ( 'NONE',  ( 13.21272562211574986, 15.00000000000000178, -6.271554226548150091 ) ) ;
#41375 = CARTESIAN_POINT ( 'NONE',  ( 17.96484262340118221, 61.18868534415482685, -7.964842623401177768 ) ) ;
#41376 = VERTEX_POINT ( 'NONE', #76547 ) ;
#41377 = CARTESIAN_POINT ( 'NONE',  ( 2.035157376598822676, 67.43868534415484817, -7.964842623401177768 ) ) ;
#41378 = FACE_OUTER_BOUND ( 'NONE', #73338, .T. ) ;
#41379 = CARTESIAN_POINT ( 'NONE',  ( 20.88017736071110875, 40.77201867748817676, -2.915334737309920321 ) ) ;
#41380 = CARTESIAN_POINT ( 'NONE',  ( 0.000000000000000000, 0.5000000000000004441, 0.000000000000000000 ) ) ;
#41381 = CARTESIAN_POINT ( 'NONE',  ( -0.8801773607111009756, 13.06368534415483929, 1.068504757029289695E-15 ) ) ;
#41382 = CARTESIAN_POINT ( 'NONE',  ( 19.84674366389459266, 3.717264484334118713, -2.638427012816827677 ) ) ;
#41383 = CARTESIAN_POINT ( 'NONE',  ( 2.917880565312948704, 7.637082168247301794, 12.26659068614894643 ) ) ;
#41384 = CARTESIAN_POINT ( 'NONE',  ( 2.791683348922237240, 10.38393115100078390, -7.208316651077763204 ) ) ;
#41385 = CARTESIAN_POINT ( 'NONE',  ( 10.00000000000000178, 9.313685344154839285, 10.88017736071110342 ) ) ;
#41386 = CARTESIAN_POINT ( 'NONE',  ( 0.1532563361054082862, 46.21726448433411605, 2.638427012816831674 ) ) ;
#41387 = ORIENTED_EDGE ( 'NONE', *, *, #43800, .T. ) ;
#41388 = ADVANCED_FACE ( 'NONE', ( #68568 ), #41136, .T. ) ;
#41389 = CARTESIAN_POINT ( 'NONE',  ( 19.84674366389459266, 48.30059781766745175, 2.638427012816836559 ) ) ;
#41390 = VERTEX_POINT ( 'NONE', #3047 ) ;
#41391 = CARTESIAN_POINT ( 'NONE',  ( 15.44008868035555260, 49.73035201082150536, 9.422509992056143702 ) ) ;
#41392 = CARTESIAN_POINT ( 'NONE',  ( 12.63842701281683922, 54.55059781766745175, -9.846743663894590881 ) ) ;
#41393 = CARTESIAN_POINT ( 'NONE',  ( 6.565887622018943937, 30.16530133659708568, 12.81628187352647430 ) ) ;
#41395 = CYLINDRICAL_SURFACE ( 'NONE', #97434, 2.999999999999999112 ) ;
#41394 = DIRECTION ( 'NONE',  ( -1.000000000000000000, 0.000000000000000000, 0.000000000000000000 ) ) ;
#41396 = CARTESIAN_POINT ( 'NONE',  ( -0.8801773607111009756, 58.06368534415484106, 1.068504757029289695E-15 ) ) ;
#41397 = CARTESIAN_POINT ( 'NONE',  ( 12.91533473730993009, 11.60535201082150714, -10.88017736071109987 ) ) ;
#41398 =( GEOMETRIC_REPRESENTATION_CONTEXT ( 3 ) GLOBAL_UNCERTAINTY_ASSIGNED_CONTEXT ( ( #3331 ) ) GLOBAL_UNIT_ASSIGNED_CONTEXT ( ( #72088, #50575, #4601 ) ) REPRESENTATION_CONTEXT ( 'NONE', 'WORKASPACE' ) );
#41399 = CIRCLE ( 'NONE', #79696, 7.000000000000005329 ) ;
#41400 = CARTESIAN_POINT ( 'NONE',  ( 3.591859063236763294, 38.29030133659708923, -11.09922568453595026 ) ) ;
#41401 = DIRECTION ( 'NONE',  ( 0.000000000000000000, 1.000000000000000000, 0.000000000000000000 ) ) ;
#41402 = VERTEX_POINT ( 'NONE', #14730 ) ;
#41403 = CARTESIAN_POINT ( 'NONE',  ( 21.09922568453595559, 27.04030133659708568, -6.408140936763230044 ) ) ;
#41404 = CARTESIAN_POINT ( 'NONE',  ( 20.88017736071110875, 30.77201867748816966, -2.915334737309920765 ) ) ;
#41405 = ORIENTED_EDGE ( 'NONE', *, *, #7858, .T. ) ;
#41406 = CARTESIAN_POINT ( 'NONE',  ( 10.00000000000000178, 7.258931151000785675, 9.846743663894594434 ) ) ;
#41407 =( BOUNDED_CURVE ( )  B_SPLINE_CURVE ( 3, ( #9130, #84165, #61143, #39150 ),
 .UNSPECIFIED., .F., .T. ) 
 B_SPLINE_CURVE_WITH_KNOTS ( ( 4, 4 ),
 ( 4.712388980384689674, 5.730377828609853452 ),
 .UNSPECIFIED. ) 
 CURVE ( )  GEOMETRIC_REPRESENTATION_ITEM ( )  RATIONAL_B_SPLINE_CURVE ( ( 1.000000000000000000, 0.9154899770527749059, 0.9154899770527749059, 1.000000000000000000 ) ) 
 REPRESENTATION_ITEM ( '' )  );
#41408 = CARTESIAN_POINT ( 'NONE',  ( 18.52753015748617571, 58.09226448433411605, 4.923371831947298993 ) ) ;
#41410 = CARTESIAN_POINT ( 'NONE',  ( 2.791683348922237240, 45.38393115100079456, -7.208316651077763204 ) ) ;
#41409 = CARTESIAN_POINT ( 'NONE',  ( 17.20831665107776587, 7.883931151000784787, 7.208316651077764980 ) ) ;
#41411 = DIRECTION ( 'NONE',  ( 0.000000000000000000, 1.000000000000000000, 0.000000000000000000 ) ) ;
#41412 =( NAMED_UNIT ( * ) SI_UNIT ( $, .STERADIAN. ) SOLID_ANGLE_UNIT ( ) );
#41413 = CARTESIAN_POINT ( 'NONE',  ( 12.63842701281683034, 42.46726448433412315, 9.846743663894596210 ) ) ;
#41414 = CARTESIAN_POINT ( 'NONE',  ( 0.000000000000000000, -97.00000000000000000, 2.750000000000000000 ) ) ;
#41415 = DIRECTION ( 'NONE',  ( 0.000000000000000000, 0.000000000000000000, 1.000000000000000000 ) ) ;
#41416 = VECTOR ( 'NONE', #87714, 1000.000000000000000 ) ;
#41418 = SURFACE_STYLE_FILL_AREA ( #93896 ) ;
#41417 = CARTESIAN_POINT ( 'NONE',  ( 10.00000000000000000, 29.75893115100078745, -9.846743663894594434 ) ) ;
#41419 = DIRECTION ( 'NONE',  ( -0.000000000000000000, -1.000000000000000000, -0.000000000000000000 ) ) ;
#41421 = EDGE_LOOP ( 'NONE', ( #44550, #48852, #68639, #69559, #29442, #48536 ) ) ;
#41420 = CARTESIAN_POINT ( 'NONE',  ( 7.361572987183170547, 57.05059781766744464, 9.846743663894590881 ) ) ;
#41422 = CARTESIAN_POINT ( 'NONE',  ( 16.40814093676323893, 20.79030133659708923, 11.09922568453595026 ) ) ;
#41423 = CARTESIAN_POINT ( 'NONE',  ( 12.63842701281683922, 39.55059781766744464, -9.846743663894590881 ) ) ;
#41424 = DIRECTION ( 'NONE',  ( 0.7808688094430307203, -0.6246950475544238435, 0.000000000000000000 ) ) ;
#41425 = CARTESIAN_POINT ( 'NONE',  ( -0.3689425029237898834, 46.17874883491397497, -10.36894250292378850 ) ) ;
#41426 = CARTESIAN_POINT ( 'NONE',  ( 19.84674366389459266, 13.71726448433411782, -2.638427012816827677 ) ) ;
#41427 = CARTESIAN_POINT ( 'NONE',  ( 20.00000000000000711, 88.21129152568526877, 4.994901225416799484 ) ) ;
#41428 = CARTESIAN_POINT ( 'NONE',  ( -2.266590686148945544, 62.22041550158063927, 7.082119434687048631 ) ) ;
#41429 = CARTESIAN_POINT ( 'NONE',  ( 19.84674366389459621, 53.50893115100078745, 7.409399052514197653E-17 ) ) ;
#41430 = CARTESIAN_POINT ( 'NONE',  ( -4.164238869374098151, 66.59541550158060375, -3.795296366450310543 ) ) ;
#41431 = CARTESIAN_POINT ( 'NONE',  ( 2.917880565312950480, 40.97041550158063217, -12.26659068614894821 ) ) ;
#41432 = CARTESIAN_POINT ( 'NONE',  ( 22.26659068614895176, 44.72041550158063927, -7.082119434687042414 ) ) ;
#41433 = DIRECTION ( 'NONE',  ( 0.000000000000000000, 0.000000000000000000, 1.000000000000000000 ) ) ;
#41434 = CIRCLE ( 'NONE', #47756, 0.2500000000000002220 ) ;
#41436 = CARTESIAN_POINT ( 'NONE',  ( 14.92337183194729988, 54.34226448433412315, -8.527530157486177487 ) ) ;
#41435 = DIRECTION ( 'NONE',  ( 0.000000000000000000, 0.000000000000000000, -1.000000000000000000 ) ) ;
#41437 = ORIENTED_EDGE ( 'NONE', *, *, #86987, .F. ) ;
#41438 = CARTESIAN_POINT ( 'NONE',  ( 2.035157376598824452, 38.68868534415483396, 7.964842623401179544 ) ) ;
#41439 = ADVANCED_FACE ( 'NONE', ( #7216 ), #55109, .T. ) ;
#41440 = SPHERICAL_SURFACE ( 'NONE', #83235, 0.2500000000000000000 ) ;
#41441 = CARTESIAN_POINT ( 'NONE',  ( 2.791683348922240793, 46.63393115100077324, 7.208316651077764092 ) ) ;
#41442 = FACE_OUTER_BOUND ( 'NONE', #79233, .T. ) ;
#41443 = CARTESIAN_POINT ( 'NONE',  ( 3.469446951953614189E-15, 3.053748834913973198, 14.16423886937410259 ) ) ;
#41444 = CARTESIAN_POINT ( 'NONE',  ( 7.361572987183170547, 52.05059781766745175, 9.846743663894590881 ) ) ;
#41445 = CARTESIAN_POINT ( 'NONE',  ( 7.361572987183169658, 64.96726448433412315, -9.846743663894592657 ) ) ;
#41446 = EDGE_LOOP ( 'NONE', ( #8949, #98324, #53543, #91392 ) ) ;
#41447 = CARTESIAN_POINT ( 'NONE',  ( 10.00000000000000178, 28.05374883491396787, 14.16423886937410082 ) ) ;
#41448 = CARTESIAN_POINT ( 'NONE',  ( 7.361572987183169658, -0.03273551566588185635, -9.846743663894592657 ) ) ;
#41450 = CARTESIAN_POINT ( 'NONE',  ( 20.88017736071110875, 45.77201867748816966, -2.915334737309920321 ) ) ;
#41449 = FILL_AREA_STYLE ('',( #70952 ) ) ;
#41451 = CARTESIAN_POINT ( 'NONE',  ( 2.035157376598822676, 22.43868534415483396, -7.964842623401177768 ) ) ;
#41452 = CARTESIAN_POINT ( 'NONE',  ( 21.09922568453594849, 26.20696800326375353, 6.408140936763242479 ) ) ;
#41453 = DIRECTION ( 'NONE',  ( 0.7132504491541897806, 0.000000000000000000, -0.7009092642998425715 ) ) ;
#41454 = CARTESIAN_POINT ( 'NONE',  ( 0.1532563361054083140, 11.00893115100078568, 1.131784320476157264E-15 ) ) ;
#41455 = DIRECTION ( 'NONE',  ( 0.000000000000000000, 0.000000000000000000, 1.000000000000000000 ) ) ;
#41456 = CARTESIAN_POINT ( 'NONE',  ( -6.857531195348600228, -50.94829529698463233, 4.000000000000000888 ) ) ;
#41457 = CARTESIAN_POINT ( 'NONE',  ( 12.91533473730993009, 6.605352010821504471, -10.88017736071109987 ) ) ;
#41458 = CARTESIAN_POINT ( 'NONE',  ( 12.67147417979175827, 0.04962887043496324452, -7.555862176155505594 ) ) ;
#41459 = CARTESIAN_POINT ( 'NONE',  ( 12.91533473730993009, 41.60535201082149825, -10.88017736071109987 ) ) ;
#41460 = CARTESIAN_POINT ( 'NONE',  ( 10.00000000000000000, 36.81368534415484106, -10.88017736071110342 ) ) ;
#41461 = CARTESIAN_POINT ( 'NONE',  ( 22.81628187352647785, 1.623634669930420271, 6.195893100308588602E-16 ) ) ;
#41462 = CARTESIAN_POINT ( 'NONE',  ( 0.2751277870542967463, 0.000000000000000000, 6.500000000000000888 ) ) ;
#41463 = CARTESIAN_POINT ( 'NONE',  ( 15.00000000000000178, 73.00000000000000000, -6.500000000000000888 ) ) ;
#41464 = CARTESIAN_POINT ( 'NONE',  ( 0.1532563361054083140, 11.00893115100078568, 1.131784320476157264E-15 ) ) ;
#41465 = EDGE_CURVE ( 'NONE', #9539, #21162, #1081, .T. ) ;
#41466 = VERTEX_POINT ( 'NONE', #73974 ) ;
#41467 = CARTESIAN_POINT ( 'NONE',  ( -0.8801773607110991993, 32.85535201082151247, -2.915334737309923874 ) ) ;
#41468 = ADVANCED_FACE ( 'NONE', ( #95506 ), #72987, .F. ) ;
#41469 = CARTESIAN_POINT ( 'NONE',  ( 19.38216949554541202, 10.99863466993042138, 9.382169495545424454 ) ) ;
#41470 = CARTESIAN_POINT ( 'NONE',  ( 10.00000000000000178, 69.31368534415484817, 10.88017736071110342 ) ) ;
#41471 = ADVANCED_FACE ( 'NONE', ( #4517 ), #32762, .T. ) ;
#41472 = CARTESIAN_POINT ( 'NONE',  ( 10.00000000000000178, 7.258931151000785675, 9.846743663894594434 ) ) ;
#41473 = CARTESIAN_POINT ( 'NONE',  ( -1.099225684535947600, 38.70696800326375353, -6.408140936763238038 ) ) ;
#41475 = CARTESIAN_POINT ( 'NONE',  ( -10.64017930668197209, 14.49999999999999112, -10.57291749337233000 ) ) ;
#41474 = CARTESIAN_POINT ( 'NONE',  ( 10.00000000000000178, 12.25893115100078568, 9.846743663894594434 ) ) ;
#41476 = ORIENTED_EDGE ( 'NONE', *, *, #57475, .F. ) ;
#41477 = SURFACE_STYLE_USAGE ( .BOTH. , #79452 ) ;
#41478 = FACE_OUTER_BOUND ( 'NONE', #7137, .T. ) ;
#41479 = CARTESIAN_POINT ( 'NONE',  ( 7.084665262690076126, 12.02201867748817143, -10.88017736071110164 ) ) ;
#41480 = LINE ( 'NONE', #26441, #28002 ) ;
#41481 = CARTESIAN_POINT ( 'NONE',  ( 2.791683348922240793, 11.63393115100078568, 7.208316651077764092 ) ) ;
#41482 = CARTESIAN_POINT ( 'NONE',  ( 20.88017736071110519, 10.56368534415483751, 2.639326808657452039E-16 ) ) ;
#41483 = CARTESIAN_POINT ( 'NONE',  ( 0.5774900079438590739, 7.647018677488171434, -5.440088680355550821 ) ) ;
#41484 = ORIENTED_EDGE ( 'NONE', *, *, #3243, .F. ) ;
#41485 = CARTESIAN_POINT ( 'NONE',  ( 12.91533473730992121, 9.522018677488171434, 10.88017736071110164 ) ) ;
#41486 = CARTESIAN_POINT ( 'NONE',  ( 19.42250999205614193, 20.14701867748817321, 5.440088680355555262 ) ) ;
#41487 = CARTESIAN_POINT ( 'NONE',  ( 13.99999999999999822, 11.00000000000000000, -6.000000000000000000 ) ) ;
#41488 = VERTEX_POINT ( 'NONE', #11020 ) ;
#41489 = CARTESIAN_POINT ( 'NONE',  ( 20.24186590665275531, 27.61633188102327807, -6.114288769123077394 ) ) ;
#41490 = CARTESIAN_POINT ( 'NONE',  ( 17.96484262340118221, 21.18868534415483396, -7.964842623401177768 ) ) ;
#41491 = CARTESIAN_POINT ( 'NONE',  ( 2.791683348922237240, 50.38393115100078035, -7.208316651077763204 ) ) ;
#41492 = DIRECTION ( 'NONE',  ( 0.000000000000000000, 0.000000000000000000, -1.000000000000000000 ) ) ;
#41493 = CARTESIAN_POINT ( 'NONE',  ( -2.816281873526471635, 48.91530133659708213, -3.434112377981056508 ) ) ;
#41494 = CARTESIAN_POINT ( 'NONE',  ( 2.831191079880678085, 79.91181047996344944, -5.000000000000000000 ) ) ;
#41495 = CARTESIAN_POINT ( 'NONE',  ( 20.36894250292379382, 38.67874883491396076, 10.36894250292379205 ) ) ;
#41496 = CARTESIAN_POINT ( 'NONE',  ( 20.88017736071110875, 40.77201867748818387, -2.915334737309920765 ) ) ;
#41497 = CARTESIAN_POINT ( 'NONE',  ( -0.8801773607111008646, 18.27201867748817321, 2.915334737309923430 ) ) ;
#41498 = CARTESIAN_POINT ( 'NONE',  ( 19.84674366389459266, 58.71726448433411605, -2.638427012816827677 ) ) ;
#41499 = CARTESIAN_POINT ( 'NONE',  ( 9.876730923139298568, 0.5000000000000004441, -11.28938378619063165 ) ) ;
#41500 = CARTESIAN_POINT ( 'NONE',  ( 7.361572987183170547, 42.05059781766745886, 9.846743663894590881 ) ) ;
#41501 = ADVANCED_FACE ( 'NONE', ( #3534 ), #34981, .F. ) ;
#41502 = CARTESIAN_POINT ( 'NONE',  ( -10.58981376305275468, 15.00000000000000000, -9.535111140613857117 ) ) ;
#41503 = CARTESIAN_POINT ( 'NONE',  ( 10.00000000000000000, 9.758931151000785675, -9.846743663894594434 ) ) ;
#41504 = CARTESIAN_POINT ( 'NONE',  ( 12.81628187352647608, -28.37636533006957507, -2.602085213965210642E-15 ) ) ;
#41505 = VERTEX_POINT ( 'NONE', #26507 ) ;
#41506 = CARTESIAN_POINT ( 'NONE',  ( 12.91533473730993009, 16.60535201082150891, -10.88017736071109987 ) ) ;
#41507 = CARTESIAN_POINT ( 'NONE',  ( 7.361572987183169658, 4.967264484334119601, -9.846743663894592657 ) ) ;
#41508 = CARTESIAN_POINT ( 'NONE',  ( 0.6178305044545818747, 3.498634669930420049, -9.382169495545419124 ) ) ;
#41510 = CARTESIAN_POINT ( 'NONE',  ( 4.559911319644449179, 47.23035201082150536, -9.422509992056141925 ) ) ;
#41509 = CARTESIAN_POINT ( 'NONE',  ( 12.91533473730992121, 44.52201867748816966, 10.88017736071110164 ) ) ;
#41512 = CARTESIAN_POINT ( 'NONE',  ( 16.40814093676323893, 50.79030133659708923, 11.09922568453595026 ) ) ;
#41511 = CARTESIAN_POINT ( 'NONE',  ( 2.035157376598822676, 22.43868534415483396, -7.964842623401177768 ) ) ;
#41513 = CARTESIAN_POINT ( 'NONE',  ( -2.266590686148945544, 37.22041550158063217, 7.082119434687048631 ) ) ;
#41514 = DIRECTION ( 'NONE',  ( 0.000000000000000000, 0.000000000000000000, 1.000000000000000000 ) ) ;
#41515 = CARTESIAN_POINT ( 'NONE',  ( -1.099225684535947600, 63.70696800326376774, -6.408140936763238038 ) ) ;
#41516 = VERTEX_POINT ( 'NONE', #49999 ) ;
#41517 = CARTESIAN_POINT ( 'NONE',  ( 7.361572987183170547, 52.05059781766745175, 9.846743663894590881 ) ) ;
#41518 =( NAMED_UNIT ( * ) PLANE_ANGLE_UNIT ( ) SI_UNIT ( $, .RADIAN. ) );
#41519 = CARTESIAN_POINT ( 'NONE',  ( 4.559911319644449179, 38.89701867748817676, 9.422509992056141925 ) ) ;
#41520 = ORIENTED_EDGE ( 'NONE', *, *, #48415, .F. ) ;
#41521 = CARTESIAN_POINT ( 'NONE',  ( 12.63842701281683922, 4.550597817667451750, -9.846743663894590881 ) ) ;
#41522 = CARTESIAN_POINT ( 'NONE',  ( 18.52753015748617571, 13.09226448433411960, 4.923371831947298993 ) ) ;
#41523 = CARTESIAN_POINT ( 'NONE',  ( 18.52753015748618282, 23.92559781766745530, -4.923371831947291888 ) ) ;
#41524 = CARTESIAN_POINT ( 'NONE',  ( 12.63842701281683034, 17.46726448433411250, 9.846743663894596210 ) ) ;
#41525 = CARTESIAN_POINT ( 'NONE',  ( 12.63842701281683922, 4.550597817667451750, -9.846743663894590881 ) ) ;
#41527 = CARTESIAN_POINT ( 'NONE',  ( 0.000000000000000000, 0.5000000000000004441, 0.000000000000000000 ) ) ;
#41526 = CARTESIAN_POINT ( 'NONE',  ( -0.8801773607111009756, 63.06368534415484106, 1.068504757029289695E-15 ) ) ;
#41528 = CARTESIAN_POINT ( 'NONE',  ( 2.035157376598822676, 57.43868534415484106, -7.964842623401177768 ) ) ;
#41530 = VERTEX_POINT ( 'NONE', #73473 ) ;
#41529 = CARTESIAN_POINT ( 'NONE',  ( 19.84674366389459266, 18.30059781766745175, 2.638427012816836559 ) ) ;
#41531 = B_SPLINE_CURVE_WITH_KNOTS ( 'NONE', 3,
 ( #95583, #11584, #79095, #42100, #50569, #50075 ),
 .UNSPECIFIED., .F., .F.,
 ( 4, 2, 4 ),
 ( 0.0002800003244075575958, 0.0006862055569968510474, 0.001092410789586144553 ),
 .UNSPECIFIED. ) ;
#41532 = CARTESIAN_POINT ( 'NONE',  ( 14.56311970191025296, 0.2301500865527682516, 3.337330457605979905 ) ) ;
#41533 = CARTESIAN_POINT ( 'NONE',  ( 18.52753015748617571, 53.09226448433412315, 4.923371831947298993 ) ) ;
#41534 = ORIENTED_EDGE ( 'NONE', *, *, #57735, .T. ) ;
#41535 = CARTESIAN_POINT ( 'NONE',  ( -5.999999999999994671, 43.00000000000000000, -4.000000000000000000 ) ) ;
#41536 = UNCERTAINTY_MEASURE_WITH_UNIT (LENGTH_MEASURE( 1.000000000000000082E-05 ), #51555, 'distance_accuracy_value', 'NONE');
#41537 = CARTESIAN_POINT ( 'NONE',  ( 2.393480905993052854, 0.5000000000000004441, 14.80781041047752922 ) ) ;
#41538 = CARTESIAN_POINT ( 'NONE',  ( 10.00000000000000178, 23.05374883491397142, 14.16423886937410082 ) ) ;
#41539 = CIRCLE ( 'NONE', #24053, 14.49999999999999822 ) ;
#41540 = CARTESIAN_POINT ( 'NONE',  ( 17.08211943468705840, 30.13708216824730357, -12.26659068614894466 ) ) ;
#41541 = EDGE_CURVE ( 'NONE', #48470, #10425, #61537, .T. ) ;
#41542 = CARTESIAN_POINT ( 'NONE',  ( -2.266590686148945544, 2.220415501580634388, 7.082119434687048631 ) ) ;
#41543 = DIRECTION ( 'NONE',  ( 1.000000000000000000, 0.000000000000000000, 0.000000000000000000 ) ) ;
#41544 = CARTESIAN_POINT ( 'NONE',  ( 12.91533473730992121, 29.52201867748817321, 10.88017736071110164 ) ) ;
#41545 = CARTESIAN_POINT ( 'NONE',  ( 8.879999999999991900, 69.99999999999998579, 6.250000000000000000 ) ) ;
#41546 = EDGE_LOOP ( 'NONE', ( #13379, #60050, #98272, #87711, #46045, #51566 ) ) ;
#41547 = CARTESIAN_POINT ( 'NONE',  ( 10.00000000000000178, 17.25893115100078745, 9.846743663894594434 ) ) ;
#41550 = AXIS2_PLACEMENT_3D ( 'NONE', #8894, #69905, #63847 ) ;
#41549 = CARTESIAN_POINT ( 'NONE',  ( 2.791683348922237240, 15.38393115100078212, -7.208316651077763204 ) ) ;
#41548 = CARTESIAN_POINT ( 'NONE',  ( 17.96484262340118221, 49.93868534415484106, 7.964842623401181321 ) ) ;
#41551 = CARTESIAN_POINT ( 'NONE',  ( 0.6178305044545818747, 43.49863466993042493, -9.382169495545419124 ) ) ;
#41552 = CARTESIAN_POINT ( 'NONE',  ( 5.076628168052704559, 40.17559781766745175, -8.527530157486179263 ) ) ;
#41553 = EDGE_CURVE ( 'NONE', #63527, #50188, #47418, .T. ) ;
#41554 = TOROIDAL_SURFACE ( 'NONE', #97436, 14.49999999999999822, 0.5000000000000000000 ) ;
#41555 = CARTESIAN_POINT ( 'NONE',  ( 12.14357320772536752, 54.02013147999952736, 3.000000000000000000 ) ) ;
#41556 = CARTESIAN_POINT ( 'NONE',  ( 15.44008868035555260, 59.73035201082151247, 9.422509992056143702 ) ) ;
#41557 = CARTESIAN_POINT ( 'NONE',  ( -2.816281873526473856, 29.12363466993041783, 9.499525473075851096E-16 ) ) ;
#41558 = CARTESIAN_POINT ( 'NONE',  ( -14.16423886937409726, -32.98791783175269643, 3.795296366450320757 ) ) ;
#41559 = CARTESIAN_POINT ( 'NONE',  ( 2.791683348922240793, 21.63393115100078745, 7.208316651077764092 ) ) ;
#41560 = CARTESIAN_POINT ( 'NONE',  ( 10.00000000000000178, 13.05374883491396787, 14.16423886937410082 ) ) ;
#41561 = ORIENTED_EDGE ( 'NONE', *, *, #91196, .T. ) ;
#41562 = CARTESIAN_POINT ( 'NONE',  ( 20.88017736071110164, 30.35535201082151247, 2.915334737309930979 ) ) ;
#41563 = CARTESIAN_POINT ( 'NONE',  ( 2.035157376598824452, 48.68868534415483396, 7.964842623401179544 ) ) ;
#41564 = CARTESIAN_POINT ( 'NONE',  ( 10.00000000000000000, 40.55374883491397497, -14.16423886937410082 ) ) ;
#41565 = CARTESIAN_POINT ( 'NONE',  ( 7.361572987183169658, 49.96726448433410894, -9.846743663894592657 ) ) ;
#41566 = CARTESIAN_POINT ( 'NONE',  ( 17.20831665107776587, 7.883931151000784787, 7.208316651077764980 ) ) ;
#41568 = DIRECTION ( 'NONE',  ( -0.000000000000000000, -1.000000000000000000, -0.000000000000000000 ) ) ;
#41567 = PLANE ( 'NONE',  #57676 ) ;
#41569 = CARTESIAN_POINT ( 'NONE',  ( 20.88017736071110875, 35.77201867748816966, -2.915334737309920765 ) ) ;
#41570 = CARTESIAN_POINT ( 'NONE',  ( 4.873787042390699931, 0.000000000000000000, 13.39061984619922718 ) ) ;
#41571 = CARTESIAN_POINT ( 'NONE',  ( -2.816281873526473856, 19.33196800326375708, 3.434112377981055619 ) ) ;
#41572 = CARTESIAN_POINT ( 'NONE',  ( 18.52753015748618282, 48.92559781766745886, -4.923371831947291888 ) ) ;
#41573 = CARTESIAN_POINT ( 'NONE',  ( -10.88017736071110164, 12.85535201082150181, -2.915334737309917212 ) ) ;
#41574 = FILL_AREA_STYLE_COLOUR ( '', #30792 ) ;
#41576 = CARTESIAN_POINT ( 'NONE',  ( -11.38910604377741898, -77.84323126545000093, -4.000000000000000888 ) ) ;
#41575 = CARTESIAN_POINT ( 'NONE',  ( 15.44008868035555793, 61.39701867748817676, -9.422509992056140149 ) ) ;
#41577 = CARTESIAN_POINT ( 'NONE',  ( -0.1503990784575403861, 14.24884699246888964, -6.262539305110056631 ) ) ;
#41578 = LINE ( 'NONE', #48058, #32066 ) ;
#41579 = CARTESIAN_POINT ( 'NONE',  ( 20.88017736071110519, 65.56368534415483396, 2.639326808657452039E-16 ) ) ;
#41580 = B_SPLINE_CURVE_WITH_KNOTS ( 'NONE', 3,
 ( #48726, #70271, #1788, #79231, #41261, #62746 ),
 .UNSPECIFIED., .F., .F.,
 ( 4, 2, 4 ),
 ( 0.0002800154274912481246, 0.0006862208078174526597, 0.001092426188143657195 ),
 .UNSPECIFIED. ) ;
#41581 = CARTESIAN_POINT ( 'NONE',  ( 2.035157376598824452, 63.68868534415484106, 7.964842623401179544 ) ) ;
#41582 = DIRECTION ( 'NONE',  ( 0.000000000000000000, 1.000000000000000000, -0.000000000000000000 ) ) ;
#41583 = EDGE_CURVE ( 'NONE', #10027, #17080, #12001, .T. ) ;
#41584 = CARTESIAN_POINT ( 'NONE',  ( 1.472469842513823179, 25.59226448433412315, -4.923371831947296329 ) ) ;
#41585 = CARTESIAN_POINT ( 'NONE',  ( 2.035157376598822676, 22.43868534415483396, -7.964842623401177768 ) ) ;
#41586 = EDGE_CURVE ( 'NONE', #63236, #48866, #88488, .T. ) ;
#41587 = CARTESIAN_POINT ( 'NONE',  ( -1.099225684535947600, -1.293031996736246469, -6.408140936763238038 ) ) ;
#41589 = CARTESIAN_POINT ( 'NONE',  ( 19.72487221294571569, 55.71833443783938833, -6.499999999999990230 ) ) ;
#41588 = CARTESIAN_POINT ( 'NONE',  ( 7.084665262690076126, 42.02201867748816966, -10.88017736071110164 ) ) ;
#41590 = FILL_AREA_STYLE ('',( #11069 ) ) ;
#41591 = CARTESIAN_POINT ( 'NONE',  ( -2.816281873526471635, 43.91530133659708923, -3.434112377981056508 ) ) ;
#41592 = ORIENTED_EDGE ( 'NONE', *, *, #28207, .T. ) ;
#41593 = CARTESIAN_POINT ( 'NONE',  ( 0.5774900079438607392, 48.48035201082150536, 5.440088680355550821 ) ) ;
#41595 = CARTESIAN_POINT ( 'NONE',  ( 14.35840480524199947, 0.5000000000000004441, -4.340070442838851683 ) ) ;
#41594 = CARTESIAN_POINT ( 'NONE',  ( 0.6178305044545838731, 24.74863466993042493, 9.382169495545420901 ) ) ;
#41596 = CARTESIAN_POINT ( 'NONE',  ( 4.559911319644449179, 22.23035201082150536, -9.422509992056141925 ) ) ;
#41597 = CARTESIAN_POINT ( 'NONE',  ( 20.36894250292379738, 54.92874883491396076, -10.36894250292379027 ) ) ;
#41598 = CARTESIAN_POINT ( 'NONE',  ( 0.1532563361054100626, 40.80059781766745886, -2.638427012816831230 ) ) ;
#41599 = CARTESIAN_POINT ( 'NONE',  ( 2.035157376598824452, 68.68868534415484817, 7.964842623401179544 ) ) ;
#41600 = CARTESIAN_POINT ( 'NONE',  ( 4.559911319644449179, 68.89701867748817676, 9.422509992056141925 ) ) ;
#41601 = CARTESIAN_POINT ( 'NONE',  ( -8.470640952599010731, 14.99999999999807443, -11.92295067085447968 ) ) ;
#41602 = CARTESIAN_POINT ( 'NONE',  ( -4.164238869374099927, 22.01208216824730357, 3.795296366450308767 ) ) ;
#41603 =( NAMED_UNIT ( * ) SI_UNIT ( $, .STERADIAN. ) SOLID_ANGLE_UNIT ( ) );
#41604 = CARTESIAN_POINT ( 'NONE',  ( 10.00000000000000178, 67.25893115100079456, 9.846743663894594434 ) ) ;
#41605 = ORIENTED_EDGE ( 'NONE', *, *, #24251, .F. ) ;
#41606 = CARTESIAN_POINT ( 'NONE',  ( -0.3689425029237881626, 47.42874883491396787, 10.36894250292379027 ) ) ;
#41607 = CARTESIAN_POINT ( 'NONE',  ( 17.08211943468705130, 48.47041550158063927, 12.26659068614894998 ) ) ;
#41608 = CARTESIAN_POINT ( 'NONE',  ( 1.472469842513823179, 15.59226448433411960, -4.923371831947296329 ) ) ;
#41609 = CARTESIAN_POINT ( 'NONE',  ( -8.900000000000002132, 83.89999999999994884, 0.000000000000000000 ) ) ;
#41610 = DIRECTION ( 'NONE',  ( 0.08715574274766037244, 0.9961946980917453232, 1.511911130105620530E-15 ) ) ;
#41612 = CARTESIAN_POINT ( 'NONE',  ( 22.81628187352647785, 26.41530133659708923, 3.434112377981063169 ) ) ;
#41611 = CARTESIAN_POINT ( 'NONE',  ( 20.88017736071110164, 5.355352010821502695, 2.915334737309930979 ) ) ;
#41613 = CARTESIAN_POINT ( 'NONE',  ( 24.16423886937409904, 44.09541550158063927, 3.795296366450317205 ) ) ;
#41614 = ADVANCED_FACE ( 'NONE', ( #5002 ), #96680, .T. ) ;
#41615 = CYLINDRICAL_SURFACE ( 'NONE', #95545, 15.00000000000000000 ) ;
#41616 =( NAMED_UNIT ( * ) PLANE_ANGLE_UNIT ( ) SI_UNIT ( $, .RADIAN. ) );
#41617 = AXIS2_PLACEMENT_3D ( 'NONE', #47452, #38983, #16479 ) ;
#41618 = CARTESIAN_POINT ( 'NONE',  ( 7.208316651077764980, 2.883931151000783455, 7.208316651077762316 ) ) ;
#41619 = ORIENTED_EDGE ( 'NONE', *, *, #37415, .T. ) ;
#41620 = CARTESIAN_POINT ( 'NONE',  ( 19.72487221294570858, 70.00000000000000000, 6.500000000000000888 ) ) ;
#41621 = CARTESIAN_POINT ( 'NONE',  ( 14.92337183194729988, 24.34226448433411960, -8.527530157486177487 ) ) ;
#41622 = DIRECTION ( 'NONE',  ( 0.000000000000000000, 1.000000000000000000, 0.000000000000000000 ) ) ;
#41623 = CIRCLE ( 'NONE', #17638, 14.49999999999999822 ) ;
#41624 = ORIENTED_EDGE ( 'NONE', *, *, #66614, .T. ) ;
#41626 = CARTESIAN_POINT ( 'NONE',  ( 10.00000000000000000, 11.81368534415483751, -10.88017736071110342 ) ) ;
#41625 = CARTESIAN_POINT ( 'NONE',  ( 20.88017736071110519, 5.563685344154838397, 2.639326808657452039E-16 ) ) ;
#41628 = CARTESIAN_POINT ( 'NONE',  ( 13.43411237798105340, 5.581968003263753531, 12.81628187352647963 ) ) ;
#41627 = CARTESIAN_POINT ( 'NONE',  ( 19.84674366389459266, 43.71726448433410894, -2.638427012816827677 ) ) ;
#41629 = LINE ( 'NONE', #87588, #98239 ) ;
#41630 = B_SPLINE_CURVE_WITH_KNOTS ( 'NONE', 3,
 ( #42332, #72805, #46998, #4347, #77491, #2027 ),
 .UNSPECIFIED., .F., .F.,
 ( 4, 2, 4 ),
 ( 0.0002800111042658719098, 0.0006862164422996730332, 0.001092421780333474157 ),
 .UNSPECIFIED. ) ;
#41631 = CARTESIAN_POINT ( 'NONE',  ( 6.565887622018943937, 13.08196800326374998, -12.81628187352647608 ) ) ;
#41632 = ORIENTED_EDGE ( 'NONE', *, *, #56758, .F. ) ;
#41633 = CARTESIAN_POINT ( 'NONE',  ( 24.16423886937410614, 54.30374883491396787, 8.672049930838204340E-16 ) ) ;
#41634 = VERTEX_POINT ( 'NONE', #43474 ) ;
#41635 = CARTESIAN_POINT ( 'NONE',  ( -4.164238869374098151, 51.59541550158063217, -3.795296366450310543 ) ) ;
#41636 = ORIENTED_EDGE ( 'NONE', *, *, #88613, .F. ) ;
#41637 = CARTESIAN_POINT ( 'NONE',  ( 2.035157376598822676, 37.43868534415484106, -7.964842623401177768 ) ) ;
#41638 = CARTESIAN_POINT ( 'NONE',  ( 20.88017736071110875, 45.77201867748816966, -2.915334737309920765 ) ) ;
#41639 = CIRCLE ( 'NONE', #84738, 3.999999999999999112 ) ;
#41640 = CARTESIAN_POINT ( 'NONE',  ( 15.44008868035555793, 41.39701867748817676, -9.422509992056140149 ) ) ;
#41641 = PRESENTATION_STYLE_ASSIGNMENT (( #87112 ) ) ;
#41642 = CARTESIAN_POINT ( 'NONE',  ( 7.084665262690076126, 42.02201867748816966, -10.88017736071110164 ) ) ;
#41643 = FACE_OUTER_BOUND ( 'NONE', #54521, .T. ) ;
#41644 = AXIS2_PLACEMENT_3D ( 'NONE', #79640, #5124, #43110 ) ;
#41645 = CARTESIAN_POINT ( 'NONE',  ( 7.361572987183170547, 17.05059781766745530, 9.846743663894590881 ) ) ;
#41646 = VERTEX_POINT ( 'NONE', #80989 ) ;
#41647 = CARTESIAN_POINT ( 'NONE',  ( 10.83696084481538691, -98.17058944465519232, 3.750000000000000000 ) ) ;
#41648 = CARTESIAN_POINT ( 'NONE',  ( 0.1532563361054100626, 50.80059781766745175, -2.638427012816831230 ) ) ;
#41649 = CARTESIAN_POINT ( 'NONE',  ( -15.08495336817617982, -0.03417435944610275333, 5.321802168063332950 ) ) ;
#41650 = CARTESIAN_POINT ( 'NONE',  ( 6.565887622018943937, 60.16530133659707502, 12.81628187352647430 ) ) ;
#41651 = CARTESIAN_POINT ( 'NONE',  ( -4.247994584727555534, -13.56436116443237516, 3.750000000000000444 ) ) ;
#41652 = DIRECTION ( 'NONE',  ( 0.000000000000000000, -0.000000000000000000, -1.000000000000000000 ) ) ;
#41653 = LINE ( 'NONE', #40661, #9094 ) ;
#41654 = CYLINDRICAL_SURFACE ( 'NONE', #45016, 0.5000000000000004441 ) ;
#41655 = CARTESIAN_POINT ( 'NONE',  ( 24.16423886937409904, 59.09541550158063217, 3.795296366450317205 ) ) ;
#41656 = DIRECTION ( 'NONE',  ( 0.000000000000000000, 1.000000000000000000, 0.000000000000000000 ) ) ;
#41657 = ORIENTED_EDGE ( 'NONE', *, *, #39775, .T. ) ;
#41658 = DIRECTION ( 'NONE',  ( 0.000000000000000000, 0.000000000000000000, 1.000000000000000000 ) ) ;
#41659 = CARTESIAN_POINT ( 'NONE',  ( 7.361572987183170547, 27.05059781766745175, 9.846743663894590881 ) ) ;
#41660 = CARTESIAN_POINT ( 'NONE',  ( 10.83696084481538691, -98.17058944465519232, 3.750000000000000000 ) ) ;
#41661 = CARTESIAN_POINT ( 'NONE',  ( -2.816281873526471635, 8.915301336597083903, -3.434112377981056508 ) ) ;
#41662 = CARTESIAN_POINT ( 'NONE',  ( 4.559911319644449179, 68.89701867748817676, 9.422509992056141925 ) ) ;
#41663 = EDGE_CURVE ( 'NONE', #19684, #18045, #12009, .T. ) ;
#41664 = CARTESIAN_POINT ( 'NONE',  ( 7.361572987183169658, 14.96726448433411960, -9.846743663894592657 ) ) ;
#41665 = CARTESIAN_POINT ( 'NONE',  ( 14.92337183194729988, 59.34226448433412315, -8.527530157486177487 ) ) ;
#41666 = DIRECTION ( 'NONE',  ( 0.000000000000000000, 1.000000000000000000, 0.000000000000000000 ) ) ;
#41667 = COLOUR_RGB ( '', 0.66274510, 0.83137255, 0.94901961) ;
#41668 = ADVANCED_FACE ( 'NONE', ( #88987 ), #48749, .T. ) ;
#41669 = VERTEX_POINT ( 'NONE', #50979 ) ;
#41670 = CARTESIAN_POINT ( 'NONE',  ( 10.00000000000000178, 68.05374883491397497, 14.16423886937410082 ) ) ;
#41671 = CARTESIAN_POINT ( 'NONE',  ( 17.96484262340118221, 44.93868534415483396, 7.964842623401181321 ) ) ;
#41672 = CIRCLE ( 'NONE', #154, 14.49999999999999822 ) ;
#41674 = CARTESIAN_POINT ( 'NONE',  ( -19.89999999999999858, 98.99999999999998579, 7.750000000000000000 ) ) ;
#41673 = CARTESIAN_POINT ( 'NONE',  ( 16.40814093676323893, 25.79030133659708923, 11.09922568453595026 ) ) ;
#41675 = CARTESIAN_POINT ( 'NONE',  ( 2.035157376598822676, 7.438685344154837509, -7.964842623401177768 ) ) ;
#41676 = DIRECTION ( 'NONE',  ( -0.000000000000000000, -0.000000000000000000, 1.000000000000000000 ) ) ;
#41677 = CARTESIAN_POINT ( 'NONE',  ( 18.52753015748617571, 48.09226448433412315, 4.923371831947298993 ) ) ;
#41678 = CARTESIAN_POINT ( 'NONE',  ( 19.84674366389459266, 18.30059781766745175, 2.638427012816836559 ) ) ;
#41679 = CARTESIAN_POINT ( 'NONE',  ( 10.88017736071110164, -19.64464798917849464, 2.915334737309921209 ) ) ;
#41680 = CARTESIAN_POINT ( 'NONE',  ( 10.00000000000000000, 27.87363466993042138, -12.81628187352647608 ) ) ;
#41681 = CARTESIAN_POINT ( 'NONE',  ( -11.02864780715742299, -96.54579228616290720, -3.750000000000000000 ) ) ;
#41682 = CARTESIAN_POINT ( 'NONE',  ( 12.91533473730993009, 26.60535201082150536, -10.88017736071109987 ) ) ;
#41683 = DIRECTION ( 'NONE',  ( -0.000000000000000000, -0.000000000000000000, 1.000000000000000000 ) ) ;
#41684 = CARTESIAN_POINT ( 'NONE',  ( -2.266590686148945544, 31.38708216824730002, -7.082119434687050408 ) ) ;
#41685 = CARTESIAN_POINT ( 'NONE',  ( 6.204703633549690345, 25.76208216824730712, -14.16423886937410259 ) ) ;
#41686 = CARTESIAN_POINT ( 'NONE',  ( -0.8801773607111009756, 8.063685344154837509, 1.068504757029289695E-15 ) ) ;
#41687 = CARTESIAN_POINT ( 'NONE',  ( 10.00000000000000178, 47.25893115100078745, 9.846743663894594434 ) ) ;
#41688 = CARTESIAN_POINT ( 'NONE',  ( 22.81628187352647785, 41.62363466993042493, 6.195893100308588602E-16 ) ) ;
#41689 = CARTESIAN_POINT ( 'NONE',  ( 2.035157376598824452, 28.68868534415484106, 7.964842623401179544 ) ) ;
#41690 = CARTESIAN_POINT ( 'NONE',  ( 18.52753015748617571, 48.09226448433412315, 4.923371831947298993 ) ) ;
#41691 = ADVANCED_FACE ( 'NONE', ( #66476 ), #72492, .T. ) ;
#41692 = CARTESIAN_POINT ( 'NONE',  ( 0.5774900079438607392, 38.48035201082150536, 5.440088680355550821 ) ) ;
#41693 = CARTESIAN_POINT ( 'NONE',  ( 22.81628187352648496, 6.831968003263753531, -3.434112377981050290 ) ) ;
#41694 = CARTESIAN_POINT ( 'NONE',  ( -2.266590686148945544, 17.22041550158063572, 7.082119434687048631 ) ) ;
#41695 = LINE ( 'NONE', #71205, #5658 ) ;
#41696 = EDGE_CURVE ( 'NONE', #35160, #71617, #79520, .T. ) ;
#41697 = CARTESIAN_POINT ( 'NONE',  ( 18.52753015748618282, 23.92559781766745530, -4.923371831947291888 ) ) ;
#41698 = CARTESIAN_POINT ( 'NONE',  ( 0.6178305044545838731, 49.74863466993041072, 9.382169495545420901 ) ) ;
#41699 = CARTESIAN_POINT ( 'NONE',  ( -2.816281873526471635, 3.915301336597087456, -3.434112377981056508 ) ) ;
#41700 = ORIENTED_EDGE ( 'NONE', *, *, #17841, .T. ) ;
#41701 = DIRECTION ( 'NONE',  ( 0.000000000000000000, 1.000000000000000000, 0.000000000000000000 ) ) ;
#41702 = CARTESIAN_POINT ( 'NONE',  ( 6.829574850499570360, -88.00372650123708240, 3.750000000000001332 ) ) ;
#41703 = CARTESIAN_POINT ( 'NONE',  ( 19.42250999205614193, 5.147018677488171434, 5.440088680355555262 ) ) ;
#41704 = CARTESIAN_POINT ( 'NONE',  ( 7.084665262690076126, 59.10535201082150536, 10.88017736071109987 ) ) ;
#41705 = CARTESIAN_POINT ( 'NONE',  ( 24.16423886937410614, 14.30374883491396787, 8.672049930838204340E-16 ) ) ;
#41706 = CARTESIAN_POINT ( 'NONE',  ( 0.5774900079438590739, 67.64701867748817676, -5.440088680355550821 ) ) ;
#41707 = CARTESIAN_POINT ( 'NONE',  ( 7.361572987183169658, 49.96726448433410894, -9.846743663894592657 ) ) ;
#41708 = CARTESIAN_POINT ( 'NONE',  ( 2.035157376598822676, 37.43868534415484106, -7.964842623401177768 ) ) ;
#41709 = DIRECTION ( 'NONE',  ( -0.1822355254921381451, 0.000000000000000000, -0.9832549075639562819 ) ) ;
#41710 = CARTESIAN_POINT ( 'NONE',  ( 1.472469842513823179, 60.59226448433412315, -4.923371831947296329 ) ) ;
#41711 = VECTOR ( 'NONE', #85819, 1000.000000000000000 ) ;
#41712 = AXIS2_PLACEMENT_3D ( 'NONE', #94778, #86305, #71310 ) ;
#41713 = EDGE_LOOP ( 'NONE', ( #49069, #34506, #4202, #28692, #80935, #42145 ) ) ;
#41714 = ORIENTED_EDGE ( 'NONE', *, *, #49558, .T. ) ;
#41715 = ORIENTED_EDGE ( 'NONE', *, *, #56679, .F. ) ;
#41716 = CIRCLE ( 'NONE', #44902, 0.2500000000000002220 ) ;
#41717 = CARTESIAN_POINT ( 'NONE',  ( 6.090257717040516106, -3.095058389267212256E-15, 13.29726560978572714 ) ) ;
#41718 = CARTESIAN_POINT ( 'NONE',  ( 24.16423886937409904, 4.095415501580634832, 3.795296366450317205 ) ) ;
#41719 = CARTESIAN_POINT ( 'NONE',  ( -4.164238869374099039, 16.80374883491396787, 8.674139862899312516E-16 ) ) ;
#41720 = CARTESIAN_POINT ( 'NONE',  ( -4.164238869374099927, 52.01208216824729647, 3.795296366450308767 ) ) ;
#41721 = CARTESIAN_POINT ( 'NONE',  ( 12.63842701281683034, 62.46726448433410894, 9.846743663894596210 ) ) ;
#41722 = CARTESIAN_POINT ( 'NONE',  ( 0.1532563361054100626, 40.80059781766745886, -2.638427012816831230 ) ) ;
#41724 = CARTESIAN_POINT ( 'NONE',  ( 1.472469842513823179, 66.42559781766745175, 4.923371831947296329 ) ) ;
#41723 = CARTESIAN_POINT ( 'NONE',  ( 4.559911319644449179, 27.23035201082150536, -9.422509992056141925 ) ) ;
#41725 = CARTESIAN_POINT ( 'NONE',  ( -0.3689425029237881626, 2.428748834913967869, 10.36894250292379027 ) ) ;
#41726 = CARTESIAN_POINT ( 'NONE',  ( 22.26659068614895176, 44.72041550158063927, -7.082119434687042414 ) ) ;
#41727 = CARTESIAN_POINT ( 'NONE',  ( -4.164238869374099927, 67.01208216824728936, 3.795296366450308767 ) ) ;
#41728 = LINE ( 'NONE', #78229, #340 ) ;
#41729 = PLANE ( 'NONE',  #77908 ) ;
#41730 = CARTESIAN_POINT ( 'NONE',  ( 10.00000000000000000, 66.81368534415484817, -10.88017736071110342 ) ) ;
#41731 = CARTESIAN_POINT ( 'NONE',  ( 1.472469842513823179, 31.42559781766745530, 4.923371831947296329 ) ) ;
#41732 = CARTESIAN_POINT ( 'NONE',  ( 4.923371831947295441, -30.65773551566587685, -8.527530157486179263 ) ) ;
#41733 = EDGE_CURVE ( 'NONE', #50081, #37711, #50961, .T. ) ;
#41734 = EDGE_LOOP ( 'NONE', ( #10479, #94371, #4293, #62399 ) ) ;
#41735 = ORIENTED_EDGE ( 'NONE', *, *, #65475, .F. ) ;
#41736 = VECTOR ( 'NONE', #72727, 1000.000000000000114 ) ;
#41737 = CARTESIAN_POINT ( 'NONE',  ( 10.00000000000000178, 22.25893115100078745, 9.846743663894594434 ) ) ;
#41738 = ORIENTED_EDGE ( 'NONE', *, *, #86183, .F. ) ;
#41739 = CARTESIAN_POINT ( 'NONE',  ( 10.00000000000000178, 28.05374883491396787, 14.16423886937410082 ) ) ;
#41740 = CARTESIAN_POINT ( 'NONE',  ( 12.63842701281683922, 34.55059781766745886, -9.846743663894590881 ) ) ;
#41741 = CARTESIAN_POINT ( 'NONE',  ( 17.96484262340118221, 54.93868534415484106, 7.964842623401181321 ) ) ;
#41742 = ADVANCED_FACE ( 'NONE', ( #97495 ), #28959, .T. ) ;
#41743 = CARTESIAN_POINT ( 'NONE',  ( 31.00000000000000355, 44.99999999999999289, -7.000000000000000000 ) ) ;
#41744 = CIRCLE ( 'NONE', #97632, 1.500000000000001332 ) ;
#41745 = CARTESIAN_POINT ( 'NONE',  ( 20.88017736071110875, 60.77201867748817676, -2.915334737309920765 ) ) ;
#41746 = CARTESIAN_POINT ( 'NONE',  ( 2.791683348922240793, 41.63393115100078745, 7.208316651077764092 ) ) ;
#41747 = CARTESIAN_POINT ( 'NONE',  ( -3.434112377981067610, 3.081968003263759304, -12.81628187352647252 ) ) ;
#41748 = EDGE_LOOP ( 'NONE', ( #77257, #61784, #66227, #84219 ) ) ;
#41749 = CARTESIAN_POINT ( 'NONE',  ( -0.3689425029237898834, 26.17874883491396432, -10.36894250292378850 ) ) ;
#41750 = ORIENTED_EDGE ( 'NONE', *, *, #71947, .T. ) ;
#41751 = CARTESIAN_POINT ( 'NONE',  ( 0.6178305044545818747, 33.49863466993042493, -9.382169495545419124 ) ) ;
#41752 = CARTESIAN_POINT ( 'NONE',  ( 1.472469842513823179, 25.59226448433412315, -4.923371831947296329 ) ) ;
#41753 = CARTESIAN_POINT ( 'NONE',  ( 24.35999999999999233, 44.99999999999997868, -9.500000000000000000 ) ) ;
#41754 = AXIS2_PLACEMENT_3D ( 'NONE', #82144, #36663, #21665 ) ;
#41755 = CARTESIAN_POINT ( 'NONE',  ( -2.816281873526473856, 59.33196800326374643, 3.434112377981055619 ) ) ;
#41756 = CARTESIAN_POINT ( 'NONE',  ( 14.47650479471819551, 0.5000000000000004441, 3.928206833722108549 ) ) ;
#41757 = CARTESIAN_POINT ( 'NONE',  ( 18.52753015748618282, 23.92559781766745530, -4.923371831947291888 ) ) ;
#41758 = CARTESIAN_POINT ( 'NONE',  ( 20.88017736071110164, 65.35535201082150536, 2.915334737309930979 ) ) ;
#41759 = DIRECTION ( 'NONE',  ( 0.000000000000000000, 0.000000000000000000, 1.000000000000000000 ) ) ;
#41760 = DIRECTION ( 'NONE',  ( -0.000000000000000000, -0.000000000000000000, -1.000000000000000000 ) ) ;
#41761 = CARTESIAN_POINT ( 'NONE',  ( -45.73405099927177986, 104.7125420406077723, 5.163390560272683061 ) ) ;
#41762 = CARTESIAN_POINT ( 'NONE',  ( 0.000000000000000000, 14.49999999999999822, 0.000000000000000000 ) ) ;
#41763 = CARTESIAN_POINT ( 'NONE',  ( 14.92337183194729633, 2.675597817667451750, 8.527530157486181039 ) ) ;
#41764 = CARTESIAN_POINT ( 'NONE',  ( 0.6178305044545838731, 29.74863466993042138, 9.382169495545420901 ) ) ;
#41765 = DIRECTION ( 'NONE',  ( 0.000000000000000000, 0.000000000000000000, 1.000000000000000000 ) ) ;
#41766 = CARTESIAN_POINT ( 'NONE',  ( 17.20831665107776587, 39.13393115100079456, -7.208316651077762316 ) ) ;
#41767 = CARTESIAN_POINT ( 'NONE',  ( 22.81628187352647785, 61.62363466993041783, 6.195893100308588602E-16 ) ) ;
#41768 = CARTESIAN_POINT ( 'NONE',  ( -0.3689425029237881626, 2.428748834913967869, 10.36894250292379027 ) ) ;
#41769 = CARTESIAN_POINT ( 'NONE',  ( 5.076628168052703671, 31.84226448433412315, 8.527530157486179263 ) ) ;
#41770 = CARTESIAN_POINT ( 'NONE',  ( 19.38216949554541202, 35.99863466993041072, 9.382169495545424454 ) ) ;
#41772 = CARTESIAN_POINT ( 'NONE',  ( 19.72487221294571214, 15.71833443783937589, -6.500000000000001776 ) ) ;
#41771 = CARTESIAN_POINT ( 'NONE',  ( -14.26139399674453578, 15.00000000000000000, -2.619664342929994838 ) ) ;
#41773 = CARTESIAN_POINT ( 'NONE',  ( -0.8801773607111009756, 68.06368534415484817, 1.068504757029289695E-15 ) ) ;
#41774 = CARTESIAN_POINT ( 'NONE',  ( 10.00000000000000000, 7.873634669930421381, -12.81628187352647608 ) ) ;
#41775 = AXIS2_PLACEMENT_3D ( 'NONE', #64266, #92811, #56780 ) ;
#41776 = CARTESIAN_POINT ( 'NONE',  ( 14.02068044289383231, 14.63606918466297557, -5.331089937175661930 ) ) ;
#41777 = CARTESIAN_POINT ( 'NONE',  ( 5.076628168052704559, 40.17559781766745175, -8.527530157486179263 ) ) ;
#41778 = CARTESIAN_POINT ( 'NONE',  ( 0.5774900079438590739, 22.64701867748817321, -5.440088680355550821 ) ) ;
#41779 = EDGE_CURVE ( 'NONE', #98193, #69690, #59955, .T. ) ;
#41780 = CARTESIAN_POINT ( 'NONE',  ( 19.38216949554541557, 27.24863466993041783, -9.382169495545420901 ) ) ;
#41781 = CARTESIAN_POINT ( 'NONE',  ( 14.92337183194729633, 27.67559781766745530, 8.527530157486181039 ) ) ;
#41782 = CARTESIAN_POINT ( 'NONE',  ( -8.099999999999999645, 75.73428692542562146, -3.000000000000000000 ) ) ;
#41783 = CARTESIAN_POINT ( 'NONE',  ( 0.5774900079438590739, 32.64701867748816966, -5.440088680355550821 ) ) ;
#41784 = VERTEX_POINT ( 'NONE', #43960 ) ;
#41785 =( BOUNDED_SURFACE ( )  B_SPLINE_SURFACE ( 3, 2, ( 
 ( #53677, #84194, #8191 ),
 ( #15703, #46188, #38688 ),
 ( #84674, #16182, #8671 ),
 ( #39183, #69672, #1201 ),
 ( #31659, #62146, #92654 ),
 ( #24180, #54649, #16676 ),
 ( #64110, #80109, #21470 ),
 ( #5979, #51969, #6457 ),
 ( #19119, #36471, #56630 ),
 ( #81957, #94626, #59453 ),
 ( #11616, #94130, #86644 ),
 ( #34105, #63624, #25657 ),
 ( #57110, #56150, #87118 ),
 ( #13471, #42132, #97484 ),
 ( #79628, #65091, #18636 ),
 ( #72598, #82454, #33614 ),
 ( #89954, #26137, #95106 ),
 ( #3149, #49600, #48626 ),
 ( #57602, #27102, #13978 ),
 ( #19611, #41156, #79130 ),
 ( #4134, #87608, #88102 ),
 ( #95615, #51468, #43952 ),
 ( #34597, #49126, #74451 ),
 ( #66965, #28951, #10642 ),
 ( #44453, #18152, #74954 ),
 ( #11129, #71641, #41647 ) ),
 .UNSPECIFIED., .F., .F., .F. ) 
 B_SPLINE_SURFACE_WITH_KNOTS ( ( 4, 2, 2, 2, 2, 2, 2, 2, 2, 2, 2, 2, 4 ),
 ( 3, 3 ),
 ( 0.000000000000000000, 0.003100998889883697755, 0.006201997779767395511, 0.01240399555953479102, 0.02480799111906958204, 0.04961598223813916408, 0.06201997779767395164, 0.07442397335720873919, 0.08682796891674353368, 0.09302996669651092398, 0.09613096558639462608, 0.09768146503133648406, 0.09923196447627832817 ),
 ( 0.000000000000000000, 1.000000000000000000 ),
 .UNSPECIFIED. ) 
 GEOMETRIC_REPRESENTATION_ITEM ( )  RATIONAL_B_SPLINE_SURFACE ( (
 ( 1.000000000000000000, 0.7071067811865475727, 1.000000000000000000),
 ( 1.000000000000000000, 0.7071067811865475727, 1.000000000000000000),
 ( 1.000000000000000000, 0.7071067811865475727, 1.000000000000000000),
 ( 1.000000000000000000, 0.7071067811865475727, 1.000000000000000000),
 ( 1.000000000000000000, 0.7071067811865475727, 1.000000000000000000),
 ( 1.000000000000000000, 0.7071067811865475727, 1.000000000000000000),
 ( 1.000000000000000000, 0.7071067811865475727, 1.000000000000000000),
 ( 1.000000000000000000, 0.7071067811865475727, 1.000000000000000000),
 ( 1.000000000000000000, 0.7071067811865475727, 1.000000000000000000),
 ( 1.000000000000000000, 0.7071067811865475727, 1.000000000000000000),
 ( 1.000000000000000000, 0.7071067811865472397, 1.000000000000000000),
 ( 1.000000000000000000, 0.7071067811865472397, 1.000000000000000000),
 ( 1.000000000000000000, 0.7071067811865475727, 1.000000000000000000),
 ( 1.000000000000000000, 0.7071067811865475727, 1.000000000000000000),
 ( 1.000000000000000000, 0.7071067811865475727, 1.000000000000000000),
 ( 1.000000000000000000, 0.7071067811865475727, 1.000000000000000000),
 ( 1.000000000000000000, 0.7071067811865477948, 1.000000000000000000),
 ( 1.000000000000000000, 0.7071067811865477948, 1.000000000000000000),
 ( 1.000000000000000000, 0.7071067811865443531, 1.000000000000000000),
 ( 1.000000000000000000, 0.7071067811865443531, 1.000000000000000000),
 ( 1.000000000000000000, 0.7071067811865475727, 1.000000000000000000),
 ( 1.000000000000000000, 0.7071067811865475727, 1.000000000000000000),
 ( 1.000000000000000000, 0.7071067811865475727, 1.000000000000000000),
 ( 1.000000000000000000, 0.7071067811865475727, 1.000000000000000000),
 ( 1.000000000000000000, 0.7071067811865475727, 1.000000000000000000),
 ( 1.000000000000000000, 0.7071067811865475727, 1.000000000000000000) ) ) 
 REPRESENTATION_ITEM ( '' )  SURFACE ( )  );
#41786 = CARTESIAN_POINT ( 'NONE',  ( 12.91533473730992121, 64.52201867748817676, 10.88017736071110164 ) ) ;
#41787 = CARTESIAN_POINT ( 'NONE',  ( 15.44008868035555793, 6.397018677488170546, -9.422509992056140149 ) ) ;
#41789 = CARTESIAN_POINT ( 'NONE',  ( 10.00000000000000178, 29.31368534415483751, 10.88017736071110342 ) ) ;
#41788 = CARTESIAN_POINT ( 'NONE',  ( 5.076628168052703671, 41.84226448433411605, 8.527530157486179263 ) ) ;
#41790 = FACE_OUTER_BOUND ( 'NONE', #36816, .T. ) ;
#41791 = CARTESIAN_POINT ( 'NONE',  ( -0.8801773607111009756, 43.06368534415484106, 1.068504757029289695E-15 ) ) ;
#41793 = CARTESIAN_POINT ( 'NONE',  ( 14.40939250469963895, 15.00000000000000000, -1.618458416365745389 ) ) ;
#41792 = CARTESIAN_POINT ( 'NONE',  ( 15.44008868035555260, 19.73035201082150536, 9.422509992056143702 ) ) ;
#41794 = CARTESIAN_POINT ( 'NONE',  ( 0.1532563361054100626, 5.800597817667452638, -2.638427012816831230 ) ) ;
#41795 = CARTESIAN_POINT ( 'NONE',  ( 14.92337183194729633, 57.67559781766745886, 8.527530157486181039 ) ) ;
#41797 = CARTESIAN_POINT ( 'NONE',  ( 20.32896413005680714, 20.57879003517447458, -5.963430220938276349 ) ) ;
#41796 = CARTESIAN_POINT ( 'NONE',  ( -2.266590686148945544, 56.38708216824731068, -7.082119434687050408 ) ) ;
#41798 = DIRECTION ( 'NONE',  ( 0.000000000000000000, 1.000000000000000000, 0.000000000000000000 ) ) ;
#41799 = CARTESIAN_POINT ( 'NONE',  ( -2.266590686148945544, 1.387082168247301128, -7.082119434687050408 ) ) ;
#41800 = CARTESIAN_POINT ( 'NONE',  ( 24.16423886937410614, 39.30374883491396787, 8.672049930838204340E-16 ) ) ;
#41801 = CIRCLE ( 'NONE', #94457, 15.00000000000000000 ) ;
#41802 = AXIS2_PLACEMENT_3D ( 'NONE', #8799, #39314, #39801 ) ;
#41803 = CARTESIAN_POINT ( 'NONE',  ( -4.260926853938491021, -13.83313663034587115, 2.750000000000000888 ) ) ;
#41804 = ORIENTED_EDGE ( 'NONE', *, *, #54038, .F. ) ;
#41805 = EDGE_CURVE ( 'NONE', #26148, #32242, #88737, .T. ) ;
#41806 = CARTESIAN_POINT ( 'NONE',  ( 17.08211943468705840, 65.13708216824730357, -12.26659068614894466 ) ) ;
#41807 = CARTESIAN_POINT ( 'NONE',  ( 14.92337183194729633, 37.67559781766745175, 8.527530157486181039 ) ) ;
#41809 = PRESENTATION_STYLE_ASSIGNMENT (( #33768 ) ) ;
#41808 = CARTESIAN_POINT ( 'NONE',  ( -10.93781366033354097, 15.00000000000000000, 10.26470809774057713 ) ) ;
#41810 = CARTESIAN_POINT ( 'NONE',  ( 12.91533473730992121, 59.52201867748816966, 10.88017736071110164 ) ) ;
#41811 = CARTESIAN_POINT ( 'NONE',  ( 5.377205135395861646, 14.76930270348882601, 13.94000429068785074 ) ) ;
#41812 = CARTESIAN_POINT ( 'NONE',  ( -0.8801773607111009756, 33.06368534415484106, 1.068504757029289695E-15 ) ) ;
#41813 = PRESENTATION_LAYER_ASSIGNMENT (  '', '', ( #51358 ) ) ;
#41814 = CARTESIAN_POINT ( 'NONE',  ( 6.565887622018943937, 55.16530133659709634, 12.81628187352647430 ) ) ;
#41815 = CARTESIAN_POINT ( 'NONE',  ( 22.81628187352647785, 16.41530133659708923, 3.434112377981063169 ) ) ;
#41816 = CARTESIAN_POINT ( 'NONE',  ( 7.361572987183169658, 19.96726448433411960, -9.846743663894592657 ) ) ;
#41818 = ORIENTED_EDGE ( 'NONE', *, *, #32320, .T. ) ;
#41817 = EDGE_CURVE ( 'NONE', #41634, #45908, #21481, .T. ) ;
#41819 = DIRECTION ( 'NONE',  ( -0.000000000000000000, 0.000000000000000000, 1.000000000000000000 ) ) ;
#41820 = PRESENTATION_STYLE_ASSIGNMENT (( #11299 ) ) ;
#41821 = CARTESIAN_POINT ( 'NONE',  ( -4.164238869374098151, 31.59541550158063927, -3.795296366450310543 ) ) ;
#41822 = CARTESIAN_POINT ( 'NONE',  ( 10.00000000000000000, 36.81368534415484106, -10.88017736071110342 ) ) ;
#41823 = CARTESIAN_POINT ( 'NONE',  ( 0.5774900079438607392, 43.48035201082151247, 5.440088680355550821 ) ) ;
#41824 = CARTESIAN_POINT ( 'NONE',  ( -0.4427729075171647488, 14.61885305295417758, -10.00000000000000000 ) ) ;
#41825 = LINE ( 'NONE', #34277, #52858 ) ;
#41826 = CARTESIAN_POINT ( 'NONE',  ( 1.472469842513823179, 15.59226448433411960, -4.923371831947296329 ) ) ;
#41827 = SURFACE_SIDE_STYLE ('',( #87789 ) ) ;
#41828 = COLOUR_RGB ( '', 0.66274510, 0.83137255, 0.94901961) ;
#41829 = CARTESIAN_POINT ( 'NONE',  ( -46.48928645636215151, 103.2957187381728232, 6.397878122523974476 ) ) ;
#41830 = CARTESIAN_POINT ( 'NONE',  ( 19.84674366389459266, 18.71726448433411960, -2.638427012816827677 ) ) ;
#41831 = CARTESIAN_POINT ( 'NONE',  ( 0.1532563361054100626, 55.80059781766745175, -2.638427012816831230 ) ) ;
#41832 = CARTESIAN_POINT ( 'NONE',  ( 20.88017736071110164, 25.35535201082150891, 2.915334737309930979 ) ) ;
#41833 = CARTESIAN_POINT ( 'NONE',  ( 21.09922568453594849, 51.20696800326375353, 6.408140936763242479 ) ) ;
#41834 = FACE_OUTER_BOUND ( 'NONE', #45801, .T. ) ;
#41835 = CARTESIAN_POINT ( 'NONE',  ( 0.5774900079438590739, 62.64701867748817676, -5.440088680355550821 ) ) ;
#41836 = CARTESIAN_POINT ( 'NONE',  ( 1.472469842513823179, 30.59226448433411960, -4.923371831947296329 ) ) ;
#41838 = CARTESIAN_POINT ( 'NONE',  ( 7.361572987183170547, 27.05059781766745175, 9.846743663894590881 ) ) ;
#41837 = CARTESIAN_POINT ( 'NONE',  ( 2.917880565312950480, 65.97041550158063217, -12.26659068614894821 ) ) ;
#41839 = CARTESIAN_POINT ( 'NONE',  ( 0.1957200283969099119, 60.25733960839542647, 6.499999999999992006 ) ) ;
#41840 = CARTESIAN_POINT ( 'NONE',  ( 10.00000000000000178, 67.25893115100079456, 9.846743663894594434 ) ) ;
#41841 = CARTESIAN_POINT ( 'NONE',  ( 24.16423886937410614, 14.30374883491396787, 8.672049930838204340E-16 ) ) ;
#41842 = CARTESIAN_POINT ( 'NONE',  ( 20.36894250292379738, 34.92874883491396076, -10.36894250292379027 ) ) ;
#41843 = CARTESIAN_POINT ( 'NONE',  ( 1.472469842513823179, 26.42559781766745175, 4.923371831947296329 ) ) ;
#41844 = CARTESIAN_POINT ( 'NONE',  ( 5.500000000000000000, 11.50000000000000000, 5.000000000000000000 ) ) ;
#41845 = CARTESIAN_POINT ( 'NONE',  ( 12.91533473730992121, 19.52201867748816611, 10.88017736071110164 ) ) ;
#41846 = CARTESIAN_POINT ( 'NONE',  ( -0.8801773607111008646, 58.27201867748816966, 2.915334737309923430 ) ) ;
#41847 = CARTESIAN_POINT ( 'NONE',  ( 0.1532563361054082862, 56.21726448433411605, 2.638427012816831674 ) ) ;
#41848 = ORIENTED_EDGE ( 'NONE', *, *, #49678, .F. ) ;
#41849 = CARTESIAN_POINT ( 'NONE',  ( -2.816281873526471635, 43.91530133659708923, -3.434112377981056508 ) ) ;
#41850 = CARTESIAN_POINT ( 'NONE',  ( 2.035157376598824452, 48.68868534415483396, 7.964842623401179544 ) ) ;
#41851 = ORIENTED_EDGE ( 'NONE', *, *, #7131, .T. ) ;
#41852 = CARTESIAN_POINT ( 'NONE',  ( -2.614810775378867191, 35.00346125376525919, 10.00000000000000000 ) ) ;
#41853 = ADVANCED_FACE ( 'NONE', ( #38459 ), #68952, .F. ) ;
#41854 = DIRECTION ( 'NONE',  ( 0.000000000000000000, 0.000000000000000000, -1.000000000000000000 ) ) ;
#41855 = ORIENTED_EDGE ( 'NONE', *, *, #71251, .F. ) ;
#41856 = CARTESIAN_POINT ( 'NONE',  ( 4.559911319644449179, 58.89701867748817676, 9.422509992056141925 ) ) ;
#41857 = SURFACE_SIDE_STYLE ('',( #85874 ) ) ;
#41858 = CIRCLE ( 'NONE', #88146, 14.49999999999999822 ) ;
#41859 = CARTESIAN_POINT ( 'NONE',  ( -9.509319644403765537, 13.17686044187662020, 7.198808227794258663 ) ) ;
#41860 = LINE ( 'NONE', #49335, #56837 ) ;
#41861 = CARTESIAN_POINT ( 'NONE',  ( 10.00000000000000178, 68.05374883491397497, 14.16423886937410082 ) ) ;
#41862 = CARTESIAN_POINT ( 'NONE',  ( 18.52753015748618282, 13.92559781766745175, -4.923371831947291888 ) ) ;
#41863 = CARTESIAN_POINT ( 'NONE',  ( 24.16423886937409904, 19.09541550158063927, 3.795296366450317205 ) ) ;
#41864 = CARTESIAN_POINT ( 'NONE',  ( 17.20831665107776587, 2.883931151000785231, 7.208316651077764980 ) ) ;
#41865 = CARTESIAN_POINT ( 'NONE',  ( 20.88017736071110519, 20.56368534415484106, 2.639326808657452039E-16 ) ) ;
#41866 = CARTESIAN_POINT ( 'NONE',  ( 10.00000000000000000, 54.75893115100078745, -9.846743663894594434 ) ) ;
#41867 = EDGE_LOOP ( 'NONE', ( #17864, #62609, #604, #66434 ) ) ;
#41868 = CARTESIAN_POINT ( 'NONE',  ( 10.00000000000000000, 49.75893115100078745, -9.846743663894594434 ) ) ;
#41869 = ORIENTED_EDGE ( 'NONE', *, *, #72813, .F. ) ;
#41870 = CARTESIAN_POINT ( 'NONE',  ( 0.000000000000000000, -97.00000000000000000, -3.750000000000000000 ) ) ;
#41871 = CARTESIAN_POINT ( 'NONE',  ( 10.00000000000000000, 51.81368534415484106, -10.88017736071110342 ) ) ;
#41872 = CARTESIAN_POINT ( 'NONE',  ( 1.472469842513823179, 51.42559781766745886, 4.923371831947296329 ) ) ;
#41874 = FACE_OUTER_BOUND ( 'NONE', #20112, .T. ) ;
#41873 = CARTESIAN_POINT ( 'NONE',  ( 0.5774900079438590739, 7.647018677488171434, -5.440088680355550821 ) ) ;
#41875 = CARTESIAN_POINT ( 'NONE',  ( 0.5774900079438607392, 63.48035201082149825, 5.440088680355550821 ) ) ;
#41876 = CARTESIAN_POINT ( 'NONE',  ( 10.00000000000000178, 9.313685344154839285, 10.88017736071110342 ) ) ;
#41877 = PRESENTATION_LAYER_ASSIGNMENT (  '', '', ( #97775 ) ) ;
#41878 = EDGE_LOOP ( 'NONE', ( #29269, #10749, #10474, #60159 ) ) ;
#41879 = CARTESIAN_POINT ( 'NONE',  ( 16.40814093676323893, 40.79030133659708923, 11.09922568453595026 ) ) ;
#41880 = CARTESIAN_POINT ( 'NONE',  ( 4.559911319644449179, 27.23035201082150536, -9.422509992056141925 ) ) ;
#41881 = DIRECTION ( 'NONE',  ( 1.000000000000000000, -0.000000000000000000, 0.000000000000000000 ) ) ;
#41882 = ORIENTED_EDGE ( 'NONE', *, *, #930, .F. ) ;
#41883 = CARTESIAN_POINT ( 'NONE',  ( 3.591859063236763294, 48.29030133659708923, -11.09922568453595026 ) ) ;
#41884 = CARTESIAN_POINT ( 'NONE',  ( 10.00000000000000178, 29.31368534415483751, 10.88017736071110342 ) ) ;
#41885 = AXIS2_PLACEMENT_3D ( 'NONE', #73215, #26738, #41765 ) ;
#41886 = VECTOR ( 'NONE', #40269, 1000.000000000000114 ) ;
#41887 = ORIENTED_EDGE ( 'NONE', *, *, #26671, .F. ) ;
#41888 = VECTOR ( 'NONE', #4094, 1000.000000000000000 ) ;
#41889 = CARTESIAN_POINT ( 'NONE',  ( 18.52753015748618282, 8.925597817667451750, -4.923371831947291888 ) ) ;
#41890 = AXIS2_PLACEMENT_3D ( 'NONE', #5523, #83483, #36003 ) ;
#41891 = CARTESIAN_POINT ( 'NONE',  ( 18.52753015748618282, 58.92559781766745886, -4.923371831947291888 ) ) ;
#41893 = CARTESIAN_POINT ( 'NONE',  ( 0.1532563361054100626, 50.80059781766745175, -2.638427012816831230 ) ) ;
#41892 = CARTESIAN_POINT ( 'NONE',  ( 14.92337183194729633, 7.675597817667451750, 8.527530157486181039 ) ) ;
#41894 = CARTESIAN_POINT ( 'NONE',  ( -0.8801773607111009756, 28.06368534415484106, 1.068504757029289695E-15 ) ) ;
#41895 = CARTESIAN_POINT ( 'NONE',  ( -0.04068437667222125909, 52.21974360917721469, -6.396802510829770583 ) ) ;
#41896 = DIRECTION ( 'NONE',  ( -0.06975647374410356982, -0.9975640502598257520, -0.000000000000000000 ) ) ;
#41898 = CARTESIAN_POINT ( 'NONE',  ( 12.63842701281683034, 12.46726448433411782, 9.846743663894596210 ) ) ;
#41897 = CARTESIAN_POINT ( 'NONE',  ( 19.84674366389459621, 28.50893115100078745, 7.409399052514197653E-17 ) ) ;
#41899 = CARTESIAN_POINT ( 'NONE',  ( 4.431036607602466759, 0.5000000000000004441, 14.33059365769913818 ) ) ;
#41900 = EDGE_CURVE ( 'NONE', #39436, #15469, #59287, .T. ) ;
#41902 = EDGE_LOOP ( 'NONE', ( #15528, #85967, #53991, #33812 ) ) ;
#41901 = CARTESIAN_POINT ( 'NONE',  ( 1.472469842513823179, 60.59226448433412315, -4.923371831947296329 ) ) ;
#41903 = CARTESIAN_POINT ( 'NONE',  ( -2.816281873526473856, 64.12363466993042493, 9.499525473075851096E-16 ) ) ;
#41904 = CARTESIAN_POINT ( 'NONE',  ( 19.72487221294570858, 7.802231764288317883, -6.499999999999999112 ) ) ;
#41905 = CARTESIAN_POINT ( 'NONE',  ( -2.816281873526473856, 24.33196800326375353, 3.434112377981055619 ) ) ;
#41906 = CARTESIAN_POINT ( 'NONE',  ( 19.84674366389459266, 38.30059781766745175, 2.638427012816836559 ) ) ;
#41907 = CARTESIAN_POINT ( 'NONE',  ( -13.95692576442134758, 14.76984994697213516, 5.331646315825635973 ) ) ;
#41909 = EDGE_CURVE ( 'NONE', #86750, #85266, #98492, .T. ) ;
#41908 = CARTESIAN_POINT ( 'NONE',  ( 17.08211943468705840, 60.13708216824729647, -12.26659068614894466 ) ) ;
#41910 = CARTESIAN_POINT ( 'NONE',  ( 1.472469842513823179, 20.59226448433411960, -4.923371831947296329 ) ) ;
#41911 = ORIENTED_EDGE ( 'NONE', *, *, #70927, .F. ) ;
#41912 = CARTESIAN_POINT ( 'NONE',  ( 20.00000000000000711, 84.97150353911858645, 5.197973391108559937 ) ) ;
#41913 = CARTESIAN_POINT ( 'NONE',  ( 20.36894250292379382, 63.67874883491396787, 10.36894250292379205 ) ) ;
#41914 = CARTESIAN_POINT ( 'NONE',  ( 7.361572987183170547, 57.05059781766744464, 9.846743663894590881 ) ) ;
#41915 = CARTESIAN_POINT ( 'NONE',  ( 6.204703633549690345, 67.84541550158060375, 14.16423886937410082 ) ) ;
#41916 = CARTESIAN_POINT ( 'NONE',  ( 20.36894250292379738, 39.92874883491396787, -10.36894250292379027 ) ) ;
#41918 = DIRECTION ( 'NONE',  ( 0.000000000000000000, 0.000000000000000000, -1.000000000000000000 ) ) ;
#41917 = CARTESIAN_POINT ( 'NONE',  ( -2.266590686148945544, 41.38708216824729647, -7.082119434687050408 ) ) ;
#41919 = CARTESIAN_POINT ( 'NONE',  ( 14.02068044289376303, 14.63595249122788999, 5.331089937175756077 ) ) ;
#41920 = EDGE_CURVE ( 'NONE', #48512, #27481, #54503, .T. ) ;
#41922 = CARTESIAN_POINT ( 'NONE',  ( 1.472469842513823179, 60.59226448433412315, -4.923371831947296329 ) ) ;
#41921 = DIRECTION ( 'NONE',  ( 0.000000000000000000, 0.000000000000000000, -1.000000000000000000 ) ) ;
#41923 = CARTESIAN_POINT ( 'NONE',  ( 20.88017736071110164, 50.35535201082151247, 2.915334737309930979 ) ) ;
#41924 = CARTESIAN_POINT ( 'NONE',  ( 11.43651723230273021, -81.64184067850541737, 3.750000000000000888 ) ) ;
#41925 = CARTESIAN_POINT ( 'NONE',  ( 12.63842701281683922, 49.55059781766744464, -9.846743663894590881 ) ) ;
#41926 = CARTESIAN_POINT ( 'NONE',  ( 0.2751277870542967463, 70.00000000000000000, -6.000000000000000000 ) ) ;
#41927 = CARTESIAN_POINT ( 'NONE',  ( 10.00000000000000000, 49.75893115100078745, -9.846743663894594434 ) ) ;
#41928 = CARTESIAN_POINT ( 'NONE',  ( 17.08211943468705130, 3.470415501580634388, 12.26659068614894998 ) ) ;
#41929 = EDGE_CURVE ( 'NONE', #10746, #85496, #72377, .T. ) ;
#41930 = CARTESIAN_POINT ( 'NONE',  ( 24.16423886937410614, 24.51208216824730002, -3.795296366450302550 ) ) ;
#41931 = SURFACE_STYLE_FILL_AREA ( #4422 ) ;
#41933 = LINE ( 'NONE', #19407, #66424 ) ;
#41932 = SURFACE_STYLE_USAGE ( .BOTH. , #27391 ) ;
#41934 = CARTESIAN_POINT ( 'NONE',  ( 2.035157376598824452, 23.68868534415484461, 7.964842623401179544 ) ) ;
#41935 = CARTESIAN_POINT ( 'NONE',  ( -2.816281873526471635, 23.91530133659708568, -3.434112377981056508 ) ) ;
#41936 = CARTESIAN_POINT ( 'NONE',  ( 0.4400000000000020006, 1.019547802438468986, 2.500000000000000000 ) ) ;
#41937 = CARTESIAN_POINT ( 'NONE',  ( 17.20831665107776587, 14.13393115100078568, -7.208316651077762316 ) ) ;
#41939 = EDGE_CURVE ( 'NONE', #91147, #48124, #69440, .T. ) ;
#41938 = ORIENTED_EDGE ( 'NONE', *, *, #91561, .F. ) ;
#41940 = CARTESIAN_POINT ( 'NONE',  ( 6.757940885639631468, -58.32678904743398363, -3.750000000000000000 ) ) ;
#41941 = CARTESIAN_POINT ( 'NONE',  ( 10.00000000000000178, 23.05374883491397142, 14.16423886937410082 ) ) ;
#41942 = CARTESIAN_POINT ( 'NONE',  ( 2.603489959281581889, 20.43575266056827999, -6.499999999999995559 ) ) ;
#41943 = CARTESIAN_POINT ( 'NONE',  ( -0.8801773607111009756, 3.063685344154838397, 1.068504757029289695E-15 ) ) ;
#41944 = CARTESIAN_POINT ( 'NONE',  ( -14.02068044289389626, 14.49999999999999112, 5.331089937175563342 ) ) ;
#41945 = CARTESIAN_POINT ( 'NONE',  ( 0.5774900079438607392, 43.48035201082151247, 5.440088680355550821 ) ) ;
#41946 = CARTESIAN_POINT ( 'NONE',  ( 15.44008868035555793, 31.39701867748817676, -9.422509992056140149 ) ) ;
#41947 = CARTESIAN_POINT ( 'NONE',  ( 6.565887622018943937, 8.081968003263751754, -12.81628187352647608 ) ) ;
#41948 = DIRECTION ( 'NONE',  ( -6.217248937900876626E-15, 0.000000000000000000, 1.000000000000000000 ) ) ;
#41949 = CARTESIAN_POINT ( 'NONE',  ( 4.873787042390789637, -0.03417435944610275333, -13.39061984619918988 ) ) ;
#41950 = CARTESIAN_POINT ( 'NONE',  ( 18.52753015748617571, 8.092264484334117824, 4.923371831947298993 ) ) ;
#41951 = ORIENTED_EDGE ( 'NONE', *, *, #18200, .F. ) ;
#41952 = CARTESIAN_POINT ( 'NONE',  ( 18.06765999051787830, 48.99127512925448258, 6.499999999999931610 ) ) ;
#41953 = CARTESIAN_POINT ( 'NONE',  ( 4.559911319644449179, 43.89701867748816966, 9.422509992056141925 ) ) ;
#41954 = CARTESIAN_POINT ( 'NONE',  ( -2.816281873526471635, 3.915301336597087456, -3.434112377981056508 ) ) ;
#41955 = CARTESIAN_POINT ( 'NONE',  ( 4.559911319644449179, 62.23035201082150536, -9.422509992056141925 ) ) ;
#41956 = CARTESIAN_POINT ( 'NONE',  ( 10.00000000000000000, 29.75893115100078745, -9.846743663894594434 ) ) ;
#41957 = CARTESIAN_POINT ( 'NONE',  ( 6.565887622018943937, 40.16530133659708923, 12.81628187352647430 ) ) ;
#41958 = AXIS2_PLACEMENT_3D ( 'NONE', #62150, #78154, #8675 ) ;
#41959 = CARTESIAN_POINT ( 'NONE',  ( 14.92337183194729988, 4.342264484334117824, -8.527530157486177487 ) ) ;
#41960 = EDGE_LOOP ( 'NONE', ( #23865, #73558, #24271, #3626, #19986, #96263 ) ) ;
#41961 = FILL_AREA_STYLE_COLOUR ( '', #3768 ) ;
#41962 = DIRECTION ( 'NONE',  ( -1.000000000000000000, 0.000000000000000000, 0.000000000000000000 ) ) ;
#41963 = CARTESIAN_POINT ( 'NONE',  ( -2.816281873526471635, 63.91530133659708923, -3.434112377981056508 ) ) ;
#41964 = CARTESIAN_POINT ( 'NONE',  ( 0.1532563361054083140, 36.00893115100078745, 1.131784320476157264E-15 ) ) ;
#41965 = CARTESIAN_POINT ( 'NONE',  ( 12.91533473730992121, 24.52201867748816966, 10.88017736071110164 ) ) ;
#41966 = CARTESIAN_POINT ( 'NONE',  ( 15.44008868035555260, 9.730352010821505360, 9.422509992056143702 ) ) ;
#41967 = VERTEX_POINT ( 'NONE', #46920 ) ;
#41968 = CIRCLE ( 'NONE', #70731, 2.999999999999999112 ) ;
#41969 = CARTESIAN_POINT ( 'NONE',  ( 0.5774900079438590739, 7.647018677488171434, -5.440088680355550821 ) ) ;
#41970 = EDGE_CURVE ( 'NONE', #56730, #35739, #67987, .T. ) ;
#41971 = CARTESIAN_POINT ( 'NONE',  ( 0.5774900079438590739, 22.64701867748817321, -5.440088680355550821 ) ) ;
#41972 = CARTESIAN_POINT ( 'NONE',  ( 6.189644032515776217, 0.04922511925147198680, -13.39157970158797006 ) ) ;
#41973 = AXIS2_PLACEMENT_3D ( 'NONE', #3596, #33084, #87565 ) ;
#41974 = EDGE_LOOP ( 'NONE', ( #16671, #85883, #29857, #8142 ) ) ;
#41975 = CARTESIAN_POINT ( 'NONE',  ( 2.791683348922240793, 66.63393115100079456, 7.208316651077764092 ) ) ;
#41976 = CARTESIAN_POINT ( 'NONE',  ( 19.42250999205614548, 25.98035201082150891, -5.440088680355545492 ) ) ;
#41977 = CARTESIAN_POINT ( 'NONE',  ( 0.1532563361054083140, 61.00893115100078745, 1.131784320476157264E-15 ) ) ;
#41978 = FACE_BOUND ( 'NONE', #95947, .T. ) ;
#41979 = CARTESIAN_POINT ( 'NONE',  ( 21.09922568453595559, 57.04030133659708923, -6.408140936763230044 ) ) ;
#41980 = CARTESIAN_POINT ( 'NONE',  ( -0.3689425029237898834, 31.17874883491396787, -10.36894250292378850 ) ) ;
#41981 = CARTESIAN_POINT ( 'NONE',  ( 10.00000000000000178, 44.31368534415484106, 10.88017736071110342 ) ) ;
#41982 = CARTESIAN_POINT ( 'NONE',  ( 20.88017736071110519, 10.56368534415483929, 2.639326808657452039E-16 ) ) ;
#41983 = CARTESIAN_POINT ( 'NONE',  ( 14.92337183194729633, 52.67559781766745175, 8.527530157486181039 ) ) ;
#41984 = LINE ( 'NONE', #26461, #85994 ) ;
#41985 = CARTESIAN_POINT ( 'NONE',  ( 2.791683348922237240, 50.38393115100078035, -7.208316651077763204 ) ) ;
#41986 = DIRECTION ( 'NONE',  ( -0.8788171126619678253, 0.000000000000000000, 0.4771587602596037425 ) ) ;
#41987 = AXIS2_PLACEMENT_3D ( 'NONE', #5493, #51467, #89466 ) ;
#41988 = CARTESIAN_POINT ( 'NONE',  ( 2.791683348922240793, 6.633931151000785675, 7.208316651077764092 ) ) ;
#41989 = CARTESIAN_POINT ( 'NONE',  ( 9.382169495545415572, -32.75136533006958217, -9.382169495545422677 ) ) ;
#41990 = ORIENTED_EDGE ( 'NONE', *, *, #98339, .F. ) ;
#41991 = CARTESIAN_POINT ( 'NONE',  ( 20.88017736071110519, 10.56368534415483751, 2.639326808657452039E-16 ) ) ;
#41992 = CARTESIAN_POINT ( 'NONE',  ( 18.52753015748617571, 8.092264484334117824, 4.923371831947298993 ) ) ;
#41993 = CARTESIAN_POINT ( 'NONE',  ( 19.84674366389459621, 63.50893115100078745, 7.409399052514197653E-17 ) ) ;
#41994 = CARTESIAN_POINT ( 'NONE',  ( 20.88017736071110875, 60.77201867748817676, -2.915334737309920765 ) ) ;
#41996 = CARTESIAN_POINT ( 'NONE',  ( 0.6178305044545838731, 44.74863466993042493, 9.382169495545420901 ) ) ;
#41995 = CARTESIAN_POINT ( 'NONE',  ( 10.00000000000000178, 19.31368534415484106, 10.88017736071110342 ) ) ;
#41997 = CARTESIAN_POINT ( 'NONE',  ( -0.3689425029237898834, 26.17874883491396432, -10.36894250292378850 ) ) ;
#41998 = CARTESIAN_POINT ( 'NONE',  ( -14.91937968691864036, 0.2306972965111904195, -0.8063277559920134507 ) ) ;
#41999 =( BOUNDED_CURVE ( )  B_SPLINE_CURVE ( 2, ( #67855, #16327, #77302, #8330, #59838, #6850, #15844, #45336, #36859 ),
 .UNSPECIFIED., .F., .T. ) 
 B_SPLINE_CURVE_WITH_KNOTS ( ( 3, 2, 2, 2, 3 ),
 ( 0.08108559304626794528, 0.08333333333333332871, 0.08928571428571428770, 0.09523809523809523281, 0.09748583552516061623 ),
 .UNSPECIFIED. ) 
 CURVE ( )  GEOMETRIC_REPRESENTATION_ITEM ( )  RATIONAL_B_SPLINE_CURVE ( ( 0.9839835555609424134, 0.9871328979762477029, 1.000000000000000000, 0.9659258262890683122, 1.000000000000000000, 0.9659258262890683122, 1.000000000000000000, 0.9871328979762477029, 0.9839835555609424134 ) ) 
 REPRESENTATION_ITEM ( '' )  );
#42000 = AXIS2_PLACEMENT_3D ( 'NONE', #5840, #13334, #66825 ) ;
#42001 = CARTESIAN_POINT ( 'NONE',  ( 21.09922568453594849, 61.20696800326376064, 6.408140936763242479 ) ) ;
#42002 = VERTEX_POINT ( 'NONE', #78905 ) ;
#42003 = CARTESIAN_POINT ( 'NONE',  ( 6.565887622018943937, -1.918031996736246692, -12.81628187352647608 ) ) ;
#42004 = CARTESIAN_POINT ( 'NONE',  ( -7.551349515323269479, 15.00000000000000000, 12.08468537022900868 ) ) ;
#42005 = CARTESIAN_POINT ( 'NONE',  ( 4.559911319644449179, 27.23035201082150536, -9.422509992056141925 ) ) ;
#42006 = CARTESIAN_POINT ( 'NONE',  ( 10.00000000000000178, 67.25893115100079456, 9.846743663894594434 ) ) ;
#42007 = ORIENTED_EDGE ( 'NONE', *, *, #32274, .F. ) ;
#42008 = CARTESIAN_POINT ( 'NONE',  ( 19.84674366389459621, 8.508931151000785675, 7.409399052514197653E-17 ) ) ;
#42009 = CARTESIAN_POINT ( 'NONE',  ( 5.076628168052703671, 6.842264484334118713, 8.527530157486179263 ) ) ;
#42010 = B_SPLINE_CURVE_WITH_KNOTS ( 'NONE', 3,
 ( #93524, #71038, #33017, #41532, #56996, #94504 ),
 .UNSPECIFIED., .F., .F.,
 ( 4, 2, 4 ),
 ( 0.0002800026249563246535, 0.0006862078800502478294, 0.001092413135144171005 ),
 .UNSPECIFIED. ) ;
#42011 = CARTESIAN_POINT ( 'NONE',  ( 17.20831665107776587, 19.13393115100078035, -7.208316651077762316 ) ) ;
#42012 = EDGE_CURVE ( 'NONE', #54920, #5711, #38947, .T. ) ;
#42013 = CARTESIAN_POINT ( 'NONE',  ( 17.20831665107776587, 12.88393115100078390, 7.208316651077764980 ) ) ;
#42014 = CARTESIAN_POINT ( 'NONE',  ( 10.00000000000000178, 2.258931151000784787, 9.846743663894594434 ) ) ;
#42016 = CARTESIAN_POINT ( 'NONE',  ( -0.8801773607111009756, 38.27201867748816966, 2.915334737309923874 ) ) ;
#42015 = CARTESIAN_POINT ( 'NONE',  ( -0.8801773607111009756, 53.06368534415484106, 1.068504757029289695E-15 ) ) ;
#42017 = CARTESIAN_POINT ( 'NONE',  ( 15.44008868035555793, 56.39701867748817676, -9.422509992056140149 ) ) ;
#42019 = ORIENTED_EDGE ( 'NONE', *, *, #24010, .T. ) ;
#42018 = CARTESIAN_POINT ( 'NONE',  ( 19.84674366389459266, 23.30059781766745530, 2.638427012816836559 ) ) ;
#42020 = EDGE_CURVE ( 'NONE', #57591, #35160, #85541, .T. ) ;
#42021 = CARTESIAN_POINT ( 'NONE',  ( 5.803070148808231465, 15.00000000000000000, 13.28812917035392260 ) ) ;
#42022 = CARTESIAN_POINT ( 'NONE',  ( 2.791683348922237240, 60.38393115100078745, -7.208316651077763204 ) ) ;
#42023 = ORIENTED_EDGE ( 'NONE', *, *, #81063, .T. ) ;
#42024 = CARTESIAN_POINT ( 'NONE',  ( 7.084665262690076126, 4.105352010821503583, 10.88017736071109987 ) ) ;
#42026 = EDGE_CURVE ( 'NONE', #35183, #6556, #53627, .T. ) ;
#42025 = CARTESIAN_POINT ( 'NONE',  ( -2.266590686148945544, 17.22041550158063572, 7.082119434687048631 ) ) ;
#42027 = AXIS2_PLACEMENT_3D ( 'NONE', #72116, #95108, #62645 ) ;
#42028 = DIRECTION ( 'NONE',  ( 0.000000000000000000, 0.000000000000000000, 1.000000000000000000 ) ) ;
#42029 = MECHANICAL_DESIGN_GEOMETRIC_PRESENTATION_REPRESENTATION (  '', ( #94684 ), #3699 ) ;
#42030 = CARTESIAN_POINT ( 'NONE',  ( 6.204703633549690345, 10.76208216824729824, -14.16423886937410259 ) ) ;
#42031 = CARTESIAN_POINT ( 'NONE',  ( 2.917880565312950480, 30.97041550158063572, -12.26659068614894821 ) ) ;
#42032 = CARTESIAN_POINT ( 'NONE',  ( -6.732636091893168029, -88.11213685669366669, 3.750000000000000000 ) ) ;
#42033 = CARTESIAN_POINT ( 'NONE',  ( 17.96484262340118221, 29.93868534415484106, 7.964842623401181321 ) ) ;
#42034 = ORIENTED_EDGE ( 'NONE', *, *, #91679, .F. ) ;
#42036 = AXIS2_PLACEMENT_3D ( 'NONE', #28343, #12352, #20850 ) ;
#42035 = CARTESIAN_POINT ( 'NONE',  ( 5.076628168052704559, 10.17559781766745175, -8.527530157486179263 ) ) ;
#42038 = CARTESIAN_POINT ( 'NONE',  ( 17.20831665107776587, 19.13393115100078035, -7.208316651077762316 ) ) ;
#42037 = CARTESIAN_POINT ( 'NONE',  ( 10.00000000000000178, 54.31368534415484106, 10.88017736071110342 ) ) ;
#42039 = CARTESIAN_POINT ( 'NONE',  ( 15.44008868035555793, 6.397018677488171434, -9.422509992056140149 ) ) ;
#42040 = CARTESIAN_POINT ( 'NONE',  ( 10.00000000000000178, 50.37363466993042493, 12.81628187352647608 ) ) ;
#42041 = CARTESIAN_POINT ( 'NONE',  ( 1.472469842513823179, 41.42559781766745886, 4.923371831947296329 ) ) ;
#42042 = CARTESIAN_POINT ( 'NONE',  ( 18.52753015748617571, 58.09226448433411605, 4.923371831947298993 ) ) ;
#42043 = CARTESIAN_POINT ( 'NONE',  ( 22.81628187352647785, 26.62363466993042138, 6.195893100308588602E-16 ) ) ;
#42044 = CARTESIAN_POINT ( 'NONE',  ( 12.26659068614894466, -35.27958449841936073, -7.082119434687053960 ) ) ;
#42045 = CARTESIAN_POINT ( 'NONE',  ( 18.52753015748617571, 28.09226448433411960, 4.923371831947298993 ) ) ;
#42046 = CARTESIAN_POINT ( 'NONE',  ( 2.917880565312948704, 7.637082168247301794, 12.26659068614894643 ) ) ;
#42047 = ORIENTED_EDGE ( 'NONE', *, *, #76649, .T. ) ;
#42048 = VERTEX_POINT ( 'NONE', #23950 ) ;
#42049 = CARTESIAN_POINT ( 'NONE',  ( 12.91533473730993009, 51.60535201082149825, -10.88017736071109987 ) ) ;
#42050 = CARTESIAN_POINT ( 'NONE',  ( 15.44008868035555260, 59.73035201082151247, 9.422509992056143702 ) ) ;
#42051 = CARTESIAN_POINT ( 'NONE',  ( 20.36894250292379382, 43.67874883491397497, 10.36894250292379205 ) ) ;
#42052 = CARTESIAN_POINT ( 'NONE',  ( 17.20831665107776587, 59.13393115100078745, -7.208316651077762316 ) ) ;
#42053 = CARTESIAN_POINT ( 'NONE',  ( 2.791683348922240793, 6.633931151000785675, 7.208316651077764092 ) ) ;
#42054 = FACE_OUTER_BOUND ( 'NONE', #3368, .T. ) ;
#42055 = CARTESIAN_POINT ( 'NONE',  ( 10.00000000000000178, 44.31368534415484106, 10.88017736071110342 ) ) ;
#42056 = EDGE_CURVE ( 'NONE', #23318, #62480, #23317, .T. ) ;
#42057 = CARTESIAN_POINT ( 'NONE',  ( -6.829866546992953147, -69.52413922185967010, -2.500000000000000000 ) ) ;
#42058 = CARTESIAN_POINT ( 'NONE',  ( 13.43411237798105340, 25.58196800326374998, 12.81628187352647963 ) ) ;
#42059 = CARTESIAN_POINT ( 'NONE',  ( 18.52753015748617571, 58.09226448433411605, 4.923371831947298993 ) ) ;
#42060 = CARTESIAN_POINT ( 'NONE',  ( -7.964842623401172439, 8.688685344154842838, 7.964842623401183097 ) ) ;
#42061 = CARTESIAN_POINT ( 'NONE',  ( 2.035157376598824452, 63.68868534415484106, 7.964842623401179544 ) ) ;
#42062 = AXIS2_PLACEMENT_3D ( 'NONE', #89135, #13132, #29978 ) ;
#42064 = EDGE_CURVE ( 'NONE', #20489, #34423, #82310, .T. ) ;
#42063 =( NAMED_UNIT ( * ) SI_UNIT ( $, .STERADIAN. ) SOLID_ANGLE_UNIT ( ) );
#42065 = CARTESIAN_POINT ( 'NONE',  ( 0.1532563361054082862, 1.217264484334117824, 2.638427012816831674 ) ) ;
#42067 = CARTESIAN_POINT ( 'NONE',  ( 7.361572987183170547, 2.050597817667451750, 9.846743663894590881 ) ) ;
#42066 = AXIS2_PLACEMENT_3D ( 'NONE', #63622, #94128, #50474 ) ;
#42068 = CARTESIAN_POINT ( 'NONE',  ( -4.250000000000000000, 36.75000000000000000, -4.000000000000000000 ) ) ;
#42069 = CARTESIAN_POINT ( 'NONE',  ( 18.52753015748617571, 38.09226448433412315, 4.923371831947298993 ) ) ;
#42070 = CARTESIAN_POINT ( 'NONE',  ( 12.91533473730992121, 24.52201867748816966, 10.88017736071110164 ) ) ;
#42071 = CARTESIAN_POINT ( 'NONE',  ( 19.84674366389459621, 58.50893115100078745, 7.409399052514197653E-17 ) ) ;
#42073 = CARTESIAN_POINT ( 'NONE',  ( -3.888677292528964102, -8.267505865805661713, -3.750000000000000000 ) ) ;
#42072 = CARTESIAN_POINT ( 'NONE',  ( 15.44008868035555793, 31.39701867748817676, -9.422509992056140149 ) ) ;
#42074 = DIRECTION ( 'NONE',  ( 0.000000000000000000, 1.000000000000000000, 0.000000000000000000 ) ) ;
#42075 = CARTESIAN_POINT ( 'NONE',  ( 3.591859063236763294, 33.29030133659708213, -11.09922568453595026 ) ) ;
#42076 = ORIENTED_EDGE ( 'NONE', *, *, #8714, .T. ) ;
#42077 = CARTESIAN_POINT ( 'NONE',  ( 20.88017736071110164, 55.35535201082149825, 2.915334737309930979 ) ) ;
#42078 = CARTESIAN_POINT ( 'NONE',  ( -2.816281873526473856, 14.12363466993041961, 9.499525473075851096E-16 ) ) ;
#42079 = CARTESIAN_POINT ( 'NONE',  ( 0.1532563361054083140, 1.008931151000784787, 1.131784320476157264E-15 ) ) ;
#42080 = CARTESIAN_POINT ( 'NONE',  ( 12.91533473730992121, 29.52201867748817321, 10.88017736071110164 ) ) ;
#42081 = CARTESIAN_POINT ( 'NONE',  ( -2.266590686148945544, 61.38708216824730357, -7.082119434687050408 ) ) ;
#42082 = CARTESIAN_POINT ( 'NONE',  ( 2.791683348922237240, 45.38393115100079456, -7.208316651077763204 ) ) ;
#42083 = CARTESIAN_POINT ( 'NONE',  ( 0.1532563361054100626, 0.8005978176674514168, -2.638427012816831230 ) ) ;
#42084 = CARTESIAN_POINT ( 'NONE',  ( 10.00000000000000000, 56.81368534415484106, -10.88017736071110342 ) ) ;
#42085 = DIRECTION ( 'NONE',  ( 1.000000000000000000, 0.000000000000000000, 0.000000000000000000 ) ) ;
#42086 = CARTESIAN_POINT ( 'NONE',  ( -0.3689425029237881626, 27.42874883491397142, 10.36894250292379027 ) ) ;
#42087 = CARTESIAN_POINT ( 'NONE',  ( 19.64275500434244748, 84.99812590208811969, -5.306653671078411350 ) ) ;
#42088 = ORIENTED_EDGE ( 'NONE', *, *, #2629, .T. ) ;
#42089 = CARTESIAN_POINT ( 'NONE',  ( 6.204703633549690345, 45.76208216824729647, -14.16423886937410259 ) ) ;
#42090 = CARTESIAN_POINT ( 'NONE',  ( -4.164238869374099039, 46.80374883491397497, 8.674139862899312516E-16 ) ) ;
#42091 = CARTESIAN_POINT ( 'NONE',  ( 1.472469842513823179, 20.59226448433411960, -4.923371831947296329 ) ) ;
#42092 = CARTESIAN_POINT ( 'NONE',  ( -1.099225684535947600, 19.54030133659708568, 6.408140936763237150 ) ) ;
#42093 = CARTESIAN_POINT ( 'NONE',  ( 0.000000000000000000, 14.49999999999999822, 0.000000000000000000 ) ) ;
#42095 = CARTESIAN_POINT ( 'NONE',  ( -10.82078848414227146, -0.03417435944610275333, 11.78082904627290795 ) ) ;
#42094 = STYLED_ITEM ( 'NONE', ( #6880 ), #96348 ) ;
#42097 = CARTESIAN_POINT ( 'NONE',  ( 19.38216949554541202, 50.99863466993042493, 9.382169495545424454 ) ) ;
#42096 = CARTESIAN_POINT ( 'NONE',  ( -13.48255862861919852, 3.931018169630358772E-16, -5.335786055104346559 ) ) ;
#42098 = CARTESIAN_POINT ( 'NONE',  ( -4.164238869374099039, 41.80374883491397497, 8.674139862899312516E-16 ) ) ;
#42099 = AXIS2_PLACEMENT_3D ( 'NONE', #55658, #85658, #17177 ) ;
#42100 = CARTESIAN_POINT ( 'NONE',  ( -4.841308736149450453, 14.76984994419931674, -14.13449535775674626 ) ) ;
#42101 = CARTESIAN_POINT ( 'NONE',  ( 19.84674366389459266, 13.71726448433411782, -2.638427012816827677 ) ) ;
#42102 = CARTESIAN_POINT ( 'NONE',  ( 7.208316651077762316, 4.133931151000787452, -7.208316651077764980 ) ) ;
#42103 = EDGE_CURVE ( 'NONE', #3422, #65076, #26010, .T. ) ;
#42104 = VERTEX_POINT ( 'NONE', #17436 ) ;
#42105 = FILL_AREA_STYLE_COLOUR ( '', #23686 ) ;
#42106 = CARTESIAN_POINT ( 'NONE',  ( 19.84674366389459621, 18.50893115100078745, 7.409399052514197653E-17 ) ) ;
#42107 = AXIS2_PLACEMENT_3D ( 'NONE', #80241, #28718, #89226 ) ;
#42108 = FACE_OUTER_BOUND ( 'NONE', #83898, .T. ) ;
#42109 = ORIENTED_EDGE ( 'NONE', *, *, #32257, .F. ) ;
#42110 = CARTESIAN_POINT ( 'NONE',  ( 6.204703633549690345, 10.76208216824729824, -14.16423886937410259 ) ) ;
#42112 = CARTESIAN_POINT ( 'NONE',  ( -0.8801773607111009756, 28.06368534415484106, 1.068504757029289695E-15 ) ) ;
#42111 = CARTESIAN_POINT ( 'NONE',  ( -0.8801773607111009756, 3.063685344154838397, 1.068504757029289695E-15 ) ) ;
#42114 = CARTESIAN_POINT ( 'NONE',  ( -2.816281873526473856, 4.331968003263754419, 3.434112377981055619 ) ) ;
#42113 = CARTESIAN_POINT ( 'NONE',  ( 10.00000000000000000, 44.75893115100078745, -9.846743663894594434 ) ) ;
#42115 = CARTESIAN_POINT ( 'NONE',  ( 11.48952521350024192, 4.570664323179305100E-16, -8.845383562533745803 ) ) ;
#42116 = EDGE_CURVE ( 'NONE', #63236, #89545, #9927, .T. ) ;
#42117 = CARTESIAN_POINT ( 'NONE',  ( 21.09922568453595559, 22.04030133659708923, -6.408140936763230044 ) ) ;
#42118 = VERTEX_POINT ( 'NONE', #31908 ) ;
#42119 = CARTESIAN_POINT ( 'NONE',  ( -2.266590686148945544, 62.22041550158063927, 7.082119434687048631 ) ) ;
#42120 = CARTESIAN_POINT ( 'NONE',  ( -0.3689425029237898834, 56.17874883491396076, -10.36894250292378850 ) ) ;
#42121 = VERTEX_POINT ( 'NONE', #62409 ) ;
#42122 = CARTESIAN_POINT ( 'NONE',  ( 20.88017736071110875, 30.77201867748816966, -2.915334737309920765 ) ) ;
#42123 = CARTESIAN_POINT ( 'NONE',  ( 15.44008868035555260, 39.73035201082150536, 9.422509992056143702 ) ) ;
#42124 = CARTESIAN_POINT ( 'NONE',  ( 2.035157376598822676, 57.43868534415484106, -7.964842623401177768 ) ) ;
#42125 = CARTESIAN_POINT ( 'NONE',  ( 17.88942678785190665, 78.22945985324594176, -4.041087757000573433 ) ) ;
#42126 = CARTESIAN_POINT ( 'NONE',  ( -0.8801773607110991993, 37.85535201082151247, -2.915334737309923874 ) ) ;
#42128 = EDGE_LOOP ( 'NONE', ( #98822, #12081, #37729, #24132, #98979, #5166, #48719, #35259, #32530, #85148 ) ) ;
#42127 = CARTESIAN_POINT ( 'NONE',  ( -2.614810775378867191, 35.00346125376525919, 9.500000000000000000 ) ) ;
#42129 = EDGE_CURVE ( 'NONE', #32729, #35669, #79657, .T. ) ;
#42130 = CARTESIAN_POINT ( 'NONE',  ( 12.63842701281683034, 17.46726448433411250, 9.846743663894596210 ) ) ;
#42131 = VERTEX_POINT ( 'NONE', #54423 ) ;
#42132 = CARTESIAN_POINT ( 'NONE',  ( 11.35644480889520302, -65.08008077083090370, 4.000000000000000000 ) ) ;
#42133 = CARTESIAN_POINT ( 'NONE',  ( 14.92337183194729988, 59.34226448433412315, -8.527530157486177487 ) ) ;
#42135 = ADVANCED_FACE ( 'NONE', ( #47904 ), #91448, .T. ) ;
#42134 = FACE_OUTER_BOUND ( 'NONE', #26501, .T. ) ;
#42136 = CARTESIAN_POINT ( 'NONE',  ( 19.38216949554541202, 60.99863466993042493, 9.382169495545424454 ) ) ;
#42137 = DIRECTION ( 'NONE',  ( 0.4461978131098069400, 0.000000000000000000, -0.8949343616020258851 ) ) ;
#42138 = EDGE_LOOP ( 'NONE', ( #69765, #73655, #7311, #11707, #86197, #6197 ) ) ;
#42139 = CARTESIAN_POINT ( 'NONE',  ( -1.915564264621230972, 4.378229052359348391E-16, -14.37291249357993372 ) ) ;
#42140 = DIRECTION ( 'NONE',  ( 0.000000000000000000, 0.000000000000000000, 1.000000000000000000 ) ) ;
#42142 = CARTESIAN_POINT ( 'NONE',  ( 5.076628168052704559, 30.17559781766745175, -8.527530157486179263 ) ) ;
#42141 = CARTESIAN_POINT ( 'NONE',  ( 5.076628168052703671, 61.84226448433412315, 8.527530157486179263 ) ) ;
#42143 = CARTESIAN_POINT ( 'NONE',  ( 20.36894250292379382, 58.67874883491396076, 10.36894250292379205 ) ) ;
#42144 = CARTESIAN_POINT ( 'NONE',  ( 19.39188664607694434, 5.837033823263999999, -6.500000000000002665 ) ) ;
#42145 = ORIENTED_EDGE ( 'NONE', *, *, #6442, .T. ) ;
#42146 = CARTESIAN_POINT ( 'NONE',  ( -7.313705784284680433, 0.5000000000000004441, 13.09617149020738935 ) ) ;
#42147 = CARTESIAN_POINT ( 'NONE',  ( 17.20831665107776587, 37.88393115100078745, 7.208316651077764980 ) ) ;
#42148 = CARTESIAN_POINT ( 'NONE',  ( 19.38216949554541202, 0.9986346699304200492, 9.382169495545424454 ) ) ;
#42149 = CARTESIAN_POINT ( 'NONE',  ( 19.42250999205614193, 65.14701867748817676, 5.440088680355555262 ) ) ;
#42150 = CARTESIAN_POINT ( 'NONE',  ( 11.81378540890930751, 15.00000000000000000, 7.968498874458199488 ) ) ;
#42151 = CARTESIAN_POINT ( 'NONE',  ( 10.00000000000000178, 7.258931151000785675, 9.846743663894594434 ) ) ;
#42152 = CARTESIAN_POINT ( 'NONE',  ( 18.52753015748618282, 58.92559781766745886, -4.923371831947291888 ) ) ;
#42153 = CARTESIAN_POINT ( 'NONE',  ( 0.2751277870542911952, 19.36607318730131055, -6.499999999999992006 ) ) ;
#42154 = VECTOR ( 'NONE', #34176, 1000.000000000000114 ) ;
#42155 = VERTEX_POINT ( 'NONE', #65858 ) ;
#42156 = CARTESIAN_POINT ( 'NONE',  ( 2.035157376598822676, 7.438685344154837509, -7.964842623401177768 ) ) ;
#42157 = CARTESIAN_POINT ( 'NONE',  ( -0.3689425029237881626, 12.42874883491396609, 10.36894250292379027 ) ) ;
#42158 = CARTESIAN_POINT ( 'NONE',  ( 1.472469842513823179, 15.59226448433411960, -4.923371831947296329 ) ) ;
#42159 = CARTESIAN_POINT ( 'NONE',  ( 7.084665262690076126, 39.10535201082150536, 10.88017736071109987 ) ) ;
#42161 = CARTESIAN_POINT ( 'NONE',  ( 12.91533473730992121, 64.52201867748817676, 10.88017736071110164 ) ) ;
#42160 = CARTESIAN_POINT ( 'NONE',  ( 10.00000000000000000, 22.87363466993042138, -12.81628187352647608 ) ) ;
#42162 = FACE_OUTER_BOUND ( 'NONE', #19982, .T. ) ;
#42163 = AXIS2_PLACEMENT_3D ( 'NONE', #96646, #87639, #80644 ) ;
#42164 = EDGE_CURVE ( 'NONE', #76530, #63379, #95381, .T. ) ;
#42165 = LINE ( 'NONE', #72628, #69289 ) ;
#42166 =( NAMED_UNIT ( * ) PLANE_ANGLE_UNIT ( ) SI_UNIT ( $, .RADIAN. ) );
#42167 = CARTESIAN_POINT ( 'NONE',  ( 10.00000000000000000, 54.75893115100078745, -9.846743663894594434 ) ) ;
#42168 = CARTESIAN_POINT ( 'NONE',  ( 0.1532563361054083140, 16.00893115100078390, 1.131784320476157264E-15 ) ) ;
#42169 = CARTESIAN_POINT ( 'NONE',  ( 5.440088680355549045, -23.60298132251182324, -9.422509992056141925 ) ) ;
#42170 = CARTESIAN_POINT ( 'NONE',  ( -2.816281873526473856, 24.12363466993042138, 9.499525473075851096E-16 ) ) ;
#42171 = CARTESIAN_POINT ( 'NONE',  ( -11.20030343255358218, -94.46585862443534154, -3.750000000000000000 ) ) ;
#42172 = CARTESIAN_POINT ( 'NONE',  ( 12.91533473730992121, 24.52201867748816966, 10.88017736071110164 ) ) ;
#42173 = CARTESIAN_POINT ( 'NONE',  ( 4.380000000000002558, 1.019547802438462547, 2.500000000000000000 ) ) ;
#42174 = CARTESIAN_POINT ( 'NONE',  ( -4.164238869374099039, 46.80374883491397497, 8.674139862899312516E-16 ) ) ;
#42175 = CARTESIAN_POINT ( 'NONE',  ( 14.29484424893245453, 14.76984993772165744, -4.345072767107134304 ) ) ;
#42176 = CARTESIAN_POINT ( 'NONE',  ( 18.52753015748618282, 43.92559781766745175, -4.923371831947291888 ) ) ;
#42177 = CARTESIAN_POINT ( 'NONE',  ( 6.565887622018943937, 35.16530133659708923, 12.81628187352647430 ) ) ;
#42178 = CARTESIAN_POINT ( 'NONE',  ( 0.5774900079438607392, 28.48035201082150891, 5.440088680355550821 ) ) ;
#42179 = CARTESIAN_POINT ( 'NONE',  ( 12.63842701281683034, 47.46726448433412315, 9.846743663894596210 ) ) ;
#42180 = CARTESIAN_POINT ( 'NONE',  ( 7.084665262690076126, 39.10535201082150536, 10.88017736071109987 ) ) ;
#42181 = CARTESIAN_POINT ( 'NONE',  ( 10.00000000000000000, 7.873634669930421381, -12.81628187352647608 ) ) ;
#42182 = CARTESIAN_POINT ( 'NONE',  ( -2.266590686148945544, 31.38708216824730002, -7.082119434687050408 ) ) ;
#42183 = CARTESIAN_POINT ( 'NONE',  ( 17.84635730667655906, 33.63791097397319163, 6.500000000000019540 ) ) ;
#42184 = CARTESIAN_POINT ( 'NONE',  ( 2.791683348922240793, 21.63393115100078745, 7.208316651077764092 ) ) ;
#42185 = CARTESIAN_POINT ( 'NONE',  ( 7.084665262690076126, 2.022018677488170990, -10.88017736071110164 ) ) ;
#42186 = CARTESIAN_POINT ( 'NONE',  ( 12.63842701281683922, 64.55059781766745175, -9.846743663894590881 ) ) ;
#42187 = EDGE_LOOP ( 'NONE', ( #51484, #30337, #81323, #93424 ) ) ;
#42188 = CYLINDRICAL_SURFACE ( 'NONE', #95649, 11.92686044187656513 ) ;
#42189 = CARTESIAN_POINT ( 'NONE',  ( 6.903457398626330566, -84.61157762779829739, 3.750000000000001332 ) ) ;
#42190 = CARTESIAN_POINT ( 'NONE',  ( 19.42250999205614193, 20.14701867748817321, 5.440088680355555262 ) ) ;
#42191 = CARTESIAN_POINT ( 'NONE',  ( 4.559911319644449179, 58.89701867748817676, 9.422509992056141925 ) ) ;
#42192 = CARTESIAN_POINT ( 'NONE',  ( 10.00000000000000000, 30.55374883491397142, -14.16423886937410082 ) ) ;
#42193 = CARTESIAN_POINT ( 'NONE',  ( 10.00000000000000000, 4.758931151000784787, -9.846743663894594434 ) ) ;
#42194 = CARTESIAN_POINT ( 'NONE',  ( 18.52753015748617571, 53.09226448433412315, 4.923371831947298993 ) ) ;
#42195 = CARTESIAN_POINT ( 'NONE',  ( 10.00000000000000000, 36.81368534415484106, -10.88017736071110342 ) ) ;
#42196 = LINE ( 'NONE', #88163, #51138 ) ;
#42197 = CARTESIAN_POINT ( 'NONE',  ( 6.879999999999995453, 43.00000000000000000, 4.250000000000000000 ) ) ;
#42198 = VERTEX_POINT ( 'NONE', #33871 ) ;
#42199 = LINE ( 'NONE', #95176, #78646 ) ;
#42200 = VERTEX_POINT ( 'NONE', #27860 ) ;
#42201 = ORIENTED_EDGE ( 'NONE', *, *, #36949, .F. ) ;
#42202 = DIRECTION ( 'NONE',  ( -0.5075383629606967650, 0.000000000000000000, -0.8616291604415300398 ) ) ;
#42203 = CARTESIAN_POINT ( 'NONE',  ( -0.3689425029237881626, 2.428748834913967869, 10.36894250292379027 ) ) ;
#42204 = CARTESIAN_POINT ( 'NONE',  ( 17.08211943468705130, 8.470415501580635720, 12.26659068614894998 ) ) ;
#42205 = CARTESIAN_POINT ( 'NONE',  ( 10.00000000000000000, 60.55374883491397497, -14.16423886937410082 ) ) ;
#42206 = CARTESIAN_POINT ( 'NONE',  ( 5.076628168052704559, 55.17559781766745175, -8.527530157486179263 ) ) ;
#42207 = CARTESIAN_POINT ( 'NONE',  ( 19.84674366389459266, 33.71726448433410894, -2.638427012816827677 ) ) ;
#42208 = CARTESIAN_POINT ( 'NONE',  ( -0.7262372900963632860, 0.05317965760449581969, 5.275332923266317309 ) ) ;
#42210 = CARTESIAN_POINT ( 'NONE',  ( -2.816281873526473856, -0.6680319967362464695, 3.434112377981055619 ) ) ;
#42209 = CARTESIAN_POINT ( 'NONE',  ( 2.035157376598822676, 32.43868534415483396, -7.964842623401177768 ) ) ;
#42211 = CARTESIAN_POINT ( 'NONE',  ( -4.164238869374098151, 6.595415501580634832, -3.795296366450310543 ) ) ;
#42212 = CARTESIAN_POINT ( 'NONE',  ( -4.164238869374099927, 52.01208216824729647, 3.795296366450308767 ) ) ;
#42213 = CARTESIAN_POINT ( 'NONE',  ( 10.00000000000000000, 1.813685344154838175, -10.88017736071110342 ) ) ;
#42214 = CARTESIAN_POINT ( 'NONE',  ( -2.826948239413729080, 0.2306972965111893925, -14.67127868811028968 ) ) ;
#42215 = LINE ( 'NONE', #72200, #31581 ) ;
#42216 = CARTESIAN_POINT ( 'NONE',  ( -8.527530157486182816, -39.40773551566587685, -4.923371831947288335 ) ) ;
#42217 = ORIENTED_EDGE ( 'NONE', *, *, #98591, .F. ) ;
#42218 = B_SPLINE_CURVE_WITH_KNOTS ( 'NONE', 3,
 ( #24456, #86429, #40934, #17449, #8939, #63416 ),
 .UNSPECIFIED., .F., .F.,
 ( 4, 2, 4 ),
 ( 0.000000000000000000, 0.0002701661927229247651, 0.0005403323854458495301 ),
 .UNSPECIFIED. ) ;
#42219 = CARTESIAN_POINT ( 'NONE',  ( 0.000000000000000000, 14.49999999999999822, 0.000000000000000000 ) ) ;
#42220 = ORIENTED_EDGE ( 'NONE', *, *, #92118, .T. ) ;
#42221 = CARTESIAN_POINT ( 'NONE',  ( 18.52753015748617571, 28.09226448433411960, 4.923371831947298993 ) ) ;
#42222 = ORIENTED_EDGE ( 'NONE', *, *, #97240, .T. ) ;
#42223 = CARTESIAN_POINT ( 'NONE',  ( 10.00000000000000000, 30.55374883491397142, -14.16423886937410082 ) ) ;
#42224 = CARTESIAN_POINT ( 'NONE',  ( 12.63842701281683034, 32.46726448433412315, 9.846743663894596210 ) ) ;
#42225 = CARTESIAN_POINT ( 'NONE',  ( 12.91533473730993009, 56.60535201082151247, -10.88017736071109987 ) ) ;
#42226 = EDGE_CURVE ( 'NONE', #79846, #23173, #57567, .T. ) ;
#42227 = CARTESIAN_POINT ( 'NONE',  ( 0.000000000000000000, 0.000000000000000000, 0.000000000000000000 ) ) ;
#42228 = CARTESIAN_POINT ( 'NONE',  ( 17.96484262340118221, 56.18868534415484817, -7.964842623401177768 ) ) ;
#42229 = CIRCLE ( 'NONE', #707, 0.2500000000000002220 ) ;
#42230 = CARTESIAN_POINT ( 'NONE',  ( 13.43411237798106583, 62.66530133659708923, -12.81628187352647252 ) ) ;
#42231 = CARTESIAN_POINT ( 'NONE',  ( 9.382169495545415572, 7.248634669930418717, -9.382169495545422677 ) ) ;
#42232 = ORIENTED_EDGE ( 'NONE', *, *, #76596, .F. ) ;
#42233 = CARTESIAN_POINT ( 'NONE',  ( 13.79529636645031943, 15.34541550158063750, -14.16423886937409904 ) ) ;
#42234 = ORIENTED_EDGE ( 'NONE', *, *, #45564, .T. ) ;
#42235 = ORIENTED_EDGE ( 'NONE', *, *, #68466, .T. ) ;
#42236 = CARTESIAN_POINT ( 'NONE',  ( 6.565887622018943937, 48.08196800326375353, -12.81628187352647608 ) ) ;
#42237 = CARTESIAN_POINT ( 'NONE',  ( 19.42250999205614548, 15.98035201082150714, -5.440088680355545492 ) ) ;
#42238 = CARTESIAN_POINT ( 'NONE',  ( 19.84674366389459266, 23.71726448433412315, -2.638427012816827677 ) ) ;
#42239 = CARTESIAN_POINT ( 'NONE',  ( 7.084665262690076126, 17.02201867748817676, -10.88017736071110164 ) ) ;
#42240 = CARTESIAN_POINT ( 'NONE',  ( -1.099225684535947600, 59.54030133659708923, 6.408140936763237150 ) ) ;
#42241 = CARTESIAN_POINT ( 'NONE',  ( -46.20769938831809753, 103.7415672121655348, -6.113268130405502987 ) ) ;
#42242 = CARTESIAN_POINT ( 'NONE',  ( 5.076628168052703671, 26.84226448433411960, 8.527530157486179263 ) ) ;
#42243 = CARTESIAN_POINT ( 'NONE',  ( 19.05914839598885990, 19.96693863883976405, 6.499999999999943157 ) ) ;
#42244 = ADVANCED_FACE ( 'NONE', ( #26883 ), #49871, .F. ) ;
#42245 = CARTESIAN_POINT ( 'NONE',  ( 4.559911319644449179, 68.89701867748817676, 9.422509992056141925 ) ) ;
#42246 = CARTESIAN_POINT ( 'NONE',  ( -1.926860441876562025, 44.47997603579418069, -3.195792623639529761 ) ) ;
#42247 = CARTESIAN_POINT ( 'NONE',  ( 2.791683348922237240, 0.3839311510007847872, -7.208316651077763204 ) ) ;
#42248 = EDGE_CURVE ( 'NONE', #71871, #54278, #12090, .T. ) ;
#42249 = CARTESIAN_POINT ( 'NONE',  ( 13.43411237798106583, 22.66530133659708923, -12.81628187352647252 ) ) ;
#42250 = DIRECTION ( 'NONE',  ( 0.9970872288863216193, 0.07626964003977222684, 0.000000000000000000 ) ) ;
#42251 = CARTESIAN_POINT ( 'NONE',  ( 18.52753015748618282, 43.92559781766745175, -4.923371831947291888 ) ) ;
#42252 = CARTESIAN_POINT ( 'NONE',  ( 18.17884179759834851, 28.66688879859530559, -6.499999999999984901 ) ) ;
#42253 = CARTESIAN_POINT ( 'NONE',  ( 10.00000000000000178, 23.05374883491397142, 14.16423886937410082 ) ) ;
#42254 = CARTESIAN_POINT ( 'NONE',  ( 14.92337183194729988, 29.34226448433411960, -8.527530157486177487 ) ) ;
#42255 = CARTESIAN_POINT ( 'NONE',  ( 6.565887622018943937, 38.08196800326376064, -12.81628187352647608 ) ) ;
#42257 = CARTESIAN_POINT ( 'NONE',  ( 20.15039907845753575, 15.60158574516642815, -6.262539305110077059 ) ) ;
#42256 = CARTESIAN_POINT ( 'NONE',  ( 3.836325488036083087, 15.00000000000000000, 14.50112432709425114 ) ) ;
#42258 = CARTESIAN_POINT ( 'NONE',  ( 4.559911319644449179, 68.89701867748817676, 9.422509992056141925 ) ) ;
#42259 = CARTESIAN_POINT ( 'NONE',  ( 16.40814093676324603, 7.456968003263754419, -11.09922568453594671 ) ) ;
#42260 = CARTESIAN_POINT ( 'NONE',  ( -27.43587634952537968, 22.49999999999998934, -10.00000000000000000 ) ) ;
#42261 = AXIS2_PLACEMENT_3D ( 'NONE', #93122, #32117, #92152 ) ;
#42262 = CARTESIAN_POINT ( 'NONE',  ( 18.52753015748617571, 38.09226448433412315, 4.923371831947298993 ) ) ;
#42263 = CARTESIAN_POINT ( 'NONE',  ( 2.035157376598822676, 27.43868534415483396, -7.964842623401177768 ) ) ;
#42264 = CARTESIAN_POINT ( 'NONE',  ( 13.43411237798105340, 25.58196800326374998, 12.81628187352647963 ) ) ;
#42265 = CARTESIAN_POINT ( 'NONE',  ( 14.92337183194729633, 32.67559781766745175, 8.527530157486181039 ) ) ;
#42266 = CARTESIAN_POINT ( 'NONE',  ( 14.99847009497950800, 14.49999999999999112, 0.2142307401081135487 ) ) ;
#42267 = CARTESIAN_POINT ( 'NONE',  ( 4.559911319644449179, 27.23035201082150536, -9.422509992056141925 ) ) ;
#42268 = ORIENTED_EDGE ( 'NONE', *, *, #92818, .T. ) ;
#42269 = CARTESIAN_POINT ( 'NONE',  ( -9.742785792574940373, 2.505135511184877206, -5.624999999999991118 ) ) ;
#42270 = CARTESIAN_POINT ( 'NONE',  ( 6.910409932109719655, -84.29236789247111972, 2.749999999999999556 ) ) ;
#42272 = CARTESIAN_POINT ( 'NONE',  ( -0.8801773607111009756, 33.06368534415484106, 1.068504757029289695E-15 ) ) ;
#42271 = CARTESIAN_POINT ( 'NONE',  ( 14.92337183194729988, 59.34226448433412315, -8.527530157486177487 ) ) ;
#42274 = B_SPLINE_CURVE_WITH_KNOTS ( 'NONE', 3,
 ( #42423, #87906, #19420, #95925, #3934, #10934 ),
 .UNSPECIFIED., .F., .F.,
 ( 4, 2, 4 ),
 ( 3.409110551496114428E-05, 0.0004400426677367863006, 0.0008459942299586114840 ),
 .UNSPECIFIED. ) ;
#42273 = DIRECTION ( 'NONE',  ( 0.000000000000000000, 1.000000000000000000, 0.000000000000000000 ) ) ;
#42275 = CARTESIAN_POINT ( 'NONE',  ( 17.96484262340118221, 51.18868534415483396, -7.964842623401177768 ) ) ;
#42276 = CARTESIAN_POINT ( 'NONE',  ( 7.084665262690076126, 22.02201867748817321, -10.88017736071110164 ) ) ;
#42277 = CARTESIAN_POINT ( 'NONE',  ( -0.4957494408796453977, 15.11603861882761812, -9.500000000000000000 ) ) ;
#42278 = VECTOR ( 'NONE', #88306, 1000.000000000000000 ) ;
#42279 = CARTESIAN_POINT ( 'NONE',  ( 10.00000000000000000, 49.75893115100078745, -9.846743663894594434 ) ) ;
#42280 = CARTESIAN_POINT ( 'NONE',  ( 20.36894250292379738, 49.92874883491396787, -10.36894250292379027 ) ) ;
#42281 = EDGE_CURVE ( 'NONE', #10227, #38291, #92569, .T. ) ;
#42282 = CARTESIAN_POINT ( 'NONE',  ( -4.164238869374098151, 6.595415501580634832, -3.795296366450310543 ) ) ;
#42283 = CARTESIAN_POINT ( 'NONE',  ( 2.917880565312950480, 40.97041550158063217, -12.26659068614894821 ) ) ;
#42284 = CARTESIAN_POINT ( 'NONE',  ( 10.00000000000000178, 10.37363466993041961, 12.81628187352647608 ) ) ;
#42285 = CARTESIAN_POINT ( 'NONE',  ( -7.124966304139052298, -78.82422094453229988, 2.750000000000000000 ) ) ;
#42286 = ORIENTED_EDGE ( 'NONE', *, *, #87259, .T. ) ;
#42287 = CARTESIAN_POINT ( 'NONE',  ( 10.00000000000000178, 4.313685344154837509, 10.88017736071110342 ) ) ;
#42288 = CARTESIAN_POINT ( 'NONE',  ( 12.63842701281683922, 34.55059781766745886, -9.846743663894590881 ) ) ;
#42289 = CARTESIAN_POINT ( 'NONE',  ( 19.72487221294570858, 70.00000000000000000, 6.500000000000000888 ) ) ;
#42290 = CARTESIAN_POINT ( 'NONE',  ( 7.084665262690076126, 59.10535201082150536, 10.88017736071109987 ) ) ;
#42291 = CIRCLE ( 'NONE', #3979, 15.00000000000000000 ) ;
#42292 = CARTESIAN_POINT ( 'NONE',  ( -0.8801773607111008646, 28.27201867748817321, 2.915334737309923430 ) ) ;
#42293 = DIRECTION ( 'NONE',  ( 0.000000000000000000, 0.000000000000000000, -1.000000000000000000 ) ) ;
#42294 = CARTESIAN_POINT ( 'NONE',  ( 13.43411237798106583, 22.66530133659708923, -12.81628187352647252 ) ) ;
#42295 = CARTESIAN_POINT ( 'NONE',  ( 2.791683348922240793, 31.63393115100078745, 7.208316651077764092 ) ) ;
#42296 = ORIENTED_EDGE ( 'NONE', *, *, #45407, .T. ) ;
#42297 = FACE_OUTER_BOUND ( 'NONE', #18288, .T. ) ;
#42298 = CARTESIAN_POINT ( 'NONE',  ( 24.16423886937409904, 64.09541550158064638, 3.795296366450317205 ) ) ;
#42299 = CARTESIAN_POINT ( 'NONE',  ( -4.164238869374099039, 46.80374883491397497, 8.674139862899312516E-16 ) ) ;
#42300 = CARTESIAN_POINT ( 'NONE',  ( 15.44008868035555260, 34.73035201082151247, 9.422509992056143702 ) ) ;
#42301 = CARTESIAN_POINT ( 'NONE',  ( -0.8801773607110991993, 52.85535201082151247, -2.915334737309923874 ) ) ;
#42302 = DIRECTION ( 'NONE',  ( -0.9799247046208282574, 0.000000000000000000, -0.1993679344172039347 ) ) ;
#42303 = CARTESIAN_POINT ( 'NONE',  ( 10.93147959995856944, -92.98161664596344167, -3.999999999999999112 ) ) ;
#42304 = CARTESIAN_POINT ( 'NONE',  ( 5.076628168052704559, 15.17559781766745175, -8.527530157486179263 ) ) ;
#42305 = PRESENTATION_STYLE_ASSIGNMENT (( #34279 ) ) ;
#42306 = SURFACE_STYLE_FILL_AREA ( #71337 ) ;
#42307 = CARTESIAN_POINT ( 'NONE',  ( 17.20831665107776587, 19.13393115100078035, -7.208316651077762316 ) ) ;
#42308 = CARTESIAN_POINT ( 'NONE',  ( 10.00000000000000178, 47.25893115100078745, 9.846743663894594434 ) ) ;
#42309 = CARTESIAN_POINT ( 'NONE',  ( 20.88017736071110875, 20.77201867748816611, -2.915334737309920765 ) ) ;
#42310 = UNCERTAINTY_MEASURE_WITH_UNIT (LENGTH_MEASURE( 1.000000000000000082E-05 ), #60788, 'distance_accuracy_value', 'NONE');
#42311 = ORIENTED_EDGE ( 'NONE', *, *, #27259, .F. ) ;
#42312 = CARTESIAN_POINT ( 'NONE',  ( 16.40814093676323893, 40.79030133659708923, 11.09922568453595026 ) ) ;
#42313 = CIRCLE ( 'NONE', #63006, 11.92686044187656513 ) ;
#42314 = CARTESIAN_POINT ( 'NONE',  ( -6.581680125707233486, -88.31141629936868753, -2.500000000000000000 ) ) ;
#42315 = CARTESIAN_POINT ( 'NONE',  ( -0.8801773607111009756, 63.06368534415484106, 1.068504757029289695E-15 ) ) ;
#42316 = CARTESIAN_POINT ( 'NONE',  ( 2.791683348922237240, 35.38393115100079456, -7.208316651077763204 ) ) ;
#42318 = CARTESIAN_POINT ( 'NONE',  ( 2.791683348922237240, 20.38393115100078745, -7.208316651077763204 ) ) ;
#42317 = CARTESIAN_POINT ( 'NONE',  ( 17.08211943468705840, 55.13708216824731068, -12.26659068614894466 ) ) ;
#42319 = CARTESIAN_POINT ( 'NONE',  ( 9.898881779040729967, 15.00000000000000000, -10.25059215482576214 ) ) ;
#42320 = CARTESIAN_POINT ( 'NONE',  ( 18.52753015748618282, 63.92559781766745886, -4.923371831947291888 ) ) ;
#42321 = CARTESIAN_POINT ( 'NONE',  ( 17.08211943468705840, 30.13708216824730357, -12.26659068614894466 ) ) ;
#42322 = CARTESIAN_POINT ( 'NONE',  ( 5.076628168052703671, 46.84226448433412315, 8.527530157486179263 ) ) ;
#42323 = DIRECTION ( 'NONE',  ( 0.000000000000000000, 1.000000000000000000, 0.000000000000000000 ) ) ;
#42324 = CARTESIAN_POINT ( 'NONE',  ( 0.5774900079438590739, 22.64701867748817321, -5.440088680355550821 ) ) ;
#42325 = CARTESIAN_POINT ( 'NONE',  ( 19.42250999205614548, 55.98035201082150536, -5.440088680355545492 ) ) ;
#42326 = CARTESIAN_POINT ( 'NONE',  ( 0.1532563361054100626, 55.80059781766744464, -2.638427012816831230 ) ) ;
#42327 = VERTEX_POINT ( 'NONE', #94393 ) ;
#42328 = CARTESIAN_POINT ( 'NONE',  ( 22.81628187352647785, 51.41530133659708923, 3.434112377981063169 ) ) ;
#42329 = APPLICATION_CONTEXT ( 'automotive_design' ) ;
#42330 = CARTESIAN_POINT ( 'NONE',  ( 19.42250999205614548, 55.98035201082150536, -5.440088680355545492 ) ) ;
#42331 = ORIENTED_EDGE ( 'NONE', *, *, #71019, .T. ) ;
#42332 = CARTESIAN_POINT ( 'NONE',  ( -9.240973841163452107, 15.00000000000000000, -11.17382667070385160 ) ) ;
#42333 = FILL_AREA_STYLE ('',( #87331 ) ) ;
#42334 = EDGE_CURVE ( 'NONE', #22610, #25163, #56411, .T. ) ;
#42335 = CARTESIAN_POINT ( 'NONE',  ( 0.5774900079438607392, 63.48035201082149825, 5.440088680355550821 ) ) ;
#42336 = ORIENTED_EDGE ( 'NONE', *, *, #11961, .F. ) ;
#42337 = CARTESIAN_POINT ( 'NONE',  ( 19.42250999205614193, 60.14701867748817676, 5.440088680355555262 ) ) ;
#42338 = CARTESIAN_POINT ( 'NONE',  ( 17.96484262340118221, 21.18868534415483396, -7.964842623401177768 ) ) ;
#42339 = CARTESIAN_POINT ( 'NONE',  ( 18.72515096720578853, 60.05509018479938277, 6.499999999999877431 ) ) ;
#42340 = CARTESIAN_POINT ( 'NONE',  ( 14.56372689393330688, 14.95037103587380756, -2.356940382833013548 ) ) ;
#42341 = CARTESIAN_POINT ( 'NONE',  ( 4.559911319644449179, 2.230352010821504916, -9.422509992056141925 ) ) ;
#42342 = CARTESIAN_POINT ( 'NONE',  ( 7.361572987183170547, 12.05059781766744997, 9.846743663894590881 ) ) ;
#42343 = CARTESIAN_POINT ( 'NONE',  ( 24.16423886937409904, 14.09541550158063217, 3.795296366450317205 ) ) ;
#42344 = CARTESIAN_POINT ( 'NONE',  ( 12.91533473730993009, 21.60535201082150536, -10.88017736071109987 ) ) ;
#42345 = CARTESIAN_POINT ( 'NONE',  ( 14.92337183194729988, 54.34226448433412315, -8.527530157486177487 ) ) ;
#42346 = ORIENTED_EDGE ( 'NONE', *, *, #40916, .T. ) ;
#42347 = CARTESIAN_POINT ( 'NONE',  ( 19.84674366389459266, 58.30059781766745886, 2.638427012816836559 ) ) ;
#42348 = VERTEX_POINT ( 'NONE', #72866 ) ;
#42349 = AXIS2_PLACEMENT_3D ( 'NONE', #12977, #56524, #96505 ) ;
#42350 = CYLINDRICAL_SURFACE ( 'NONE', #74937, 15.00000000000000000 ) ;
#42351 = CARTESIAN_POINT ( 'NONE',  ( 15.44008868035555793, 51.39701867748816966, -9.422509992056140149 ) ) ;
#42352 = CARTESIAN_POINT ( 'NONE',  ( 27.50000000000000355, 35.99999999999997158, 7.000000000000000888 ) ) ;
#42353 = EDGE_CURVE ( 'NONE', #46257, #49695, #37656, .T. ) ;
#42354 = CARTESIAN_POINT ( 'NONE',  ( 10.00000000000000000, 32.87363466993042493, -12.81628187352647608 ) ) ;
#42356 = CARTESIAN_POINT ( 'NONE',  ( -8.758038983380448173, 2.271305648288091561, -7.488716559648692872 ) ) ;
#42355 = CARTESIAN_POINT ( 'NONE',  ( 4.559911319644449179, 13.89701867748817143, 9.422509992056141925 ) ) ;
#42357 = CARTESIAN_POINT ( 'NONE',  ( 7.084665262690076126, 59.10535201082150536, 10.88017736071109987 ) ) ;
#42358 = CARTESIAN_POINT ( 'NONE',  ( 2.917880565312948704, 67.63708216824730357, 12.26659068614894643 ) ) ;
#42359 = ORIENTED_EDGE ( 'NONE', *, *, #68707, .T. ) ;
#42360 = EDGE_CURVE ( 'NONE', #56243, #30649, #57863, .T. ) ;
#42361 = CARTESIAN_POINT ( 'NONE',  ( 19.38216949554541202, 45.99863466993041072, 9.382169495545424454 ) ) ;
#42362 = CARTESIAN_POINT ( 'NONE',  ( 10.00000000000000000, 26.81368534415484106, -10.88017736071110342 ) ) ;
#42363 = CARTESIAN_POINT ( 'NONE',  ( -33.19000000000001194, 92.00000000000000000, -9.500000000000000000 ) ) ;
#42364 = ORIENTED_EDGE ( 'NONE', *, *, #52104, .T. ) ;
#42365 = CARTESIAN_POINT ( 'NONE',  ( 10.00000000000000000, 42.87363466993042493, -12.81628187352647608 ) ) ;
#42366 = CARTESIAN_POINT ( 'NONE',  ( -0.8801773607110991993, 32.85535201082151247, -2.915334737309923874 ) ) ;
#42367 = CARTESIAN_POINT ( 'NONE',  ( 5.076628168052703671, 56.84226448433412315, 8.527530157486179263 ) ) ;
#42368 = EDGE_CURVE ( 'NONE', #6749, #34270, #50780, .T. ) ;
#42369 = ORIENTED_EDGE ( 'NONE', *, *, #55560, .T. ) ;
#42370 = CARTESIAN_POINT ( 'NONE',  ( 5.076628168052703671, 56.84226448433412315, 8.527530157486179263 ) ) ;
#42372 = CARTESIAN_POINT ( 'NONE',  ( 7.361572987183169658, 54.96726448433413026, -9.846743663894592657 ) ) ;
#42371 = CARTESIAN_POINT ( 'NONE',  ( 4.782492776157768688, 54.66414256906417535, 3.000000000000000000 ) ) ;
#42373 = CARTESIAN_POINT ( 'NONE',  ( 0.5774900079438607392, 28.48035201082150891, 5.440088680355550821 ) ) ;
#42374 = CARTESIAN_POINT ( 'NONE',  ( 2.791683348922237240, 35.38393115100079456, -7.208316651077763204 ) ) ;
#42375 = CARTESIAN_POINT ( 'NONE',  ( 11.35178980618967337, 0.5000000000000004441, 9.804941009311999522 ) ) ;
#42376 = DIRECTION ( 'NONE',  ( 0.000000000000000000, 1.000000000000000000, 0.000000000000000000 ) ) ;
#42378 = CARTESIAN_POINT ( 'NONE',  ( 12.63842701281683034, 7.467264484334118713, 9.846743663894596210 ) ) ;
#42377 = CARTESIAN_POINT ( 'NONE',  ( 0.1532563361054100626, 45.80059781766745886, -2.638427012816831230 ) ) ;
#42380 = EDGE_LOOP ( 'NONE', ( #86874, #64487, #11935, #69528, #44898, #71646 ) ) ;
#42379 = CARTESIAN_POINT ( 'NONE',  ( 2.791683348922240793, 61.63393115100079456, 7.208316651077764092 ) ) ;
#42381 = CARTESIAN_POINT ( 'NONE',  ( 9.402796353261059892, 14.63606911086599283, 11.68706210897767761 ) ) ;
#42382 = CARTESIAN_POINT ( 'NONE',  ( 6.565887622018943937, 33.08196800326374643, -12.81628187352647608 ) ) ;
#42383 = CARTESIAN_POINT ( 'NONE',  ( 19.84674366389459621, 43.50893115100078745, 7.409399052514197653E-17 ) ) ;
#42384 = CARTESIAN_POINT ( 'NONE',  ( 11.25000000000000178, 7.618033628982655792, -2.373340393710807175E-15 ) ) ;
#42385 = CARTESIAN_POINT ( 'NONE',  ( 17.08211943468705130, 53.47041550158063217, 12.26659068614894998 ) ) ;
#42386 = CARTESIAN_POINT ( 'NONE',  ( 17.20831665107776587, 34.13393115100078745, -7.208316651077762316 ) ) ;
#42387 = CARTESIAN_POINT ( 'NONE',  ( 19.67387888393819750, 87.39346174270656320, 5.439610960095202508 ) ) ;
#42388 = CARTESIAN_POINT ( 'NONE',  ( -0.3689425029237898834, 56.17874883491396076, -10.36894250292378850 ) ) ;
#42389 = CARTESIAN_POINT ( 'NONE',  ( 7.684764310694878198, 0.5000000000000004441, -12.88194075009934991 ) ) ;
#42390 = CARTESIAN_POINT ( 'NONE',  ( -0.8801773607110991993, 2.855352010821504471, -2.915334737309923874 ) ) ;
#42391 = CARTESIAN_POINT ( 'NONE',  ( 20.36894250292379738, 34.92874883491396076, -10.36894250292379027 ) ) ;
#42393 = DIRECTION ( 'NONE',  ( 0.000000000000000000, 1.000000000000000000, 0.000000000000000000 ) ) ;
#42392 = CARTESIAN_POINT ( 'NONE',  ( 10.00000000000000178, 33.05374883491396787, 14.16423886937410082 ) ) ;
#42394 = CARTESIAN_POINT ( 'NONE',  ( 19.72487221294570858, 70.00000000000000000, 6.500000000000000888 ) ) ;
#42395 = EDGE_CURVE ( 'NONE', #67582, #56519, #48890, .T. ) ;
#42396 = CARTESIAN_POINT ( 'NONE',  ( 0.1532563361054100626, 5.800597817667452638, -2.638427012816831230 ) ) ;
#42398 = CARTESIAN_POINT ( 'NONE',  ( -2.816281873526473856, -0.6680319967362464695, 3.434112377981055619 ) ) ;
#42397 = CARTESIAN_POINT ( 'NONE',  ( 6.910443788307254032, -84.29081344371353168, 2.500000000014485302 ) ) ;
#42399 = VERTEX_POINT ( 'NONE', #21865 ) ;
#42400 = CARTESIAN_POINT ( 'NONE',  ( 20.88017736071110164, 55.35535201082149825, 2.915334737309930979 ) ) ;
#42401 = AXIS2_PLACEMENT_3D ( 'NONE', #39212, #69699, #1229 ) ;
#42402 = CARTESIAN_POINT ( 'NONE',  ( 10.83696084481538691, -98.17058944465519232, 3.750000000000000000 ) ) ;
#42403 = EDGE_CURVE ( 'NONE', #38271, #37318, #21361, .T. ) ;
#42404 = CARTESIAN_POINT ( 'NONE',  ( 1.274849032794294290, 53.57228050351032067, 6.499999999999979572 ) ) ;
#42405 = CARTESIAN_POINT ( 'NONE',  ( 17.20831665107776587, 59.13393115100078745, -7.208316651077762316 ) ) ;
#42406 = CARTESIAN_POINT ( 'NONE',  ( 14.49440716394873618, 15.00000000000000000, -0.4026921475166200803 ) ) ;
#42407 = ORIENTED_EDGE ( 'NONE', *, *, #64664, .F. ) ;
#42408 = CARTESIAN_POINT ( 'NONE',  ( 24.16423886937409904, 29.09541550158063572, 3.795296366450317205 ) ) ;
#42409 = LINE ( 'NONE', #71912, #29492 ) ;
#42410 = CARTESIAN_POINT ( 'NONE',  ( -4.259797194938747644, -13.81744876718660819, -2.500000000001613820 ) ) ;
#42411 = CARTESIAN_POINT ( 'NONE',  ( 20.88017736071110164, 25.35535201082150891, 2.915334737309930979 ) ) ;
#42412 = CARTESIAN_POINT ( 'NONE',  ( 19.38216949554541202, 25.99863466993042138, 9.382169495545424454 ) ) ;
#42413 = CARTESIAN_POINT ( 'NONE',  ( 0.000000000000000000, 84.07179676972448590, -12.00000000000000000 ) ) ;
#42414 = CARTESIAN_POINT ( 'NONE',  ( 19.84674366389459266, 13.30059781766745353, 2.638427012816836559 ) ) ;
#42415 = EDGE_LOOP ( 'NONE', ( #23069, #12132, #75640, #4018 ) ) ;
#42416 = CARTESIAN_POINT ( 'NONE',  ( 4.879999999999991900, 76.07179676972444327, 4.250000000000000000 ) ) ;
#42417 = EDGE_CURVE ( 'NONE', #30382, #5711, #45638, .T. ) ;
#42418 = CARTESIAN_POINT ( 'NONE',  ( -0.3689425029237898834, 31.17874883491396787, -10.36894250292378850 ) ) ;
#42419 = FILL_AREA_STYLE ('',( #72899 ) ) ;
#42420 = SURFACE_STYLE_USAGE ( .BOTH. , #56916 ) ;
#42421 = CARTESIAN_POINT ( 'NONE',  ( 15.44008868035555260, 9.730352010821505360, 9.422509992056143702 ) ) ;
#42422 = CARTESIAN_POINT ( 'NONE',  ( 13.21236992757670059, -0.03417435944610275333, 5.338143956176803151 ) ) ;
#42423 = CARTESIAN_POINT ( 'NONE',  ( 4.431036607602561794, 0.5000000000000004441, -14.33059365769911153 ) ) ;
#42424 = CARTESIAN_POINT ( 'NONE',  ( 15.44008868035555793, 36.39701867748816966, -9.422509992056140149 ) ) ;
#42425 = CARTESIAN_POINT ( 'NONE',  ( 2.035157376598824452, 53.68868534415484817, 7.964842623401179544 ) ) ;
#42426 = CARTESIAN_POINT ( 'NONE',  ( -1.099225684535947600, 13.70696800326375353, -6.408140936763238038 ) ) ;
#42427 = CARTESIAN_POINT ( 'NONE',  ( 0.1532563361054082862, 66.21726448433413736, 2.638427012816831674 ) ) ;
#42428 = LINE ( 'NONE', #73897, #2063 ) ;
#42429 = CARTESIAN_POINT ( 'NONE',  ( 17.20831665107776587, 7.883931151000784787, 7.208316651077764980 ) ) ;
#42430 = CARTESIAN_POINT ( 'NONE',  ( 4.559911319644449179, 42.23035201082151247, -9.422509992056141925 ) ) ;
#42431 = MECHANICAL_DESIGN_GEOMETRIC_PRESENTATION_REPRESENTATION (  '', ( #20080 ), #75968 ) ;
#42432 = UNCERTAINTY_MEASURE_WITH_UNIT (LENGTH_MEASURE( 1.000000000000000082E-05 ), #21396, 'distance_accuracy_value', 'NONE');
#42433 = AXIS2_PLACEMENT_3D ( 'NONE', #55918, #2447, #61923 ) ;
#42434 = CARTESIAN_POINT ( 'NONE',  ( 13.43411237798106583, 7.665301336597086568, -12.81628187352647252 ) ) ;
#42435 = CARTESIAN_POINT ( 'NONE',  ( 15.44008868035555793, 61.39701867748817676, -9.422509992056140149 ) ) ;
#42436 = COLOUR_RGB ( '', 0.08235294, 0.09019608, 0.10196078) ;
#42437 = CARTESIAN_POINT ( 'NONE',  ( 0.1532563361054083140, 26.00893115100078745, 1.131784320476157264E-15 ) ) ;
#42438 = CARTESIAN_POINT ( 'NONE',  ( 19.38216949554541202, 45.99863466993041072, 9.382169495545424454 ) ) ;
#42439 = CARTESIAN_POINT ( 'NONE',  ( 19.84674366389459266, 3.717264484334118713, -2.638427012816827677 ) ) ;
#42440 = ORIENTED_EDGE ( 'NONE', *, *, #54731, .T. ) ;
#42441 = CARTESIAN_POINT ( 'NONE',  ( 2.377183314879976805, 55.78593319516822646, -6.500000000000005329 ) ) ;
#42442 = CARTESIAN_POINT ( 'NONE',  ( 18.00000000000000355, 77.07179676972445748, -4.250000000000000000 ) ) ;
#42443 = CARTESIAN_POINT ( 'NONE',  ( 20.88017736071110875, 25.77201867748816966, -2.915334737309920765 ) ) ;
#42444 = CARTESIAN_POINT ( 'NONE',  ( 16.40814093676323893, 55.79030133659708923, 11.09922568453595026 ) ) ;
#42445 = CARTESIAN_POINT ( 'NONE',  ( 18.52753015748618282, 28.92559781766745175, -4.923371831947291888 ) ) ;
#42446 = CARTESIAN_POINT ( 'NONE',  ( 4.559911319644449179, 23.89701867748817321, 9.422509992056141925 ) ) ;
#42447 = CARTESIAN_POINT ( 'NONE',  ( -0.3689425029237881626, 67.42874883491396076, 10.36894250292379027 ) ) ;
#42448 = ORIENTED_EDGE ( 'NONE', *, *, #66289, .F. ) ;
#42449 = CARTESIAN_POINT ( 'NONE',  ( 0.5774900079438590739, 12.64701867748817143, -5.440088680355550821 ) ) ;
#42450 = EDGE_CURVE ( 'NONE', #63634, #67813, #13862, .T. ) ;
#42451 = CARTESIAN_POINT ( 'NONE',  ( 2.035157376598822676, 32.43868534415483396, -7.964842623401177768 ) ) ;
#42453 = CARTESIAN_POINT ( 'NONE',  ( 10.00000000000000178, 24.31368534415484106, 10.88017736071110342 ) ) ;
#42452 = DIRECTION ( 'NONE',  ( -1.084202172485504434E-16, -1.000000000000000000, 0.000000000000000000 ) ) ;
#42454 = VERTEX_POINT ( 'NONE', #5385 ) ;
#42455 = CARTESIAN_POINT ( 'NONE',  ( 0.1532563361054083140, 66.00893115100079456, 1.131784320476157264E-15 ) ) ;
#42456 = CARTESIAN_POINT ( 'NONE',  ( 0.5774900079438607392, 23.48035201082150536, 5.440088680355550821 ) ) ;
#42457 = CARTESIAN_POINT ( 'NONE',  ( 2.791683348922237240, 65.38393115100078035, -7.208316651077763204 ) ) ;
#42458 = CARTESIAN_POINT ( 'NONE',  ( -8.375939845167836850, 15.00000000000000000, 11.52849216984293257 ) ) ;
#42459 = CARTESIAN_POINT ( 'NONE',  ( -2.816281873526473856, 59.12363466993042493, 9.499525473075851096E-16 ) ) ;
#42460 = CARTESIAN_POINT ( 'NONE',  ( 0.8952175423695025724, 68.52576239577081196, 5.990408912944351627 ) ) ;
#42461 = CARTESIAN_POINT ( 'NONE',  ( -0.3689425029237881626, 32.42874883491395366, 10.36894250292379027 ) ) ;
#42462 = CARTESIAN_POINT ( 'NONE',  ( 10.00000000000000000, 36.81368534415484106, -10.88017736071110342 ) ) ;
#42463 = CARTESIAN_POINT ( 'NONE',  ( 4.559911319644449179, 18.89701867748817321, 9.422509992056141925 ) ) ;
#42464 = EDGE_CURVE ( 'NONE', #91634, #25488, #5866, .T. ) ;
#42465 = CARTESIAN_POINT ( 'NONE',  ( -6.898461952320517732, 4.837215022590613936E-16, 12.75387089053304557 ) ) ;
#42466 = CARTESIAN_POINT ( 'NONE',  ( 0.1532563361054100626, 50.80059781766745175, -2.638427012816831230 ) ) ;
#42467 = CARTESIAN_POINT ( 'NONE',  ( 7.361572987183169658, 14.96726448433411960, -9.846743663894592657 ) ) ;
#42468 = CARTESIAN_POINT ( 'NONE',  ( 12.81628187352647252, -33.16803199673624647, -3.434112377981059172 ) ) ;
#42469 = CARTESIAN_POINT ( 'NONE',  ( 10.00000000000000000, 6.813685344154838397, -10.88017736071110342 ) ) ;
#42470 = CARTESIAN_POINT ( 'NONE',  ( 19.84674366389459266, 13.30059781766745353, 2.638427012816836559 ) ) ;
#42471 = CARTESIAN_POINT ( 'NONE',  ( -0.8801773607111009756, 63.06368534415484106, 1.068504757029289695E-15 ) ) ;
#42473 = CARTESIAN_POINT ( 'NONE',  ( 22.81628187352647785, 51.62363466993042493, 6.195893100308588602E-16 ) ) ;
#42472 = CARTESIAN_POINT ( 'NONE',  ( 12.91533473730993009, 21.60535201082150536, -10.88017736071109987 ) ) ;
#42474 = CARTESIAN_POINT ( 'NONE',  ( -0.3689425029237881626, 32.42874883491395366, 10.36894250292379027 ) ) ;
#42475 = CIRCLE ( 'NONE', #42401, 14.49999999999999822 ) ;
#42476 = DIRECTION ( 'NONE',  ( -1.000000000000000000, -0.000000000000000000, -0.000000000000000000 ) ) ;
#42477 = EDGE_CURVE ( 'NONE', #81875, #30157, #59835, .T. ) ;
#42478 = CARTESIAN_POINT ( 'NONE',  ( -2.816281873526473856, 64.12363466993042493, 9.499525473075851096E-16 ) ) ;
#42479 = ORIENTED_EDGE ( 'NONE', *, *, #54863, .T. ) ;
#42480 = CARTESIAN_POINT ( 'NONE',  ( 19.38216949554541557, 7.248634669930421381, -9.382169495545420901 ) ) ;
#42481 = CARTESIAN_POINT ( 'NONE',  ( -1.926860441876564023, 14.68830936912750573, 1.004413902775740781E-15 ) ) ;
#42482 = CARTESIAN_POINT ( 'NONE',  ( 10.00000000000000000, 36.81368534415484106, -10.88017736071110342 ) ) ;
#42484 = EDGE_CURVE ( 'NONE', #11760, #32896, #43691, .T. ) ;
#42483 = CARTESIAN_POINT ( 'NONE',  ( 8.375939845167682307, 0.000000000000000000, 11.52849216984304448 ) ) ;
#42485 = B_SPLINE_CURVE_WITH_KNOTS ( 'NONE', 3,
 ( #32193, #62695, #3200, #25226, #47704, #33182 ),
 .UNSPECIFIED., .F., .F.,
 ( 4, 2, 4 ),
 ( 3.409110551494653465E-05, 0.0004400426677367932937, 0.0008459942299586401069 ),
 .UNSPECIFIED. ) ;
#42486 = ORIENTED_EDGE ( 'NONE', *, *, #91572, .F. ) ;
#42487 = CARTESIAN_POINT ( 'NONE',  ( 1.472469842513823179, 21.42559781766745175, 4.923371831947296329 ) ) ;
#42488 = CARTESIAN_POINT ( 'NONE',  ( 19.84674366389459266, 13.30059781766745353, 2.638427012816836559 ) ) ;
#42489 = CARTESIAN_POINT ( 'NONE',  ( 1.472469842513823179, 21.42559781766745175, 4.923371831947296329 ) ) ;
#42490 = CARTESIAN_POINT ( 'NONE',  ( 17.20831665107776587, 7.883931151000784787, 7.208316651077764980 ) ) ;
#42492 = DIRECTION ( 'NONE',  ( 0.000000000000000000, -0.000000000000000000, -1.000000000000000000 ) ) ;
#42491 = CARTESIAN_POINT ( 'NONE',  ( -0.8801773607111008646, 68.27201867748817676, 2.915334737309923430 ) ) ;
#42493 = CARTESIAN_POINT ( 'NONE',  ( 17.20831665107776587, 7.883931151000784787, 7.208316651077764980 ) ) ;
#42495 = ORIENTED_EDGE ( 'NONE', *, *, #2301, .T. ) ;
#42494 = CARTESIAN_POINT ( 'NONE',  ( 10.00000000000000000, 19.75893115100078390, -9.846743663894594434 ) ) ;
#42496 = VECTOR ( 'NONE', #36690, 1000.000000000000000 ) ;
#42497 = CARTESIAN_POINT ( 'NONE',  ( 10.64017930668211598, 14.49999999999999112, -10.57291749337218256 ) ) ;
#42498 = CARTESIAN_POINT ( 'NONE',  ( 0.1532563361054083140, 66.00893115100079456, 1.131784320476157264E-15 ) ) ;
#42499 = ORIENTED_EDGE ( 'NONE', *, *, #44238, .T. ) ;
#42500 = ORIENTED_EDGE ( 'NONE', *, *, #10969, .T. ) ;
#42501 = CARTESIAN_POINT ( 'NONE',  ( 10.00000000000000000, 6.813685344154838397, -10.88017736071110342 ) ) ;
#42502 = AXIS2_PLACEMENT_3D ( 'NONE', #28208, #35203, #43207 ) ;
#42503 = CARTESIAN_POINT ( 'NONE',  ( -2.266590686148945544, 22.22041550158063572, 7.082119434687048631 ) ) ;
#42504 = UNCERTAINTY_MEASURE_WITH_UNIT (LENGTH_MEASURE( 1.000000000000000082E-05 ), #86783, 'distance_accuracy_value', 'NONE');
#42505 = CARTESIAN_POINT ( 'NONE',  ( 0.000000000000000000, 0.5000000000000004441, 0.000000000000000000 ) ) ;
#42506 = CARTESIAN_POINT ( 'NONE',  ( -0.3689425029237898834, 16.17874883491396076, -10.36894250292378850 ) ) ;
#42507 = CARTESIAN_POINT ( 'NONE',  ( -0.3689425029237881626, 37.42874883491396787, 10.36894250292379027 ) ) ;
#42508 = CARTESIAN_POINT ( 'NONE',  ( 7.084665262690076126, 32.02201867748816966, -10.88017736071110164 ) ) ;
#42509 = CARTESIAN_POINT ( 'NONE',  ( 6.937721053838227014, -80.66520463107747219, -2.750000000000000000 ) ) ;
#42510 = CARTESIAN_POINT ( 'NONE',  ( 18.52753015748617571, 13.09226448433411960, 4.923371831947298993 ) ) ;
#42512 = CARTESIAN_POINT ( 'NONE',  ( 7.361572987183169658, 14.96726448433411960, -9.846743663894592657 ) ) ;
#42511 = CARTESIAN_POINT ( 'NONE',  ( -0.8801773607110991993, 62.85535201082150536, -2.915334737309923874 ) ) ;
#42513 = CARTESIAN_POINT ( 'NONE',  ( 20.88017736071110519, 5.563685344154838397, 2.639326808657452039E-16 ) ) ;
#42514 = CARTESIAN_POINT ( 'NONE',  ( -2.816281873526473856, 39.12363466993041783, 9.499525473075851096E-16 ) ) ;
#42515 = CARTESIAN_POINT ( 'NONE',  ( 10.00000000000000178, 47.25893115100078745, 9.846743663894594434 ) ) ;
#42516 = CARTESIAN_POINT ( 'NONE',  ( 5.500000000000000000, 61.00000000000000711, -6.000000000000000000 ) ) ;
#42517 = ADVANCED_FACE ( 'NONE', ( #52343 ), #97371, .F. ) ;
#42518 = CARTESIAN_POINT ( 'NONE',  ( 10.00000000000000178, 25.37363466993041783, 12.81628187352647608 ) ) ;
#42519 = CARTESIAN_POINT ( 'NONE',  ( -12.26659068614895354, -28.61291783175269643, -7.082119434687038861 ) ) ;
#42520 = CARTESIAN_POINT ( 'NONE',  ( 0.1532563361054083140, 41.00893115100078745, 1.131784320476157264E-15 ) ) ;
#42521 = CARTESIAN_POINT ( 'NONE',  ( -4.164238869374099039, 11.80374883491396965, 8.674139862899312516E-16 ) ) ;
#42522 = ORIENTED_EDGE ( 'NONE', *, *, #64906, .F. ) ;
#42523 = DIRECTION ( 'NONE',  ( -0.9969173337331284079, 0.000000000000000000, 0.07845909572783860142 ) ) ;
#42524 = CARTESIAN_POINT ( 'NONE',  ( 0.5774900079438607392, 53.48035201082151247, 5.440088680355550821 ) ) ;
#42525 = CARTESIAN_POINT ( 'NONE',  ( 0.5774900079438607392, 48.48035201082150536, 5.440088680355550821 ) ) ;
#42526 = CARTESIAN_POINT ( 'NONE',  ( 17.08211943468705840, 40.13708216824731068, -12.26659068614894466 ) ) ;
#42527 = CARTESIAN_POINT ( 'NONE',  ( 17.20831665107776587, 49.13393115100078745, -7.208316651077762316 ) ) ;
#42528 = CARTESIAN_POINT ( 'NONE',  ( -14.64921366071931530, 14.95037108083259625, -1.748670679920710569 ) ) ;
#42529 = CARTESIAN_POINT ( 'NONE',  ( -0.8801773607111009756, 38.06368534415484106, 1.068504757029289695E-15 ) ) ;
#42530 = CARTESIAN_POINT ( 'NONE',  ( -45.94000000000001194, 99.99999999999998579, 9.500000000000000000 ) ) ;
#42531 = CARTESIAN_POINT ( 'NONE',  ( 7.361572987183169658, 54.96726448433413026, -9.846743663894592657 ) ) ;
#42532 = CARTESIAN_POINT ( 'NONE',  ( 5.440088680355549045, 11.39701867748817854, -9.422509992056141925 ) ) ;
#42533 = CARTESIAN_POINT ( 'NONE',  ( -0.8801773607111009756, 3.063685344154837509, 1.068504757029289695E-15 ) ) ;
#42534 = LINE ( 'NONE', #43027, #18455 ) ;
#42535 = VECTOR ( 'NONE', #63557, 1000.000000000000000 ) ;
#42536 = CARTESIAN_POINT ( 'NONE',  ( 4.559911319644449179, 3.897018677488170990, 9.422509992056141925 ) ) ;
#42537 = CYLINDRICAL_SURFACE ( 'NONE', #60777, 1.500000000000001332 ) ;
#42538 = CARTESIAN_POINT ( 'NONE',  ( 5.076628168052704559, 0.1755978176674514724, -8.527530157486179263 ) ) ;
#42539 = CARTESIAN_POINT ( 'NONE',  ( 7.361572987183169658, 4.967264484334119601, -9.846743663894592657 ) ) ;
#42540 = DIRECTION ( 'NONE',  ( -0.000000000000000000, -1.000000000000000000, -0.000000000000000000 ) ) ;
#42541 = CARTESIAN_POINT ( 'NONE',  ( 1.472469842513823179, 31.42559781766745530, 4.923371831947296329 ) ) ;
#42542 = CARTESIAN_POINT ( 'NONE',  ( 7.084665262690076126, 22.02201867748817321, -10.88017736071110164 ) ) ;
#42543 =( GEOMETRIC_REPRESENTATION_CONTEXT ( 3 ) GLOBAL_UNCERTAINTY_ASSIGNED_CONTEXT ( ( #23130 ) ) GLOBAL_UNIT_ASSIGNED_CONTEXT ( ( #20942, #66924, #74918 ) ) REPRESENTATION_CONTEXT ( 'NONE', 'WORKASPACE' ) );
#42544 = CARTESIAN_POINT ( 'NONE',  ( 6.565887622018943937, 8.081968003263751754, -12.81628187352647608 ) ) ;
#42546 = DIRECTION ( 'NONE',  ( -1.257568779154408793E-17, -1.000000000000000000, 0.000000000000000000 ) ) ;
#42545 = CARTESIAN_POINT ( 'NONE',  ( 10.00000000000000178, 34.31368534415484106, 10.88017736071110342 ) ) ;
#42547 = DIRECTION ( 'NONE',  ( -1.000000000000000000, 0.000000000000000000, 0.000000000000000000 ) ) ;
#42548 = CARTESIAN_POINT ( 'NONE',  ( 16.40814093676323893, 35.79030133659708923, 11.09922568453595026 ) ) ;
#42549 = ORIENTED_EDGE ( 'NONE', *, *, #98116, .T. ) ;
#42550 = CARTESIAN_POINT ( 'NONE',  ( -15.86177583122253765, -0.03417435944610275333, 2.069169861586545700 ) ) ;
#42552 = CARTESIAN_POINT ( 'NONE',  ( 5.056330833737696651, 15.00000000000000000, -13.58983143751348521 ) ) ;
#42551 = CARTESIAN_POINT ( 'NONE',  ( 10.00000000000000178, 15.37363466993042138, 12.81628187352647608 ) ) ;
#42553 = FILL_AREA_STYLE_COLOUR ( '', #77079 ) ;
#42554 = CARTESIAN_POINT ( 'NONE',  ( -0.8801773607111008646, 23.27201867748817676, 2.915334737309923430 ) ) ;
#42555 = CARTESIAN_POINT ( 'NONE',  ( 22.26659068614894466, 58.88708216824729647, 7.082119434687054849 ) ) ;
#42556 = CARTESIAN_POINT ( 'NONE',  ( 1.472469842513823179, 55.59226448433412315, -4.923371831947296329 ) ) ;
#42557 = CARTESIAN_POINT ( 'NONE',  ( 5.076628168052704559, 5.175597817667451750, -8.527530157486179263 ) ) ;
#42558 = CARTESIAN_POINT ( 'NONE',  ( 20.88017736071110875, 65.77201867748817676, -2.915334737309920765 ) ) ;
#42559 = FILL_AREA_STYLE_COLOUR ( '', #60212 ) ;
#42560 = CARTESIAN_POINT ( 'NONE',  ( 20.36894250292379382, 28.67874883491396787, 10.36894250292379205 ) ) ;
#42561 = STYLED_ITEM ( 'NONE', ( #96776 ), #776 ) ;
#42562 =( GEOMETRIC_REPRESENTATION_CONTEXT ( 3 ) GLOBAL_UNCERTAINTY_ASSIGNED_CONTEXT ( ( #87430 ) ) GLOBAL_UNIT_ASSIGNED_CONTEXT ( ( #37746, #68726, #74735 ) ) REPRESENTATION_CONTEXT ( 'NONE', 'WORKASPACE' ) );
#42563 = FACE_OUTER_BOUND ( 'NONE', #58808, .T. ) ;
#42564 =( BOUNDED_SURFACE ( )  B_SPLINE_SURFACE ( 1, 2, ( 
 ( #20130, #87144, #72143, #35121, #5140, #26163, #87638, #65621, #18668, #49155, #19152, #58114, #79656, #88623, #35631, #89123, #49630, #34627, #51123, #96645, #80139, #50634, #58622, #20634, #81615, #5639, #94655, #41675, #11649, #65126, #67115, #15615, #46099, #38117, #89618, #6125, #45597, #75105, #84100, #91598, #44609, #37125, #21130, #82608, #29590, #82109, #14632, #76095, #45096, #22121, #6612, #8103, #52601, #7114, #83607, #29105, #67621, #98129, #23114, #60092, #90594, #51629, #14125, #83104, #13620, #75603, #7625, #37619, #68113, #98638, #66623, #30089, #60596, #15121, #59607, #91091, #22619, #53095, #68606, #134, #52116, #30584, #53586, #61088, #97640, #76583, #97150, #28621, #59107, #44101, #74611, #36630, #90102, #21630, #25088, #70082, #92086, #631, #8589, #69586, #62065, #23612, #39095, #1106, #94053, #63543, #48047, #9078, #9570, #62556, #39591, #48544, #92568, #69097, #61575, #25574, #77077, #70573, #24094, #31569, #40570, #54563, #46579, #78561, #17089, #93555, #56066, #86561, #18065, #54077, #84592, #79043, #55571, #86070, #1604, #31077, #85575, #47569, #38599, #40072, #17581, #32053, #85079, #16092, #16588, #77562, #47064, #63058, #93060, #24593, #78067, #10071, #55056, #2098, #32557, #71068, #2593, #33048, #88020, #41067, #4545, #58008, #5028, #41569, #87532, #66006, #12518, #72036, #80531, #43020, #12030, #50029, #11535, #35007, #42529, #73013, #88518, #11048, #58505, #89015, #81017, #33532, #49044, #20019, #19046, #28009, #10556, #50520, #73502, #35514, #3076, #20522, #65510, #27024, #49522, #96032, #71563, #96534, #27516, #3564, #80030, #34023, #64027, #51007, #42055, #94540, #26058, #79548, #95535, #72519, #56548, #87043, #18552, #19533, #64520, #95026, #26535, #57031, #57524, #4053, #34515, #65008, #22504, #83489, #36511, #14013, #67502, #37506, #21018, #37005, #66510, #51507, #98021, #67999, #36007, #98523, #28988, #14512, #15008, #75489, #44494, #38000, #60481, #30467, #29976, #60968, #44982, #90970, #43503, #7001, #59005, #74994, #59496, #6497, #89507, #67004, #81502, #45478, #82497, #52975, #29476, #97525, #59984, #75980, #43993, #82000, #7509, #68492, #90477, #74002, #82994, #89994, #19, #91478, #22012, #13511, #23001, #21510, #52486, #74495, #13007, #5527, #97035, #28511, #6019, #52008, #23496, #9452, #16967, #38488, #46950, #54937, #47446, #31936, #32932, #24967, #92940, #70956, #62940, #2476, #24474, #62437, #70456, #91968, #55452, #16472, #77444, #77946, #69469, #92452, #39953, #53968, #69964, #9952, #63432, #23978, #93938, #53468, #84477, #39474, #61952, #93442, #76474, #1976, #85453 ),
 ( #1483, #32441, #40458, #85953, #17463, #8957, #61460, #83978, #46466, #54450, #15503, #47931, #45985, #30962, #78437, #7989, #68982, #15977, #516, #76960, #8471, #38978, #990, #31450, #84959, #72894, #19900, #56437, #3439, #80901, #27396, #86924, #95412, #57888, #26907, #64884, #26411, #49902, #57404, #87894, #4428, #25936, #74746, #6258, #95916, #48430, #63909, #34894, #33898, #44242, #50392, #64404, #94912, #78932, #41454, #87413, #40949, #72399, #65389, #3927, #79907, #56912, #67254, #11416, #19411, #42414, #18437, #18930, #49407, #41937, #88402, #34396, #10928, #13756, #36761, #25463, #48919, #80412, #11912, #55946, #86445, #17944, #10442, #71447, #2961, #71918, #33411, #94420, #79432, #59740, #67754, #29730, #22259, #52247, #98273, #60238, #54206, #23746, #8238, #68253, #68738, #22749, #98773, #8713, #52733, #29243, #21768, #92218, #90235, #46708, #270, #15259, #7252, #30714, #97778, #38732, #61224, #90733, #37756, #83241, #82741, #16228, #30221, #39232, #14261, #37267, #83737, #60725, #69232, #44739, #15747, #76236, #31208, #14764, #84723, #7753, #45740, #6750, #77208, #45237, #757, #61704, #75734, #91224, #38247, #53726, #53232, #91729, #75240, #23251, #84243, #46233, #76719, #86689, #17221, #2723, #3194, #63669, #2227, #26182, #48674, #18688, #18194, #49172, #33177, #25705, #31702, #94174, #47194, #63181, #47700, #32686, #77697, #24717, #69720, #71684, #70709, #56196, #93688, #55190, #48182, #79176, #32188, #9209, #10691, #41204, #25221, #62194, #71200, #78192, #56674, #79674, #78694, #39722, #87163, #85705, #55702, #70215, #86198, #17710, #33659, #10204, #11171, #64155, #1734, #94673, #1246, #54694, #40697, #92703, #24228, #85216, #16720, #62690, #93190, #9705, #40203, #59123, #12643, #50652, #58640, #80155, #43634, #4676, #65638, #5158, #57650, #80660, #66131, #42179, #58129, #97166, #41690, #81628, #20649, #72161, #35644, #89139, #36134, #72643, #19658, #28634, #74120, #4176, #43140, #5656, #73632, #81140, #42660, #96660, #28141, #51140, #13136, #34647, #89632, #21143, #66642, #64643, #11666, #51643, #50149, #82124, #3688, #12155, #73136, #95154, #88147, #35138, #57157, #88639, #34149, #20147, #96162, #27644, #26663, #87655, #19168, #49648, #65142, #95663, #27148, #37632, #30597, #91106, #98146, #61103, #69111, #91612, #44626, #68129, #52618, #45613, #98657, #7642, #60611, #92099, #6141, #60111, #150, #45111, #67129, #74627, #82627, #75121, #37143, #97656, #14141, #6629, #644, #38613, #23128, #83119, #83621, #30103, #14648, #23630, #67637, #44118, #36644, #31093, #52130, #76111, #29607, #90612, #15632 ) ),
 .UNSPECIFIED., .F., .F., .F. ) 
 B_SPLINE_SURFACE_WITH_KNOTS ( ( 2, 2 ),
 ( 3, 2, 2, 2, 2, 2, 2, 2, 2, 2, 2, 2, 2, 2, 2, 2, 2, 2, 2, 2, 2, 2, 2, 2, 2, 2, 2, 2, 2, 2, 2, 2, 2, 2, 2, 2, 2, 2, 2, 2, 2, 2, 2, 2, 2, 2, 2, 2, 2, 2, 2, 2, 2, 2, 2, 2, 2, 2, 2, 2, 2, 2, 2, 2, 2, 2, 2, 2, 2, 2, 2, 2, 2, 2, 2, 2, 2, 2, 2, 2, 2, 2, 2, 2, 2, 2, 2, 2, 2, 2, 2, 2, 2, 2, 2, 2, 2, 2, 2, 2, 2, 2, 2, 2, 2, 2, 2, 2, 2, 2, 2, 2, 2, 2, 2, 2, 2, 2, 2, 2, 2, 2, 2, 2, 2, 2, 2, 2, 2, 2, 2, 2, 2, 2, 2, 2, 2, 2, 2, 2, 2, 2, 2, 2, 2, 2, 2, 2, 2, 2, 2, 2, 2, 2, 2, 2, 2, 2, 2, 2, 2, 2, 3 ),
 ( 0.000000000000000000, 1.000000000000000000 ),
 ( 0.000000000000000000, 0.005952380952380952051, 0.01190476190476190410, 0.01785714285714285615, 0.02380952380952380820, 0.02976190476190476025, 0.03571428571428571230, 0.04166666666666666435, 0.04761904761904761640, 0.05357142857142856845, 0.05952380952380952051, 0.06547619047619047949, 0.07142857142857142461, 0.07738095238095238360, 0.08333333333333332871, 0.08928571428571428770, 0.09523809523809523281, 0.1011904761904761918, 0.1071428571428571369, 0.1130952380952380959, 0.1190476190476190410, 0.1250000000000000000, 0.1309523809523809590, 0.1369047619047619180, 0.1428571428571428492, 0.1488095238095238082, 0.1547619047619047672, 0.1607142857142857262, 0.1666666666666666574, 0.1726190476190476164, 0.1785714285714285754, 0.1845238095238095344, 0.1904761904761904656, 0.1964285714285714246, 0.2023809523809523836, 0.2083333333333333426, 0.2142857142857142738, 0.2202380952380952328, 0.2261904761904761918, 0.2321428571428571508, 0.2380952380952380820, 0.2440476190476190410, 0.2500000000000000000, 0.2559523809523809312, 0.2619047619047619180, 0.2678571428571428492, 0.2738095238095238360, 0.2797619047619047672, 0.2857142857142856984, 0.2916666666666666852, 0.2976190476190476164, 0.3035714285714285476, 0.3095238095238095344, 0.3154761904761904656, 0.3214285714285714524, 0.3273809523809523836, 0.3333333333333333148, 0.3392857142857143016, 0.3452380952380952328, 0.3511904761904761640, 0.3571428571428571508, 0.3630952380952380820, 0.3690476190476190688, 0.3750000000000000000, 0.3809523809523809312, 0.3869047619047619180, 0.3928571428571428492, 0.3988095238095238360, 0.4047619047619047672, 0.4107142857142856984, 0.4166666666666666852, 0.4226190476190476164, 0.4285714285714285476, 0.4345238095238095344, 0.4404761904761904656, 0.4464285714285714524, 0.4523809523809523836, 0.4583333333333333148, 0.4642857142857143016, 0.4702380952380952328, 0.4761904761904761640, 0.4821428571428571508, 0.4880952380952380820, 0.4940476190476190688, 0.5000000000000000000, 0.5059523809523809312, 0.5119047619047618625, 0.5178571428571429047, 0.5238095238095238360, 0.5297619047619047672, 0.5357142857142856984, 0.5416666666666666297, 0.5476190476190476719, 0.5535714285714286031, 0.5595238095238095344, 0.5654761904761904656, 0.5714285714285713969, 0.5773809523809523281, 0.5833333333333333703, 0.5892857142857143016, 0.5952380952380952328, 0.6011904761904761640, 0.6071428571428570953, 0.6130952380952381375, 0.6190476190476190688, 0.6250000000000000000, 0.6309523809523809312, 0.6369047619047618625, 0.6428571428571429047, 0.6488095238095238360, 0.6547619047619047672, 0.6607142857142856984, 0.6666666666666666297, 0.6726190476190476719, 0.6785714285714286031, 0.6845238095238095344, 0.6904761904761904656, 0.6964285714285713969, 0.7023809523809523281, 0.7083333333333333703, 0.7142857142857143016, 0.7202380952380952328, 0.7261904761904761640, 0.7321428571428570953, 0.7380952380952381375, 0.7440476190476190688, 0.7500000000000000000, 0.7559523809523809312, 0.7619047619047618625, 0.7678571428571429047, 0.7738095238095238360, 0.7797619047619047672, 0.7857142857142856984, 0.7916666666666666297, 0.7976190476190476719, 0.8035714285714286031, 0.8095238095238095344, 0.8154761904761904656, 0.8214285714285713969, 0.8273809523809523281, 0.8333333333333333703, 0.8392857142857143016, 0.8452380952380952328, 0.8511904761904761640, 0.8571428571428570953, 0.8630952380952381375, 0.8690476190476190688, 0.8750000000000000000, 0.8809523809523809312, 0.8869047619047618625, 0.8928571428571429047, 0.8988095238095238360, 0.9047619047619047672, 0.9107142857142856984, 0.9166666666666666297, 0.9226190476190476719, 0.9285714285714286031, 0.9345238095238095344, 0.9404761904761904656, 0.9464285714285713969, 0.9523809523809523281, 0.9583333333333333703, 0.9642857142857143016 ),
 .UNSPECIFIED. ) 
 GEOMETRIC_REPRESENTATION_ITEM ( )  RATIONAL_B_SPLINE_SURFACE ( (
 ( 1.000000000000000000, 0.9659258262890683122, 1.000000000000000000, 0.9659258262890683122, 1.000000000000000000, 0.9659258262890683122, 1.000000000000000000, 0.9659258262890683122, 1.000000000000000000, 0.9659258262890683122, 1.000000000000000000, 0.9659258262890683122, 1.000000000000000000, 0.9659258262890683122, 1.000000000000000000, 0.9659258262890683122, 1.000000000000000000, 0.9659258262890683122, 1.000000000000000000, 0.9659258262890683122, 1.000000000000000000, 0.9659258262890683122, 1.000000000000000000, 0.9659258262890683122, 1.000000000000000000, 0.9659258262890683122, 1.000000000000000000, 0.9659258262890683122, 1.000000000000000000, 0.9659258262890683122, 1.000000000000000000, 0.9659258262890683122, 1.000000000000000000, 0.9659258262890683122, 1.000000000000000000, 0.9659258262890683122, 1.000000000000000000, 0.9659258262890683122, 1.000000000000000000, 0.9659258262890683122, 1.000000000000000000, 0.9659258262890683122, 1.000000000000000000, 0.9659258262890683122, 1.000000000000000000, 0.9659258262890683122, 1.000000000000000000, 0.9659258262890683122, 1.000000000000000000, 0.9659258262890683122, 1.000000000000000000, 0.9659258262890683122, 1.000000000000000000, 0.9659258262890683122, 1.000000000000000000, 0.9659258262890683122, 1.000000000000000000, 0.9659258262890683122, 1.000000000000000000, 0.9659258262890683122, 1.000000000000000000, 0.9659258262890683122, 1.000000000000000000, 0.9659258262890683122, 1.000000000000000000, 0.9659258262890683122, 1.000000000000000000, 0.9659258262890683122, 1.000000000000000000, 0.9659258262890683122, 1.000000000000000000, 0.9659258262890683122, 1.000000000000000000, 0.9659258262890683122, 1.000000000000000000, 0.9659258262890683122, 1.000000000000000000, 0.9659258262890683122, 1.000000000000000000, 0.9659258262890683122, 1.000000000000000000, 0.9659258262890683122, 1.000000000000000000, 0.9659258262890683122, 1.000000000000000000, 0.9659258262890683122, 1.000000000000000000, 0.9659258262890683122, 1.000000000000000000, 0.9659258262890683122, 1.000000000000000000, 0.9659258262890683122, 1.000000000000000000, 0.9659258262890683122, 1.000000000000000000, 0.9659258262890683122, 1.000000000000000000, 0.9659258262890683122, 1.000000000000000000, 0.9659258262890683122, 1.000000000000000000, 0.9659258262890683122, 1.000000000000000000, 0.9659258262890683122, 1.000000000000000000, 0.9659258262890683122, 1.000000000000000000, 0.9659258262890683122, 1.000000000000000000, 0.9659258262890683122, 1.000000000000000000, 0.9659258262890683122, 1.000000000000000000, 0.9659258262890683122, 1.000000000000000000, 0.9659258262890683122, 1.000000000000000000, 0.9659258262890683122, 1.000000000000000000, 0.9659258262890683122, 1.000000000000000000, 0.9659258262890683122, 1.000000000000000000, 0.9659258262890683122, 1.000000000000000000, 0.9659258262890683122, 1.000000000000000000, 0.9659258262890683122, 1.000000000000000000, 0.9659258262890683122, 1.000000000000000000, 0.9659258262890683122, 1.000000000000000000, 0.9659258262890683122, 1.000000000000000000, 0.9659258262890683122, 1.000000000000000000, 0.9659258262890683122, 1.000000000000000000, 0.9659258262890683122, 1.000000000000000000, 0.9659258262890683122, 1.000000000000000000, 0.9659258262890683122, 1.000000000000000000, 0.9659258262890683122, 1.000000000000000000, 0.9659258262890683122, 1.000000000000000000, 0.9659258262890683122, 1.000000000000000000, 0.9659258262890683122, 1.000000000000000000, 0.9659258262890683122, 1.000000000000000000, 0.9659258262890683122, 1.000000000000000000, 0.9659258262890683122, 1.000000000000000000, 0.9659258262890683122, 1.000000000000000000, 0.9659258262890683122, 1.000000000000000000, 0.9659258262890683122, 1.000000000000000000, 0.9659258262890683122, 1.000000000000000000, 0.9659258262890683122, 1.000000000000000000, 0.9659258262890683122, 1.000000000000000000, 0.9659258262890683122, 1.000000000000000000, 0.9659258262890683122, 1.000000000000000000, 0.9659258262890683122, 1.000000000000000000, 0.9659258262890683122, 1.000000000000000000, 0.9659258262890683122, 1.000000000000000000, 0.9659258262890683122, 1.000000000000000000, 0.9659258262890683122, 1.000000000000000000, 0.9659258262890683122, 1.000000000000000000, 0.9659258262890683122, 1.000000000000000000, 0.9659258262890683122, 1.000000000000000000, 0.9659258262890683122, 1.000000000000000000, 0.9659258262890683122, 1.000000000000000000, 0.9659258262890683122, 1.000000000000000000, 0.9659258262890683122, 1.000000000000000000, 0.9659258262890683122, 1.000000000000000000, 0.9659258262890683122, 1.000000000000000000, 0.9659258262890683122, 1.000000000000000000, 0.9659258262890683122, 1.000000000000000000, 0.9659258262890683122, 1.000000000000000000, 0.9659258262890683122, 1.000000000000000000, 0.9659258262890683122, 1.000000000000000000, 0.9659258262890683122, 1.000000000000000000, 0.9659258262890683122, 1.000000000000000000, 0.9659258262890683122, 1.000000000000000000, 0.9659258262890683122, 1.000000000000000000, 0.9659258262890683122, 1.000000000000000000, 0.9659258262890683122, 1.000000000000000000, 0.9659258262890683122, 1.000000000000000000, 0.9659258262890683122, 1.000000000000000000, 0.9659258262890683122, 1.000000000000000000, 0.9659258262890683122, 1.000000000000000000, 0.9659258262890683122, 1.000000000000000000, 0.9659258262890683122, 1.000000000000000000, 0.9659258262890683122, 1.000000000000000000, 0.9659258262890683122, 1.000000000000000000, 0.9659258262890683122, 1.000000000000000000, 0.9659258262890683122, 1.000000000000000000, 0.9659258262890683122, 1.000000000000000000, 0.9659258262890683122, 1.000000000000000000, 0.9659258262890683122, 1.000000000000000000, 0.9659258262890683122, 1.000000000000000000, 0.9659258262890683122, 1.000000000000000000, 0.9659258262890683122, 1.000000000000000000, 0.9659258262890683122, 1.000000000000000000, 0.9659258262890683122, 1.000000000000000000, 0.9659258262890683122, 1.000000000000000000, 0.9659258262890683122, 1.000000000000000000, 0.9659258262890683122, 1.000000000000000000, 0.9659258262890683122, 1.000000000000000000, 0.9659258262890683122, 1.000000000000000000, 0.9659258262890683122, 1.000000000000000000, 0.9659258262890683122, 1.000000000000000000, 0.9659258262890683122, 1.000000000000000000, 0.9659258262890683122, 1.000000000000000000, 0.9659258262890683122, 1.000000000000000000, 0.9659258262890683122, 1.000000000000000000, 0.9659258262890683122, 1.000000000000000000, 0.9659258262890683122, 1.000000000000000000, 0.9659258262890683122, 1.000000000000000000, 0.9659258262890683122, 1.000000000000000000, 0.9659258262890683122, 1.000000000000000000, 0.9659258262890683122, 1.000000000000000000, 0.9659258262890683122, 1.000000000000000000, 0.9659258262890683122, 1.000000000000000000, 0.9659258262890683122, 1.000000000000000000, 0.9659258262890683122, 1.000000000000000000, 0.9659258262890683122, 1.000000000000000000, 0.9659258262890683122, 1.000000000000000000, 0.9659258262890683122, 1.000000000000000000, 0.9659258262890683122, 1.000000000000000000, 0.9659258262890683122, 1.000000000000000000, 0.9659258262890683122, 1.000000000000000000, 0.9659258262890683122, 1.000000000000000000, 0.9659258262890683122, 1.000000000000000000, 0.9659258262890683122, 1.000000000000000000, 0.9659258262890683122, 1.000000000000000000, 0.9659258262890683122, 1.000000000000000000),
 ( 1.000000000000000000, 0.9659258262890683122, 1.000000000000000000, 0.9659258262890683122, 1.000000000000000000, 0.9659258262890683122, 1.000000000000000000, 0.9659258262890683122, 1.000000000000000000, 0.9659258262890683122, 1.000000000000000000, 0.9659258262890683122, 1.000000000000000000, 0.9659258262890683122, 1.000000000000000000, 0.9659258262890683122, 1.000000000000000000, 0.9659258262890683122, 1.000000000000000000, 0.9659258262890683122, 1.000000000000000000, 0.9659258262890683122, 1.000000000000000000, 0.9659258262890683122, 1.000000000000000000, 0.9659258262890683122, 1.000000000000000000, 0.9659258262890683122, 1.000000000000000000, 0.9659258262890683122, 1.000000000000000000, 0.9659258262890683122, 1.000000000000000000, 0.9659258262890683122, 1.000000000000000000, 0.9659258262890683122, 1.000000000000000000, 0.9659258262890683122, 1.000000000000000000, 0.9659258262890683122, 1.000000000000000000, 0.9659258262890683122, 1.000000000000000000, 0.9659258262890683122, 1.000000000000000000, 0.9659258262890683122, 1.000000000000000000, 0.9659258262890683122, 1.000000000000000000, 0.9659258262890683122, 1.000000000000000000, 0.9659258262890683122, 1.000000000000000000, 0.9659258262890683122, 1.000000000000000000, 0.9659258262890683122, 1.000000000000000000, 0.9659258262890683122, 1.000000000000000000, 0.9659258262890683122, 1.000000000000000000, 0.9659258262890683122, 1.000000000000000000, 0.9659258262890683122, 1.000000000000000000, 0.9659258262890683122, 1.000000000000000000, 0.9659258262890683122, 1.000000000000000000, 0.9659258262890683122, 1.000000000000000000, 0.9659258262890683122, 1.000000000000000000, 0.9659258262890683122, 1.000000000000000000, 0.9659258262890683122, 1.000000000000000000, 0.9659258262890683122, 1.000000000000000000, 0.9659258262890683122, 1.000000000000000000, 0.9659258262890683122, 1.000000000000000000, 0.9659258262890683122, 1.000000000000000000, 0.9659258262890683122, 1.000000000000000000, 0.9659258262890683122, 1.000000000000000000, 0.9659258262890683122, 1.000000000000000000, 0.9659258262890683122, 1.000000000000000000, 0.9659258262890683122, 1.000000000000000000, 0.9659258262890683122, 1.000000000000000000, 0.9659258262890683122, 1.000000000000000000, 0.9659258262890683122, 1.000000000000000000, 0.9659258262890683122, 1.000000000000000000, 0.9659258262890683122, 1.000000000000000000, 0.9659258262890683122, 1.000000000000000000, 0.9659258262890683122, 1.000000000000000000, 0.9659258262890683122, 1.000000000000000000, 0.9659258262890683122, 1.000000000000000000, 0.9659258262890683122, 1.000000000000000000, 0.9659258262890683122, 1.000000000000000000, 0.9659258262890683122, 1.000000000000000000, 0.9659258262890683122, 1.000000000000000000, 0.9659258262890683122, 1.000000000000000000, 0.9659258262890683122, 1.000000000000000000, 0.9659258262890683122, 1.000000000000000000, 0.9659258262890683122, 1.000000000000000000, 0.9659258262890683122, 1.000000000000000000, 0.9659258262890683122, 1.000000000000000000, 0.9659258262890683122, 1.000000000000000000, 0.9659258262890683122, 1.000000000000000000, 0.9659258262890683122, 1.000000000000000000, 0.9659258262890683122, 1.000000000000000000, 0.9659258262890683122, 1.000000000000000000, 0.9659258262890683122, 1.000000000000000000, 0.9659258262890683122, 1.000000000000000000, 0.9659258262890683122, 1.000000000000000000, 0.9659258262890683122, 1.000000000000000000, 0.9659258262890683122, 1.000000000000000000, 0.9659258262890683122, 1.000000000000000000, 0.9659258262890683122, 1.000000000000000000, 0.9659258262890683122, 1.000000000000000000, 0.9659258262890683122, 1.000000000000000000, 0.9659258262890683122, 1.000000000000000000, 0.9659258262890683122, 1.000000000000000000, 0.9659258262890683122, 1.000000000000000000, 0.9659258262890683122, 1.000000000000000000, 0.9659258262890683122, 1.000000000000000000, 0.9659258262890683122, 1.000000000000000000, 0.9659258262890683122, 1.000000000000000000, 0.9659258262890683122, 1.000000000000000000, 0.9659258262890683122, 1.000000000000000000, 0.9659258262890683122, 1.000000000000000000, 0.9659258262890683122, 1.000000000000000000, 0.9659258262890683122, 1.000000000000000000, 0.9659258262890683122, 1.000000000000000000, 0.9659258262890683122, 1.000000000000000000, 0.9659258262890683122, 1.000000000000000000, 0.9659258262890683122, 1.000000000000000000, 0.9659258262890683122, 1.000000000000000000, 0.9659258262890683122, 1.000000000000000000, 0.9659258262890683122, 1.000000000000000000, 0.9659258262890683122, 1.000000000000000000, 0.9659258262890683122, 1.000000000000000000, 0.9659258262890683122, 1.000000000000000000, 0.9659258262890683122, 1.000000000000000000, 0.9659258262890683122, 1.000000000000000000, 0.9659258262890683122, 1.000000000000000000, 0.9659258262890683122, 1.000000000000000000, 0.9659258262890683122, 1.000000000000000000, 0.9659258262890683122, 1.000000000000000000, 0.9659258262890683122, 1.000000000000000000, 0.9659258262890683122, 1.000000000000000000, 0.9659258262890683122, 1.000000000000000000, 0.9659258262890683122, 1.000000000000000000, 0.9659258262890683122, 1.000000000000000000, 0.9659258262890683122, 1.000000000000000000, 0.9659258262890683122, 1.000000000000000000, 0.9659258262890683122, 1.000000000000000000, 0.9659258262890683122, 1.000000000000000000, 0.9659258262890683122, 1.000000000000000000, 0.9659258262890683122, 1.000000000000000000, 0.9659258262890683122, 1.000000000000000000, 0.9659258262890683122, 1.000000000000000000, 0.9659258262890683122, 1.000000000000000000, 0.9659258262890683122, 1.000000000000000000, 0.9659258262890683122, 1.000000000000000000, 0.9659258262890683122, 1.000000000000000000, 0.9659258262890683122, 1.000000000000000000, 0.9659258262890683122, 1.000000000000000000, 0.9659258262890683122, 1.000000000000000000, 0.9659258262890683122, 1.000000000000000000, 0.9659258262890683122, 1.000000000000000000, 0.9659258262890683122, 1.000000000000000000, 0.9659258262890683122, 1.000000000000000000, 0.9659258262890683122, 1.000000000000000000, 0.9659258262890683122, 1.000000000000000000, 0.9659258262890683122, 1.000000000000000000, 0.9659258262890683122, 1.000000000000000000, 0.9659258262890683122, 1.000000000000000000, 0.9659258262890683122, 1.000000000000000000, 0.9659258262890683122, 1.000000000000000000, 0.9659258262890683122, 1.000000000000000000, 0.9659258262890683122, 1.000000000000000000, 0.9659258262890683122, 1.000000000000000000, 0.9659258262890683122, 1.000000000000000000, 0.9659258262890683122, 1.000000000000000000, 0.9659258262890683122, 1.000000000000000000, 0.9659258262890683122, 1.000000000000000000, 0.9659258262890683122, 1.000000000000000000, 0.9659258262890683122, 1.000000000000000000, 0.9659258262890683122, 1.000000000000000000, 0.9659258262890683122, 1.000000000000000000, 0.9659258262890683122, 1.000000000000000000, 0.9659258262890683122, 1.000000000000000000, 0.9659258262890683122, 1.000000000000000000, 0.9659258262890683122, 1.000000000000000000, 0.9659258262890683122, 1.000000000000000000, 0.9659258262890683122, 1.000000000000000000, 0.9659258262890683122, 1.000000000000000000, 0.9659258262890683122, 1.000000000000000000, 0.9659258262890683122, 1.000000000000000000, 0.9659258262890683122, 1.000000000000000000, 0.9659258262890683122, 1.000000000000000000, 0.9659258262890683122, 1.000000000000000000) ) ) 
 REPRESENTATION_ITEM ( '' )  SURFACE ( )  );
#42566 = ORIENTED_EDGE ( 'NONE', *, *, #26120, .T. ) ;
#42565 = EDGE_CURVE ( 'NONE', #75573, #31275, #75334, .T. ) ;
#42567 = ORIENTED_EDGE ( 'NONE', *, *, #10740, .F. ) ;
#42568 = CARTESIAN_POINT ( 'NONE',  ( 13.79529636645031943, 50.34541550158064638, -14.16423886937409904 ) ) ;
#42569 = CARTESIAN_POINT ( 'NONE',  ( 24.16423886937410614, 49.51208216824730357, -3.795296366450302550 ) ) ;
#42570 = CARTESIAN_POINT ( 'NONE',  ( 5.076628168052704559, 15.17559781766745175, -8.527530157486179263 ) ) ;
#42571 = CARTESIAN_POINT ( 'NONE',  ( 19.38216949554541202, 30.99863466993042138, 9.382169495545424454 ) ) ;
#42572 = CARTESIAN_POINT ( 'NONE',  ( 15.00000000000000000, 77.07179676972447169, -6.250000000000000000 ) ) ;
#42573 =( NAMED_UNIT ( * ) SI_UNIT ( $, .STERADIAN. ) SOLID_ANGLE_UNIT ( ) );
#42574 = FILL_AREA_STYLE ('',( #65053 ) ) ;
#42575 = CARTESIAN_POINT ( 'NONE',  ( 24.16423886937410614, 44.30374883491397497, 8.672049930838204340E-16 ) ) ;
#42576 = EDGE_CURVE ( 'NONE', #52625, #48349, #98867, .T. ) ;
#42577 =( GEOMETRIC_REPRESENTATION_CONTEXT ( 3 ) GLOBAL_UNCERTAINTY_ASSIGNED_CONTEXT ( ( #58475 ) ) GLOBAL_UNIT_ASSIGNED_CONTEXT ( ( #23083, #52570, #14596 ) ) REPRESENTATION_CONTEXT ( 'NONE', 'WORKASPACE' ) );
#42578 = EDGE_CURVE ( 'NONE', #18624, #98326, #40162, .T. ) ;
#42579 = CARTESIAN_POINT ( 'NONE',  ( 10.19513985507834342, 0.3639309290920412776, -11.00268709613220786 ) ) ;
#42580 = CARTESIAN_POINT ( 'NONE',  ( 7.361572987183169658, 14.96726448433411960, -9.846743663894592657 ) ) ;
#42581 = CARTESIAN_POINT ( 'NONE',  ( -9.846743663894590881, -3.782735515665876846, 2.638427012816840111 ) ) ;
#42582 = ORIENTED_EDGE ( 'NONE', *, *, #11493, .T. ) ;
#42583 = CARTESIAN_POINT ( 'NONE',  ( 4.219999999999999751, 10.25000000000000000, 2.750000000000000000 ) ) ;
#42584 = ORIENTED_EDGE ( 'NONE', *, *, #15404, .T. ) ;
#42585 = PRESENTATION_STYLE_ASSIGNMENT (( #20072 ) ) ;
#42586 = ORIENTED_EDGE ( 'NONE', *, *, #68231, .T. ) ;
#42587 = MECHANICAL_DESIGN_GEOMETRIC_PRESENTATION_REPRESENTATION (  '', ( #85695 ), #55363 ) ;
#42589 = CARTESIAN_POINT ( 'NONE',  ( 20.88017736071110164, 25.35535201082150891, 2.915334737309930979 ) ) ;
#42588 = CARTESIAN_POINT ( 'NONE',  ( 20.88017736071110519, 20.56368534415484106, 2.639326808657452039E-16 ) ) ;
#42591 = CARTESIAN_POINT ( 'NONE',  ( 19.38216949554541557, 12.24863466993041961, -9.382169495545420901 ) ) ;
#42590 = CARTESIAN_POINT ( 'NONE',  ( 10.00000000000000000, 49.75893115100078745, -9.846743663894594434 ) ) ;
#42592 = DIRECTION ( 'NONE',  ( 1.000000000000000000, -0.000000000000000000, 0.000000000000000000 ) ) ;
#42593 = PRESENTATION_LAYER_ASSIGNMENT (  '', '', ( #2659 ) ) ;
#42594 =( GEOMETRIC_REPRESENTATION_CONTEXT ( 3 ) GLOBAL_UNCERTAINTY_ASSIGNED_CONTEXT ( ( #73158 ) ) GLOBAL_UNIT_ASSIGNED_CONTEXT ( ( #3395, #24928, #85914 ) ) REPRESENTATION_CONTEXT ( 'NONE', 'WORKASPACE' ) );
#42595 = CARTESIAN_POINT ( 'NONE',  ( 22.81628187352647785, 21.62363466993041783, 6.195893100308588602E-16 ) ) ;
#42596 = ORIENTED_EDGE ( 'NONE', *, *, #98732, .T. ) ;
#42597 = CARTESIAN_POINT ( 'NONE',  ( 0.1532563361054100626, 30.80059781766744820, -2.638427012816831230 ) ) ;
#42598 = CARTESIAN_POINT ( 'NONE',  ( 24.16423886937410614, 59.51208216824728936, -3.795296366450302550 ) ) ;
#42599 = VERTEX_POINT ( 'NONE', #43358 ) ;
#42600 = EDGE_CURVE ( 'NONE', #89676, #59403, #82840, .T. ) ;
#42601 = CARTESIAN_POINT ( 'NONE',  ( 17.96484262340118221, 9.938685344154839285, 7.964842623401181321 ) ) ;
#42602 = VERTEX_POINT ( 'NONE', #60336 ) ;
#42603 = CARTESIAN_POINT ( 'NONE',  ( 15.44008868035555793, 41.39701867748817676, -9.422509992056140149 ) ) ;
#42604 = CARTESIAN_POINT ( 'NONE',  ( 2.035157376598822676, 42.43868534415483396, -7.964842623401177768 ) ) ;
#42605 = CARTESIAN_POINT ( 'NONE',  ( -0.8801773607111009756, 58.06368534415484106, 1.068504757029289695E-15 ) ) ;
#42606 = SURFACE_SIDE_STYLE ('',( #11609 ) ) ;
#42607 = CARTESIAN_POINT ( 'NONE',  ( 17.96484262340118221, 36.18868534415484106, -7.964842623401177768 ) ) ;
#42608 = FACE_OUTER_BOUND ( 'NONE', #93739, .T. ) ;
#42609 = AXIS2_PLACEMENT_3D ( 'NONE', #3634, #50100, #72591 ) ;
#42610 = CARTESIAN_POINT ( 'NONE',  ( 10.00000000000000000, 29.75893115100078745, -9.846743663894594434 ) ) ;
#42611 = VERTEX_POINT ( 'NONE', #52831 ) ;
#42612 = CARTESIAN_POINT ( 'NONE',  ( 1.472469842513823179, 56.42559781766745886, 4.923371831947296329 ) ) ;
#42613 = CARTESIAN_POINT ( 'NONE',  ( 0.000000000000000000, 0.000000000000000000, -3.000000000000000000 ) ) ;
#42614 = CARTESIAN_POINT ( 'NONE',  ( -5.812563760649267941, -35.09659463721938977, 2.750000000000000000 ) ) ;
#42615 = VERTEX_POINT ( 'NONE', #73855 ) ;
#42616 = CARTESIAN_POINT ( 'NONE',  ( -14.62617646268090077, 14.49999999999999112, -3.327906561567068433 ) ) ;
#42617 = CARTESIAN_POINT ( 'NONE',  ( 17.39651004071838614, 47.93575266056826933, 6.500000000000032863 ) ) ;
#42619 = CARTESIAN_POINT ( 'NONE',  ( 14.92337183194729633, 32.67559781766745175, 8.527530157486181039 ) ) ;
#42618 = CARTESIAN_POINT ( 'NONE',  ( 7.361572987183169658, 64.96726448433412315, -9.846743663894592657 ) ) ;
#42620 = CARTESIAN_POINT ( 'NONE',  ( 10.00000000000000178, 58.05374883491397497, 14.16423886937410082 ) ) ;
#42621 = CARTESIAN_POINT ( 'NONE',  ( 14.62617646268087768, 15.00000000000000000, -3.327906561566883692 ) ) ;
#42622 = VERTEX_POINT ( 'NONE', #14360 ) ;
#42623 = CARTESIAN_POINT ( 'NONE',  ( -6.898461952320517732, 4.837215022590613936E-16, 12.75387089053304557 ) ) ;
#42624 = CARTESIAN_POINT ( 'NONE',  ( 2.791683348922237240, 35.38393115100079456, -7.208316651077763204 ) ) ;
#42625 = CARTESIAN_POINT ( 'NONE',  ( 11.57153612472183646, -43.60599867514397943, -3.750000000000001776 ) ) ;
#42626 = CARTESIAN_POINT ( 'NONE',  ( 6.565887622018943937, 5.165301336597086568, 12.81628187352647430 ) ) ;
#42627 = CARTESIAN_POINT ( 'NONE',  ( 10.00000000000000178, 7.258931151000785675, 9.846743663894594434 ) ) ;
#42628 = CARTESIAN_POINT ( 'NONE',  ( -14.09394518620614711, 4.304378373471060795E-16, 3.407449058785263940 ) ) ;
#42629 = CARTESIAN_POINT ( 'NONE',  ( 14.92337183194729633, 7.675597817667451750, 8.527530157486181039 ) ) ;
#42630 = CARTESIAN_POINT ( 'NONE',  ( 0.1532563361054082862, 61.21726448433412315, 2.638427012816831674 ) ) ;
#42631 = DIRECTION ( 'NONE',  ( 1.000000000000000000, 0.000000000000000000, 0.000000000000000000 ) ) ;
#42632 = MECHANICAL_DESIGN_GEOMETRIC_PRESENTATION_REPRESENTATION (  '', ( #33060 ), #87310 ) ;
#42633 = AXIS2_PLACEMENT_3D ( 'NONE', #72722, #80735, #12230 ) ;
#42634 = ORIENTED_EDGE ( 'NONE', *, *, #78578, .T. ) ;
#42635 = CARTESIAN_POINT ( 'NONE',  ( 4.559911319644449179, 12.23035201082150714, -9.422509992056141925 ) ) ;
#42636 = CARTESIAN_POINT ( 'NONE',  ( 17.08211943468705130, 3.470415501580634388, 12.26659068614894998 ) ) ;
#42637 = CARTESIAN_POINT ( 'NONE',  ( 2.791683348922237240, 15.38393115100078212, -7.208316651077763204 ) ) ;
#42638 = CARTESIAN_POINT ( 'NONE',  ( -0.8801773607110991993, 42.85535201082150536, -2.915334737309923874 ) ) ;
#42640 = DIRECTION ( 'NONE',  ( -0.3338068592337649076, 0.000000000000000000, -0.9426414910921805390 ) ) ;
#42639 = CARTESIAN_POINT ( 'NONE',  ( -1.099225684535947600, 29.54030133659708923, 6.408140936763237150 ) ) ;
#42641 = PRESENTATION_STYLE_ASSIGNMENT (( #95645 ) ) ;
#42642 = CARTESIAN_POINT ( 'NONE',  ( -0.2418659066527731605, 57.23410085661204505, -6.114288769123041867 ) ) ;
#42643 = FILL_AREA_STYLE ('',( #27631 ) ) ;
#42644 = CIRCLE ( 'NONE', #79408, 0.2500000000000002220 ) ;
#42645 = CARTESIAN_POINT ( 'NONE',  ( 21.09922568453595559, 7.040301336597086568, -6.408140936763230044 ) ) ;
#42646 = CARTESIAN_POINT ( 'NONE',  ( -2.816281873526471635, -1.084698663402913210, -3.434112377981056508 ) ) ;
#42647 = CARTESIAN_POINT ( 'NONE',  ( 12.63842701281683922, 14.55059781766744997, -9.846743663894590881 ) ) ;
#42648 = CARTESIAN_POINT ( 'NONE',  ( -5.204170427930421283E-15, -23.18631465584515894, -10.88017736071110342 ) ) ;
#42649 = CARTESIAN_POINT ( 'NONE',  ( 0.6178305044545818747, 23.49863466993041783, -9.382169495545419124 ) ) ;
#42650 = CARTESIAN_POINT ( 'NONE',  ( -11.58434547256946168, -69.53046085282417721, -4.000000000003604228 ) ) ;
#42651 = CARTESIAN_POINT ( 'NONE',  ( -0.8801773607111009756, 33.06368534415484106, 1.068504757029289695E-15 ) ) ;
#42652 = DIRECTION ( 'NONE',  ( 0.4924235601034769871, 0.000000000000000000, -0.8703556959398941473 ) ) ;
#42653 = EDGE_CURVE ( 'NONE', #71557, #1898, #6848, .T. ) ;
#42654 = CARTESIAN_POINT ( 'NONE',  ( -4.164238869374098151, 46.59541550158063927, -3.795296366450310543 ) ) ;
#42655 = AXIS2_PLACEMENT_3D ( 'NONE', #13477, #20490, #57493 ) ;
#42656 = DIRECTION ( 'NONE',  ( 0.000000000000000000, 0.000000000000000000, -1.000000000000000000 ) ) ;
#42657 =( GEOMETRIC_REPRESENTATION_CONTEXT ( 3 ) GLOBAL_UNCERTAINTY_ASSIGNED_CONTEXT ( ( #69258 ) ) GLOBAL_UNIT_ASSIGNED_CONTEXT ( ( #21545, #44526, #90024 ) ) REPRESENTATION_CONTEXT ( 'NONE', 'WORKASPACE' ) );
#42658 = CARTESIAN_POINT ( 'NONE',  ( 16.40814093676323893, 35.79030133659708923, 11.09922568453595026 ) ) ;
#42659 = CARTESIAN_POINT ( 'NONE',  ( 10.00000000000000000, 21.81368534415484106, -10.88017736071110342 ) ) ;
#42660 = CARTESIAN_POINT ( 'NONE',  ( 1.472469842513823179, 51.42559781766745886, 4.923371831947296329 ) ) ;
#42661 = CARTESIAN_POINT ( 'NONE',  ( 19.42250999205614193, 50.14701867748817676, 5.440088680355555262 ) ) ;
#42662 = CARTESIAN_POINT ( 'NONE',  ( 6.204703633549690345, 37.84541550158063927, 14.16423886937410082 ) ) ;
#42663 = DIRECTION ( 'NONE',  ( 0.000000000000000000, 0.000000000000000000, 1.000000000000000000 ) ) ;
#42664 = CARTESIAN_POINT ( 'NONE',  ( 19.84674366389459621, 23.50893115100078390, 7.409399052514197653E-17 ) ) ;
#42665 = DIRECTION ( 'NONE',  ( 0.000000000000000000, 1.000000000000000000, 0.000000000000000000 ) ) ;
#42666 = CARTESIAN_POINT ( 'NONE',  ( 6.565887622018943937, 5.165301336597086568, 12.81628187352647430 ) ) ;
#42667 = ORIENTED_EDGE ( 'NONE', *, *, #13044, .F. ) ;
#42668 = DIRECTION ( 'NONE',  ( -1.000000000000000000, -0.000000000000000000, -0.000000000000000000 ) ) ;
#42669 =( NAMED_UNIT ( * ) SI_UNIT ( $, .STERADIAN. ) SOLID_ANGLE_UNIT ( ) );
#42670 = CARTESIAN_POINT ( 'NONE',  ( 20.88017736071110875, 15.77201867748817143, -2.915334737309920765 ) ) ;
#42671 = CARTESIAN_POINT ( 'NONE',  ( -4.164238869374099927, 22.01208216824730357, 3.795296366450308767 ) ) ;
#42672 = CARTESIAN_POINT ( 'NONE',  ( 2.791683348922237240, 15.38393115100078212, -7.208316651077763204 ) ) ;
#42673 = DIRECTION ( 'NONE',  ( 0.7826081568524191345, 0.000000000000000000, -0.6225146366376130835 ) ) ;
#42674 = CARTESIAN_POINT ( 'NONE',  ( -0.8801773607111008646, 33.27201867748817676, 2.915334737309923430 ) ) ;
#42675 = CARTESIAN_POINT ( 'NONE',  ( 18.17884179759848706, 13.66688879859523276, -6.499999999999968914 ) ) ;
#42676 = DIRECTION ( 'NONE',  ( -0.5905099943842175847, -0.8070303256584298035, 0.000000000000000000 ) ) ;
#42677 = ADVANCED_FACE ( 'NONE', ( #96887 ), #58851, .T. ) ;
#42678 = ORIENTED_EDGE ( 'NONE', *, *, #62762, .F. ) ;
#42679 = CARTESIAN_POINT ( 'NONE',  ( 0.000000000000000000, 0.000000000000000000, -8.000000000000000000 ) ) ;
#42680 = CARTESIAN_POINT ( 'NONE',  ( 0.1532563361054100626, 40.80059781766745886, -2.638427012816831230 ) ) ;
#42682 = ORIENTED_EDGE ( 'NONE', *, *, #56791, .F. ) ;
#42681 = EDGE_CURVE ( 'NONE', #88686, #30837, #44116, .T. ) ;
#42683 = EDGE_LOOP ( 'NONE', ( #70781, #95721, #35430, #25596 ) ) ;
#42684 = CARTESIAN_POINT ( 'NONE',  ( 0.2751277870542967463, 0.000000000000000000, 6.500000000000000888 ) ) ;
#42685 = CARTESIAN_POINT ( 'NONE',  ( 17.08211943468705130, 3.470415501580634388, 12.26659068614894998 ) ) ;
#42686 = CARTESIAN_POINT ( 'NONE',  ( -0.3689425029237881626, 12.42874883491396609, 10.36894250292379027 ) ) ;
#42687 = CARTESIAN_POINT ( 'NONE',  ( 15.44008868035555260, 49.73035201082150536, 9.422509992056143702 ) ) ;
#42688 = CARTESIAN_POINT ( 'NONE',  ( 10.00000000000000000, 50.55374883491396787, -14.16423886937410082 ) ) ;
#42689 = CARTESIAN_POINT ( 'NONE',  ( 6.565887622018943937, 3.081968003263753531, -12.81628187352647608 ) ) ;
#42690 = CARTESIAN_POINT ( 'NONE',  ( 5.076628168052704559, 30.17559781766745175, -8.527530157486179263 ) ) ;
#42691 = CARTESIAN_POINT ( 'NONE',  ( -16.94999999999999929, 100.0000000000000000, 7.896446609406727823 ) ) ;
#42693 = CARTESIAN_POINT ( 'NONE',  ( 21.09922568453595559, 12.04030133659708746, -6.408140936763230044 ) ) ;
#42692 = CARTESIAN_POINT ( 'NONE',  ( 4.559911319644449179, 32.23035201082150536, -9.422509992056141925 ) ) ;
#42694 = CARTESIAN_POINT ( 'NONE',  ( -2.266590686148945544, 2.220415501580634388, 7.082119434687048631 ) ) ;
#42695 = CARTESIAN_POINT ( 'NONE',  ( -0.3689425029237898834, 51.17874883491397497, -10.36894250292378850 ) ) ;
#42696 = EDGE_CURVE ( 'NONE', #32629, #20168, #5892, .T. ) ;
#42697 = AXIS2_PLACEMENT_3D ( 'NONE', #16857, #14902, #31347 ) ;
#42698 = CARTESIAN_POINT ( 'NONE',  ( 15.44008868035555793, 11.39701867748817143, -9.422509992056140149 ) ) ;
#42699 = CARTESIAN_POINT ( 'NONE',  ( 9.879999999999991900, 20.99999999999999645, 1.249999999999987121 ) ) ;
#42700 = DIRECTION ( 'NONE',  ( -0.8320502943378436100, 0.5547001962252291474, -0.000000000000000000 ) ) ;
#42701 = CARTESIAN_POINT ( 'NONE',  ( 8.527530157486175710, -36.07440218233254114, -4.923371831947298993 ) ) ;
#42702 = ORIENTED_EDGE ( 'NONE', *, *, #84704, .T. ) ;
#42703 = CARTESIAN_POINT ( 'NONE',  ( -46.44000000000001194, 100.8660254037844339, 9.500000000000000000 ) ) ;
#42704 = ORIENTED_EDGE ( 'NONE', *, *, #94550, .F. ) ;
#42705 = CARTESIAN_POINT ( 'NONE',  ( 17.20831665107776587, 32.88393115100078745, 7.208316651077764980 ) ) ;
#42706 = ORIENTED_EDGE ( 'NONE', *, *, #77720, .F. ) ;
#42707 = CARTESIAN_POINT ( 'NONE',  ( 13.79529636645031943, 40.34541550158063217, -14.16423886937409904 ) ) ;
#42708 = CARTESIAN_POINT ( 'NONE',  ( 5.076628168052703671, 36.84226448433412315, 8.527530157486179263 ) ) ;
#42709 = CARTESIAN_POINT ( 'NONE',  ( 0.5774900079438607392, 63.48035201082149825, 5.440088680355550821 ) ) ;
#42710 = DIRECTION ( 'NONE',  ( -1.000000000000000000, 0.000000000000000000, 0.000000000000000000 ) ) ;
#42711 = CARTESIAN_POINT ( 'NONE',  ( 0.5774900079438590739, 52.64701867748817676, -5.440088680355550821 ) ) ;
#42712 = CARTESIAN_POINT ( 'NONE',  ( 0.6178305044545818747, 53.49863466993041072, -9.382169495545419124 ) ) ;
#42713 = CARTESIAN_POINT ( 'NONE',  ( 3.469446951953614189E-15, 5.373634669930425822, 12.81628187352647608 ) ) ;
#42714 = ORIENTED_EDGE ( 'NONE', *, *, #86519, .T. ) ;
#42715 = CARTESIAN_POINT ( 'NONE',  ( 24.16423886937410614, 14.30374883491396787, 8.672049930838204340E-16 ) ) ;
#42716 = ORIENTED_EDGE ( 'NONE', *, *, #36058, .F. ) ;
#42717 = EDGE_CURVE ( 'NONE', #75803, #81788, #32923, .T. ) ;
#42718 = CARTESIAN_POINT ( 'NONE',  ( -2.816281873526471635, 23.91530133659708568, -3.434112377981056508 ) ) ;
#42719 = ORIENTED_EDGE ( 'NONE', *, *, #74909, .F. ) ;
#42720 = CARTESIAN_POINT ( 'NONE',  ( 10.00000000000000178, 40.37363466993042493, 12.81628187352647608 ) ) ;
#42721 = VECTOR ( 'NONE', #61745, 1000.000000000000000 ) ;
#42722 = CARTESIAN_POINT ( 'NONE',  ( 17.20831665107776587, 24.13393115100078035, -7.208316651077762316 ) ) ;
#42723 = CARTESIAN_POINT ( 'NONE',  ( 0.5774900079438590739, 12.64701867748817143, -5.440088680355550821 ) ) ;
#42724 = CARTESIAN_POINT ( 'NONE',  ( 6.565887622018943937, 55.16530133659709634, 12.81628187352647430 ) ) ;
#42725 = CARTESIAN_POINT ( 'NONE',  ( -46.68456736488006698, 103.6675473310227034, -5.775421524742656132 ) ) ;
#42726 = CARTESIAN_POINT ( 'NONE',  ( 14.92337183194729988, 44.34226448433412315, -8.527530157486177487 ) ) ;
#42727 = VECTOR ( 'NONE', #38692, 1000.000000000000000 ) ;
#42728 = ADVANCED_FACE ( 'NONE', ( #16815 ), #32783, .F. ) ;
#42729 = VECTOR ( 'NONE', #49319, 1000.000000000000114 ) ;
#42731 = VERTEX_POINT ( 'NONE', #47292 ) ;
#42730 = CARTESIAN_POINT ( 'NONE',  ( 0.5774900079438590739, 67.64701867748817676, -5.440088680355550821 ) ) ;
#42732 = CARTESIAN_POINT ( 'NONE',  ( 19.42250999205614548, 65.98035201082151957, -5.440088680355545492 ) ) ;
#42733 = CARTESIAN_POINT ( 'NONE',  ( 10.64017930668205736, 0.5000000000000004441, -10.57291749337215592 ) ) ;
#42734 = CARTESIAN_POINT ( 'NONE',  ( -1.926860441876563801, 44.89664270246083788, 3.195792623639529761 ) ) ;
#42735 = CARTESIAN_POINT ( 'NONE',  ( 17.20831665107776587, 22.88393115100078745, 7.208316651077764980 ) ) ;
#42736 = CARTESIAN_POINT ( 'NONE',  ( 6.565887622018943937, 23.08196800326375708, -12.81628187352647608 ) ) ;
#42737 = CARTESIAN_POINT ( 'NONE',  ( 6.579634127946654587, -87.99828267815715321, -2.750000000000000000 ) ) ;
#42738 = CARTESIAN_POINT ( 'NONE',  ( 14.92337183194729988, 39.34226448433412315, -8.527530157486177487 ) ) ;
#42739 = CARTESIAN_POINT ( 'NONE',  ( -9.000000000000001776, 80.99999999999994316, -1.249999999999987121 ) ) ;
#42740 = CARTESIAN_POINT ( 'NONE',  ( 13.79529636645030344, 23.26208216824730002, 14.16423886937410614 ) ) ;
#42741 = CARTESIAN_POINT ( 'NONE',  ( 18.52753015748617571, 33.09226448433411605, 4.923371831947298993 ) ) ;
#42742 = CARTESIAN_POINT ( 'NONE',  ( 21.09922568453594849, 46.20696800326376064, 6.408140936763242479 ) ) ;
#42743 = DIRECTION ( 'NONE',  ( 0.000000000000000000, 1.000000000000000000, 0.000000000000000000 ) ) ;
#42744 = CARTESIAN_POINT ( 'NONE',  ( 15.44008868035555793, 61.39701867748817676, -9.422509992056140149 ) ) ;
#42746 = CARTESIAN_POINT ( 'NONE',  ( 13.43411237798105340, 15.58196800326374998, 12.81628187352647963 ) ) ;
#42745 = B_SPLINE_CURVE_WITH_KNOTS ( 'NONE', 3,
 ( #91375, #70735, #52881, #86219, #17731, #90377 ),
 .UNSPECIFIED., .F., .F.,
 ( 4, 2, 4 ),
 ( 0.0002800518438787976978, 0.0006862575805824382581, 0.001092463317286078818 ),
 .UNSPECIFIED. ) ;
#42747 = DIRECTION ( 'NONE',  ( -0.000000000000000000, -1.000000000000000000, -0.000000000000000000 ) ) ;
#42748 = ORIENTED_EDGE ( 'NONE', *, *, #36474, .F. ) ;
#42749 = CARTESIAN_POINT ( 'NONE',  ( 17.20831665107776587, 37.88393115100078745, 7.208316651077764980 ) ) ;
#42750 = CARTESIAN_POINT ( 'NONE',  ( -0.8801773607111008646, 28.27201867748817321, 2.915334737309923430 ) ) ;
#42751 = CARTESIAN_POINT ( 'NONE',  ( -2.816281873526473856, 29.33196800326376064, 3.434112377981055619 ) ) ;
#42752 = CARTESIAN_POINT ( 'NONE',  ( 5.076628168052703671, 36.84226448433412315, 8.527530157486179263 ) ) ;
#42753 = CARTESIAN_POINT ( 'NONE',  ( 14.62232599144295264, 15.00000000000000888, 0.3548652576989754781 ) ) ;
#42754 = CARTESIAN_POINT ( 'NONE',  ( 12.91533473730993009, 36.60535201082151247, -10.88017736071109987 ) ) ;
#42755 = ORIENTED_EDGE ( 'NONE', *, *, #1056, .F. ) ;
#42756 = CARTESIAN_POINT ( 'NONE',  ( -3.897244926436033374, 3.994152527635309729E-16, -13.96644127841335958 ) ) ;
#42757 = CARTESIAN_POINT ( 'NONE',  ( 2.035157376598822676, 2.438685344154837953, -7.964842623401177768 ) ) ;
#42759 = CARTESIAN_POINT ( 'NONE',  ( 10.00000000000000178, 34.31368534415484106, 10.88017736071110342 ) ) ;
#42758 = CARTESIAN_POINT ( 'NONE',  ( 5.076628168052704559, 60.17559781766745175, -8.527530157486179263 ) ) ;
#42760 = DIRECTION ( 'NONE',  ( 0.000000000000000000, 0.000000000000000000, 1.000000000000000000 ) ) ;
#42761 = CARTESIAN_POINT ( 'NONE',  ( 7.084665262690076126, 54.10535201082151247, 10.88017736071109987 ) ) ;
#42763 = LINE ( 'NONE', #51747, #84659 ) ;
#42762 = CARTESIAN_POINT ( 'NONE',  ( 4.559911319644449179, 23.89701867748817321, 9.422509992056141925 ) ) ;
#42764 = FILL_AREA_STYLE_COLOUR ( '', #21196 ) ;
#42765 = CARTESIAN_POINT ( 'NONE',  ( 12.63842701281683922, 29.55059781766745175, -9.846743663894590881 ) ) ;
#42766 = DIRECTION ( 'NONE',  ( 0.8070303256584299145, -0.5905099943842175847, 0.000000000000000000 ) ) ;
#42767 = CARTESIAN_POINT ( 'NONE',  ( 0.1532563361054083140, 46.00893115100079456, 1.131784320476157264E-15 ) ) ;
#42768 = FACE_OUTER_BOUND ( 'NONE', #26296, .T. ) ;
#42770 = CARTESIAN_POINT ( 'NONE',  ( 6.829574850505126804, -88.00372650098204019, 3.750000000000001332 ) ) ;
#42769 = CARTESIAN_POINT ( 'NONE',  ( -4.164238869374099039, 56.80374883491397497, 8.674139862899312516E-16 ) ) ;
#42771 = DIRECTION ( 'NONE',  ( -0.000000000000000000, 1.000000000000000000, -0.000000000000000000 ) ) ;
#42772 = EDGE_CURVE ( 'NONE', #54617, #2502, #80823, .T. ) ;
#42773 = CARTESIAN_POINT ( 'NONE',  ( 2.917880565312950480, 10.97041550158063572, -12.26659068614894821 ) ) ;
#42774 = CARTESIAN_POINT ( 'NONE',  ( 6.204703633549690345, 32.84541550158063927, 14.16423886937410082 ) ) ;
#42775 = CARTESIAN_POINT ( 'NONE',  ( 6.565887622018943937, 0.1653013365970866511, 12.81628187352647430 ) ) ;
#42776 = CARTESIAN_POINT ( 'NONE',  ( 5.129999999999990123, 76.07179676972444327, 6.500000000000000888 ) ) ;
#42777 = ORIENTED_EDGE ( 'NONE', *, *, #86726, .F. ) ;
#42778 = CARTESIAN_POINT ( 'NONE',  ( 7.084665262690076126, 19.10535201082150181, 10.88017736071109987 ) ) ;
#42779 = CARTESIAN_POINT ( 'NONE',  ( 14.92337183194729633, 32.67559781766745175, 8.527530157486181039 ) ) ;
#42781 = CARTESIAN_POINT ( 'NONE',  ( -2.913501739333568707, 15.00000000000000000, -14.20427779279538960 ) ) ;
#42780 = CARTESIAN_POINT ( 'NONE',  ( -10.58521204051718101, -0.03417435944610275333, -11.99294302885424024 ) ) ;
#42782 = CARTESIAN_POINT ( 'NONE',  ( -0.8801773607111008646, 58.27201867748816966, 2.915334737309923430 ) ) ;
#42783 = FACE_OUTER_BOUND ( 'NONE', #70737, .T. ) ;
#42784 = CARTESIAN_POINT ( 'NONE',  ( 22.81628187352647785, 61.62363466993041783, 6.195893100308588602E-16 ) ) ;
#42785 = CARTESIAN_POINT ( 'NONE',  ( 22.81628187352648496, 26.83196800326374998, -3.434112377981050290 ) ) ;
#42786 = CARTESIAN_POINT ( 'NONE',  ( 17.20831665107776587, 34.13393115100078745, -7.208316651077762316 ) ) ;
#42787 = ORIENTED_EDGE ( 'NONE', *, *, #32753, .T. ) ;
#42788 = CARTESIAN_POINT ( 'NONE',  ( 1.472469842513823179, 0.5922644843341181575, -4.923371831947296329 ) ) ;
#42789 = CARTESIAN_POINT ( 'NONE',  ( -11.35178980618963784, 0.3639309078821091892, -9.804941009312090117 ) ) ;
#42790 = CARTESIAN_POINT ( 'NONE',  ( 2.917880565312950480, 65.97041550158063217, -12.26659068614894821 ) ) ;
#42791 = CARTESIAN_POINT ( 'NONE',  ( 17.96484262340118221, 19.93868534415484106, 7.964842623401181321 ) ) ;
#42792 = CARTESIAN_POINT ( 'NONE',  ( 24.16423886937410614, 44.30374883491397497, 8.672049930838204340E-16 ) ) ;
#42793 = CARTESIAN_POINT ( 'NONE',  ( 2.035157376598824452, 33.68868534415484106, 7.964842623401179544 ) ) ;
#42794 = MECHANICAL_DESIGN_GEOMETRIC_PRESENTATION_REPRESENTATION (  '', ( #65097 ), #1290 ) ;
#42795 = LINE ( 'NONE', #8250, #90458 ) ;
#42796 = CARTESIAN_POINT ( 'NONE',  ( 8.564643372776625796, 0.3639308585234187210, -12.31449893000744211 ) ) ;
#42797 = CARTESIAN_POINT ( 'NONE',  ( 10.58840669699852199, -98.14374106289703548, -4.000000000000000000 ) ) ;
#42798 = CARTESIAN_POINT ( 'NONE',  ( 2.791683348922237240, 5.383931151000785675, -7.208316651077763204 ) ) ;
#42799 = CARTESIAN_POINT ( 'NONE',  ( 10.64017930668198453, 0.5000000000000004441, 10.57291749337222875 ) ) ;
#42800 = CARTESIAN_POINT ( 'NONE',  ( 10.00000000000000178, 2.258931151000784787, 9.846743663894594434 ) ) ;
#42801 = CARTESIAN_POINT ( 'NONE',  ( 10.00000000000000178, 37.25893115100078745, 9.846743663894594434 ) ) ;
#42802 = CARTESIAN_POINT ( 'NONE',  ( 2.791683348922240793, 66.63393115100079456, 7.208316651077764092 ) ) ;
#42803 = AXIS2_PLACEMENT_3D ( 'NONE', #22137, #52620, #40087 ) ;
#42804 =( GEOMETRIC_REPRESENTATION_CONTEXT ( 3 ) GLOBAL_UNCERTAINTY_ASSIGNED_CONTEXT ( ( #1272 ) ) GLOBAL_UNIT_ASSIGNED_CONTEXT ( ( #83156, #68168, #45652 ) ) REPRESENTATION_CONTEXT ( 'NONE', 'WORKASPACE' ) );
#42805 = ADVANCED_FACE ( 'NONE', ( #32288 ), #48909, .T. ) ;
#42806 = VERTEX_POINT ( 'NONE', #38832 ) ;
#42807 = CARTESIAN_POINT ( 'NONE',  ( 13.43411237798105340, 40.58196800326375353, 12.81628187352647963 ) ) ;
#42808 = CARTESIAN_POINT ( 'NONE',  ( 15.44008868035555793, 66.39701867748817676, -9.422509992056140149 ) ) ;
#42809 = CARTESIAN_POINT ( 'NONE',  ( 10.00000000000000178, 50.37363466993042493, 12.81628187352647608 ) ) ;
#42811 = CARTESIAN_POINT ( 'NONE',  ( 5.076628168052703671, 41.84226448433411605, 8.527530157486179263 ) ) ;
#42810 = CARTESIAN_POINT ( 'NONE',  ( 20.36894250292379382, 63.67874883491396787, 10.36894250292379205 ) ) ;
#42812 = DIRECTION ( 'NONE',  ( 0.000000000000000000, 0.000000000000000000, 1.000000000000000000 ) ) ;
#42813 = CARTESIAN_POINT ( 'NONE',  ( 0.1532563361054100626, 65.80059781766745175, -2.638427012816831230 ) ) ;
#42814 = EDGE_CURVE ( 'NONE', #31058, #71952, #77299, .T. ) ;
#42815 = CARTESIAN_POINT ( 'NONE',  ( 13.79529636645030344, 33.26208216824730357, 14.16423886937410614 ) ) ;
#42816 = CARTESIAN_POINT ( 'NONE',  ( 7.361572987183169658, 44.96726448433412315, -9.846743663894592657 ) ) ;
#42817 = CARTESIAN_POINT ( 'NONE',  ( -0.1503990784575328643, 69.92552686551195507, 6.262539305110068177 ) ) ;
#42818 = CARTESIAN_POINT ( 'NONE',  ( 0.5774900079438590739, 37.64701867748817676, -5.440088680355550821 ) ) ;
#42819 = CARTESIAN_POINT ( 'NONE',  ( 2.035157376598822676, 52.43868534415483396, -7.964842623401177768 ) ) ;
#42820 = FACE_OUTER_BOUND ( 'NONE', #60039, .T. ) ;
#42821 = ORIENTED_EDGE ( 'NONE', *, *, #44484, .F. ) ;
#42822 = CARTESIAN_POINT ( 'NONE',  ( 0.6178305044545818747, 43.49863466993042493, -9.382169495545419124 ) ) ;
#42823 = CARTESIAN_POINT ( 'NONE',  ( 20.88017736071110164, 50.35535201082151247, 2.915334737309930979 ) ) ;
#42824 = ORIENTED_EDGE ( 'NONE', *, *, #95568, .T. ) ;
#42825 = CARTESIAN_POINT ( 'NONE',  ( 18.52753015748617571, 63.09226448433412315, 4.923371831947298993 ) ) ;
#42826 = CARTESIAN_POINT ( 'NONE',  ( 13.07751017357383994, 15.00000000000000000, -6.263284095430508458 ) ) ;
#42827 = CARTESIAN_POINT ( 'NONE',  ( 4.792102989642838651, 15.00000000000000000, 15.26149223938176291 ) ) ;
#42828 = VERTEX_POINT ( 'NONE', #69821 ) ;
#42829 = DIRECTION ( 'NONE',  ( 0.000000000000000000, 0.000000000000000000, 1.000000000000000000 ) ) ;
#42830 = CARTESIAN_POINT ( 'NONE',  ( -0.8801773607111009756, 13.06368534415483929, 1.068504757029289695E-15 ) ) ;
#42831 = CARTESIAN_POINT ( 'NONE',  ( -11.92686044187656513, 12.66212336850781206, 3.903127820947815962E-15 ) ) ;
#42832 = CARTESIAN_POINT ( 'NONE',  ( -4.164238869374099927, 67.01208216824728936, 3.795296366450308767 ) ) ;
#42833 = EDGE_CURVE ( 'NONE', #39764, #6556, #93591, .T. ) ;
#42834 = CARTESIAN_POINT ( 'NONE',  ( 10.00000000000000178, 18.05374883491396787, 14.16423886937410082 ) ) ;
#42835 = CARTESIAN_POINT ( 'NONE',  ( 4.559911319644449179, 22.23035201082150536, -9.422509992056141925 ) ) ;
#42836 = CARTESIAN_POINT ( 'NONE',  ( 1.472469842513823179, 55.59226448433412315, -4.923371831947296329 ) ) ;
#42837 = ORIENTED_EDGE ( 'NONE', *, *, #97835, .F. ) ;
#42838 = CARTESIAN_POINT ( 'NONE',  ( 12.63842701281683922, 64.55059781766745175, -9.846743663894590881 ) ) ;
#42839 = ORIENTED_EDGE ( 'NONE', *, *, #89400, .T. ) ;
#42840 = CARTESIAN_POINT ( 'NONE',  ( 2.035157376598824452, 48.68868534415483396, 7.964842623401179544 ) ) ;
#42841 = CARTESIAN_POINT ( 'NONE',  ( 7.361572987183170547, 62.05059781766745886, 9.846743663894590881 ) ) ;
#42842 = CARTESIAN_POINT ( 'NONE',  ( 3.591859063236763294, 33.29030133659708213, -11.09922568453595026 ) ) ;
#42844 = LINE ( 'NONE', #95852, #33513 ) ;
#42843 = CARTESIAN_POINT ( 'NONE',  ( -0.8801773607111009756, 8.063685344154837509, 1.068504757029289695E-15 ) ) ;
#42845 = CARTESIAN_POINT ( 'NONE',  ( 7.084665262690076126, 54.10535201082151247, 10.88017736071109987 ) ) ;
#42846 = CARTESIAN_POINT ( 'NONE',  ( 7.084665262690076126, 17.02201867748817676, -10.88017736071110164 ) ) ;
#42847 = ORIENTED_EDGE ( 'NONE', *, *, #53624, .F. ) ;
#42848 = CARTESIAN_POINT ( 'NONE',  ( 6.565887622018943937, 55.16530133659709634, 12.81628187352647430 ) ) ;
#42849 = CARTESIAN_POINT ( 'NONE',  ( 19.42250999205614548, 25.98035201082150891, -5.440088680355545492 ) ) ;
#42850 = CARTESIAN_POINT ( 'NONE',  ( 19.67858290521088804, 89.00000000000000000, 5.461713021790605360 ) ) ;
#42851 = B_SPLINE_CURVE_WITH_KNOTS ( 'NONE', 3,
 ( #76025, #75532, #7556, #45025, #38045, #29521 ),
 .UNSPECIFIED., .F., .F.,
 ( 4, 2, 4 ),
 ( 3.409110551477859173E-05, 0.0004400426677366043172, 0.0008459942299584299885 ),
 .UNSPECIFIED. ) ;
#42852 = CARTESIAN_POINT ( 'NONE',  ( 22.81628187352648496, 46.83196800326376064, -3.434112377981050290 ) ) ;
#42853 = CARTESIAN_POINT ( 'NONE',  ( 0.5774900079438590739, 52.64701867748817676, -5.440088680355550821 ) ) ;
#42854 = CARTESIAN_POINT ( 'NONE',  ( 0.1532563361054100626, 60.80059781766744464, -2.638427012816831230 ) ) ;
#42855 = EDGE_LOOP ( 'NONE', ( #43703, #62537, #37359, #45408, #82679, #66484 ) ) ;
#42856 = CARTESIAN_POINT ( 'NONE',  ( -0.1503990784575242878, 44.24884699246889852, -6.262539305110083276 ) ) ;
#42857 = VECTOR ( 'NONE', #37932, 1000.000000000000000 ) ;
#42858 = CARTESIAN_POINT ( 'NONE',  ( 17.20831665107776587, 62.88393115100078745, 7.208316651077764980 ) ) ;
#42860 = CARTESIAN_POINT ( 'NONE',  ( 19.84674366389459621, 53.50893115100078745, 7.409399052514197653E-17 ) ) ;
#42859 = DIRECTION ( 'NONE',  ( -0.9961946980917458783, 0.08715574274765407192, 0.000000000000000000 ) ) ;
#42861 = CARTESIAN_POINT ( 'NONE',  ( -0.8801773607111009756, 23.06368534415484106, 1.068504757029289695E-15 ) ) ;
#42862 = DIRECTION ( 'NONE',  ( 0.5547001962252290364, 0.8320502943378437211, 0.000000000000000000 ) ) ;
#42863 = CARTESIAN_POINT ( 'NONE',  ( 1.472469842513823179, 36.42559781766745175, 4.923371831947296329 ) ) ;
#42864 = CARTESIAN_POINT ( 'NONE',  ( -14.47650479471827722, 0.3639311865617156361, 3.928206833721935354 ) ) ;
#42867 = CARTESIAN_POINT ( 'NONE',  ( 14.92337183194729633, 7.675597817667451750, 8.527530157486181039 ) ) ;
#42866 = VECTOR ( 'NONE', #22287, 1000.000000000000227 ) ;
#42865 = CARTESIAN_POINT ( 'NONE',  ( 1.472469842513823179, 45.59226448433412315, -4.923371831947296329 ) ) ;
#42868 = SURFACE_STYLE_FILL_AREA ( #19378 ) ;
#42870 = ORIENTED_EDGE ( 'NONE', *, *, #30452, .T. ) ;
#42869 = CARTESIAN_POINT ( 'NONE',  ( 1.472469842513823179, 56.42559781766745886, 4.923371831947296329 ) ) ;
#42871 = CIRCLE ( 'NONE', #23695, 7.000000000000002665 ) ;
#42872 = CARTESIAN_POINT ( 'NONE',  ( 10.00000000000000000, 42.87363466993042493, -12.81628187352647608 ) ) ;
#42873 = CARTESIAN_POINT ( 'NONE',  ( 1.472469842513823179, 41.42559781766745886, 4.923371831947296329 ) ) ;
#42874 = CARTESIAN_POINT ( 'NONE',  ( -7.595945211628163385, 4.385640548506873962E-16, -12.35117874301652030 ) ) ;
#42875 = CARTESIAN_POINT ( 'NONE',  ( 24.16423886937409904, 54.09541550158063217, 3.795296366450317205 ) ) ;
#42876 = CARTESIAN_POINT ( 'NONE',  ( 17.20831665107776587, 29.13393115100078390, -7.208316651077762316 ) ) ;
#42877 = CARTESIAN_POINT ( 'NONE',  ( 8.439016546559892973, 15.00000000000000000, -11.79122553964970876 ) ) ;
#42878 = CARTESIAN_POINT ( 'NONE',  ( 13.79529636645031943, 55.34541550158062506, -14.16423886937409904 ) ) ;
#42879 = CARTESIAN_POINT ( 'NONE',  ( 7.595945211628331251, 3.826527677142797770E-16, -12.35117874301642082 ) ) ;
#42880 = CARTESIAN_POINT ( 'NONE',  ( 20.88017736071110875, 20.77201867748816611, -2.915334737309920765 ) ) ;
#42881 = CARTESIAN_POINT ( 'NONE',  ( 10.00000000000000178, 38.05374883491396787, 14.16423886937410082 ) ) ;
#42883 = DIRECTION ( 'NONE',  ( -1.000000000000000000, 5.782411586589362323E-17, 0.000000000000000000 ) ) ;
#42882 = CARTESIAN_POINT ( 'NONE',  ( 24.16423886937410614, 54.51208216824730357, -3.795296366450302550 ) ) ;
#42884 = DIRECTION ( 'NONE',  ( -0.000000000000000000, 1.000000000000000000, 0.000000000000000000 ) ) ;
#42885 = CARTESIAN_POINT ( 'NONE',  ( 7.361572987183169658, 14.96726448433411960, -9.846743663894592657 ) ) ;
#42886 = CARTESIAN_POINT ( 'NONE',  ( 10.00000000000000000, -2.126365330069579951, -12.81628187352647608 ) ) ;
#42887 = EDGE_LOOP ( 'NONE', ( #30509, #25929, #95062, #70627 ) ) ;
#42888 = CARTESIAN_POINT ( 'NONE',  ( 0.5774900079438607392, 53.48035201082151247, 5.440088680355550821 ) ) ;
#42889 = CARTESIAN_POINT ( 'NONE',  ( -0.03743638938522213938, 64.25197528031021932, -6.399506433553973750 ) ) ;
#42890 = EDGE_CURVE ( 'NONE', #79587, #49408, #38929, .T. ) ;
#42891 = CARTESIAN_POINT ( 'NONE',  ( 2.791683348922240793, 51.63393115100078745, 7.208316651077764092 ) ) ;
#42892 = CARTESIAN_POINT ( 'NONE',  ( 0.000000000000000000, 15.00000000000000000, 0.000000000000000000 ) ) ;
#42893 = CARTESIAN_POINT ( 'NONE',  ( 5.076628168052704559, 55.17559781766745175, -8.527530157486179263 ) ) ;
#42894 = CARTESIAN_POINT ( 'NONE',  ( 14.97687855664614176, 14.49999999999999112, 0.8325315005901842147 ) ) ;
#42895 = ORIENTED_EDGE ( 'NONE', *, *, #18000, .T. ) ;
#42896 = CARTESIAN_POINT ( 'NONE',  ( 2.917880565312948704, 32.63708216824730357, 12.26659068614894643 ) ) ;
#42897 = DIRECTION ( 'NONE',  ( 2.569960705150826877E-16, -1.000000000000000000, 0.000000000000000000 ) ) ;
#42899 = CARTESIAN_POINT ( 'NONE',  ( -8.235571585149871865, 7.296802177851538396, -8.235571585149866536 ) ) ;
#42898 = CARTESIAN_POINT ( 'NONE',  ( -6.982525766850296911, -88.11956318484570261, -2.750000000000000444 ) ) ;
#42900 = CARTESIAN_POINT ( 'NONE',  ( 15.44008868035555260, 19.73035201082150536, 9.422509992056143702 ) ) ;
#42901 = CARTESIAN_POINT ( 'NONE',  ( 19.38216949554541557, 32.24863466993041783, -9.382169495545420901 ) ) ;
#42902 = CARTESIAN_POINT ( 'NONE',  ( -6.898461952320240620, 15.00000000000000000, -12.75387089053316636 ) ) ;
#42903 = CARTESIAN_POINT ( 'NONE',  ( -2.816281873526471635, 63.91530133659708923, -3.434112377981056508 ) ) ;
#42904 = VERTEX_POINT ( 'NONE', #71778 ) ;
#42905 = CARTESIAN_POINT ( 'NONE',  ( 6.034747819266367053, -36.07388523691940918, -3.999999999999999556 ) ) ;
#42906 = CARTESIAN_POINT ( 'NONE',  ( -2.266590686148945544, 27.22041550158063572, 7.082119434687048631 ) ) ;
#42907 = CARTESIAN_POINT ( 'NONE',  ( 17.08211943468705840, 5.137082168247300906, -12.26659068614894466 ) ) ;
#42908 = CARTESIAN_POINT ( 'NONE',  ( -5.580435433942707135, -28.67474180225212166, 4.000000000000000888 ) ) ;
#42909 = CARTESIAN_POINT ( 'NONE',  ( -0.8801773607110991993, 17.85535201082150536, -2.915334737309923874 ) ) ;
#42910 = CARTESIAN_POINT ( 'NONE',  ( 3.969999999999999751, 37.00000000000000000, 4.000000000000000000 ) ) ;
#42911 =( GEOMETRIC_REPRESENTATION_CONTEXT ( 3 ) GLOBAL_UNCERTAINTY_ASSIGNED_CONTEXT ( ( #33183 ) ) GLOBAL_UNIT_ASSIGNED_CONTEXT ( ( #3816, #95288, #69246 ) ) REPRESENTATION_CONTEXT ( 'NONE', 'WORKASPACE' ) );
#42912 = CARTESIAN_POINT ( 'NONE',  ( -1.236355250167479491, 14.95037107271117627, 14.70131747622448515 ) ) ;
#42913 = CARTESIAN_POINT ( 'NONE',  ( 19.42250999205614548, 45.98035201082150536, -5.440088680355545492 ) ) ;
#42914 = CARTESIAN_POINT ( 'NONE',  ( 12.91533473730993009, 56.60535201082151247, -10.88017736071109987 ) ) ;
#42915 = CARTESIAN_POINT ( 'NONE',  ( 16.40814093676324603, 7.456968003263754419, -11.09922568453594671 ) ) ;
#42916 = PLANE ( 'NONE',  #7595 ) ;
#42917 = LINE ( 'NONE', #4442, #78689 ) ;
#42918 = CARTESIAN_POINT ( 'NONE',  ( 14.92337183194729988, 24.34226448433411960, -8.527530157486177487 ) ) ;
#42919 = CARTESIAN_POINT ( 'NONE',  ( -0.6999999999999957367, 99.99999999999998579, -8.525133428036873795 ) ) ;
#42920 = CARTESIAN_POINT ( 'NONE',  ( -0.8801773607111009756, 38.06368534415484106, 1.068504757029289695E-15 ) ) ;
#42921 = EDGE_CURVE ( 'NONE', #48471, #17079, #4274, .T. ) ;
#42922 = CARTESIAN_POINT ( 'NONE',  ( -1.099225684535947600, 8.706968003263753531, -6.408140936763238038 ) ) ;
#42923 = CARTESIAN_POINT ( 'NONE',  ( 15.44008868035555793, 56.39701867748817676, -9.422509992056140149 ) ) ;
#42924 = CARTESIAN_POINT ( 'NONE',  ( 0.1532563361054100626, 25.80059781766744820, -2.638427012816831230 ) ) ;
#42925 = CARTESIAN_POINT ( 'NONE',  ( -1.099225684535947600, 44.54030133659708923, 6.408140936763237150 ) ) ;
#42926 = CARTESIAN_POINT ( 'NONE',  ( 0.1532563361054082862, 1.217264484334117824, 2.638427012816831674 ) ) ;
#42927 = EDGE_LOOP ( 'NONE', ( #88602, #64020, #82769, #19124 ) ) ;
#42928 = FACE_OUTER_BOUND ( 'NONE', #3474, .T. ) ;
#42929 = CARTESIAN_POINT ( 'NONE',  ( 12.91533473730992121, 14.52201867748817143, 10.88017736071110164 ) ) ;
#42931 = CARTESIAN_POINT ( 'NONE',  ( -4.164238869374098151, 21.59541550158063217, -3.795296366450310543 ) ) ;
#42930 = CARTESIAN_POINT ( 'NONE',  ( 13.43411237798106583, 62.66530133659708923, -12.81628187352647252 ) ) ;
#42932 = CARTESIAN_POINT ( 'NONE',  ( 0.1532563361054083140, 31.00893115100078390, 1.131784320476157264E-15 ) ) ;
#42933 = CIRCLE ( 'NONE', #98844, 0.2500000000000002220 ) ;
#42934 = CARTESIAN_POINT ( 'NONE',  ( 15.44008868035555793, 16.39701867748817321, -9.422509992056140149 ) ) ;
#42935 = CARTESIAN_POINT ( 'NONE',  ( -0.8801773607110991993, 2.855352010821504471, -2.915334737309923874 ) ) ;
#42936 = EDGE_LOOP ( 'NONE', ( #95733, #41855, #78262, #97441 ) ) ;
#42937 = CARTESIAN_POINT ( 'NONE',  ( 0.5774900079438607392, 18.48035201082150536, 5.440088680355550821 ) ) ;
#42938 = CIRCLE ( 'NONE', #18964, 0.5000000000000004441 ) ;
#42939 = CARTESIAN_POINT ( 'NONE',  ( 17.96484262340118221, 31.18868534415483751, -7.964842623401177768 ) ) ;
#42941 = CARTESIAN_POINT ( 'NONE',  ( 2.035157376598822676, 42.43868534415483396, -7.964842623401177768 ) ) ;
#42940 = CARTESIAN_POINT ( 'NONE',  ( -12.60589901313231564, 14.63606915354311155, 8.129656208641970139 ) ) ;
#42942 = CIRCLE ( 'NONE', #17408, 14.49999999999999822 ) ;
#42943 = ORIENTED_EDGE ( 'NONE', *, *, #80851, .F. ) ;
#42944 = CARTESIAN_POINT ( 'NONE',  ( 0.1532563361054082862, 61.21726448433412315, 2.638427012816831674 ) ) ;
#42945 = CARTESIAN_POINT ( 'NONE',  ( 19.42250999205614193, 20.14701867748817321, 5.440088680355555262 ) ) ;
#42946 = CARTESIAN_POINT ( 'NONE',  ( 7.361572987183170547, 67.05059781766746596, 9.846743663894590881 ) ) ;
#42947 = B_SPLINE_CURVE_WITH_KNOTS ( 'NONE', 3,
 ( #28650, #90625, #90131, #59140, #21661, #82641 ),
 .UNSPECIFIED., .F., .F.,
 ( 4, 2, 4 ),
 ( 0.0002800392683747309061, 0.0006862448819834952689, 0.001092450495592259523 ),
 .UNSPECIFIED. ) ;
#42948 = DIRECTION ( 'NONE',  ( 0.000000000000000000, -1.000000000000000000, 0.000000000000000000 ) ) ;
#42949 = CARTESIAN_POINT ( 'NONE',  ( 16.40814093676324603, 57.45696800326375353, -11.09922568453594671 ) ) ;
#42950 = CARTESIAN_POINT ( 'NONE',  ( -1.899999999999997247, 98.49999999999998579, 8.000000000000000000 ) ) ;
#42951 = CARTESIAN_POINT ( 'NONE',  ( 24.16423886937410614, 34.30374883491396787, 8.672049930838204340E-16 ) ) ;
#42952 = CARTESIAN_POINT ( 'NONE',  ( 15.44008868035555793, 46.39701867748817676, -9.422509992056140149 ) ) ;
#42953 = CARTESIAN_POINT ( 'NONE',  ( 12.91533473730993009, 36.60535201082151247, -10.88017736071109987 ) ) ;
#42954 = PLANE ( 'NONE',  #65753 ) ;
#42955 = CARTESIAN_POINT ( 'NONE',  ( -14.17193700899788134, -0.03417435944610275333, -1.489530601564206247 ) ) ;
#42956 = CARTESIAN_POINT ( 'NONE',  ( 19.84674366389459621, 43.50893115100078745, 7.409399052514197653E-17 ) ) ;
#42957 = VERTEX_POINT ( 'NONE', #35239 ) ;
#42958 = CARTESIAN_POINT ( 'NONE',  ( 5.076628168052703671, 21.84226448433411960, 8.527530157486179263 ) ) ;
#42959 = CARTESIAN_POINT ( 'NONE',  ( -12.81628187352647963, -26.08469866340290721, -3.434112377981046293 ) ) ;
#42960 = ADVANCED_FACE ( 'NONE', ( #87750 ), #61544, .T. ) ;
#42961 = CARTESIAN_POINT ( 'NONE',  ( 4.559911319644449179, 8.897018677488171434, 9.422509992056141925 ) ) ;
#42962 = CARTESIAN_POINT ( 'NONE',  ( 7.361572987183169658, 29.96726448433411960, -9.846743663894592657 ) ) ;
#42963 = CARTESIAN_POINT ( 'NONE',  ( -2.816281873526473856, 14.12363466993041961, 9.499525473075851096E-16 ) ) ;
#42964 = CARTESIAN_POINT ( 'NONE',  ( 7.084665262690076126, 54.10535201082151247, 10.88017736071109987 ) ) ;
#42966 = CARTESIAN_POINT ( 'NONE',  ( -2.816281873526471635, 53.91530133659709634, -3.434112377981056508 ) ) ;
#42965 = CARTESIAN_POINT ( 'NONE',  ( 20.88017736071110164, 25.35535201082150891, 2.915334737309930979 ) ) ;
#42967 = CARTESIAN_POINT ( 'NONE',  ( 17.08211943468705130, 38.47041550158063217, 12.26659068614894998 ) ) ;
#42968 = ADVANCED_FACE ( 'NONE', ( #82333 ), #45330, .T. ) ;
#42969 = DIRECTION ( 'NONE',  ( 0.5224985647159551272, 0.000000000000000000, -0.8526401643540884034 ) ) ;
#42970 = ORIENTED_EDGE ( 'NONE', *, *, #50461, .T. ) ;
#42971 = CARTESIAN_POINT ( 'NONE',  ( 5.076628168052703671, 66.84226448433412315, 8.527530157486179263 ) ) ;
#42972 = DIRECTION ( 'NONE',  ( -0.9969173337331274087, 0.000000000000000000, -0.07845909572785238206 ) ) ;
#42973 = CARTESIAN_POINT ( 'NONE',  ( 0.5774900079438590739, 27.64701867748817676, -5.440088680355550821 ) ) ;
#42974 = CARTESIAN_POINT ( 'NONE',  ( 18.52753015748617571, 63.09226448433412315, 4.923371831947298993 ) ) ;
#42975 = ORIENTED_EDGE ( 'NONE', *, *, #77203, .F. ) ;
#42976 = CARTESIAN_POINT ( 'NONE',  ( 2.791683348922237240, 20.38393115100078745, -7.208316651077763204 ) ) ;
#42977 = CARTESIAN_POINT ( 'NONE',  ( 19.84674366389459266, 13.71726448433411782, -2.638427012816827677 ) ) ;
#42978 = CARTESIAN_POINT ( 'NONE',  ( 14.92337183194729633, 27.67559781766745530, 8.527530157486181039 ) ) ;
#42979 = CARTESIAN_POINT ( 'NONE',  ( 10.00000000000000178, 17.25893115100078745, 9.846743663894594434 ) ) ;
#42980 = CARTESIAN_POINT ( 'NONE',  ( 0.1532563361054083140, 1.008931151000784787, 1.131784320476157264E-15 ) ) ;
#42981 = CARTESIAN_POINT ( 'NONE',  ( -6.866255446112624838, -80.67934795256483937, 2.500000000000000000 ) ) ;
#42983 = CARTESIAN_POINT ( 'NONE',  ( -2.913501739333569152, 4.140530414402051497E-16, -14.20427779279538960 ) ) ;
#42982 = CARTESIAN_POINT ( 'NONE',  ( 7.361572987183169658, -0.03273551566588185635, -9.846743663894592657 ) ) ;
#42984 = CARTESIAN_POINT ( 'NONE',  ( 7.361572987183170547, 7.050597817667451750, 9.846743663894590881 ) ) ;
#42986 = VERTEX_POINT ( 'NONE', #97868 ) ;
#42985 = CARTESIAN_POINT ( 'NONE',  ( 0.1532563361054083140, 26.00893115100078745, 1.131784320476157264E-15 ) ) ;
#42987 = DIRECTION ( 'NONE',  ( -0.1822355254921514123, 0.000000000000000000, 0.9832549075639538394 ) ) ;
#42988 = CARTESIAN_POINT ( 'NONE',  ( -2.816281873526471635, 3.915301336597087456, -3.434112377981056508 ) ) ;
#42989 = CARTESIAN_POINT ( 'NONE',  ( 6.204703633549690345, 20.76208216824730357, -14.16423886937410259 ) ) ;
#42990 = DIRECTION ( 'NONE',  ( 0.5664062369248313855, 0.000000000000000000, -0.8241261886220165866 ) ) ;
#42991 = CARTESIAN_POINT ( 'NONE',  ( 24.16423886937410614, 14.51208216824730179, -3.795296366450302550 ) ) ;
#42992 = CARTESIAN_POINT ( 'NONE',  ( -0.3689425029237881626, 52.42874883491396076, 10.36894250292379027 ) ) ;
#42993 = AXIS2_PLACEMENT_3D ( 'NONE', #57662, #40344, #63311 ) ;
#42994 = CARTESIAN_POINT ( 'NONE',  ( 6.204703633549690345, 0.7620821682473009062, -14.16423886937410259 ) ) ;
#42995 = CARTESIAN_POINT ( 'NONE',  ( 2.917880565312948704, 7.637082168247301794, 12.26659068614894643 ) ) ;
#42996 = CARTESIAN_POINT ( 'NONE',  ( 4.559911319644449179, 32.23035201082150536, -9.422509992056141925 ) ) ;
#42997 = DIRECTION ( 'NONE',  ( 0.000000000000000000, 1.000000000000000000, 0.000000000000000000 ) ) ;
#42998 = VERTEX_POINT ( 'NONE', #29328 ) ;
#42999 = CARTESIAN_POINT ( 'NONE',  ( 18.52753015748617571, 18.09226448433411960, 4.923371831947298993 ) ) ;
#43001 = CARTESIAN_POINT ( 'NONE',  ( 19.84674366389459266, 28.30059781766745886, 2.638427012816836559 ) ) ;
#43000 = CARTESIAN_POINT ( 'NONE',  ( 10.00000000000000000, 61.81368534415484106, -10.88017736071110342 ) ) ;
#43002 = CARTESIAN_POINT ( 'NONE',  ( 20.88017736071110164, 10.35535201082150714, 2.915334737309930979 ) ) ;
#43003 = CARTESIAN_POINT ( 'NONE',  ( 16.40814093676323893, 40.79030133659708923, 11.09922568453595026 ) ) ;
#43004 = CARTESIAN_POINT ( 'NONE',  ( 0.1532563361054100626, 45.80059781766745886, -2.638427012816831230 ) ) ;
#43005 = VECTOR ( 'NONE', #68548, 1000.000000000000000 ) ;
#43006 = FACE_OUTER_BOUND ( 'NONE', #17972, .T. ) ;
#43007 = ADVANCED_FACE ( 'NONE', ( #98862 ), #91317, .F. ) ;
#43008 = CARTESIAN_POINT ( 'NONE',  ( 16.40814093676323893, 40.79030133659708923, 11.09922568453595026 ) ) ;
#43009 = CARTESIAN_POINT ( 'NONE',  ( -10.36894250292378317, -27.57125116508602503, 10.36894250292379560 ) ) ;
#43010 = CARTESIAN_POINT ( 'NONE',  ( 19.84674366389459621, 43.50893115100078745, 7.409399052514197653E-17 ) ) ;
#43011 = CARTESIAN_POINT ( 'NONE',  ( 6.204703633549690345, 30.76208216824730357, -14.16423886937410259 ) ) ;
#43012 = EDGE_LOOP ( 'NONE', ( #27909, #4224, #21095, #54821 ) ) ;
#43013 = CYLINDRICAL_SURFACE ( 'NONE', #82693, 15.00000000000000000 ) ;
#43014 = EDGE_CURVE ( 'NONE', #65339, #19933, #47234, .T. ) ;
#43015 = CARTESIAN_POINT ( 'NONE',  ( -0.8801773607110991993, 47.85535201082150536, -2.915334737309923874 ) ) ;
#43016 = CARTESIAN_POINT ( 'NONE',  ( 19.42250999205614548, 55.98035201082150536, -5.440088680355545492 ) ) ;
#43017 = CARTESIAN_POINT ( 'NONE',  ( -0.3689425029237898834, 41.17874883491397497, -10.36894250292378850 ) ) ;
#43018 = CARTESIAN_POINT ( 'NONE',  ( 5.076628168052704559, 65.17559781766745175, -8.527530157486179263 ) ) ;
#43019 = CARTESIAN_POINT ( 'NONE',  ( 3.591859063236763294, 63.29030133659708923, -11.09922568453595026 ) ) ;
#43020 = CARTESIAN_POINT ( 'NONE',  ( 7.084665262690076126, 37.02201867748817676, -10.88017736071110164 ) ) ;
#43021 = CARTESIAN_POINT ( 'NONE',  ( -5.780262629516635720, -39.80185923444033591, -2.500000000000000000 ) ) ;
#43022 = VECTOR ( 'NONE', #47125, 1000.000000000000000 ) ;
#43023 = CARTESIAN_POINT ( 'NONE',  ( 19.38216949554541202, 25.99863466993042138, 9.382169495545424454 ) ) ;
#43024 = CARTESIAN_POINT ( 'NONE',  ( 5.076628168052704559, 60.17559781766745175, -8.527530157486179263 ) ) ;
#43025 = CARTESIAN_POINT ( 'NONE',  ( -7.964842623401179544, 17.43868534415483751, -7.964842623401174215 ) ) ;
#43026 = CARTESIAN_POINT ( 'NONE',  ( 19.42250999205614193, 5.147018677488171434, 5.440088680355555262 ) ) ;
#43027 = CARTESIAN_POINT ( 'NONE',  ( -0.1503990784575328643, 70.00000000000000000, 6.262539305110068177 ) ) ;
#43028 = ORIENTED_EDGE ( 'NONE', *, *, #47684, .T. ) ;
#43029 = AXIS2_PLACEMENT_3D ( 'NONE', #9981, #48945, #27424 ) ;
#43030 = CARTESIAN_POINT ( 'NONE',  ( 17.96484262340118221, 6.188685344154836621, -7.964842623401177768 ) ) ;
#43031 = SURFACE_STYLE_USAGE ( .BOTH. , #28017 ) ;
#43032 = CARTESIAN_POINT ( 'NONE',  ( 4.559911319644449179, 62.23035201082150536, -9.422509992056141925 ) ) ;
#43033 = CARTESIAN_POINT ( 'NONE',  ( 20.88017736071110164, 65.35535201082150536, 2.915334737309930979 ) ) ;
#43034 = DIRECTION ( 'NONE',  ( 0.000000000000000000, 1.000000000000000000, 0.000000000000000000 ) ) ;
#43035 = EDGE_CURVE ( 'NONE', #96234, #76621, #17798, .T. ) ;
#43036 = CARTESIAN_POINT ( 'NONE',  ( 5.076628168052704559, 30.17559781766745175, -8.527530157486179263 ) ) ;
#43037 = CARTESIAN_POINT ( 'NONE',  ( 0.5774900079438590739, 22.64701867748817321, -5.440088680355550821 ) ) ;
#43038 = B_SPLINE_CURVE_WITH_KNOTS ( 'NONE', 3,
 ( #6222, #13220, #19736, #5734 ),
 .UNSPECIFIED., .F., .F.,
 ( 4, 4 ),
 ( 4.906538933386798166E-18, 0.002392975128318429977 ),
 .UNSPECIFIED. ) ;
#43039 = CARTESIAN_POINT ( 'NONE',  ( -2.816281873526473856, 4.123634669930420493, 9.499525473075851096E-16 ) ) ;
#43041 = CARTESIAN_POINT ( 'NONE',  ( 8.731067818237042033, 9.537123368507819166, 8.731067818237033151 ) ) ;
#43040 = CARTESIAN_POINT ( 'NONE',  ( 20.88017736071110519, 40.56368534415484106, 2.639326808657452039E-16 ) ) ;
#43042 = FACE_OUTER_BOUND ( 'NONE', #68737, .T. ) ;
#43043 = CARTESIAN_POINT ( 'NONE',  ( 3.591859063236763294, 43.29030133659708923, -11.09922568453595026 ) ) ;
#43044 = VERTEX_POINT ( 'NONE', #9800 ) ;
#43045 = CARTESIAN_POINT ( 'NONE',  ( 4.559911319644449179, 58.89701867748817676, 9.422509992056141925 ) ) ;
#43046 = EDGE_CURVE ( 'NONE', #72967, #57072, #66351, .T. ) ;
#43048 = DIRECTION ( 'NONE',  ( -1.000000000000000000, 0.000000000000000000, 0.000000000000000000 ) ) ;
#43047 = CARTESIAN_POINT ( 'NONE',  ( 3.591859063236763294, 23.29030133659708568, -11.09922568453595026 ) ) ;
#43049 = CARTESIAN_POINT ( 'NONE',  ( 20.15039907845753220, 31.74884699246888786, 6.262539305110077059 ) ) ;
#43050 = CARTESIAN_POINT ( 'NONE',  ( 17.96484262340118221, 39.93868534415484106, 7.964842623401181321 ) ) ;
#43051 = CARTESIAN_POINT ( 'NONE',  ( 10.00000000000000000, 64.75893115100078035, -9.846743663894594434 ) ) ;
#43052 = CARTESIAN_POINT ( 'NONE',  ( 17.08211943468705840, 65.13708216824730357, -12.26659068614894466 ) ) ;
#43053 = CARTESIAN_POINT ( 'NONE',  ( 7.361572987183170547, 52.05059781766745175, 9.846743663894590881 ) ) ;
#43054 = AXIS2_PLACEMENT_3D ( 'NONE', #53833, #37366, #84345 ) ;
#43055 = CARTESIAN_POINT ( 'NONE',  ( 1.472469842513823179, 5.592264484334118713, -4.923371831947296329 ) ) ;
#43056 = CARTESIAN_POINT ( 'NONE',  ( 7.084665262690076126, 67.02201867748817676, -10.88017736071110164 ) ) ;
#43057 = DIRECTION ( 'NONE',  ( 1.000000000000000000, 0.000000000000000000, -0.000000000000000000 ) ) ;
#43058 = CARTESIAN_POINT ( 'NONE',  ( 2.917880565312950480, 25.97041550158063572, -12.26659068614894821 ) ) ;
#43059 = CARTESIAN_POINT ( 'NONE',  ( 10.93542311823294355, -97.13826248502067529, -3.749999999999999112 ) ) ;
#43060 = ORIENTED_EDGE ( 'NONE', *, *, #19153, .T. ) ;
#43061 = ORIENTED_EDGE ( 'NONE', *, *, #17005, .T. ) ;
#43062 = CARTESIAN_POINT ( 'NONE',  ( 7.084665262690076126, 2.022018677488171434, -10.88017736071110164 ) ) ;
#43063 = CARTESIAN_POINT ( 'NONE',  ( 24.16423886937410614, 54.51208216824730357, -3.795296366450302550 ) ) ;
#43064 = CARTESIAN_POINT ( 'NONE',  ( 5.076628168052703671, 31.84226448433412315, 8.527530157486179263 ) ) ;
#43065 = CARTESIAN_POINT ( 'NONE',  ( 13.48086198287162141, -0.03417435944610275333, 8.610676897597548063 ) ) ;
#43066 = SURFACE_STYLE_FILL_AREA ( #96577 ) ;
#43067 = CARTESIAN_POINT ( 'NONE',  ( -2.266590686148945544, 52.22041550158064638, 7.082119434687048631 ) ) ;
#43068 = CARTESIAN_POINT ( 'NONE',  ( -0.1503990784575328643, 0.1277717457861260453, 6.262539305110068177 ) ) ;
#43069 = CARTESIAN_POINT ( 'NONE',  ( 14.92337183194729988, 14.34226448433411782, -8.527530157486177487 ) ) ;
#43070 = DIRECTION ( 'NONE',  ( 0.000000000000000000, 0.000000000000000000, 1.000000000000000000 ) ) ;
#43071 = CARTESIAN_POINT ( 'NONE',  ( 9.846743663894594434, 3.508931151000788340, -2.168404344971008868E-15 ) ) ;
#43072 = ORIENTED_EDGE ( 'NONE', *, *, #2208, .F. ) ;
#43073 = ORIENTED_EDGE ( 'NONE', *, *, #51830, .T. ) ;
#43074 = ORIENTED_EDGE ( 'NONE', *, *, #51136, .F. ) ;
#43076 = CARTESIAN_POINT ( 'NONE',  ( 15.44008868035555260, 19.73035201082150536, 9.422509992056143702 ) ) ;
#43075 = CARTESIAN_POINT ( 'NONE',  ( 7.084665262690076126, 14.10535201082150358, 10.88017736071109987 ) ) ;
#43078 = CARTESIAN_POINT ( 'NONE',  ( -2.816281873526471635, 18.91530133659708213, -3.434112377981056508 ) ) ;
#43077 = CARTESIAN_POINT ( 'NONE',  ( 18.52753015748617571, 53.09226448433412315, 4.923371831947298993 ) ) ;
#43079 = DIRECTION ( 'NONE',  ( 0.000000000000000000, 0.000000000000000000, -1.000000000000000000 ) ) ;
#43080 = EDGE_CURVE ( 'NONE', #75865, #24283, #55795, .T. ) ;
#43081 = CARTESIAN_POINT ( 'NONE',  ( 13.43411237798106583, 27.66530133659708568, -12.81628187352647252 ) ) ;
#43082 = ORIENTED_EDGE ( 'NONE', *, *, #54749, .F. ) ;
#43083 = CARTESIAN_POINT ( 'NONE',  ( 17.20831665107776587, 37.88393115100078745, 7.208316651077764980 ) ) ;
#43084 = CARTESIAN_POINT ( 'NONE',  ( 2.917880565312950480, 65.97041550158063217, -12.26659068614894821 ) ) ;
#43085 = ORIENTED_EDGE ( 'NONE', *, *, #53278, .T. ) ;
#43086 = CARTESIAN_POINT ( 'NONE',  ( 22.26659068614894466, 63.88708216824730357, 7.082119434687054849 ) ) ;
#43087 = VERTEX_POINT ( 'NONE', #94267 ) ;
#43088 = CARTESIAN_POINT ( 'NONE',  ( 0.5774900079438590739, 47.64701867748817676, -5.440088680355550821 ) ) ;
#43089 = CARTESIAN_POINT ( 'NONE',  ( 12.91533473730992121, 44.52201867748816966, 10.88017736071110164 ) ) ;
#43090 = CARTESIAN_POINT ( 'NONE',  ( 7.084665262690076126, 49.10535201082149825, 10.88017736071109987 ) ) ;
#43091 = CARTESIAN_POINT ( 'NONE',  ( 12.91533473730993009, 36.60535201082151247, -10.88017736071109987 ) ) ;
#43092 = VECTOR ( 'NONE', #12825, 1000.000000000000000 ) ;
#43093 = CARTESIAN_POINT ( 'NONE',  ( -6.382347221874564269, 14.49999999999999112, 13.57444820018227993 ) ) ;
#43094 = VECTOR ( 'NONE', #78983, 1000.000000000000000 ) ;
#43096 = VERTEX_POINT ( 'NONE', #24325 ) ;
#43095 = CARTESIAN_POINT ( 'NONE',  ( 10.04755927614745481, 15.00000000000000533, 10.62803196998863697 ) ) ;
#43097 = CARTESIAN_POINT ( 'NONE',  ( 7.361572987183170547, 32.05059781766745175, 9.846743663894590881 ) ) ;
#43098 = ORIENTED_EDGE ( 'NONE', *, *, #57228, .F. ) ;
#43099 = CARTESIAN_POINT ( 'NONE',  ( 2.791683348922237240, 55.38393115100078745, -7.208316651077763204 ) ) ;
#43100 = CARTESIAN_POINT ( 'NONE',  ( 4.856044144387611894, -2.574980159653071059E-16, 13.79699902221164720 ) ) ;
#43101 = EDGE_CURVE ( 'NONE', #49843, #12573, #86291, .T. ) ;
#43102 = SURFACE_SIDE_STYLE ('',( #81099 ) ) ;
#43103 = CIRCLE ( 'NONE', #51099, 15.00000000000000000 ) ;
#43104 = CARTESIAN_POINT ( 'NONE',  ( 0.000000000000000000, 36.75000000000000000, 2.750000000000000000 ) ) ;
#43105 = DIRECTION ( 'NONE',  ( 0.000000000000000000, 0.000000000000000000, 1.000000000000000000 ) ) ;
#43106 = CARTESIAN_POINT ( 'NONE',  ( 18.52753015748618282, 38.92559781766745175, -4.923371831947291888 ) ) ;
#43107 = CARTESIAN_POINT ( 'NONE',  ( -4.164238869374099927, 62.01208216824728936, 3.795296366450308767 ) ) ;
#43108 = CARTESIAN_POINT ( 'NONE',  ( 17.84635730667659104, 63.63791097397319874, 6.499999999999953815 ) ) ;
#43109 = ORIENTED_EDGE ( 'NONE', *, *, #68592, .F. ) ;
#43110 = DIRECTION ( 'NONE',  ( 0.000000000000000000, -1.000000000000000000, 0.000000000000000000 ) ) ;
#43111 = CARTESIAN_POINT ( 'NONE',  ( 5.076628168052704559, 35.17559781766745175, -8.527530157486179263 ) ) ;
#43112 = CYLINDRICAL_SURFACE ( 'NONE', #8392, 0.5000000000000004441 ) ;
#43113 = CARTESIAN_POINT ( 'NONE',  ( 22.81628187352648496, 1.831968003263753753, -3.434112377981050290 ) ) ;
#43114 = CARTESIAN_POINT ( 'NONE',  ( 14.92337183194729633, 12.67559781766745353, 8.527530157486181039 ) ) ;
#43115 = DIRECTION ( 'NONE',  ( 0.000000000000000000, 0.000000000000000000, 1.000000000000000000 ) ) ;
#43116 = EDGE_CURVE ( 'NONE', #37093, #52793, #85799, .T. ) ;
#43117 = CARTESIAN_POINT ( 'NONE',  ( 1.472469842513823179, 10.59226448433411782, -4.923371831947296329 ) ) ;
#43118 = CARTESIAN_POINT ( 'NONE',  ( 5.076628168052703671, 56.84226448433412315, 8.527530157486179263 ) ) ;
#43119 = CARTESIAN_POINT ( 'NONE',  ( 26.00000000000000355, 35.99999999999997158, 10.00000000000000000 ) ) ;
#43120 = EDGE_CURVE ( 'NONE', #8841, #952, #8759, .T. ) ;
#43121 = VERTEX_POINT ( 'NONE', #63761 ) ;
#43122 = CARTESIAN_POINT ( 'NONE',  ( 17.96484262340118221, 4.938685344154837509, 7.964842623401181321 ) ) ;
#43123 = CARTESIAN_POINT ( 'NONE',  ( -4.164238869374099039, 11.80374883491396965, 8.674139862899312516E-16 ) ) ;
#43124 = CARTESIAN_POINT ( 'NONE',  ( 0.1532563361054082862, 16.21726448433411960, 2.638427012816831674 ) ) ;
#43125 = CARTESIAN_POINT ( 'NONE',  ( 7.084665262690076126, 54.10535201082151247, 10.88017736071109987 ) ) ;
#43126 = CARTESIAN_POINT ( 'NONE',  ( 13.43411237798105340, 20.58196800326374643, 12.81628187352647963 ) ) ;
#43127 = CARTESIAN_POINT ( 'NONE',  ( -0.3289641300567998083, 58.07879003517447813, 5.963430220938281678 ) ) ;
#43128 = FACE_OUTER_BOUND ( 'NONE', #39017, .T. ) ;
#43129 = CARTESIAN_POINT ( 'NONE',  ( 10.00000000000000178, 0.3736346699304200492, 12.81628187352647608 ) ) ;
#43130 = CARTESIAN_POINT ( 'NONE',  ( 14.92337183194729633, 17.67559781766745175, 8.527530157486181039 ) ) ;
#43131 = CARTESIAN_POINT ( 'NONE',  ( 9.422509992056141925, -19.01964798917849109, -5.440088680355554374 ) ) ;
#43132 = CARTESIAN_POINT ( 'NONE',  ( 13.43411237798105340, 15.58196800326374998, 12.81628187352647963 ) ) ;
#43133 = CARTESIAN_POINT ( 'NONE',  ( -11.33436264776094404, -69.53389133807300482, -4.000000000000000000 ) ) ;
#43134 = CARTESIAN_POINT ( 'NONE',  ( 4.559911319644449179, 27.23035201082150536, -9.422509992056141925 ) ) ;
#43135 = LINE ( 'NONE', #28135, #53180 ) ;
#43136 = CARTESIAN_POINT ( 'NONE',  ( 6.204703633549690345, 45.76208216824729647, -14.16423886937410259 ) ) ;
#43137 = CARTESIAN_POINT ( 'NONE',  ( 10.00000000000000178, 70.00000000000000000, 0.000000000000000000 ) ) ;
#43138 = CARTESIAN_POINT ( 'NONE',  ( -0.8801773607110991993, 27.85535201082150181, -2.915334737309923874 ) ) ;
#43139 = VECTOR ( 'NONE', #64295, 1000.000000000000000 ) ;
#43140 = CARTESIAN_POINT ( 'NONE',  ( 1.472469842513823179, 50.59226448433411605, -4.923371831947296329 ) ) ;
#43141 = ADVANCED_FACE ( 'NONE', ( #77790 ), #44312, .T. ) ;
#43142 = CARTESIAN_POINT ( 'NONE',  ( -0.8801773607111008646, 53.27201867748816966, 2.915334737309923430 ) ) ;
#43143 = CARTESIAN_POINT ( 'NONE',  ( 13.79529636645030344, 33.26208216824730357, 14.16423886937410614 ) ) ;
#43144 = FACE_OUTER_BOUND ( 'NONE', #68794, .T. ) ;
#43145 = UNCERTAINTY_MEASURE_WITH_UNIT (LENGTH_MEASURE( 1.000000000000000082E-05 ), #7920, 'distance_accuracy_value', 'NONE');
#43146 = CARTESIAN_POINT ( 'NONE',  ( 19.84674366389459266, 33.71726448433410894, -2.638427012816827677 ) ) ;
#43147 = CARTESIAN_POINT ( 'NONE',  ( 22.81628187352647785, 61.41530133659709634, 3.434112377981063169 ) ) ;
#43148 = CIRCLE ( 'NONE', #89475, 14.49999999999999822 ) ;
#43149 = CARTESIAN_POINT ( 'NONE',  ( 10.00000000000000178, 0.3736346699304200492, 12.81628187352647608 ) ) ;
#43150 = ORIENTED_EDGE ( 'NONE', *, *, #47408, .T. ) ;
#43151 = CARTESIAN_POINT ( 'NONE',  ( 7.084665262690076126, 27.02201867748817676, -10.88017736071110164 ) ) ;
#43152 = EDGE_CURVE ( 'NONE', #3873, #47878, #96120, .T. ) ;
#43153 = DIRECTION ( 'NONE',  ( 0.000000000000000000, 1.000000000000000000, 0.000000000000000000 ) ) ;
#43154 = CARTESIAN_POINT ( 'NONE',  ( 6.937721053838227014, -80.66520463107747219, 2.750000000000000000 ) ) ;
#43155 = STYLED_ITEM ( 'NONE', ( #39844 ), #19831 ) ;
#43156 = CARTESIAN_POINT ( 'NONE',  ( 2.035157376598822676, 12.43868534415483751, -7.964842623401177768 ) ) ;
#43157 = CARTESIAN_POINT ( 'NONE',  ( 2.035157376598822676, 67.43868534415484817, -7.964842623401177768 ) ) ;
#43158 = CARTESIAN_POINT ( 'NONE',  ( 22.26659068614894466, 18.88708216824730002, 7.082119434687054849 ) ) ;
#43159 = CARTESIAN_POINT ( 'NONE',  ( 14.92337183194729633, 17.67559781766745175, 8.527530157486181039 ) ) ;
#43160 = CARTESIAN_POINT ( 'NONE',  ( 7.361572987183169658, 59.96726448433410894, -9.846743663894592657 ) ) ;
#43161 = CARTESIAN_POINT ( 'NONE',  ( 17.96484262340118221, 34.93868534415482685, 7.964842623401181321 ) ) ;
#43162 = CARTESIAN_POINT ( 'NONE',  ( 0.2751277870542911952, 34.36607318730131055, -6.499999999999992006 ) ) ;
#43163 = FACE_OUTER_BOUND ( 'NONE', #66808, .T. ) ;
#43164 = VECTOR ( 'NONE', #16293, 1000.000000000000000 ) ;
#43165 = ORIENTED_EDGE ( 'NONE', *, *, #40534, .F. ) ;
#43166 = DIRECTION ( 'NONE',  ( 5.818595309480552676E-17, 1.000000000000000000, -0.000000000000000000 ) ) ;
#43167 = CARTESIAN_POINT ( 'NONE',  ( 1.472469842513823179, 51.42559781766745886, 4.923371831947296329 ) ) ;
#43168 = ORIENTED_EDGE ( 'NONE', *, *, #52270, .F. ) ;
#43169 = ORIENTED_EDGE ( 'NONE', *, *, #29241, .T. ) ;
#43170 = DIRECTION ( 'NONE',  ( 0.000000000000000000, 0.000000000000000000, 1.000000000000000000 ) ) ;
#43171 = CARTESIAN_POINT ( 'NONE',  ( -4.164238869374098151, 26.59541550158063217, -3.795296366450310543 ) ) ;
#43172 = CARTESIAN_POINT ( 'NONE',  ( -4.164238869374099039, 6.803748834913967869, 8.674139862899312516E-16 ) ) ;
#43173 = CARTESIAN_POINT ( 'NONE',  ( 15.44008868035555260, 64.73035201082151957, 9.422509992056143702 ) ) ;
#43174 = CARTESIAN_POINT ( 'NONE',  ( -4.164238869374099039, 51.80374883491396787, 8.674139862899312516E-16 ) ) ;
#43175 = CARTESIAN_POINT ( 'NONE',  ( 10.00000000000000178, 0.3736346699304200492, 12.81628187352647608 ) ) ;
#43176 = CARTESIAN_POINT ( 'NONE',  ( 19.84674366389459621, 33.50893115100078745, 7.409399052514197653E-17 ) ) ;
#43178 = CARTESIAN_POINT ( 'NONE',  ( 22.81628187352647785, 11.41530133659708390, 3.434112377981063169 ) ) ;
#43177 = CARTESIAN_POINT ( 'NONE',  ( 4.559911319644449179, 28.89701867748817321, 9.422509992056141925 ) ) ;
#43179 = CARTESIAN_POINT ( 'NONE',  ( 22.26659068614894466, 3.887082168247300906, 7.082119434687054849 ) ) ;
#43180 = CARTESIAN_POINT ( 'NONE',  ( 22.26659068614895176, 49.72041550158063927, -7.082119434687042414 ) ) ;
#43181 = CARTESIAN_POINT ( 'NONE',  ( 20.88017736071110875, 15.77201867748817143, -2.915334737309920765 ) ) ;
#43182 = CARTESIAN_POINT ( 'NONE',  ( 18.72515096720569971, 5.055090184799359676, 6.500000000000000000 ) ) ;
#43183 = DIRECTION ( 'NONE',  ( 0.000000000000000000, 1.000000000000000000, 0.000000000000000000 ) ) ;
#43184 = CARTESIAN_POINT ( 'NONE',  ( 12.91533473730993009, 46.60535201082150536, -10.88017736071109987 ) ) ;
#43185 = AXIS2_PLACEMENT_3D ( 'NONE', #92094, #32566, #32062 ) ;
#43186 = ORIENTED_EDGE ( 'NONE', *, *, #57470, .T. ) ;
#43187 = ORIENTED_EDGE ( 'NONE', *, *, #72783, .T. ) ;
#43188 = ORIENTED_EDGE ( 'NONE', *, *, #51539, .T. ) ;
#43189 = CARTESIAN_POINT ( 'NONE',  ( 17.08211943468705840, 40.13708216824731068, -12.26659068614894466 ) ) ;
#43190 = CARTESIAN_POINT ( 'NONE',  ( 18.52753015748617571, 53.09226448433412315, 4.923371831947298993 ) ) ;
#43191 = CARTESIAN_POINT ( 'NONE',  ( 2.035157376598824452, 58.68868534415482685, 7.964842623401179544 ) ) ;
#43192 = CARTESIAN_POINT ( 'NONE',  ( -19.64999999999999858, 98.99999999999998579, -8.000000000000000000 ) ) ;
#43193 = CARTESIAN_POINT ( 'NONE',  ( 7.084665262690076126, 52.02201867748816255, -10.88017736071110164 ) ) ;
#43194 = AXIS2_PLACEMENT_3D ( 'NONE', #14731, #22717, #82212 ) ;
#43195 = CARTESIAN_POINT ( 'NONE',  ( -2.816281873526473856, 59.12363466993042493, 9.499525473075851096E-16 ) ) ;
#43196 = CARTESIAN_POINT ( 'NONE',  ( -6.408140936763246032, 8.290301336597091009, -11.09922568453594316 ) ) ;
#43197 = VERTEX_POINT ( 'NONE', #72735 ) ;
#43198 = CARTESIAN_POINT ( 'NONE',  ( 6.204703633549690345, 20.76208216824730357, -14.16423886937410259 ) ) ;
#43199 = CARTESIAN_POINT ( 'NONE',  ( 13.43411237798106583, 17.66530133659708923, -12.81628187352647252 ) ) ;
#43200 = VERTEX_POINT ( 'NONE', #72253 ) ;
#43201 = CARTESIAN_POINT ( 'NONE',  ( 6.565887622018943937, 38.08196800326376064, -12.81628187352647608 ) ) ;
#43202 = CARTESIAN_POINT ( 'NONE',  ( 7.084665262690076126, 17.02201867748817676, -10.88017736071110164 ) ) ;
#43203 = CARTESIAN_POINT ( 'NONE',  ( 12.63842701281683034, 37.46726448433411605, 9.846743663894596210 ) ) ;
#43204 = CARTESIAN_POINT ( 'NONE',  ( 2.035157376598824452, 13.68868534415483751, 7.964842623401179544 ) ) ;
#43205 = CARTESIAN_POINT ( 'NONE',  ( 21.09922568453595559, 57.04030133659708923, -6.408140936763230044 ) ) ;
#43206 = CARTESIAN_POINT ( 'NONE',  ( 19.84674366389459621, 48.50893115100078745, 7.409399052514197653E-17 ) ) ;
#43207 = DIRECTION ( 'NONE',  ( 0.000000000000000000, 0.000000000000000000, 1.000000000000000000 ) ) ;
#43208 = CARTESIAN_POINT ( 'NONE',  ( -3.192513988408218761, 15.00000000000000533, 14.27292421863748473 ) ) ;
#43209 = DIRECTION ( 'NONE',  ( -0.000000000000000000, -1.000000000000000000, -0.000000000000000000 ) ) ;
#43210 = FACE_OUTER_BOUND ( 'NONE', #29045, .T. ) ;
#43211 = DIRECTION ( 'NONE',  ( -1.000000000000000000, 0.000000000000000000, 0.000000000000000000 ) ) ;
#43212 = CARTESIAN_POINT ( 'NONE',  ( 5.076628168052703671, 16.84226448433411960, 8.527530157486179263 ) ) ;
#43213 = CARTESIAN_POINT ( 'NONE',  ( 19.38216949554541202, 25.99863466993042138, 9.382169495545424454 ) ) ;
#43214 = AXIS2_PLACEMENT_3D ( 'NONE', #46361, #76849, #76368 ) ;
#43215 = SURFACE_STYLE_FILL_AREA ( #4254 ) ;
#43216 = VECTOR ( 'NONE', #9475, 1000.000000000000000 ) ;
#43217 = ORIENTED_EDGE ( 'NONE', *, *, #24251, .T. ) ;
#43218 = CARTESIAN_POINT ( 'NONE',  ( 18.52753015748617571, 63.09226448433412315, 4.923371831947298993 ) ) ;
#43219 = CARTESIAN_POINT ( 'NONE',  ( -9.876730923139378504, 0.5000000000000004441, 11.28938378619056415 ) ) ;
#43220 = CARTESIAN_POINT ( 'NONE',  ( 6.204703633549690345, 15.76208216824730179, -14.16423886937410259 ) ) ;
#43221 = CARTESIAN_POINT ( 'NONE',  ( 18.52753015748618282, 48.92559781766745886, -4.923371831947291888 ) ) ;
#43222 = CARTESIAN_POINT ( 'NONE',  ( 3.591859063236761518, 39.95696800326375353, 11.09922568453594849 ) ) ;
#43224 = FACE_OUTER_BOUND ( 'NONE', #49870, .T. ) ;
#43223 = DIRECTION ( 'NONE',  ( -1.000000000000000000, 0.000000000000000000, 0.000000000000000000 ) ) ;
#43225 = CARTESIAN_POINT ( 'NONE',  ( 20.88017736071110875, 60.77201867748817676, -2.915334737309920765 ) ) ;
#43226 = EDGE_CURVE ( 'NONE', #27622, #45246, #74687, .T. ) ;
#43227 = AXIS2_PLACEMENT_3D ( 'NONE', #88691, #59674, #19218 ) ;
#43228 = DIRECTION ( 'NONE',  ( -0.000000000000000000, 0.000000000000000000, -1.000000000000000000 ) ) ;
#43229 = CARTESIAN_POINT ( 'NONE',  ( 2.791683348922240793, 41.63393115100078745, 7.208316651077764092 ) ) ;
#43230 = CARTESIAN_POINT ( 'NONE',  ( 7.084665262690076126, 34.10535201082151247, 10.88017736071109987 ) ) ;
#43231 = CARTESIAN_POINT ( 'NONE',  ( 0.6178305044545838731, 44.74863466993042493, 9.382169495545420901 ) ) ;
#43232 = DIRECTION ( 'NONE',  ( 0.000000000000000000, -1.000000000000000000, 0.000000000000000000 ) ) ;
#43233 = EDGE_CURVE ( 'NONE', #58661, #12573, #66194, .T. ) ;
#43234 = CARTESIAN_POINT ( 'NONE',  ( 0.5774900079438590739, 37.64701867748817676, -5.440088680355550821 ) ) ;
#43235 = EDGE_CURVE ( 'NONE', #63974, #27580, #11263, .T. ) ;
#43236 = ORIENTED_EDGE ( 'NONE', *, *, #24390, .F. ) ;
#43237 = CARTESIAN_POINT ( 'NONE',  ( 2.035157376598824452, 68.68868534415484817, 7.964842623401179544 ) ) ;
#43238 = CARTESIAN_POINT ( 'NONE',  ( 0.5774900079438590739, 12.64701867748817143, -5.440088680355550821 ) ) ;
#43240 = CARTESIAN_POINT ( 'NONE',  ( 17.96484262340118221, 49.93868534415484106, 7.964842623401181321 ) ) ;
#43239 = CARTESIAN_POINT ( 'NONE',  ( 12.63842701281683922, 59.55059781766744464, -9.846743663894590881 ) ) ;
#43241 = DIRECTION ( 'NONE',  ( -0.02617694830787626811, 0.000000000000000000, 0.9996573249755572599 ) ) ;
#43242 = CARTESIAN_POINT ( 'NONE',  ( 17.96484262340118221, 66.18868534415483396, -7.964842623401177768 ) ) ;
#43244 = DIRECTION ( 'NONE',  ( 1.000000000000000000, 0.000000000000000000, 0.000000000000000000 ) ) ;
#43243 = CARTESIAN_POINT ( 'NONE',  ( 20.88017736071110519, 30.56368534415484106, 2.639326808657452039E-16 ) ) ;
#43245 = CARTESIAN_POINT ( 'NONE',  ( 5.076628168052703671, 1.842264484334118047, 8.527530157486179263 ) ) ;
#43246 = CARTESIAN_POINT ( 'NONE',  ( 0.1532563361054083140, 21.00893115100078745, 1.131784320476157264E-15 ) ) ;
#43247 = CARTESIAN_POINT ( 'NONE',  ( -8.900000000000002132, 80.99999999999994316, -3.000000000000000000 ) ) ;
#43248 = CARTESIAN_POINT ( 'NONE',  ( -7.082119434687044190, 7.637082168247301794, 12.26659068614894998 ) ) ;
#43249 = CARTESIAN_POINT ( 'NONE',  ( 2.791683348922240793, 51.63393115100078745, 7.208316651077764092 ) ) ;
#43251 = CARTESIAN_POINT ( 'NONE',  ( 4.395800986235852470, -0.8373804211230448935, 3.750000000000000000 ) ) ;
#43250 = CARTESIAN_POINT ( 'NONE',  ( 22.26659068614895176, 59.72041550158063927, -7.082119434687042414 ) ) ;
#43252 = AXIS2_PLACEMENT_3D ( 'NONE', #68112, #27628, #36116 ) ;
#43253 = CARTESIAN_POINT ( 'NONE',  ( -8.439016546559740206, 3.923478264313957572E-16, -11.79122553964984910 ) ) ;
#43254 = CARTESIAN_POINT ( 'NONE',  ( 24.16423886937409904, 4.095415501580634832, 3.795296366450317205 ) ) ;
#43255 = CARTESIAN_POINT ( 'NONE',  ( -4.164238869374098151, 41.59541550158061796, -3.795296366450310543 ) ) ;
#43256 = CARTESIAN_POINT ( 'NONE',  ( 19.38216949554541202, 0.9986346699304200492, 9.382169495545424454 ) ) ;
#43257 = CIRCLE ( 'NONE', #68833, 6.999999999999995559 ) ;
#43258 = ORIENTED_EDGE ( 'NONE', *, *, #44571, .T. ) ;
#43259 = CARTESIAN_POINT ( 'NONE',  ( 17.96484262340118221, 19.93868534415484106, 7.964842623401181321 ) ) ;
#43260 = CARTESIAN_POINT ( 'NONE',  ( 1.472469842513823179, 31.42559781766745530, 4.923371831947296329 ) ) ;
#43262 = CARTESIAN_POINT ( 'NONE',  ( -12.19495285927234463, 90.49761223356972550, -7.228801115472371031 ) ) ;
#43261 = DIRECTION ( 'NONE',  ( -0.008726535498374266009, 0.000000000000000000, 0.9999619230641713097 ) ) ;
#43263 = CARTESIAN_POINT ( 'NONE',  ( 8.979999999999991545, 21.00000000000000000, 0.000000000000000000 ) ) ;
#43264 = CARTESIAN_POINT ( 'NONE',  ( -2.816281873526471635, 23.91530133659708568, -3.434112377981056508 ) ) ;
#43265 = CARTESIAN_POINT ( 'NONE',  ( 19.84674366389459621, 28.50893115100078745, 7.409399052514197653E-17 ) ) ;
#43266 = VERTEX_POINT ( 'NONE', #41782 ) ;
#43267 = CARTESIAN_POINT ( 'NONE',  ( 2.791683348922237240, 10.38393115100078390, -7.208316651077763204 ) ) ;
#43268 = EDGE_CURVE ( 'NONE', #72111, #32092, #23121, .T. ) ;
#43269 = CARTESIAN_POINT ( 'NONE',  ( 34.56412365047464874, 11.49999999999999645, 9.500000000000000000 ) ) ;
#43270 = CARTESIAN_POINT ( 'NONE',  ( 2.917880565312948704, 62.63708216824730357, 12.26659068614894643 ) ) ;
#43271 = CARTESIAN_POINT ( 'NONE',  ( 0.5774900079438607392, 8.480352010821505360, 5.440088680355550821 ) ) ;
#43272 = CARTESIAN_POINT ( 'NONE',  ( 24.16423886937410614, 39.30374883491396787, 8.672049930838204340E-16 ) ) ;
#43273 = CARTESIAN_POINT ( 'NONE',  ( 0.5774900079438607392, 43.48035201082151247, 5.440088680355550821 ) ) ;
#43274 = CARTESIAN_POINT ( 'NONE',  ( 12.91533473730992121, 64.52201867748817676, 10.88017736071110164 ) ) ;
#43275 = CARTESIAN_POINT ( 'NONE',  ( -13.61464873478178284, 14.49999999999999112, 6.296136897217746942 ) ) ;
#43276 = CARTESIAN_POINT ( 'NONE',  ( -6.000000000000014211, 80.32179676972448590, 4.000000000000000000 ) ) ;
#43277 = CARTESIAN_POINT ( 'NONE',  ( 1.472469842513823179, 26.42559781766745175, 4.923371831947296329 ) ) ;
#43278 = CARTESIAN_POINT ( 'NONE',  ( -7.750000000000000000, 41.24999999999999289, 6.250000000000000000 ) ) ;
#43279 = CARTESIAN_POINT ( 'NONE',  ( 0.1532563361054100626, 10.80059781766745175, -2.638427012816831230 ) ) ;
#43280 = DIRECTION ( 'NONE',  ( -0.000000000000000000, 0.000000000000000000, 1.000000000000000000 ) ) ;
#43281 = CARTESIAN_POINT ( 'NONE',  ( 10.00000000000000000, 34.75893115100078745, -9.846743663894594434 ) ) ;
#43282 = CARTESIAN_POINT ( 'NONE',  ( 7.361572987183170547, 57.05059781766744464, 9.846743663894590881 ) ) ;
#43283 = CARTESIAN_POINT ( 'NONE',  ( 0.5774900079438590739, 42.64701867748816966, -5.440088680355550821 ) ) ;
#43284 = EDGE_CURVE ( 'NONE', #47816, #93851, #80253, .T. ) ;
#43285 = VERTEX_POINT ( 'NONE', #57740 ) ;
#43286 = CARTESIAN_POINT ( 'NONE',  ( 0.6178305044545838731, 49.74863466993041072, 9.382169495545420901 ) ) ;
#43287 = CARTESIAN_POINT ( 'NONE',  ( 15.44008868035555260, 64.73035201082151957, 9.422509992056143702 ) ) ;
#43288 = CARTESIAN_POINT ( 'NONE',  ( 0.6178305044545838731, 44.74863466993042493, 9.382169495545420901 ) ) ;
#43290 = CARTESIAN_POINT ( 'NONE',  ( 10.00000000000000178, 37.25893115100078745, 9.846743663894594434 ) ) ;
#43289 = CARTESIAN_POINT ( 'NONE',  ( 17.08211943468705130, 53.47041550158063217, 12.26659068614894998 ) ) ;
#43291 = CARTESIAN_POINT ( 'NONE',  ( 17.75000000000000000, 84.07179676972448590, 12.00000000000000000 ) ) ;
#43292 = CARTESIAN_POINT ( 'NONE',  ( 0.1532563361054082862, 66.21726448433413736, 2.638427012816831674 ) ) ;
#43293 = CARTESIAN_POINT ( 'NONE',  ( 6.204703633549690345, 17.84541550158063217, 14.16423886937410082 ) ) ;
#43294 = CARTESIAN_POINT ( 'NONE',  ( -4.164238869374099927, 42.01208216824728936, 3.795296366450308767 ) ) ;
#43295 = CARTESIAN_POINT ( 'NONE',  ( 7.361572987183170547, 47.05059781766745175, 9.846743663894590881 ) ) ;
#43296 = COLOUR_RGB ( '', 0.72549020, 0.75294118, 0.79215686) ;
#43297 = DIRECTION ( 'NONE',  ( -0.8338858220671696575, 0.000000000000000000, 0.5519369853120560387 ) ) ;
#43298 = CARTESIAN_POINT ( 'NONE',  ( -0.8801773607110991993, 37.85535201082151247, -2.915334737309923874 ) ) ;
#43299 = CARTESIAN_POINT ( 'NONE',  ( 19.42250999205614548, 60.98035201082151247, -5.440088680355545492 ) ) ;
#43300 = CARTESIAN_POINT ( 'NONE',  ( 20.88017736071110519, 50.56368534415484106, 2.639326808657452039E-16 ) ) ;
#43301 = VERTEX_POINT ( 'NONE', #58730 ) ;
#43302 = CARTESIAN_POINT ( 'NONE',  ( 3.591859063236763294, 48.29030133659708923, -11.09922568453595026 ) ) ;
#43303 = ORIENTED_EDGE ( 'NONE', *, *, #21978, .F. ) ;
#43304 = CARTESIAN_POINT ( 'NONE',  ( -0.8801773607110991993, 62.85535201082150536, -2.915334737309923874 ) ) ;
#43305 = ORIENTED_EDGE ( 'NONE', *, *, #23736, .T. ) ;
#43306 = CARTESIAN_POINT ( 'NONE',  ( 6.204703633549690345, 12.84541550158063572, 14.16423886937410082 ) ) ;
#43307 = CARTESIAN_POINT ( 'NONE',  ( 18.52753015748618282, 8.925597817667451750, -4.923371831947291888 ) ) ;
#43308 = DIRECTION ( 'NONE',  ( 0.6246950475544238435, 0.7808688094430307203, 0.000000000000000000 ) ) ;
#43309 = ORIENTED_EDGE ( 'NONE', *, *, #62861, .T. ) ;
#43310 = DIRECTION ( 'NONE',  ( 0.000000000000000000, 1.000000000000000000, 0.000000000000000000 ) ) ;
#43311 = CARTESIAN_POINT ( 'NONE',  ( -0.8801773607111009756, 18.06368534415484106, 1.068504757029289695E-15 ) ) ;
#43312 = CARTESIAN_POINT ( 'NONE',  ( 18.72515096720590577, 61.07228050351029935, -6.499999999999718447 ) ) ;
#43313 = CARTESIAN_POINT ( 'NONE',  ( 24.16423886937410614, 14.51208216824730179, -3.795296366450302550 ) ) ;
#43314 = CARTESIAN_POINT ( 'NONE',  ( 17.96484262340118221, 19.93868534415484106, 7.964842623401181321 ) ) ;
#43315 = CARTESIAN_POINT ( 'NONE',  ( 7.361572987183169658, 59.96726448433410894, -9.846743663894592657 ) ) ;
#43316 = ORIENTED_EDGE ( 'NONE', *, *, #81721, .F. ) ;
#43317 = CARTESIAN_POINT ( 'NONE',  ( 0.1532563361054100626, 60.80059781766744464, -2.638427012816831230 ) ) ;
#43318 = ORIENTED_EDGE ( 'NONE', *, *, #24899, .F. ) ;
#43319 = EDGE_CURVE ( 'NONE', #68457, #71952, #73436, .T. ) ;
#43320 = CARTESIAN_POINT ( 'NONE',  ( 10.00000000000000178, 64.31368534415483396, 10.88017736071110342 ) ) ;
#43321 = CARTESIAN_POINT ( 'NONE',  ( 2.258855624577643439, 14.95037108984192997, -14.57926203528950637 ) ) ;
#43322 = CARTESIAN_POINT ( 'NONE',  ( 22.81628187352647785, 36.62363466993041783, 6.195893100308588602E-16 ) ) ;
#43324 = CARTESIAN_POINT ( 'NONE',  ( -7.232415441807423129, -88.12698951299773853, -4.000000000000000000 ) ) ;
#43323 = CARTESIAN_POINT ( 'NONE',  ( 10.00000000000000178, 9.313685344154839285, 10.88017736071110342 ) ) ;
#43325 = CARTESIAN_POINT ( 'NONE',  ( 12.63842701281683922, 4.550597817667451750, -9.846743663894590881 ) ) ;
#43326 = CARTESIAN_POINT ( 'NONE',  ( 4.559911319644449179, 23.89701867748817321, 9.422509992056141925 ) ) ;
#43327 = ADVANCED_FACE ( 'NONE', ( #27737 ), #81236, .T. ) ;
#43328 = AXIS2_PLACEMENT_3D ( 'NONE', #29375, #59876, #63803 ) ;
#43329 = EDGE_LOOP ( 'NONE', ( #50725, #54381, #82282, #66982, #9946, #3748 ) ) ;
#43330 = CARTESIAN_POINT ( 'NONE',  ( 19.38216949554541202, 50.99863466993042493, 9.382169495545424454 ) ) ;
#43331 = CARTESIAN_POINT ( 'NONE',  ( 19.42250999205614548, 40.98035201082150536, -5.440088680355545492 ) ) ;
#43332 = LINE ( 'NONE', #90301, #13208 ) ;
#43333 = CARTESIAN_POINT ( 'NONE',  ( 21.09922568453594849, 36.20696800326375353, 6.408140936763242479 ) ) ;
#43334 = CARTESIAN_POINT ( 'NONE',  ( 10.00000000000000000, 41.81368534415484106, -10.88017736071110342 ) ) ;
#43335 = CARTESIAN_POINT ( 'NONE',  ( 10.00000000000000178, 57.25893115100078745, 9.846743663894594434 ) ) ;
#43336 = ORIENTED_EDGE ( 'NONE', *, *, #25222, .T. ) ;
#43337 = CARTESIAN_POINT ( 'NONE',  ( -5.378451019861605786, 0.000000000000000000, 0.9000440264802068713 ) ) ;
#43338 = CARTESIAN_POINT ( 'NONE',  ( 1.472469842513823179, 20.59226448433411960, -4.923371831947296329 ) ) ;
#43339 = CARTESIAN_POINT ( 'NONE',  ( 19.38216949554541557, 12.24863466993041961, -9.382169495545420901 ) ) ;
#43341 = CARTESIAN_POINT ( 'NONE',  ( 7.361572987183169658, 59.96726448433410894, -9.846743663894592657 ) ) ;
#43340 = CARTESIAN_POINT ( 'NONE',  ( 4.862001128006681050, 15.00000000000000000, 13.66056166602463229 ) ) ;
#43342 = CARTESIAN_POINT ( 'NONE',  ( 20.88017736071110875, 20.77201867748816611, -2.915334737309920765 ) ) ;
#43343 = CARTESIAN_POINT ( 'NONE',  ( 10.00000000000000000, 54.75893115100078745, -9.846743663894594434 ) ) ;
#43344 = CARTESIAN_POINT ( 'NONE',  ( -14.42525372082714696, 0.2301507929055852109, 3.890283033989091255 ) ) ;
#43345 = CARTESIAN_POINT ( 'NONE',  ( 0.1532563361054100626, 10.80059781766745175, -2.638427012816831230 ) ) ;
#43347 = ORIENTED_EDGE ( 'NONE', *, *, #54627, .F. ) ;
#43346 = CARTESIAN_POINT ( 'NONE',  ( 2.791683348922240793, 66.63393115100079456, 7.208316651077764092 ) ) ;
#43348 = AXIS2_PLACEMENT_3D ( 'NONE', #80461, #36436, #28914 ) ;
#43349 = CARTESIAN_POINT ( 'NONE',  ( 9.402796353261066997, 14.49999999999999112, 11.68706210897770070 ) ) ;
#43350 = DIRECTION ( 'NONE',  ( 1.000000000000000000, 0.000000000000000000, 0.000000000000000000 ) ) ;
#43351 = EDGE_CURVE ( 'NONE', #40063, #51377, #35737, .T. ) ;
#43352 = CARTESIAN_POINT ( 'NONE',  ( 21.09922568453595559, 42.04030133659708213, -6.408140936763230044 ) ) ;
#43353 = FACE_OUTER_BOUND ( 'NONE', #20768, .T. ) ;
#43354 = CARTESIAN_POINT ( 'NONE',  ( 6.204703633549690345, 62.84541550158063927, 14.16423886937410082 ) ) ;
#43355 = CARTESIAN_POINT ( 'NONE',  ( 12.63842701281683922, 29.55059781766745175, -9.846743663894590881 ) ) ;
#43356 = ADVANCED_FACE ( 'NONE', ( #5745 ), #36235, .F. ) ;
#43357 = CIRCLE ( 'NONE', #17823, 15.00000000000000000 ) ;
#43358 = CARTESIAN_POINT ( 'NONE',  ( 17.39651004071842166, 22.93575266056828355, 6.499999999999998224 ) ) ;
#43359 = CARTESIAN_POINT ( 'NONE',  ( 10.00000000000000178, 53.05374883491396787, 14.16423886937410082 ) ) ;
#43360 = CARTESIAN_POINT ( 'NONE',  ( 15.44008868035555260, 19.73035201082150536, 9.422509992056143702 ) ) ;
#43361 = CARTESIAN_POINT ( 'NONE',  ( 6.204703633549690345, 37.84541550158063927, 14.16423886937410082 ) ) ;
#43363 = DIRECTION ( 'NONE',  ( 3.552713678800501560E-14, 0.000000000000000000, 1.000000000000000000 ) ) ;
#43362 = CARTESIAN_POINT ( 'NONE',  ( 2.917880565312948704, 52.63708216824730357, 12.26659068614894643 ) ) ;
#43364 = CIRCLE ( 'NONE', #16273, 0.2500000000000002220 ) ;
#43365 = CARTESIAN_POINT ( 'NONE',  ( 1.472469842513823179, 10.59226448433411782, -4.923371831947296329 ) ) ;
#43366 = CARTESIAN_POINT ( 'NONE',  ( -1.099225684535947600, -1.293031996736246469, -6.408140936763238038 ) ) ;
#43367 = EDGE_LOOP ( 'NONE', ( #69066, #28640, #38671, #42824 ) ) ;
#43368 = CARTESIAN_POINT ( 'NONE',  ( 12.91533473730992121, 44.52201867748816966, 10.88017736071110164 ) ) ;
#43369 =( NAMED_UNIT ( * ) PLANE_ANGLE_UNIT ( ) SI_UNIT ( $, .RADIAN. ) );
#43370 = LINE ( 'NONE', #43856, #84288 ) ;
#43371 = CARTESIAN_POINT ( 'NONE',  ( 19.84674366389459266, 63.71726448433412315, -2.638427012816827677 ) ) ;
#43372 = CARTESIAN_POINT ( 'NONE',  ( -7.754989057094396010, 84.52548903604051134, 4.000000000000000888 ) ) ;
#43373 = ORIENTED_EDGE ( 'NONE', *, *, #89400, .F. ) ;
#43374 = CARTESIAN_POINT ( 'NONE',  ( 2.917880565312950480, 35.97041550158063217, -12.26659068614894821 ) ) ;
#43375 = ORIENTED_EDGE ( 'NONE', *, *, #94952, .T. ) ;
#43376 = ADVANCED_FACE ( 'NONE', ( #6724 ), #7726, .F. ) ;
#43377 = DIRECTION ( 'NONE',  ( 0.000000000000000000, 0.000000000000000000, 1.000000000000000000 ) ) ;
#43379 = CARTESIAN_POINT ( 'NONE',  ( -11.25000000000000178, 7.713468844518206247, -3.014428414850123250 ) ) ;
#43378 = CARTESIAN_POINT ( 'NONE',  ( -6.822528426060553208, -84.39592987140930802, -2.500000000000000000 ) ) ;
#43380 = CARTESIAN_POINT ( 'NONE',  ( 7.084665262690076126, 14.10535201082150358, 10.88017736071109987 ) ) ;
#43381 = CARTESIAN_POINT ( 'NONE',  ( 0.6178305044545818747, 33.49863466993042493, -9.382169495545419124 ) ) ;
#43382 = CARTESIAN_POINT ( 'NONE',  ( 7.084665262690076126, 7.022018677488169658, -10.88017736071110164 ) ) ;
#43383 = B_SPLINE_CURVE_WITH_KNOTS ( 'NONE', 3,
 ( #30666, #61175, #92171, #38201, #7705, #38683 ),
 .UNSPECIFIED., .F., .F.,
 ( 4, 2, 4 ),
 ( 0.0002800056097769410175, 0.0006862108940652281337, 0.001092416178353515250 ),
 .UNSPECIFIED. ) ;
#43384 = CARTESIAN_POINT ( 'NONE',  ( 13.43411237798105340, 40.58196800326375353, 12.81628187352647963 ) ) ;
#43385 = CARTESIAN_POINT ( 'NONE',  ( 0.000000000000000000, 0.5000000000000004441, 0.000000000000000000 ) ) ;
#43386 = EDGE_LOOP ( 'NONE', ( #41373, #78059, #11803, #32550 ) ) ;
#43387 = CARTESIAN_POINT ( 'NONE',  ( 0.000000000000000000, 14.49999999999999822, 0.000000000000000000 ) ) ;
#43388 = EDGE_CURVE ( 'NONE', #52625, #28728, #91326, .T. ) ;
#43389 = CARTESIAN_POINT ( 'NONE',  ( 12.83294900548063744, 15.00000000000000000, -7.766300266068363101 ) ) ;
#43390 = CARTESIAN_POINT ( 'NONE',  ( 17.08211943468705130, 23.47041550158063572, 12.26659068614894998 ) ) ;
#43391 = FILL_AREA_STYLE_COLOUR ( '', #85387 ) ;
#43392 = CARTESIAN_POINT ( 'NONE',  ( 20.88017736071110875, 20.77201867748816611, -2.915334737309920765 ) ) ;
#43393 = DIRECTION ( 'NONE',  ( 0.000000000000000000, 0.000000000000000000, 1.000000000000000000 ) ) ;
#43394 = DIRECTION ( 'NONE',  ( 0.9588197348681928300, -0.000000000000000000, 0.2840153447039234780 ) ) ;
#43395 = CARTESIAN_POINT ( 'NONE',  ( 15.44008868035555260, 49.73035201082150536, 9.422509992056143702 ) ) ;
#43396 = CARTESIAN_POINT ( 'NONE',  ( 17.96484262340118221, 46.18868534415484106, -7.964842623401177768 ) ) ;
#43397 = CARTESIAN_POINT ( 'NONE',  ( 22.81628187352648496, 11.83196800326375531, -3.434112377981050290 ) ) ;
#43398 = DIRECTION ( 'NONE',  ( -1.000000000000000000, 0.000000000000000000, -0.000000000000000000 ) ) ;
#43399 = CYLINDRICAL_SURFACE ( 'NONE', #67490, 15.00000000000000000 ) ;
#43400 = CARTESIAN_POINT ( 'NONE',  ( 12.63842701281683034, 22.46726448433411605, 9.846743663894596210 ) ) ;
#43401 = DIRECTION ( 'NONE',  ( 0.000000000000000000, -1.000000000000000000, 0.000000000000000000 ) ) ;
#43402 = CARTESIAN_POINT ( 'NONE',  ( 20.88017736071110519, 40.56368534415484106, 2.639326808657452039E-16 ) ) ;
#43403 = VECTOR ( 'NONE', #92742, 1000.000000000000000 ) ;
#43404 = CARTESIAN_POINT ( 'NONE',  ( 13.43411237798106583, 2.665301336597086568, -12.81628187352647252 ) ) ;
#43405 = CARTESIAN_POINT ( 'NONE',  ( 10.00000000000000178, 2.258931151000784787, 9.846743663894594434 ) ) ;
#43406 = CARTESIAN_POINT ( 'NONE',  ( 17.20831665107776587, 29.13393115100078390, -7.208316651077762316 ) ) ;
#43407 = CARTESIAN_POINT ( 'NONE',  ( -1.099225684535947600, 54.54030133659708923, 6.408140936763237150 ) ) ;
#43408 = CARTESIAN_POINT ( 'NONE',  ( 1.472469842513823179, 10.59226448433411782, -4.923371831947296329 ) ) ;
#43409 = VERTEX_POINT ( 'NONE', #67729 ) ;
#43410 = DIRECTION ( 'NONE',  ( -1.000000000000000000, 0.000000000000000000, 0.000000000000000000 ) ) ;
#43411 = CARTESIAN_POINT ( 'NONE',  ( 2.831191079880678085, 79.91181047996344944, -12.00000000000000000 ) ) ;
#43412 = CARTESIAN_POINT ( 'NONE',  ( 20.88017736071110519, 25.56368534415483751, 2.639326808657452039E-16 ) ) ;
#43414 = CARTESIAN_POINT ( 'NONE',  ( -4.164238869374098151, 31.59541550158063927, -3.795296366450310543 ) ) ;
#43413 = FACE_OUTER_BOUND ( 'NONE', #35194, .T. ) ;
#43415 = CARTESIAN_POINT ( 'NONE',  ( 18.52753015748617571, 33.09226448433411605, 4.923371831947298993 ) ) ;
#43416 = CARTESIAN_POINT ( 'NONE',  ( -0.8801773607111009756, 18.06368534415484106, 1.068504757029289695E-15 ) ) ;
#43417 = CARTESIAN_POINT ( 'NONE',  ( 10.00000000000000000, 1.813685344154838175, -10.88017736071110342 ) ) ;
#43418 = ORIENTED_EDGE ( 'NONE', *, *, #30998, .F. ) ;
#43419 = CARTESIAN_POINT ( 'NONE',  ( 15.44008868035555793, 26.39701867748817321, -9.422509992056140149 ) ) ;
#43420 = CARTESIAN_POINT ( 'NONE',  ( 20.88017736071110875, 30.77201867748816966, -2.915334737309920765 ) ) ;
#43422 = CARTESIAN_POINT ( 'NONE',  ( 19.42250999205614548, 40.98035201082150536, -5.440088680355545492 ) ) ;
#43421 = CARTESIAN_POINT ( 'NONE',  ( -13.40508947812159235, 3.877950237245923868E-16, -5.527528931046294502 ) ) ;
#43423 = STYLED_ITEM ( 'NONE', ( #77160 ), #65030 ) ;
#43424 = VERTEX_POINT ( 'NONE', #44217 ) ;
#43425 = CARTESIAN_POINT ( 'NONE',  ( 19.84674366389459621, 58.50893115100078745, 7.409399052514197653E-17 ) ) ;
#43426 = CARTESIAN_POINT ( 'NONE',  ( 2.035157376598824452, 33.68868534415484106, 7.964842623401179544 ) ) ;
#43427 = FILL_AREA_STYLE ('',( #59906 ) ) ;
#43428 = CARTESIAN_POINT ( 'NONE',  ( 10.00000000000000000, 62.87363466993042493, -12.81628187352647608 ) ) ;
#43429 = DIRECTION ( 'NONE',  ( -0.000000000000000000, 1.000000000000000000, 0.000000000000000000 ) ) ;
#43430 = CARTESIAN_POINT ( 'NONE',  ( 2.917880565312950480, 30.97041550158063572, -12.26659068614894821 ) ) ;
#43431 = CARTESIAN_POINT ( 'NONE',  ( 15.44008868035555793, 56.39701867748817676, -9.422509992056140149 ) ) ;
#43432 = CARTESIAN_POINT ( 'NONE',  ( 12.63842701281683922, 64.55059781766745175, -9.846743663894590881 ) ) ;
#43433 = CARTESIAN_POINT ( 'NONE',  ( 8.564643372776551189, 14.49999999999999112, 12.31449893000752915 ) ) ;
#43434 = CARTESIAN_POINT ( 'NONE',  ( 19.84674366389459266, 48.71726448433413026, -2.638427012816827677 ) ) ;
#43435 = EDGE_LOOP ( 'NONE', ( #43186, #76278, #52635, #25501 ) ) ;
#43436 = VECTOR ( 'NONE', #24632, 1000.000000000000000 ) ;
#43437 = CARTESIAN_POINT ( 'NONE',  ( 2.602060718268817574, 0.000000000000000000, 4.792399674598875947 ) ) ;
#43438 = CARTESIAN_POINT ( 'NONE',  ( 0.1532563361054083140, 21.00893115100078745, 1.131784320476157264E-15 ) ) ;
#43439 = CARTESIAN_POINT ( 'NONE',  ( 3.434112377981054287, -12.33469866340291432, -12.81628187352647608 ) ) ;
#43440 = CARTESIAN_POINT ( 'NONE',  ( 7.084665262690076126, 27.02201867748817676, -10.88017736071110164 ) ) ;
#43441 = CARTESIAN_POINT ( 'NONE',  ( 0.1532563361054100626, 20.80059781766744464, -2.638427012816831230 ) ) ;
#43442 = CARTESIAN_POINT ( 'NONE',  ( 10.00000000000000178, 59.31368534415484106, 10.88017736071110342 ) ) ;
#43444 = CARTESIAN_POINT ( 'NONE',  ( 22.81628187352648496, 56.83196800326374643, -3.434112377981050290 ) ) ;
#43443 = CARTESIAN_POINT ( 'NONE',  ( 2.035157376598822676, 27.43868534415483396, -7.964842623401177768 ) ) ;
#43445 = CARTESIAN_POINT ( 'NONE',  ( 24.16423886937410614, 39.51208216824731068, -3.795296366450302550 ) ) ;
#43446 = EDGE_CURVE ( 'NONE', #25266, #60197, #53206, .T. ) ;
#43447 = FACE_OUTER_BOUND ( 'NONE', #48880, .T. ) ;
#43448 = ORIENTED_EDGE ( 'NONE', *, *, #69562, .T. ) ;
#43449 = B_SPLINE_CURVE_WITH_KNOTS ( 'NONE', 3,
 ( #50195, #80209, #72692, #4229, #35187, #12201 ),
 .UNSPECIFIED., .F., .F.,
 ( 4, 2, 4 ),
 ( 0.000000000000000000, 0.0002626113303184867526, 0.0005252226606369735052 ),
 .UNSPECIFIED. ) ;
#43450 = CARTESIAN_POINT ( 'NONE',  ( 0.6178305044545838731, -0.2513653300695798953, 9.382169495545420901 ) ) ;
#43451 = CARTESIAN_POINT ( 'NONE',  ( 7.084665262690076126, 14.10535201082150358, 10.88017736071109987 ) ) ;
#43452 = CARTESIAN_POINT ( 'NONE',  ( 20.88017736071110519, 50.56368534415484106, 2.639326808657452039E-16 ) ) ;
#43453 = CARTESIAN_POINT ( 'NONE',  ( 0.1532563361054100626, 65.80059781766745175, -2.638427012816831230 ) ) ;
#43454 = ORIENTED_EDGE ( 'NONE', *, *, #1268, .F. ) ;
#43455 = CARTESIAN_POINT ( 'NONE',  ( 5.076628168052703671, 11.84226448433411960, 8.527530157486179263 ) ) ;
#43456 = CARTESIAN_POINT ( 'NONE',  ( 0.1532563361054083140, 16.00893115100078390, 1.131784320476157264E-15 ) ) ;
#43457 = CARTESIAN_POINT ( 'NONE',  ( 2.791683348922237240, 40.38393115100078035, -7.208316651077763204 ) ) ;
#43458 = CARTESIAN_POINT ( 'NONE',  ( 10.00000000000000178, 7.258931151000785675, 9.846743663894594434 ) ) ;
#43459 = CARTESIAN_POINT ( 'NONE',  ( 0.1532563361054100626, 10.80059781766745175, -2.638427012816831230 ) ) ;
#43460 = CARTESIAN_POINT ( 'NONE',  ( 0.4195498155886412950, 0.5000000000000000000, -10.00000000000000000 ) ) ;
#43462 = CARTESIAN_POINT ( 'NONE',  ( 0.1922240491738430590, 23.18878173731740588, 6.499999999999968914 ) ) ;
#43461 = CARTESIAN_POINT ( 'NONE',  ( 15.44008868035555260, 64.73035201082151957, 9.422509992056143702 ) ) ;
#43463 = CARTESIAN_POINT ( 'NONE',  ( 0.1532563361054083140, 11.00893115100078568, 1.131784320476157264E-15 ) ) ;
#43465 = ORIENTED_EDGE ( 'NONE', *, *, #4559, .T. ) ;
#43464 = CARTESIAN_POINT ( 'NONE',  ( 0.1532563361054083140, 16.00893115100078390, 1.131784320476157264E-15 ) ) ;
#43466 = AXIS2_PLACEMENT_3D ( 'NONE', #63373, #41881, #34340 ) ;
#43467 = CARTESIAN_POINT ( 'NONE',  ( 2.621477372531582528, 15.00000000000000000, 15.77990027919563154 ) ) ;
#43468 = EDGE_CURVE ( 'NONE', #40449, #38087, #82663, .T. ) ;
#43469 = CARTESIAN_POINT ( 'NONE',  ( 21.09922568453595559, 2.040301336597086568, -6.408140936763230044 ) ) ;
#43470 = SURFACE_STYLE_USAGE ( .BOTH. , #96002 ) ;
#43471 = CARTESIAN_POINT ( 'NONE',  ( 2.917880565312950480, 20.97041550158063217, -12.26659068614894821 ) ) ;
#43472 = ADVANCED_FACE ( 'NONE', ( #15230 ), #91705, .T. ) ;
#43473 = UNCERTAINTY_MEASURE_WITH_UNIT (LENGTH_MEASURE( 1.000000000000000082E-05 ), #33300, 'distance_accuracy_value', 'NONE');
#43474 = CARTESIAN_POINT ( 'NONE',  ( 64.56412365047461321, 28.99999999999999645, 9.500000000000000000 ) ) ;
#43475 = CARTESIAN_POINT ( 'NONE',  ( 17.08211943468705840, 15.13708216824730179, -12.26659068614894466 ) ) ;
#43476 = CARTESIAN_POINT ( 'NONE',  ( 10.00000000000000000, 50.55374883491396787, -14.16423886937410082 ) ) ;
#43477 = CARTESIAN_POINT ( 'NONE',  ( 11.35178980618967337, 0.5000000000000004441, 9.804941009311999522 ) ) ;
#43478 = CARTESIAN_POINT ( 'NONE',  ( 13.79529636645031943, 15.34541550158063750, -14.16423886937409904 ) ) ;
#43479 = CARTESIAN_POINT ( 'NONE',  ( 0.5774900079438607392, 28.48035201082150891, 5.440088680355550821 ) ) ;
#43480 = CARTESIAN_POINT ( 'NONE',  ( 6.829574850499570360, -88.00372650123708240, -3.750000000000000888 ) ) ;
#43481 = VERTEX_POINT ( 'NONE', #8212 ) ;
#43482 = CARTESIAN_POINT ( 'NONE',  ( 0.1532563361054083140, 26.00893115100078745, 1.131784320476157264E-15 ) ) ;
#43484 = CARTESIAN_POINT ( 'NONE',  ( 12.63842701281683922, 29.55059781766745175, -9.846743663894590881 ) ) ;
#43483 = CARTESIAN_POINT ( 'NONE',  ( 5.419894505350582925, 0.5000000000000004441, -13.98659156302458761 ) ) ;
#43485 = CARTESIAN_POINT ( 'NONE',  ( 7.084665262690076126, 7.022018677488170546, -10.88017736071110164 ) ) ;
#43486 = CARTESIAN_POINT ( 'NONE',  ( 19.38216949554541202, 60.99863466993042493, 9.382169495545424454 ) ) ;
#43487 = CARTESIAN_POINT ( 'NONE',  ( 17.20831665107776587, 49.13393115100078745, -7.208316651077762316 ) ) ;
#43488 = DIRECTION ( 'NONE',  ( 0.000000000000000000, 0.000000000000000000, 1.000000000000000000 ) ) ;
#43489 = CARTESIAN_POINT ( 'NONE',  ( -2.816281873526471635, 43.91530133659708923, -3.434112377981056508 ) ) ;
#43490 = CARTESIAN_POINT ( 'NONE',  ( 10.36894250292379027, -21.32125116508603213, 10.36894250292378672 ) ) ;
#43491 =( GEOMETRIC_REPRESENTATION_CONTEXT ( 3 ) GLOBAL_UNCERTAINTY_ASSIGNED_CONTEXT ( ( #39255 ) ) GLOBAL_UNIT_ASSIGNED_CONTEXT ( ( #41171, #3163, #79642 ) ) REPRESENTATION_CONTEXT ( 'NONE', 'WORKASPACE' ) );
#43492 = CARTESIAN_POINT ( 'NONE',  ( 10.00000000000000000, 46.81368534415484106, -10.88017736071110342 ) ) ;
#43493 = CARTESIAN_POINT ( 'NONE',  ( 2.791683348922240793, 41.63393115100078745, 7.208316651077764092 ) ) ;
#43494 = CARTESIAN_POINT ( 'NONE',  ( -2.266590686148945544, 26.38708216824730357, -7.082119434687050408 ) ) ;
#43495 = ORIENTED_EDGE ( 'NONE', *, *, #23853, .T. ) ;
#43496 = CARTESIAN_POINT ( 'NONE',  ( 10.00000000000000178, 3.053748834913967425, 14.16423886937410082 ) ) ;
#43497 = CARTESIAN_POINT ( 'NONE',  ( 20.88017736071110875, 45.77201867748816966, -2.915334737309920765 ) ) ;
#43498 = CARTESIAN_POINT ( 'NONE',  ( 7.084665262690076126, 64.10535201082150536, 10.88017736071109987 ) ) ;
#43499 = CARTESIAN_POINT ( 'NONE',  ( 24.16423886937410614, 44.30374883491397497, 8.672049930838204340E-16 ) ) ;
#43500 = CARTESIAN_POINT ( 'NONE',  ( 21.09922568453595559, 2.040301336597086568, -6.408140936763230044 ) ) ;
#43501 = CIRCLE ( 'NONE', #70644, 2.999999999999997335 ) ;
#43502 = CARTESIAN_POINT ( 'NONE',  ( -0.1503990784575282014, 57.22266099184919597, -6.262539305110077947 ) ) ;
#43503 = CARTESIAN_POINT ( 'NONE',  ( 0.5774900079438607392, 53.48035201082151247, 5.440088680355550821 ) ) ;
#43504 = COLOUR_RGB ( '', 0.09019608, 0.27058824, 0.51372549) ;
#43505 = DIRECTION ( 'NONE',  ( -1.000000000000000000, 0.000000000000000000, -0.000000000000000000 ) ) ;
#43506 = CARTESIAN_POINT ( 'NONE',  ( 22.81628187352648496, 26.83196800326374998, -3.434112377981050290 ) ) ;
#43507 = CARTESIAN_POINT ( 'NONE',  ( 0.1532563361054083140, 56.00893115100078745, 1.131784320476157264E-15 ) ) ;
#43508 = CARTESIAN_POINT ( 'NONE',  ( 7.964842623401181321, 19.93868534415484106, 7.964842623401174215 ) ) ;
#43509 =( NAMED_UNIT ( * ) SI_UNIT ( $, .STERADIAN. ) SOLID_ANGLE_UNIT ( ) );
#43510 = CARTESIAN_POINT ( 'NONE',  ( 20.88017736071110164, 15.35535201082150358, 2.915334737309930979 ) ) ;
#43511 = PLANE ( 'NONE',  #47201 ) ;
#43512 = VERTEX_POINT ( 'NONE', #82220 ) ;
#43513 = EDGE_CURVE ( 'NONE', #42986, #31058, #83215, .T. ) ;
#43514 = CARTESIAN_POINT ( 'NONE',  ( -0.8801773607111008646, 8.272018677488171434, 2.915334737309923430 ) ) ;
#43515 = DIRECTION ( 'NONE',  ( 0.000000000000000000, 0.000000000000000000, -1.000000000000000000 ) ) ;
#43516 = CIRCLE ( 'NONE', #88200, 3.750000000000001776 ) ;
#43517 = CARTESIAN_POINT ( 'NONE',  ( -0.8801773607110991993, 62.85535201082150536, -2.915334737309923874 ) ) ;
#43518 = CARTESIAN_POINT ( 'NONE',  ( 18.52753015748618282, 3.925597817667451306, -4.923371831947291888 ) ) ;
#43519 = CARTESIAN_POINT ( 'NONE',  ( 19.84674366389459621, 38.50893115100078745, 7.409399052514197653E-17 ) ) ;
#43520 = CARTESIAN_POINT ( 'NONE',  ( 20.88017736071110875, 40.77201867748818387, -2.915334737309920765 ) ) ;
#43521 = CARTESIAN_POINT ( 'NONE',  ( 16.40814093676323893, 5.790301336597087456, 11.09922568453595026 ) ) ;
#43523 = CARTESIAN_POINT ( 'NONE',  ( 17.74999999999999645, 91.00000000000000000, 8.000000000000000000 ) ) ;
#43522 = CARTESIAN_POINT ( 'NONE',  ( 20.88017736071110164, 40.35535201082150536, 2.915334737309930979 ) ) ;
#43524 = CARTESIAN_POINT ( 'NONE',  ( 16.40814093676324603, 37.45696800326376064, -11.09922568453594671 ) ) ;
#43525 = ORIENTED_EDGE ( 'NONE', *, *, #68349, .F. ) ;
#43526 = CARTESIAN_POINT ( 'NONE',  ( 15.44008868035555260, 59.73035201082151247, 9.422509992056143702 ) ) ;
#43528 = CARTESIAN_POINT ( 'NONE',  ( -4.164238869374099927, 7.012082168247302683, 3.795296366450308767 ) ) ;
#43527 = CARTESIAN_POINT ( 'NONE',  ( 3.591859063236763294, 28.29030133659708568, -11.09922568453595026 ) ) ;
#43529 = CARTESIAN_POINT ( 'NONE',  ( 5.076628168052704559, 0.1755978176674514724, -8.527530157486179263 ) ) ;
#43530 = CARTESIAN_POINT ( 'NONE',  ( 12.91533473730993009, 41.60535201082149825, -10.88017736071109987 ) ) ;
#43531 = CARTESIAN_POINT ( 'NONE',  ( -6.000000000000009770, 41.24999999999999289, -6.250000000000000000 ) ) ;
#43532 = CARTESIAN_POINT ( 'NONE',  ( 24.16423886937410614, 59.30374883491397497, 8.672049930838204340E-16 ) ) ;
#43533 = PRESENTATION_LAYER_ASSIGNMENT (  '', '', ( #29182 ) ) ;
#43534 = CARTESIAN_POINT ( 'NONE',  ( 18.52753015748617571, 58.09226448433411605, 4.923371831947298993 ) ) ;
#43535 = CARTESIAN_POINT ( 'NONE',  ( 0.1532563361054082862, 11.21726448433411605, 2.638427012816831674 ) ) ;
#43536 = CARTESIAN_POINT ( 'NONE',  ( 20.88017736071110164, 60.35535201082151957, 2.915334737309930979 ) ) ;
#43537 = CARTESIAN_POINT ( 'NONE',  ( 0.1957200283969147692, 5.257339608395445119, 6.500000000000001776 ) ) ;
#43538 = CARTESIAN_POINT ( 'NONE',  ( 20.36894250292379738, 29.92874883491396432, -10.36894250292379027 ) ) ;
#43539 = CARTESIAN_POINT ( 'NONE',  ( -3.836050625226794963, -2.701282487336928106, -4.000000000000000000 ) ) ;
#43540 = ORIENTED_EDGE ( 'NONE', *, *, #77203, .T. ) ;
#43541 = COLOUR_RGB ( '', 0.40784314, 0.44705882, 0.49803922) ;
#43542 = CARTESIAN_POINT ( 'NONE',  ( 2.917880565312950480, 60.97041550158063927, -12.26659068614894821 ) ) ;
#43543 = CARTESIAN_POINT ( 'NONE',  ( 2.917880565312948704, 62.63708216824730357, 12.26659068614894643 ) ) ;
#43544 = CARTESIAN_POINT ( 'NONE',  ( 18.52753015748617571, 33.09226448433411605, 4.923371831947298993 ) ) ;
#43545 = CARTESIAN_POINT ( 'NONE',  ( 0.6178305044545818747, 28.49863466993041783, -9.382169495545419124 ) ) ;
#43546 = CARTESIAN_POINT ( 'NONE',  ( -45.94000000000001194, 107.5383484153110061, -12.00000000000000000 ) ) ;
#43547 = CARTESIAN_POINT ( 'NONE',  ( -23.44000000000001194, 92.00000000000000000, -10.09898361729590199 ) ) ;
#43548 = CARTESIAN_POINT ( 'NONE',  ( 2.035157376598822676, 17.43868534415483751, -7.964842623401177768 ) ) ;
#43549 = CARTESIAN_POINT ( 'NONE',  ( 6.204703633549690345, 60.76208216824730357, -14.16423886937410259 ) ) ;
#43550 = CARTESIAN_POINT ( 'NONE',  ( 12.63842701281683034, 32.46726448433412315, 9.846743663894596210 ) ) ;
#43551 = CARTESIAN_POINT ( 'NONE',  ( 12.25993886608609351, 14.49999999999999112, -8.642563219313673883 ) ) ;
#43552 = CARTESIAN_POINT ( 'NONE',  ( 18.52753015748618282, 13.92559781766745175, -4.923371831947291888 ) ) ;
#43553 = CARTESIAN_POINT ( 'NONE',  ( -4.923371831947292776, 21.84226448433413026, 8.527530157486181039 ) ) ;
#43554 = ORIENTED_EDGE ( 'NONE', *, *, #65705, .F. ) ;
#43555 = EDGE_LOOP ( 'NONE', ( #83298, #41605, #22842 ) ) ;
#43556 = ORIENTED_EDGE ( 'NONE', *, *, #59631, .T. ) ;
#43557 = CARTESIAN_POINT ( 'NONE',  ( 7.361572987183170547, 42.05059781766745886, 9.846743663894590881 ) ) ;
#43559 = CARTESIAN_POINT ( 'NONE',  ( -0.8801773607111009756, 23.06368534415484106, 1.068504757029289695E-15 ) ) ;
#43558 = CARTESIAN_POINT ( 'NONE',  ( 15.44008868035555260, 24.73035201082150891, 9.422509992056143702 ) ) ;
#43561 = CARTESIAN_POINT ( 'NONE',  ( 3.591859063236763294, 13.29030133659708746, -11.09922568453595026 ) ) ;
#43560 = CARTESIAN_POINT ( 'NONE',  ( 17.20831665107776587, 59.13393115100078745, -7.208316651077762316 ) ) ;
#43562 = CARTESIAN_POINT ( 'NONE',  ( -0.3689425029237881626, 7.428748834913967869, 10.36894250292379027 ) ) ;
#43563 = CARTESIAN_POINT ( 'NONE',  ( -3.499999999999998668, 1.019547802438465434, 3.750000000000000000 ) ) ;
#43564 = ADVANCED_FACE ( 'NONE', ( #60214 ), #39567, .T. ) ;
#43565 = AXIS2_PLACEMENT_3D ( 'NONE', #49305, #96306, #58268 ) ;
#43566 = CARTESIAN_POINT ( 'NONE',  ( 0.6178305044545838731, 29.74863466993042138, 9.382169495545420901 ) ) ;
#43567 = ORIENTED_EDGE ( 'NONE', *, *, #64664, .T. ) ;
#43568 = STYLED_ITEM ( 'NONE', ( #85660 ), #25021 ) ;
#43569 = CARTESIAN_POINT ( 'NONE',  ( 5.076628168052704559, 30.17559781766745175, -8.527530157486179263 ) ) ;
#43570 = AXIS2_PLACEMENT_3D ( 'NONE', #70437, #78912, #86903 ) ;
#43571 = CARTESIAN_POINT ( 'NONE',  ( 20.88017736071110164, 5.355352010821503583, 2.915334737309930979 ) ) ;
#43572 = VERTEX_POINT ( 'NONE', #6233 ) ;
#43573 = PRESENTATION_LAYER_ASSIGNMENT (  '', '', ( #86700 ) ) ;
#43574 = CARTESIAN_POINT ( 'NONE',  ( 4.559911319644449179, 7.230352010821505360, -9.422509992056141925 ) ) ;
#43575 = ORIENTED_EDGE ( 'NONE', *, *, #70369, .T. ) ;
#43576 = CARTESIAN_POINT ( 'NONE',  ( 0.5774900079438590739, 52.64701867748817676, -5.440088680355550821 ) ) ;
#43577 = CARTESIAN_POINT ( 'NONE',  ( 10.00000000000000178, 49.31368534415484106, 10.88017736071110342 ) ) ;
#43578 = CARTESIAN_POINT ( 'NONE',  ( 17.96484262340118221, 51.18868534415483396, -7.964842623401177768 ) ) ;
#43579 = VECTOR ( 'NONE', #73342, 1000.000000000000000 ) ;
#43580 = ADVANCED_FACE ( 'NONE', ( #75213 ), #69900, .T. ) ;
#43581 = DIRECTION ( 'NONE',  ( 0.9799247046208295897, 0.000000000000000000, -0.1993679344171971901 ) ) ;
#43582 = CARTESIAN_POINT ( 'NONE',  ( 10.00000000000000000, 41.81368534415484106, -10.88017736071110342 ) ) ;
#43583 = CARTESIAN_POINT ( 'NONE',  ( -5.073789285385991832, 0.000000000000000000, 1.998618750576336867 ) ) ;
#43585 = VERTEX_POINT ( 'NONE', #22233 ) ;
#43584 = CARTESIAN_POINT ( 'NONE',  ( 10.19513985507827236, 14.63606907090794351, 11.00268709613227891 ) ) ;
#43586 = EDGE_CURVE ( 'NONE', #49831, #24464, #22014, .T. ) ;
#43587 = CARTESIAN_POINT ( 'NONE',  ( 14.92337183194729988, 34.34226448433411605, -8.527530157486177487 ) ) ;
#43588 = ORIENTED_EDGE ( 'NONE', *, *, #22580, .F. ) ;
#43589 = CARTESIAN_POINT ( 'NONE',  ( 7.361572987183169658, 54.96726448433413026, -9.846743663894592657 ) ) ;
#43590 = DIRECTION ( 'NONE',  ( 0.000000000000000000, -1.000000000000000000, 0.000000000000000000 ) ) ;
#43591 = ADVANCED_FACE ( 'NONE', ( #7225 ), #68230, .F. ) ;
#43592 = VECTOR ( 'NONE', #11831, 1000.000000000000000 ) ;
#43593 = CARTESIAN_POINT ( 'NONE',  ( -0.3689425029237898834, 11.17874883491396787, -10.36894250292378850 ) ) ;
#43594 = ORIENTED_EDGE ( 'NONE', *, *, #52040, .F. ) ;
#43595 = CARTESIAN_POINT ( 'NONE',  ( -11.36476366739559651, 12.94173722837749452, 2.760244389056020431 ) ) ;
#43596 = CARTESIAN_POINT ( 'NONE',  ( -3.500000492100954652, 0.08994223334896143951, 3.750000000000000444 ) ) ;
#43597 =( NAMED_UNIT ( * ) SI_UNIT ( $, .STERADIAN. ) SOLID_ANGLE_UNIT ( ) );
#43598 = CARTESIAN_POINT ( 'NONE',  ( 17.08211943468705840, 60.13708216824729647, -12.26659068614894466 ) ) ;
#43599 = DIRECTION ( 'NONE',  ( -0.000000000000000000, -0.000000000000000000, -1.000000000000000000 ) ) ;
#43600 = VERTEX_POINT ( 'NONE', #45710 ) ;
#43601 = DIRECTION ( 'NONE',  ( 0.000000000000000000, 1.000000000000000000, 0.000000000000000000 ) ) ;
#43602 = CARTESIAN_POINT ( 'NONE',  ( 2.791683348922237240, 50.38393115100078035, -7.208316651077763204 ) ) ;
#43603 = DIRECTION ( 'NONE',  ( 0.6225146366376079765, 0.000000000000000000, 0.7826081568524232424 ) ) ;
#43605 = AXIS2_PLACEMENT_3D ( 'NONE', #24708, #92696, #56187 ) ;
#43604 = CARTESIAN_POINT ( 'NONE',  ( -2.816281873526471635, 18.91530133659708213, -3.434112377981056508 ) ) ;
#43606 = CARTESIAN_POINT ( 'NONE',  ( 2.791683348922237240, 5.383931151000785675, -7.208316651077763204 ) ) ;
#43607 = FACE_OUTER_BOUND ( 'NONE', #4346, .T. ) ;
#43608 = CARTESIAN_POINT ( 'NONE',  ( 18.52753015748618282, 13.92559781766745175, -4.923371831947291888 ) ) ;
#43609 = CARTESIAN_POINT ( 'NONE',  ( 7.361572987183170547, 67.05059781766746596, 9.846743663894590881 ) ) ;
#43610 = DIRECTION ( 'NONE',  ( 1.776356839400250465E-15, 0.000000000000000000, 1.000000000000000000 ) ) ;
#43611 = AXIS2_PLACEMENT_3D ( 'NONE', #79872, #47892, #71406 ) ;
#43612 = ORIENTED_EDGE ( 'NONE', *, *, #3881, .T. ) ;
#43613 = CARTESIAN_POINT ( 'NONE',  ( 10.00000000000000178, 14.31368534415483929, 10.88017736071110342 ) ) ;
#43614 = CARTESIAN_POINT ( 'NONE',  ( -4.164238869374099039, 1.803748834913967647, 8.674139862899312516E-16 ) ) ;
#43615 = CARTESIAN_POINT ( 'NONE',  ( 7.361572987183170547, 22.05059781766745530, 9.846743663894590881 ) ) ;
#43616 = CARTESIAN_POINT ( 'NONE',  ( 0.5774900079438607392, 58.48035201082151247, 5.440088680355550821 ) ) ;
#43618 = CARTESIAN_POINT ( 'NONE',  ( -3.500000000000000444, -0.04521315095527938394, -2.750000000000000444 ) ) ;
#43617 = CARTESIAN_POINT ( 'NONE',  ( -1.099225684535947600, 23.70696800326375708, -6.408140936763238038 ) ) ;
#43619 = CARTESIAN_POINT ( 'NONE',  ( 11.48952521350015488, 15.00000000000000000, 8.845383562533813304 ) ) ;
#43620 = CARTESIAN_POINT ( 'NONE',  ( 69.60148758828984228, 0.4999999999999982792, 10.00000000000000000 ) ) ;
#43621 = CARTESIAN_POINT ( 'NONE',  ( -4.250000000000000000, 78.07179676972445748, -6.250000000000000000 ) ) ;
#43622 = CARTESIAN_POINT ( 'NONE',  ( 6.565887622018943937, 3.081968003263753531, -12.81628187352647608 ) ) ;
#43623 = CARTESIAN_POINT ( 'NONE',  ( 14.92337183194729633, 62.67559781766745886, 8.527530157486181039 ) ) ;
#43624 = CARTESIAN_POINT ( 'NONE',  ( 14.92337183194729633, 7.675597817667451750, 8.527530157486181039 ) ) ;
#43625 = CARTESIAN_POINT ( 'NONE',  ( 9.422509992056141925, -24.01964798917849109, -5.440088680355554374 ) ) ;
#43626 = CARTESIAN_POINT ( 'NONE',  ( 16.40814093676323893, 15.79030133659708746, 11.09922568453595026 ) ) ;
#43627 = CARTESIAN_POINT ( 'NONE',  ( -11.07532115276637086, -96.02567358741556802, -3.750000000000000000 ) ) ;
#43629 = CARTESIAN_POINT ( 'NONE',  ( 10.84451454130498149, 15.00000000000000000, 9.625305416630897781 ) ) ;
#43628 = CARTESIAN_POINT ( 'NONE',  ( 10.00000000000000178, 34.31368534415484106, 10.88017736071110342 ) ) ;
#43630 = CARTESIAN_POINT ( 'NONE',  ( 17.39651004071842522, 24.08210964143329491, -6.499999999999992895 ) ) ;
#43631 = EDGE_CURVE ( 'NONE', #84722, #21240, #98639, .T. ) ;
#43632 =( LENGTH_UNIT ( ) NAMED_UNIT ( * ) SI_UNIT ( .MILLI., .METRE. ) );
#43633 = CARTESIAN_POINT ( 'NONE',  ( 4.559911319644449179, 23.89701867748817321, 9.422509992056141925 ) ) ;
#43634 = CARTESIAN_POINT ( 'NONE',  ( 0.1532563361054083140, 46.00893115100079456, 1.131784320476157264E-15 ) ) ;
#43635 = CARTESIAN_POINT ( 'NONE',  ( 7.084665262690076126, 57.02201867748817676, -10.88017736071110164 ) ) ;
#43636 = CARTESIAN_POINT ( 'NONE',  ( -2.266590686148945544, 37.22041550158063217, 7.082119434687048631 ) ) ;
#43637 = CARTESIAN_POINT ( 'NONE',  ( 64.56412365047461321, 11.99999999999999467, 10.00000000000000000 ) ) ;
#43638 = VECTOR ( 'NONE', #3642, 1000.000000000000000 ) ;
#43639 = CARTESIAN_POINT ( 'NONE',  ( 0.1532563361054100626, 40.80059781766745886, -2.638427012816831230 ) ) ;
#43640 = CARTESIAN_POINT ( 'NONE',  ( 0.1532563361054100626, 65.80059781766745175, -2.638427012816831230 ) ) ;
#43641 = ORIENTED_EDGE ( 'NONE', *, *, #2869, .T. ) ;
#43642 = CARTESIAN_POINT ( 'NONE',  ( 10.00000000000000178, 29.31368534415483751, 10.88017736071110342 ) ) ;
#43643 =( GEOMETRIC_REPRESENTATION_CONTEXT ( 3 ) GLOBAL_UNCERTAINTY_ASSIGNED_CONTEXT ( ( #30437 ) ) GLOBAL_UNIT_ASSIGNED_CONTEXT ( ( #9479, #24996, #63460 ) ) REPRESENTATION_CONTEXT ( 'NONE', 'WORKASPACE' ) );
#43644 = EDGE_CURVE ( 'NONE', #42998, #55876, #47533, .T. ) ;
#43645 = CARTESIAN_POINT ( 'NONE',  ( 12.91533473730993009, 6.605352010821504471, -10.88017736071109987 ) ) ;
#43646 = CARTESIAN_POINT ( 'NONE',  ( 15.44008868035555793, 11.39701867748817143, -9.422509992056140149 ) ) ;
#43647 = CARTESIAN_POINT ( 'NONE',  ( 20.88017736071110875, 65.77201867748817676, -2.915334737309920765 ) ) ;
#43648 = CARTESIAN_POINT ( 'NONE',  ( 20.36894250292379738, 29.92874883491396432, -10.36894250292379027 ) ) ;
#43649 = CARTESIAN_POINT ( 'NONE',  ( 19.84674366389459621, 13.50893115100078568, 7.409399052514197653E-17 ) ) ;
#43650 = CARTESIAN_POINT ( 'NONE',  ( -14.24131928502211863, 0.000000000000000000, 0.4973178280104966764 ) ) ;
#43651 = CARTESIAN_POINT ( 'NONE',  ( 20.88017736071110875, 30.77201867748816966, -2.915334737309920765 ) ) ;
#43652 = AXIS2_PLACEMENT_3D ( 'NONE', #43531, #6526, #75021 ) ;
#43653 = CARTESIAN_POINT ( 'NONE',  ( 17.39651004071838969, 39.08210964143329846, -6.500000000000027534 ) ) ;
#43654 = CARTESIAN_POINT ( 'NONE',  ( 19.10478245763047056, 26.02576239577082262, -5.990408912944402253 ) ) ;
#43655 = VERTEX_POINT ( 'NONE', #77180 ) ;
#43656 = CARTESIAN_POINT ( 'NONE',  ( 4.129999999999999893, 0.09092508111800794157, 2.499999999999999112 ) ) ;
#43657 = CARTESIAN_POINT ( 'NONE',  ( 2.791683348922237240, 45.38393115100079456, -7.208316651077763204 ) ) ;
#43658 = VERTEX_POINT ( 'NONE', #85676 ) ;
#43659 = ORIENTED_EDGE ( 'NONE', *, *, #14598, .T. ) ;
#43660 = FILL_AREA_STYLE ('',( #97680 ) ) ;
#43661 = CARTESIAN_POINT ( 'NONE',  ( 17.08211943468705840, 20.13708216824730357, -12.26659068614894466 ) ) ;
#43662 = CARTESIAN_POINT ( 'NONE',  ( 22.26659068614894466, 8.887082168247300018, 7.082119434687054849 ) ) ;
#43663 = CARTESIAN_POINT ( 'NONE',  ( 12.91533473730992121, 54.52201867748816255, 10.88017736071110164 ) ) ;
#43664 = CARTESIAN_POINT ( 'NONE',  ( 6.204703633549690345, 50.76208216824730357, -14.16423886937410259 ) ) ;
#43665 = CARTESIAN_POINT ( 'NONE',  ( 0.1532563361054100626, 65.80059781766745175, -2.638427012816831230 ) ) ;
#43666 = CARTESIAN_POINT ( 'NONE',  ( 7.361572987183169658, 44.96726448433412315, -9.846743663894592657 ) ) ;
#43668 = CARTESIAN_POINT ( 'NONE',  ( 22.81628187352648496, 1.831968003263753753, -3.434112377981050290 ) ) ;
#43667 = CARTESIAN_POINT ( 'NONE',  ( 2.035157376598822676, 47.43868534415484817, -7.964842623401177768 ) ) ;
#43669 = CARTESIAN_POINT ( 'NONE',  ( -0.3689425029237881626, 22.42874883491397142, 10.36894250292379027 ) ) ;
#43670 = CARTESIAN_POINT ( 'NONE',  ( 20.36894250292379738, 49.92874883491396787, -10.36894250292379027 ) ) ;
#43671 = CARTESIAN_POINT ( 'NONE',  ( 17.96484262340118221, 24.93868534415484461, 7.964842623401181321 ) ) ;
#43672 = CARTESIAN_POINT ( 'NONE',  ( 19.72487221294570858, 4.782175860852374782, 6.500000000000002665 ) ) ;
#43673 = CARTESIAN_POINT ( 'NONE',  ( 19.42250999205614548, 45.98035201082150536, -5.440088680355545492 ) ) ;
#43674 = CARTESIAN_POINT ( 'NONE',  ( 8.527530157486175710, -31.07440218233254470, -4.923371831947298993 ) ) ;
#43675 = ORIENTED_EDGE ( 'NONE', *, *, #80278, .F. ) ;
#43676 = CARTESIAN_POINT ( 'NONE',  ( 13.61464873478166204, 0.3639308181217354443, 6.296136897217934347 ) ) ;
#43677 = VERTEX_POINT ( 'NONE', #46685 ) ;
#43678 = EDGE_LOOP ( 'NONE', ( #61568, #95626, #89706, #16610 ) ) ;
#43679 = CARTESIAN_POINT ( 'NONE',  ( 10.00000000000000000, 45.55374883491397497, -14.16423886937410082 ) ) ;
#43680 = CARTESIAN_POINT ( 'NONE',  ( 17.20831665107776587, 44.13393115100078745, -7.208316651077762316 ) ) ;
#43681 = CARTESIAN_POINT ( 'NONE',  ( 20.88017736071110164, 65.35535201082150536, 2.915334737309930979 ) ) ;
#43682 = AXIS2_PLACEMENT_3D ( 'NONE', #38240, #83234, #97771 ) ;
#43683 = DIRECTION ( 'NONE',  ( -0.000000000000000000, -1.000000000000000000, -0.000000000000000000 ) ) ;
#43684 = EDGE_CURVE ( 'NONE', #53272, #36801, #75931, .T. ) ;
#43685 = CARTESIAN_POINT ( 'NONE',  ( 4.559911319644449179, 52.23035201082151247, -9.422509992056141925 ) ) ;
#43686 = EDGE_CURVE ( 'NONE', #24464, #3878, #79459, .T. ) ;
#43687 = CARTESIAN_POINT ( 'NONE',  ( 6.565887622018943937, 55.16530133659709634, 12.81628187352647430 ) ) ;
#43688 = CARTESIAN_POINT ( 'NONE',  ( 9.382169495545419124, 10.99863466993041783, 9.382169495545417348 ) ) ;
#43689 = ORIENTED_EDGE ( 'NONE', *, *, #24868, .F. ) ;
#43690 = CARTESIAN_POINT ( 'NONE',  ( 20.36894250292379382, 23.67874883491397142, 10.36894250292379205 ) ) ;
#43691 = B_SPLINE_CURVE_WITH_KNOTS ( 'NONE', 3,
 ( #67349, #51359, #44341, #60823 ),
 .UNSPECIFIED., .F., .F.,
 ( 4, 4 ),
 ( 1.242751103718668000E-16, 0.001060528352561993307 ),
 .UNSPECIFIED. ) ;
#43692 = CARTESIAN_POINT ( 'NONE',  ( 22.81628187352648496, 21.83196800326374643, -3.434112377981050290 ) ) ;
#43693 = ORIENTED_EDGE ( 'NONE', *, *, #35087, .F. ) ;
#43694 = CARTESIAN_POINT ( 'NONE',  ( -1.099225684535947600, 44.54030133659708923, 6.408140936763237150 ) ) ;
#43695 = CARTESIAN_POINT ( 'NONE',  ( 0.5774900079438607392, 18.48035201082150536, 5.440088680355550821 ) ) ;
#43696 = CARTESIAN_POINT ( 'NONE',  ( 19.84674366389459266, 43.30059781766744464, 2.638427012816836559 ) ) ;
#43697 = CARTESIAN_POINT ( 'NONE',  ( 15.44008868035555260, 14.73035201082150536, 9.422509992056143702 ) ) ;
#43698 = CARTESIAN_POINT ( 'NONE',  ( -2.816281873526473856, 49.33196800326374643, 3.434112377981055619 ) ) ;
#43699 = ADVANCED_FACE ( 'NONE', ( #92672 ), #71172, .T. ) ;
#43700 = LINE ( 'NONE', #21711, #79923 ) ;
#43701 = CARTESIAN_POINT ( 'NONE',  ( 12.63842701281683922, 44.55059781766745175, -9.846743663894590881 ) ) ;
#43703 = ORIENTED_EDGE ( 'NONE', *, *, #67149, .T. ) ;
#43702 = DIRECTION ( 'NONE',  ( -0.08715574274766037244, -0.9961946980917453232, -0.000000000000000000 ) ) ;
#43704 = DIRECTION ( 'NONE',  ( 1.000000000000000000, -5.818595309480553908E-17, 0.000000000000000000 ) ) ;
#43705 = VECTOR ( 'NONE', #1276, 1000.000000000000000 ) ;
#43706 = CARTESIAN_POINT ( 'NONE',  ( 14.24131928502211686, 15.00000000000000000, -0.4973178280105898241 ) ) ;
#43707 = CARTESIAN_POINT ( 'NONE',  ( -9.402796353260967521, 0.3640475087720753677, -11.68706210897770426 ) ) ;
#43708 = CARTESIAN_POINT ( 'NONE',  ( 14.92337183194729633, 17.67559781766745175, 8.527530157486181039 ) ) ;
#43709 = CARTESIAN_POINT ( 'NONE',  ( 6.565887622018943937, 28.08196800326375353, -12.81628187352647608 ) ) ;
#43710 = EDGE_CURVE ( 'NONE', #30649, #22949, #66172, .T. ) ;
#43712 = CARTESIAN_POINT ( 'NONE',  ( 0.2751277870542911952, 38.21833443783937412, 6.499999999999992006 ) ) ;
#43711 = VECTOR ( 'NONE', #81126, 1000.000000000000000 ) ;
#43713 = B_SPLINE_CURVE_WITH_KNOTS ( 'NONE', 3,
 ( #93693, #55707, #86203, #17715, #10209, #86694, #20652, #42183, #11671, #28145 ),
 .UNSPECIFIED., .F., .F.,
 ( 4, 3, 3, 4 ),
 ( 1.551583845779545699E-17, 0.0006253016069560773937, 0.001250604074564914785, 0.002501455912506532226 ),
 .UNSPECIFIED. ) ;
#43714 = VERTEX_POINT ( 'NONE', #78169 ) ;
#43715 = CARTESIAN_POINT ( 'NONE',  ( 1.472469842513823179, 61.42559781766745175, 4.923371831947296329 ) ) ;
#43716 = CARTESIAN_POINT ( 'NONE',  ( -4.873787042390612001, 15.00000000000000000, -13.39061984619925916 ) ) ;
#43717 = CARTESIAN_POINT ( 'NONE',  ( 24.16423886937409904, 24.09541550158063927, 3.795296366450317205 ) ) ;
#43718 = CARTESIAN_POINT ( 'NONE',  ( 10.00000000000000178, 47.25893115100078745, 9.846743663894594434 ) ) ;
#43719 = CARTESIAN_POINT ( 'NONE',  ( 22.81628187352647785, 41.62363466993042493, 6.195893100308588602E-16 ) ) ;
#43721 = CARTESIAN_POINT ( 'NONE',  ( -1.829604203029787435, -0.03417435944610275333, 15.89119079541584334 ) ) ;
#43720 = CARTESIAN_POINT ( 'NONE',  ( 21.92686044187657046, 37.39664270246084499, -3.195792623639524432 ) ) ;
#43722 = CARTESIAN_POINT ( 'NONE',  ( 4.559911319644449179, 63.89701867748817676, 9.422509992056141925 ) ) ;
#43723 = CARTESIAN_POINT ( 'NONE',  ( 6.579634127946650146, -87.99828267815715321, -2.750000000000000000 ) ) ;
#43724 = CARTESIAN_POINT ( 'NONE',  ( 17.20831665107776587, 29.13393115100078390, -7.208316651077762316 ) ) ;
#43725 = CARTESIAN_POINT ( 'NONE',  ( 19.42250999205614548, 35.98035201082151247, -5.440088680355545492 ) ) ;
#43726 = CARTESIAN_POINT ( 'NONE',  ( 19.84674366389459266, 33.30059781766744464, 2.638427012816836559 ) ) ;
#43727 = APPLICATION_PROTOCOL_DEFINITION ( 'draft international standard', 'automotive_design', 1998, #6554 ) ;
#43728 = CARTESIAN_POINT ( 'NONE',  ( 2.831191079880678085, 79.91181047996344944, 5.000000000000000000 ) ) ;
#43729 = CARTESIAN_POINT ( 'NONE',  ( 4.559911319644449179, 48.89701867748817676, 9.422509992056141925 ) ) ;
#43730 = ORIENTED_EDGE ( 'NONE', *, *, #31652, .F. ) ;
#43731 = CARTESIAN_POINT ( 'NONE',  ( -11.25000000000000178, 5.118033628982653127, 3.674383000693412496E-15 ) ) ;
#43732 = CARTESIAN_POINT ( 'NONE',  ( 17.96484262340118221, 16.18868534415483396, -7.964842623401177768 ) ) ;
#43734 = CARTESIAN_POINT ( 'NONE',  ( 20.88017736071110875, 40.77201867748818387, -2.915334737309920765 ) ) ;
#43733 = CARTESIAN_POINT ( 'NONE',  ( 5.076628168052703671, 56.84226448433412315, 8.527530157486179263 ) ) ;
#43735 = CARTESIAN_POINT ( 'NONE',  ( 20.88017736071110519, 65.56368534415483396, 2.639326808657452039E-16 ) ) ;
#43737 = CARTESIAN_POINT ( 'NONE',  ( -2.913501739333854701, 4.099883984707052505E-16, 14.20427779279533098 ) ) ;
#43736 = CARTESIAN_POINT ( 'NONE',  ( 15.44008868035555793, 31.39701867748817676, -9.422509992056140149 ) ) ;
#43738 = CARTESIAN_POINT ( 'NONE',  ( 19.84674366389459266, 3.300597817667451750, 2.638427012816836559 ) ) ;
#43739 = CARTESIAN_POINT ( 'NONE',  ( 0.1532563361054082862, 26.21726448433411605, 2.638427012816831674 ) ) ;
#43740 = DIRECTION ( 'NONE',  ( 1.000000000000000000, 0.000000000000000000, 0.000000000000000000 ) ) ;
#43741 = CARTESIAN_POINT ( 'NONE',  ( -7.082119434687044190, 2.637082168247310676, 12.26659068614894998 ) ) ;
#43742 = CARTESIAN_POINT ( 'NONE',  ( 19.84674366389459266, 53.71726448433411605, -2.638427012816827677 ) ) ;
#43744 = CARTESIAN_POINT ( 'NONE',  ( 0.000000000000000000, 10.25000000000000000, 2.750000000000000000 ) ) ;
#43743 = CARTESIAN_POINT ( 'NONE',  ( 13.79529636645030344, 58.26208216824728936, 14.16423886937410614 ) ) ;
#43745 = CARTESIAN_POINT ( 'NONE',  ( 1.932340009482124588, 61.49127512925447547, -6.499999999999922728 ) ) ;
#43746 = CARTESIAN_POINT ( 'NONE',  ( 22.26659068614894466, 8.887082168247300018, 7.082119434687054849 ) ) ;
#43747 = EDGE_CURVE ( 'NONE', #89307, #39417, #54307, .T. ) ;
#43748 = CARTESIAN_POINT ( 'NONE',  ( -2.266590686148945544, 41.38708216824729647, -7.082119434687050408 ) ) ;
#43749 = CARTESIAN_POINT ( 'NONE',  ( -2.816281873526471635, -1.084698663402913210, -3.434112377981056508 ) ) ;
#43750 = ORIENTED_EDGE ( 'NONE', *, *, #66277, .T. ) ;
#43751 = CARTESIAN_POINT ( 'NONE',  ( 7.084665262690076126, 12.02201867748817321, -10.88017736071110164 ) ) ;
#43752 = CARTESIAN_POINT ( 'NONE',  ( 1.472469842513823179, 50.59226448433411605, -4.923371831947296329 ) ) ;
#43754 = CARTESIAN_POINT ( 'NONE',  ( 17.75000000000001776, 4.561680251642722724E-15, 4.000000000000000000 ) ) ;
#43753 = DIRECTION ( 'NONE',  ( -0.000000000000000000, -1.000000000000000000, -0.000000000000000000 ) ) ;
#43755 = DIRECTION ( 'NONE',  ( 1.000000000000000000, 0.000000000000000000, 0.000000000000000000 ) ) ;
#43756 = CARTESIAN_POINT ( 'NONE',  ( -2.816281873526471635, 28.91530133659708213, -3.434112377981056508 ) ) ;
#43757 = CARTESIAN_POINT ( 'NONE',  ( 17.20831665107776587, 24.13393115100078035, -7.208316651077762316 ) ) ;
#43758 = ORIENTED_EDGE ( 'NONE', *, *, #14272, .T. ) ;
#43759 = CARTESIAN_POINT ( 'NONE',  ( 19.84674366389459266, 3.717264484334118713, -2.638427012816827677 ) ) ;
#43760 = CARTESIAN_POINT ( 'NONE',  ( 18.39792806157249672, 4.522241923386406626, 6.500000000000004441 ) ) ;
#43761 = CARTESIAN_POINT ( 'NONE',  ( -14.42956166534410656, 14.99999999999807443, 2.386684097923415404 ) ) ;
#43762 = CARTESIAN_POINT ( 'NONE',  ( 4.559911319644449179, 13.89701867748817143, 9.422509992056141925 ) ) ;
#43763 = CARTESIAN_POINT ( 'NONE',  ( -4.164238869374099039, 41.80374883491397497, 8.674139862899312516E-16 ) ) ;
#43764 = CARTESIAN_POINT ( 'NONE',  ( 0.5774900079438590739, 42.64701867748816966, -5.440088680355550821 ) ) ;
#43765 = CARTESIAN_POINT ( 'NONE',  ( 2.035157376598822676, 57.43868534415484106, -7.964842623401177768 ) ) ;
#43766 = CARTESIAN_POINT ( 'NONE',  ( 7.361572987183170547, 22.05059781766745530, 9.846743663894590881 ) ) ;
#43767 = CARTESIAN_POINT ( 'NONE',  ( 19.72487221294570858, 21.86607318730131411, 6.500000000000000888 ) ) ;
#43768 = CARTESIAN_POINT ( 'NONE',  ( 7.361572987183170547, 7.050597817667451750, 9.846743663894590881 ) ) ;
#43769 = CARTESIAN_POINT ( 'NONE',  ( -1.504961813935599357, 2.551371850025192809E-18, 0.8438823471837141321 ) ) ;
#43770 = CARTESIAN_POINT ( 'NONE',  ( 14.92337183194729988, 39.34226448433412315, -8.527530157486177487 ) ) ;
#43771 = CARTESIAN_POINT ( 'NONE',  ( 5.076628168052704559, 65.17559781766745175, -8.527530157486179263 ) ) ;
#43772 = CARTESIAN_POINT ( 'NONE',  ( 2.035157376598824452, 38.68868534415483396, 7.964842623401179544 ) ) ;
#43773 = ORIENTED_EDGE ( 'NONE', *, *, #75556, .T. ) ;
#43774 = CARTESIAN_POINT ( 'NONE',  ( 19.38216949554541202, 60.99863466993042493, 9.382169495545424454 ) ) ;
#43775 = CARTESIAN_POINT ( 'NONE',  ( -8.000000000000000000, 0.000000000000000000, -6.250000000000000000 ) ) ;
#43776 = CARTESIAN_POINT ( 'NONE',  ( 20.88017736071110519, 65.56368534415483396, 2.639326808657452039E-16 ) ) ;
#43777 = CARTESIAN_POINT ( 'NONE',  ( 19.38216949554541557, 42.24863466993041783, -9.382169495545420901 ) ) ;
#43779 = CARTESIAN_POINT ( 'NONE',  ( 19.84674366389459621, 38.50893115100078745, 7.409399052514197653E-17 ) ) ;
#43778 = CARTESIAN_POINT ( 'NONE',  ( 22.26659068614894466, 63.88708216824730357, 7.082119434687054849 ) ) ;
#43780 = CARTESIAN_POINT ( 'NONE',  ( 7.361572987183170547, 2.050597817667451750, 9.846743663894590881 ) ) ;
#43781 = CARTESIAN_POINT ( 'NONE',  ( -0.3689425029237881626, 42.42874883491396787, 10.36894250292379027 ) ) ;
#43782 = CARTESIAN_POINT ( 'NONE',  ( 12.63842701281683034, 42.46726448433412315, 9.846743663894596210 ) ) ;
#43783 = CARTESIAN_POINT ( 'NONE',  ( 6.660464271194198815, -84.28715080305920537, -2.500000000000000444 ) ) ;
#43784 = CARTESIAN_POINT ( 'NONE',  ( 0.5774900079438590739, 42.64701867748816966, -5.440088680355550821 ) ) ;
#43785 = AXIS2_PLACEMENT_3D ( 'NONE', #49631, #4660, #59108 ) ;
#43786 = CARTESIAN_POINT ( 'NONE',  ( 12.91533473730992121, 59.52201867748816966, 10.88017736071110164 ) ) ;
#43787 = ORIENTED_EDGE ( 'NONE', *, *, #63640, .T. ) ;
#43788 = CARTESIAN_POINT ( 'NONE',  ( 16.40814093676324603, 42.45696800326375353, -11.09922568453594671 ) ) ;
#43789 = B_SPLINE_CURVE_WITH_KNOTS ( 'NONE', 3,
 ( #60072, #58599, #59586, #37594 ),
 .UNSPECIFIED., .F., .F.,
 ( 4, 4 ),
 ( 5.811364099686433976E-18, 0.002657014572710831961 ),
 .UNSPECIFIED. ) ;
#43790 = CARTESIAN_POINT ( 'NONE',  ( 2.791683348922240793, 1.633931151000784565, 7.208316651077764092 ) ) ;
#43791 = ORIENTED_EDGE ( 'NONE', *, *, #4245, .F. ) ;
#43792 = CARTESIAN_POINT ( 'NONE',  ( 2.917880565312950480, 5.970415501580634832, -12.26659068614894821 ) ) ;
#43793 = CARTESIAN_POINT ( 'NONE',  ( 19.84674366389459266, 13.30059781766745353, 2.638427012816836559 ) ) ;
#43794 = CARTESIAN_POINT ( 'NONE',  ( -0.3289641300568005855, 59.27164270246083788, -5.963430220938281678 ) ) ;
#43795 = ORIENTED_EDGE ( 'NONE', *, *, #95894, .T. ) ;
#43796 = EDGE_CURVE ( 'NONE', #4701, #88366, #13657, .T. ) ;
#43797 = CARTESIAN_POINT ( 'NONE',  ( 15.44008868035555793, 11.39701867748817143, -9.422509992056140149 ) ) ;
#43798 = FACE_OUTER_BOUND ( 'NONE', #76762, .T. ) ;
#43799 = EDGE_CURVE ( 'NONE', #22448, #40720, #18562, .T. ) ;
#43800 = EDGE_CURVE ( 'NONE', #53231, #94197, #67809, .T. ) ;
#43801 = ORIENTED_EDGE ( 'NONE', *, *, #21522, .T. ) ;
#43802 = CARTESIAN_POINT ( 'NONE',  ( 12.91533473730992121, 29.52201867748817321, 10.88017736071110164 ) ) ;
#43803 = CARTESIAN_POINT ( 'NONE',  ( 2.791683348922240793, 61.63393115100079456, 7.208316651077764092 ) ) ;
#43804 = ORIENTED_EDGE ( 'NONE', *, *, #60392, .F. ) ;
#43805 = CARTESIAN_POINT ( 'NONE',  ( 7.361572987183169658, 64.96726448433412315, -9.846743663894592657 ) ) ;
#43806 = ORIENTED_EDGE ( 'NONE', *, *, #70842, .F. ) ;
#43807 = CARTESIAN_POINT ( 'NONE',  ( 1.472469842513823179, 1.425597817667451528, 4.923371831947296329 ) ) ;
#43808 = PLANE ( 'NONE',  #17893 ) ;
#43809 = CARTESIAN_POINT ( 'NONE',  ( -1.099225684535947600, 39.54030133659708923, 6.408140936763237150 ) ) ;
#43811 = DIRECTION ( 'NONE',  ( 0.000000000000000000, 0.000000000000000000, 1.000000000000000000 ) ) ;
#43810 = CARTESIAN_POINT ( 'NONE',  ( 4.559911319644449179, 3.897018677488170990, 9.422509992056141925 ) ) ;
#43812 = CARTESIAN_POINT ( 'NONE',  ( 0.1532563361054100626, 5.800597817667452638, -2.638427012816831230 ) ) ;
#43813 = CARTESIAN_POINT ( 'NONE',  ( 4.559911319644449179, 12.23035201082150714, -9.422509992056141925 ) ) ;
#43814 = CIRCLE ( 'NONE', #82142, 15.00000000000000000 ) ;
#43815 = VERTEX_POINT ( 'NONE', #65116 ) ;
#43816 = CARTESIAN_POINT ( 'NONE',  ( -2.816281873526473856, 49.33196800326374643, 3.434112377981055619 ) ) ;
#43817 = CARTESIAN_POINT ( 'NONE',  ( 12.91533473730992121, 44.52201867748816966, 10.88017736071110164 ) ) ;
#43818 = DIRECTION ( 'NONE',  ( 0.000000000000000000, -1.000000000000000000, 0.000000000000000000 ) ) ;
#43819 = CARTESIAN_POINT ( 'NONE',  ( 10.00000000000000000, 37.87363466993041783, -12.81628187352647608 ) ) ;
#43820 = CARTESIAN_POINT ( 'NONE',  ( 4.559911319644449179, 48.89701867748817676, 9.422509992056141925 ) ) ;
#43821 = CARTESIAN_POINT ( 'NONE',  ( 2.791683348922240793, 51.63393115100078745, 7.208316651077764092 ) ) ;
#43822 = EDGE_CURVE ( 'NONE', #83218, #67137, #13767, .T. ) ;
#43823 = DIRECTION ( 'NONE',  ( 0.000000000000000000, -0.000000000000000000, -1.000000000000000000 ) ) ;
#43824 = CARTESIAN_POINT ( 'NONE',  ( 7.361572987183170547, 12.05059781766744997, 9.846743663894590881 ) ) ;
#43825 = CARTESIAN_POINT ( 'NONE',  ( -1.099225684535947600, 3.706968003263753531, -6.408140936763238038 ) ) ;
#43827 = CARTESIAN_POINT ( 'NONE',  ( 12.63842701281683922, 59.55059781766744464, -9.846743663894590881 ) ) ;
#43826 = CARTESIAN_POINT ( 'NONE',  ( 10.58171042697168929, 0.2301503269722701694, 10.54749450092408658 ) ) ;
#43828 = CARTESIAN_POINT ( 'NONE',  ( 2.035157376598822676, 27.43868534415483396, -7.964842623401177768 ) ) ;
#43829 = CARTESIAN_POINT ( 'NONE',  ( 12.63842701281683922, 44.55059781766745175, -9.846743663894590881 ) ) ;
#43830 = PLANE ( 'NONE',  #37590 ) ;
#43831 = CARTESIAN_POINT ( 'NONE',  ( 19.84674366389459266, 13.71726448433411782, -2.638427012816827677 ) ) ;
#43832 = CARTESIAN_POINT ( 'NONE',  ( 18.52753015748618282, 28.92559781766745175, -4.923371831947291888 ) ) ;
#43834 = ORIENTED_EDGE ( 'NONE', *, *, #3637, .F. ) ;
#43833 = CARTESIAN_POINT ( 'NONE',  ( 16.40814093676323893, 5.790301336597087456, 11.09922568453595026 ) ) ;
#43835 = CARTESIAN_POINT ( 'NONE',  ( 9.281709892946398810, 15.00000000000000178, 11.30302492080712540 ) ) ;
#43836 = DIRECTION ( 'NONE',  ( 0.8320502943378436100, -0.5547001962252291474, 0.000000000000000000 ) ) ;
#43837 = CARTESIAN_POINT ( 'NONE',  ( -1.099225684535947600, 43.70696800326375353, -6.408140936763238038 ) ) ;
#43838 = CARTESIAN_POINT ( 'NONE',  ( 1.472469842513823179, 30.59226448433411960, -4.923371831947296329 ) ) ;
#43839 = SURFACE_SIDE_STYLE ('',( #34368 ) ) ;
#43840 = CARTESIAN_POINT ( 'NONE',  ( 15.44008868035555793, 11.39701867748817143, -9.422509992056140149 ) ) ;
#43841 = CARTESIAN_POINT ( 'NONE',  ( 2.791683348922240793, 36.63393115100078035, 7.208316651077764092 ) ) ;
#43842 = MECHANICAL_DESIGN_GEOMETRIC_PRESENTATION_REPRESENTATION (  '', ( #61406 ), #27859 ) ;
#43843 = CARTESIAN_POINT ( 'NONE',  ( 0.000000000000000000, 15.00000000000000000, 0.000000000000000000 ) ) ;
#43844 = CIRCLE ( 'NONE', #792, 15.00000000000000000 ) ;
#43845 = CARTESIAN_POINT ( 'NONE',  ( 20.88017736071110519, 10.56368534415483929, 2.639326808657452039E-16 ) ) ;
#43846 = DIRECTION ( 'NONE',  ( 0.000000000000000000, 1.000000000000000000, 0.000000000000000000 ) ) ;
#43847 = CARTESIAN_POINT ( 'NONE',  ( 12.91533473730992121, 24.52201867748816966, 10.88017736071110164 ) ) ;
#43848 = CARTESIAN_POINT ( 'NONE',  ( 24.16423886937410614, 44.51208216824730357, -3.795296366450302550 ) ) ;
#43850 = DIRECTION ( 'NONE',  ( -0.000000000000000000, 1.000000000000000000, 0.000000000000000000 ) ) ;
#43849 = CARTESIAN_POINT ( 'NONE',  ( 2.917880565312948704, 47.63708216824730357, 12.26659068614894643 ) ) ;
#43851 = CARTESIAN_POINT ( 'NONE',  ( 10.00000000000000000, 9.758931151000785675, -9.846743663894594434 ) ) ;
#43852 = CARTESIAN_POINT ( 'NONE',  ( 19.84674366389459621, 63.50893115100078745, 7.409399052514197653E-17 ) ) ;
#43853 = ORIENTED_EDGE ( 'NONE', *, *, #61910, .T. ) ;
#43854 = CARTESIAN_POINT ( 'NONE',  ( 0.5774900079438590739, 52.64701867748817676, -5.440088680355550821 ) ) ;
#43855 = CARTESIAN_POINT ( 'NONE',  ( 1.274849032794164172, 18.57228050351029935, 6.499999999999802824 ) ) ;
#43856 = CARTESIAN_POINT ( 'NONE',  ( -3.836325488036278930, 15.00000000000000000, 14.50112432709419785 ) ) ;
#43857 = CARTESIAN_POINT ( 'NONE',  ( 17.20831665107776587, 64.13393115100079456, -7.208316651077762316 ) ) ;
#43858 = CARTESIAN_POINT ( 'NONE',  ( 14.99847009497948669, 14.63606908182952715, -0.2142307401080164042 ) ) ;
#43859 = CARTESIAN_POINT ( 'NONE',  ( 7.361572987183170547, 22.05059781766745530, 9.846743663894590881 ) ) ;
#43860 = DIRECTION ( 'NONE',  ( -1.000000000000000000, 0.000000000000000000, 0.000000000000000000 ) ) ;
#43861 = ORIENTED_EDGE ( 'NONE', *, *, #64231, .T. ) ;
#43862 = VECTOR ( 'NONE', #68371, 1000.000000000000000 ) ;
#43863 = CARTESIAN_POINT ( 'NONE',  ( 17.08211943468705840, 45.13708216824730357, -12.26659068614894466 ) ) ;
#43864 = CARTESIAN_POINT ( 'NONE',  ( 14.92337183194729633, 2.675597817667451750, 8.527530157486181039 ) ) ;
#43865 = DIRECTION ( 'NONE',  ( -1.000000000000000000, -0.000000000000000000, -0.000000000000000000 ) ) ;
#43866 = CARTESIAN_POINT ( 'NONE',  ( 15.44008868035555793, 36.39701867748816966, -9.422509992056140149 ) ) ;
#43867 = CARTESIAN_POINT ( 'NONE',  ( 3.591859063236761518, 34.95696800326375353, 11.09922568453594849 ) ) ;
#43868 =( LENGTH_UNIT ( ) NAMED_UNIT ( * ) SI_UNIT ( .MILLI., .METRE. ) );
#43869 = CARTESIAN_POINT ( 'NONE',  ( 22.81628187352648496, 31.83196800326375353, -3.434112377981050290 ) ) ;
#43870 = CARTESIAN_POINT ( 'NONE',  ( 0.6178305044545838731, 59.74863466993041783, 9.382169495545420901 ) ) ;
#43871 = ORIENTED_EDGE ( 'NONE', *, *, #22498, .F. ) ;
#43872 = SURFACE_SIDE_STYLE ('',( #21392 ) ) ;
#43873 = DIRECTION ( 'NONE',  ( 0.06975647374412534407, 0.9975640502598241977, -0.000000000000000000 ) ) ;
#43874 = CARTESIAN_POINT ( 'NONE',  ( -0.3689425029237898834, 26.17874883491396432, -10.36894250292378850 ) ) ;
#43875 = CARTESIAN_POINT ( 'NONE',  ( 20.36894250292379738, 4.928748834913967869, -10.36894250292379027 ) ) ;
#43876 = CARTESIAN_POINT ( 'NONE',  ( 17.96484262340118221, 4.938685344154837509, 7.964842623401181321 ) ) ;
#43877 = CARTESIAN_POINT ( 'NONE',  ( 15.44008868035555260, 24.73035201082150891, 9.422509992056143702 ) ) ;
#43878 = CARTESIAN_POINT ( 'NONE',  ( -8.099999999999999645, 75.73428692542562146, 2.900000000000000355 ) ) ;
#43879 = DIRECTION ( 'NONE',  ( -1.000000000000000000, 0.000000000000000000, 0.000000000000000000 ) ) ;
#43880 = CARTESIAN_POINT ( 'NONE',  ( 15.44008868035555793, 51.39701867748816966, -9.422509992056140149 ) ) ;
#43881 = CARTESIAN_POINT ( 'NONE',  ( 10.00000000000000178, 54.31368534415484106, 10.88017736071110342 ) ) ;
#43882 = CARTESIAN_POINT ( 'NONE',  ( 16.40814093676323893, 15.79030133659708746, 11.09922568453595026 ) ) ;
#43883 = LINE ( 'NONE', #74379, #66677 ) ;
#43884 = CARTESIAN_POINT ( 'NONE',  ( -0.03447792253739217355, 30.15514106990690024, 6.401564815979747358 ) ) ;
#43885 = CARTESIAN_POINT ( 'NONE',  ( 17.20831665107776587, 24.13393115100078035, -7.208316651077762316 ) ) ;
#43887 = EDGE_CURVE ( 'NONE', #13064, #73542, #41178, .T. ) ;
#43886 = AXIS2_PLACEMENT_3D ( 'NONE', #34574, #26121, #66067 ) ;
#43888 = CARTESIAN_POINT ( 'NONE',  ( 7.084665262690076126, 54.10535201082151247, 10.88017736071109987 ) ) ;
#43889 = CARTESIAN_POINT ( 'NONE',  ( 3.591859063236761518, 14.95696800326375531, 11.09922568453594849 ) ) ;
#43890 = CARTESIAN_POINT ( 'NONE',  ( 0.5774900079438590739, 42.64701867748816966, -5.440088680355550821 ) ) ;
#43891 = CARTESIAN_POINT ( 'NONE',  ( 10.00000000000000178, 22.25893115100078745, 9.846743663894594434 ) ) ;
#43892 = CARTESIAN_POINT ( 'NONE',  ( 13.43411237798105340, 50.58196800326375353, 12.81628187352647963 ) ) ;
#43894 = SURFACE_SIDE_STYLE ('',( #78463 ) ) ;
#43893 = CARTESIAN_POINT ( 'NONE',  ( 18.52753015748618282, 23.92559781766745530, -4.923371831947291888 ) ) ;
#43895 = ORIENTED_EDGE ( 'NONE', *, *, #77030, .F. ) ;
#43896 = CARTESIAN_POINT ( 'NONE',  ( 22.26659068614895176, 4.720415501580633943, -7.082119434687042414 ) ) ;
#43897 = CARTESIAN_POINT ( 'NONE',  ( 1.959929470562282283, 36.50257860105348584, 5.767676674365853629 ) ) ;
#43898 = CARTESIAN_POINT ( 'NONE',  ( 10.00000000000000178, 24.31368534415484106, 10.88017736071110342 ) ) ;
#43899 = CARTESIAN_POINT ( 'NONE',  ( 11.62719953690058361, 15.00000000000000000, 9.476720473301874392 ) ) ;
#43900 = CARTESIAN_POINT ( 'NONE',  ( 14.92337183194729988, 29.34226448433411960, -8.527530157486177487 ) ) ;
#43901 = CARTESIAN_POINT ( 'NONE',  ( 4.559911319644449179, 12.23035201082150536, -9.422509992056141925 ) ) ;
#43902 = CARTESIAN_POINT ( 'NONE',  ( 2.035157376598824452, 13.68868534415483751, 7.964842623401179544 ) ) ;
#43903 = ORIENTED_EDGE ( 'NONE', *, *, #14061, .T. ) ;
#43904 = VECTOR ( 'NONE', #22294, 1000.000000000000000 ) ;
#43905 = CARTESIAN_POINT ( 'NONE',  ( 20.88017736071110875, 25.77201867748816966, -2.915334737309920765 ) ) ;
#43906 = CARTESIAN_POINT ( 'NONE',  ( 21.09922568453595559, 47.04030133659708923, -6.408140936763230044 ) ) ;
#43907 = CARTESIAN_POINT ( 'NONE',  ( 20.88017736071110875, 35.77201867748816966, -2.915334737309920765 ) ) ;
#43908 = DIRECTION ( 'NONE',  ( -0.1650476058606810681, 0.000000000000000000, 0.9862856015372308827 ) ) ;
#43909 = EDGE_LOOP ( 'NONE', ( #49883, #38255, #27330, #55749 ) ) ;
#43911 = EDGE_CURVE ( 'NONE', #14317, #66694, #40906, .T. ) ;
#43910 = CARTESIAN_POINT ( 'NONE',  ( 4.559911319644449179, 42.23035201082151247, -9.422509992056141925 ) ) ;
#43912 = CARTESIAN_POINT ( 'NONE',  ( 4.630000000000001670, 1.019547802438464545, 4.000000000000000000 ) ) ;
#43913 =( LENGTH_UNIT ( ) NAMED_UNIT ( * ) SI_UNIT ( .MILLI., .METRE. ) );
#43914 = CARTESIAN_POINT ( 'NONE',  ( 13.43411237798106583, 62.66530133659708923, -12.81628187352647252 ) ) ;
#43915 = FACE_OUTER_BOUND ( 'NONE', #23707, .T. ) ;
#43916 = CARTESIAN_POINT ( 'NONE',  ( 22.26659068614894466, 48.88708216824730357, 7.082119434687054849 ) ) ;
#43917 = CARTESIAN_POINT ( 'NONE',  ( 20.88017736071110519, 50.56368534415484106, 2.639326808657452039E-16 ) ) ;
#43918 = CARTESIAN_POINT ( 'NONE',  ( 0.000000000000000000, 0.5000000000000004441, 0.000000000000000000 ) ) ;
#43919 = CIRCLE ( 'NONE', #40731, 0.2500000000000002220 ) ;
#43920 = ADVANCED_FACE ( 'NONE', ( #50625 ), #87630, .F. ) ;
#43921 = DIRECTION ( 'NONE',  ( -0.6494480483301851015, 0.000000000000000000, 0.7604059656000297096 ) ) ;
#43922 = CARTESIAN_POINT ( 'NONE',  ( 14.92337183194729988, 49.34226448433411605, -8.527530157486177487 ) ) ;
#43923 = CARTESIAN_POINT ( 'NONE',  ( 19.84674366389459266, 13.71726448433411782, -2.638427012816827677 ) ) ;
#43924 = ORIENTED_EDGE ( 'NONE', *, *, #62672, .T. ) ;
#43925 = CARTESIAN_POINT ( 'NONE',  ( 7.361572987183169658, 19.96726448433411960, -9.846743663894592657 ) ) ;
#43926 = CARTESIAN_POINT ( 'NONE',  ( 11.09922568453595026, -23.79303199673624292, 6.408140936763232709 ) ) ;
#43927 = CARTESIAN_POINT ( 'NONE',  ( 17.96484262340118221, 24.93868534415484461, 7.964842623401181321 ) ) ;
#43928 = CARTESIAN_POINT ( 'NONE',  ( 2.791683348922240793, 21.63393115100078745, 7.208316651077764092 ) ) ;
#43929 = CARTESIAN_POINT ( 'NONE',  ( 3.591859063236763294, 13.29030133659708746, -11.09922568453595026 ) ) ;
#43931 = CARTESIAN_POINT ( 'NONE',  ( 7.084665262690076126, 52.02201867748816255, -10.88017736071110164 ) ) ;
#43930 = CARTESIAN_POINT ( 'NONE',  ( 10.00000000000000000, 61.81368534415484106, -10.88017736071110342 ) ) ;
#43933 = CARTESIAN_POINT ( 'NONE',  ( 13.43411237798105340, 55.58196800326374643, 12.81628187352647963 ) ) ;
#43932 = CARTESIAN_POINT ( 'NONE',  ( 19.42250999205614548, 35.98035201082151247, -5.440088680355545492 ) ) ;
#43934 = CARTESIAN_POINT ( 'NONE',  ( 17.08211943468705840, 50.13708216824730357, -12.26659068614894466 ) ) ;
#43935 = PRESENTATION_LAYER_ASSIGNMENT (  '', '', ( #865 ) ) ;
#43936 = CYLINDRICAL_SURFACE ( 'NONE', #81794, 15.00000000000000000 ) ;
#43937 = VERTEX_POINT ( 'NONE', #27619 ) ;
#43938 = CARTESIAN_POINT ( 'NONE',  ( -2.816281873526473856, 4.123634669930420493, 9.499525473075851096E-16 ) ) ;
#43939 = CARTESIAN_POINT ( 'NONE',  ( 20.88017736071110164, 10.35535201082150714, 2.915334737309930979 ) ) ;
#43940 = CARTESIAN_POINT ( 'NONE',  ( 2.035157376598824452, 43.68868534415484106, 7.964842623401179544 ) ) ;
#43942 = ORIENTED_EDGE ( 'NONE', *, *, #51950, .T. ) ;
#43941 = EDGE_CURVE ( 'NONE', #27291, #79587, #10566, .T. ) ;
#43943 = CARTESIAN_POINT ( 'NONE',  ( 19.84674366389459266, 13.30059781766745353, 2.638427012816836559 ) ) ;
#43944 = CARTESIAN_POINT ( 'NONE',  ( 2.035157376598822676, 52.43868534415483396, -7.964842623401177768 ) ) ;
#43945 = CARTESIAN_POINT ( 'NONE',  ( 1.472469842513823179, 30.59226448433411960, -4.923371831947296329 ) ) ;
#43946 = CARTESIAN_POINT ( 'NONE',  ( 12.63842701281683922, 29.55059781766745175, -9.846743663894590881 ) ) ;
#43947 = CARTESIAN_POINT ( 'NONE',  ( 19.84674366389459266, 13.71726448433411782, -2.638427012816827677 ) ) ;
#43948 = MECHANICAL_DESIGN_GEOMETRIC_PRESENTATION_REPRESENTATION (  '', ( #890 ), #93427 ) ;
#43949 = CARTESIAN_POINT ( 'NONE',  ( 14.29730467489529389, 15.00000000000000000, 2.416004766803322656 ) ) ;
#43951 = DIRECTION ( 'NONE',  ( -0.1073935270325955676, -0.9942165912674659767, -0.000000000000000000 ) ) ;
#43950 = CARTESIAN_POINT ( 'NONE',  ( 2.035157376598824452, 68.68868534415484817, 7.964842623401179544 ) ) ;
#43952 = CARTESIAN_POINT ( 'NONE',  ( 11.04805072375712705, -95.57913125338676252, 3.750000000000000000 ) ) ;
#43954 = ORIENTED_EDGE ( 'NONE', *, *, #47299, .F. ) ;
#43953 = CARTESIAN_POINT ( 'NONE',  ( 18.52753015748618282, 33.92559781766745886, -4.923371831947291888 ) ) ;
#43955 = LINE ( 'NONE', #12484, #59766 ) ;
#43956 = CARTESIAN_POINT ( 'NONE',  ( 2.791683348922240793, 66.63393115100079456, 7.208316651077764092 ) ) ;
#43957 = CIRCLE ( 'NONE', #894, 0.2500000000000002220 ) ;
#43958 = LINE ( 'NONE', #95503, #34640 ) ;
#43959 = CARTESIAN_POINT ( 'NONE',  ( -0.3689425029237881626, 22.42874883491397142, 10.36894250292379027 ) ) ;
#43960 = CARTESIAN_POINT ( 'NONE',  ( 12.98685442714194949, 4.417933709739653524E-16, 6.449155920601044478 ) ) ;
#43961 = CARTESIAN_POINT ( 'NONE',  ( 17.08211943468705840, 35.13708216824730357, -12.26659068614894466 ) ) ;
#43962 = CARTESIAN_POINT ( 'NONE',  ( 20.36894250292379382, 43.67874883491397497, 10.36894250292379205 ) ) ;
#43963 = CARTESIAN_POINT ( 'NONE',  ( 10.00000000000000000, 10.55374883491396787, -14.16423886937410082 ) ) ;
#43965 = CARTESIAN_POINT ( 'NONE',  ( 20.88017736071110519, 65.56368534415483396, 2.639326808657452039E-16 ) ) ;
#43964 = CARTESIAN_POINT ( 'NONE',  ( -4.164238869374099039, 6.803748834913967869, 8.674139862899312516E-16 ) ) ;
#43966 = CARTESIAN_POINT ( 'NONE',  ( 12.91533473730992121, 54.52201867748816255, 10.88017736071110164 ) ) ;
#43967 = CARTESIAN_POINT ( 'NONE',  ( 14.88232117145530431, 0.3640475087720976277, 1.875237731503244243 ) ) ;
#43968 = AXIS2_PLACEMENT_3D ( 'NONE', #4025, #5501, #35974 ) ;
#43969 = EDGE_LOOP ( 'NONE', ( #57135, #69930, #57658, #46055 ) ) ;
#43970 = CARTESIAN_POINT ( 'NONE',  ( 18.52753015748617571, 28.09226448433411960, 4.923371831947298993 ) ) ;
#43972 = CARTESIAN_POINT ( 'NONE',  ( 19.84674366389459266, 23.30059781766745530, 2.638427012816836559 ) ) ;
#43971 = CARTESIAN_POINT ( 'NONE',  ( -0.8801773607111009756, 68.06368534415484817, 1.068504757029289695E-15 ) ) ;
#43973 = CARTESIAN_POINT ( 'NONE',  ( 17.96484262340118221, 11.18868534415484106, -7.964842623401177768 ) ) ;
#43974 = CARTESIAN_POINT ( 'NONE',  ( 10.00000000000000000, 62.87363466993042493, -12.81628187352647608 ) ) ;
#43975 = CARTESIAN_POINT ( 'NONE',  ( 5.076628168052704559, 45.17559781766745175, -8.527530157486179263 ) ) ;
#43976 = CARTESIAN_POINT ( 'NONE',  ( 18.00000000000000355, 78.65116054140185042, 3.749999999999999112 ) ) ;
#43977 = CARTESIAN_POINT ( 'NONE',  ( 12.63842701281683922, 24.55059781766745175, -9.846743663894590881 ) ) ;
#43978 = CARTESIAN_POINT ( 'NONE',  ( 19.38216949554541557, 37.24863466993041783, -9.382169495545420901 ) ) ;
#43980 = AXIS2_PLACEMENT_3D ( 'NONE', #93481, #70992, #32968 ) ;
#43979 = CARTESIAN_POINT ( 'NONE',  ( 7.082119434687054849, -16.52958449841936073, 12.26659068614894288 ) ) ;
#43981 = CARTESIAN_POINT ( 'NONE',  ( 15.44008868035555260, 49.73035201082150536, 9.422509992056143702 ) ) ;
#43982 = CARTESIAN_POINT ( 'NONE',  ( 1.472469842513823179, 40.59226448433411605, -4.923371831947296329 ) ) ;
#43983 = B_SPLINE_CURVE_WITH_KNOTS ( 'NONE', 3,
 ( #2267, #47232, #8272, #63221 ),
 .UNSPECIFIED., .F., .F.,
 ( 4, 4 ),
 ( 1.532679976604137452E-17, 0.002392975128318449059 ),
 .UNSPECIFIED. ) ;
#43984 = CARTESIAN_POINT ( 'NONE',  ( 2.917880565312948704, 27.63708216824730357, 12.26659068614894643 ) ) ;
#43985 = VERTEX_POINT ( 'NONE', #66106 ) ;
#43986 = CARTESIAN_POINT ( 'NONE',  ( 20.36894250292379382, 3.678748834913967869, 10.36894250292379205 ) ) ;
#43987 = CIRCLE ( 'NONE', #29640, 0.1000000000000001166 ) ;
#43988 = CARTESIAN_POINT ( 'NONE',  ( -0.8801773607111009756, 48.06368534415484817, 1.068504757029289695E-15 ) ) ;
#43989 = CARTESIAN_POINT ( 'NONE',  ( 10.00000000000000178, 69.31368534415484817, 10.88017736071110342 ) ) ;
#43990 = CARTESIAN_POINT ( 'NONE',  ( 17.08211943468705130, 53.47041550158063217, 12.26659068614894998 ) ) ;
#43991 = CARTESIAN_POINT ( 'NONE',  ( 3.591859063236761518, -0.04303199673624671928, 11.09922568453594849 ) ) ;
#43992 = DIRECTION ( 'NONE',  ( 0.000000000000000000, 0.000000000000000000, -1.000000000000000000 ) ) ;
#43993 = CARTESIAN_POINT ( 'NONE',  ( 10.00000000000000000, 56.81368534415484106, -10.88017736071110342 ) ) ;
#43994 = CARTESIAN_POINT ( 'NONE',  ( 12.60589901313216110, 15.00000000000000000, 8.129656208642140669 ) ) ;
#43995 = CARTESIAN_POINT ( 'NONE',  ( 17.20831665107776587, 64.13393115100079456, -7.208316651077762316 ) ) ;
#43996 = CARTESIAN_POINT ( 'NONE',  ( -5.440088680355558814, 27.23035201082150891, -9.422509992056136596 ) ) ;
#43997 = CARTESIAN_POINT ( 'NONE',  ( 12.91533473730992121, 14.52201867748817143, 10.88017736071110164 ) ) ;
#43998 = CARTESIAN_POINT ( 'NONE',  ( 15.44008868035555793, 11.39701867748817143, -9.422509992056140149 ) ) ;
#43999 = CARTESIAN_POINT ( 'NONE',  ( 18.52753015748617571, 38.09226448433412315, 4.923371831947298993 ) ) ;
#44000 = DIRECTION ( 'NONE',  ( -0.1927083333333330095, 0.9812560818990572198, -5.348730717595142060E-15 ) ) ;
#44001 = ORIENTED_EDGE ( 'NONE', *, *, #90571, .T. ) ;
#44002 = ADVANCED_FACE ( 'NONE', ( #4153 ), #95636, .F. ) ;
#44003 = CARTESIAN_POINT ( 'NONE',  ( 20.88017736071110164, 10.35535201082150714, 2.915334737309930979 ) ) ;
#44004 = CARTESIAN_POINT ( 'NONE',  ( 6.565887622018943937, 0.1653013365970866511, 12.81628187352647430 ) ) ;
#44005 = CARTESIAN_POINT ( 'NONE',  ( 2.603489959281613420, 60.43575266056826933, -6.500000000000031086 ) ) ;
#44006 = CARTESIAN_POINT ( 'NONE',  ( 1.472469842513823179, 16.42559781766745175, 4.923371831947296329 ) ) ;
#44007 = AXIS2_PLACEMENT_3D ( 'NONE', #65128, #3673, #64627 ) ;
#44008 = CARTESIAN_POINT ( 'NONE',  ( 12.63842701281683034, 32.46726448433412315, 9.846743663894596210 ) ) ;
#44009 = CARTESIAN_POINT ( 'NONE',  ( 20.88017736071110875, 35.77201867748816966, -2.915334737309920765 ) ) ;
#44010 = CARTESIAN_POINT ( 'NONE',  ( 3.591859063236763294, 13.29030133659708746, -11.09922568453595026 ) ) ;
#44012 = CARTESIAN_POINT ( 'NONE',  ( 3.195792623639471142, 11.20379003517448346, -11.92686044187660066 ) ) ;
#44011 = CARTESIAN_POINT ( 'NONE',  ( 10.00000000000000178, 49.31368534415484106, 10.88017736071110342 ) ) ;
#44013 = DIRECTION ( 'NONE',  ( 6.608470384673550777E-17, 1.000000000000000000, -0.000000000000000000 ) ) ;
#44014 = CARTESIAN_POINT ( 'NONE',  ( 13.43411237798106583, 57.66530133659708923, -12.81628187352647252 ) ) ;
#44015 = VERTEX_POINT ( 'NONE', #50124 ) ;
#44016 = CARTESIAN_POINT ( 'NONE',  ( -0.8801773607111008646, 68.27201867748817676, 2.915334737309923430 ) ) ;
#44018 = CARTESIAN_POINT ( 'NONE',  ( 10.00000000000000178, 8.053748834913967869, 14.16423886937410082 ) ) ;
#44017 = CARTESIAN_POINT ( 'NONE',  ( 10.00000000000000178, 30.37363466993042138, 12.81628187352647608 ) ) ;
#44019 = CARTESIAN_POINT ( 'NONE',  ( 34.56412365047463453, 26.99999999999999645, -10.00000000000000000 ) ) ;
#44020 = CARTESIAN_POINT ( 'NONE',  ( 0.5774900079438607392, 38.48035201082150536, 5.440088680355550821 ) ) ;
#44021 = CARTESIAN_POINT ( 'NONE',  ( 0.1532563361054082862, 66.21726448433413736, 2.638427012816831674 ) ) ;
#44022 = CARTESIAN_POINT ( 'NONE',  ( 1.472469842513823179, 51.42559781766745886, 4.923371831947296329 ) ) ;
#44023 = CARTESIAN_POINT ( 'NONE',  ( 14.92337183194729988, 14.34226448433411782, -8.527530157486177487 ) ) ;
#44024 = CARTESIAN_POINT ( 'NONE',  ( 7.361572987183170547, 7.050597817667451750, 9.846743663894590881 ) ) ;
#44025 = DIRECTION ( 'NONE',  ( 0.000000000000000000, 1.000000000000000000, 0.000000000000000000 ) ) ;
#44026 = CARTESIAN_POINT ( 'NONE',  ( 13.79529636645031943, 30.34541550158063927, -14.16423886937409904 ) ) ;
#44027 = AXIS2_PLACEMENT_3D ( 'NONE', #20256, #58737, #95258 ) ;
#44028 = CARTESIAN_POINT ( 'NONE',  ( -4.000000000000000000, 10.00000000000000000, 2.750000000000000000 ) ) ;
#44029 = SURFACE_SIDE_STYLE ('',( #90515 ) ) ;
#44030 = SURFACE_STYLE_FILL_AREA ( #73539 ) ;
#44031 = EDGE_LOOP ( 'NONE', ( #2253, #37080, #91683, #3139 ) ) ;
#44032 = CARTESIAN_POINT ( 'NONE',  ( 20.36894250292379738, 59.92874883491397497, -10.36894250292379027 ) ) ;
#44034 = EDGE_CURVE ( 'NONE', #85266, #66421, #79226, .T. ) ;
#44033 = CARTESIAN_POINT ( 'NONE',  ( -4.164238869374099927, 57.01208216824731068, 3.795296366450308767 ) ) ;
#44035 = CARTESIAN_POINT ( 'NONE',  ( 2.791683348922240793, 26.63393115100078745, 7.208316651077764092 ) ) ;
#44037 = CARTESIAN_POINT ( 'NONE',  ( 13.43411237798105340, 30.58196800326374998, 12.81628187352647963 ) ) ;
#44036 = VECTOR ( 'NONE', #2376, 1000.000000000000114 ) ;
#44038 = DIRECTION ( 'NONE',  ( 0.000000000000000000, -1.000000000000000000, 0.000000000000000000 ) ) ;
#44039 = CARTESIAN_POINT ( 'NONE',  ( -1.926860441876563801, 42.66212336850781384, 1.004413902775740978E-15 ) ) ;
#44040 = CARTESIAN_POINT ( 'NONE',  ( 0.5774900079438607392, 18.48035201082150536, 5.440088680355550821 ) ) ;
#44041 = CARTESIAN_POINT ( 'NONE',  ( 13.79529636645030344, 53.26208216824730357, 14.16423886937410614 ) ) ;
#44042 = CARTESIAN_POINT ( 'NONE',  ( 19.84674366389459266, 23.30059781766745530, 2.638427012816836559 ) ) ;
#44043 = ADVANCED_FACE ( 'NONE', ( #79649 ), #89115, .T. ) ;
#44044 = CARTESIAN_POINT ( 'NONE',  ( 4.746257547686181688, 0.000000000000000000, 2.685303318749109547 ) ) ;
#44045 = CARTESIAN_POINT ( 'NONE',  ( 0.1532563361054082862, 16.21726448433411960, 2.638427012816831674 ) ) ;
#44046 = CARTESIAN_POINT ( 'NONE',  ( 18.39792806157247895, 59.52224192338640307, 6.500000000000035527 ) ) ;
#44047 = CARTESIAN_POINT ( 'NONE',  ( 7.208316651077764980, 12.88393115100078390, 7.208316651077762316 ) ) ;
#44048 = ORIENTED_EDGE ( 'NONE', *, *, #66946, .F. ) ;
#44049 = ORIENTED_EDGE ( 'NONE', *, *, #97728, .F. ) ;
#44050 = DIRECTION ( 'NONE',  ( -0.000000000000000000, -0.000000000000000000, -1.000000000000000000 ) ) ;
#44051 = VERTEX_POINT ( 'NONE', #33630 ) ;
#44053 = CARTESIAN_POINT ( 'NONE',  ( 10.00000000000000178, 24.31368534415484106, 10.88017736071110342 ) ) ;
#44052 = CARTESIAN_POINT ( 'NONE',  ( 20.88017736071110519, 25.56368534415483751, 2.639326808657452039E-16 ) ) ;
#44055 = CARTESIAN_POINT ( 'NONE',  ( 13.43411237798106583, 22.66530133659708923, -12.81628187352647252 ) ) ;
#44054 = CARTESIAN_POINT ( 'NONE',  ( 14.92337183194729633, 62.67559781766745886, 8.527530157486181039 ) ) ;
#44056 = CARTESIAN_POINT ( 'NONE',  ( -4.164238869374099927, 7.012082168247302683, 3.795296366450308767 ) ) ;
#44057 = CIRCLE ( 'NONE', #39300, 14.49999999999999822 ) ;
#44058 = CARTESIAN_POINT ( 'NONE',  ( 22.81628187352647785, 26.62363466993042138, 6.195893100308588602E-16 ) ) ;
#44059 = ORIENTED_EDGE ( 'NONE', *, *, #7933, .T. ) ;
#44060 = CARTESIAN_POINT ( 'NONE',  ( 0.1532563361054082862, 31.21726448433412315, 2.638427012816831674 ) ) ;
#44061 = CARTESIAN_POINT ( 'NONE',  ( 15.44008868035555260, 9.730352010821505360, 9.422509992056143702 ) ) ;
#44062 = B_SPLINE_CURVE_WITH_KNOTS ( 'NONE', 3,
 ( #21282, #59760, #90254, #37284, #90753, #67774 ),
 .UNSPECIFIED., .F., .F.,
 ( 4, 2, 4 ),
 ( 0.0002800003243993108831, 0.0006862055569927221887, 0.001092410789586133494 ),
 .UNSPECIFIED. ) ;
#44063 = CARTESIAN_POINT ( 'NONE',  ( 6.204703633549690345, 65.76208216824731778, -14.16423886937410259 ) ) ;
#44064 = ORIENTED_EDGE ( 'NONE', *, *, #52783, .T. ) ;
#44065 = CARTESIAN_POINT ( 'NONE',  ( 0.5774900079438607392, 53.48035201082151247, 5.440088680355550821 ) ) ;
#44066 = CARTESIAN_POINT ( 'NONE',  ( -0.8801773607111008646, 53.27201867748816966, 2.915334737309923430 ) ) ;
#44067 = CARTESIAN_POINT ( 'NONE',  ( 15.44008868035555793, 51.39701867748816966, -9.422509992056140149 ) ) ;
#44068 = FILL_AREA_STYLE_COLOUR ( '', #63108 ) ;
#44069 = CARTESIAN_POINT ( 'NONE',  ( 4.559911319644449179, 52.23035201082151247, -9.422509992056141925 ) ) ;
#44070 = DIRECTION ( 'NONE',  ( -0.8703556959399010307, 0.000000000000000000, 0.4924235601034648302 ) ) ;
#44071 = PRESENTATION_STYLE_ASSIGNMENT (( #13588 ) ) ;
#44072 = CARTESIAN_POINT ( 'NONE',  ( 14.92337183194729633, 27.67559781766745530, 8.527530157486181039 ) ) ;
#44073 = EDGE_LOOP ( 'NONE', ( #8073, #78541, #59896, #66811 ) ) ;
#44074 = CARTESIAN_POINT ( 'NONE',  ( 17.20831665107776587, 54.13393115100079456, -7.208316651077762316 ) ) ;
#44075 = B_SPLINE_CURVE_WITH_KNOTS ( 'NONE', 3,
 ( #2260, #62721, #78724, #11699 ),
 .UNSPECIFIED., .F., .F.,
 ( 4, 4 ),
 ( 5.284504157781969479E-17, 0.002562518741975526333 ),
 .UNSPECIFIED. ) ;
#44076 = CARTESIAN_POINT ( 'NONE',  ( 14.04391541078762984, 15.00000000000000000, -3.608107528142820986 ) ) ;
#44077 = EDGE_LOOP ( 'NONE', ( #46613, #71660, #88156, #7075, #52675, #75003, #65517, #65817 ) ) ;
#44078 = DIRECTION ( 'NONE',  ( -0.6626200482157408311, 0.000000000000000000, 0.7489557207889990798 ) ) ;
#44079 = CARTESIAN_POINT ( 'NONE',  ( -7.072466569316883778, -84.40185462517210624, 3.750000000000001776 ) ) ;
#44080 = DIRECTION ( 'NONE',  ( 2.309263891220325920E-14, 0.000000000000000000, 1.000000000000000000 ) ) ;
#44081 = CARTESIAN_POINT ( 'NONE',  ( 15.44008868035555793, 11.39701867748817143, -9.422509992056140149 ) ) ;
#44082 = CARTESIAN_POINT ( 'NONE',  ( 0.000000000000000000, 14.49999999999999822, 0.000000000000000000 ) ) ;
#44083 = VERTEX_POINT ( 'NONE', #35622 ) ;
#44084 = CARTESIAN_POINT ( 'NONE',  ( -10.32896413005680536, 4.271642702460845875, -5.963430220938272797 ) ) ;
#44085 = CARTESIAN_POINT ( 'NONE',  ( 5.076628168052703671, 51.84226448433412315, 8.527530157486179263 ) ) ;
#44086 = LINE ( 'NONE', #68096, #24393 ) ;
#44087 = AXIS2_PLACEMENT_3D ( 'NONE', #84606, #48556, #85589 ) ;
#44088 = CARTESIAN_POINT ( 'NONE',  ( 13.43411237798106583, 12.66530133659708746, -12.81628187352647252 ) ) ;
#44089 = CARTESIAN_POINT ( 'NONE',  ( 0.1532563361054082862, 11.21726448433411605, 2.638427012816831674 ) ) ;
#44090 = FACE_OUTER_BOUND ( 'NONE', #36197, .T. ) ;
#44091 = CARTESIAN_POINT ( 'NONE',  ( 19.84674366389459266, 18.71726448433411960, -2.638427012816827677 ) ) ;
#44092 = CARTESIAN_POINT ( 'NONE',  ( 19.38216949554541557, 2.248634669930420049, -9.382169495545420901 ) ) ;
#44093 = DIRECTION ( 'NONE',  ( 0.1132032137679039180, -0.000000000000000000, 0.9935718556765877896 ) ) ;
#44094 = ORIENTED_EDGE ( 'NONE', *, *, #92595, .T. ) ;
#44095 = CARTESIAN_POINT ( 'NONE',  ( 17.96484262340118221, 6.188685344154837509, -7.964842623401177768 ) ) ;
#44096 = CARTESIAN_POINT ( 'NONE',  ( 22.26659068614894466, 3.887082168247300906, 7.082119434687054849 ) ) ;
#44097 = CARTESIAN_POINT ( 'NONE',  ( 18.52753015748618282, 23.92559781766745530, -4.923371831947291888 ) ) ;
#44098 = CARTESIAN_POINT ( 'NONE',  ( 0.5774900079438607392, 53.48035201082151247, 5.440088680355550821 ) ) ;
#44100 = DIRECTION ( 'NONE',  ( -1.000000000000000000, 0.000000000000000000, 0.000000000000000000 ) ) ;
#44099 = CARTESIAN_POINT ( 'NONE',  ( -2.816281873526471635, 38.91530133659708213, -3.434112377981056508 ) ) ;
#44101 = CARTESIAN_POINT ( 'NONE',  ( 20.88017736071110164, 20.35535201082150891, 2.915334737309930979 ) ) ;
#44102 = CARTESIAN_POINT ( 'NONE',  ( 20.10239578412225825, 17.63377557478296609, -6.340343622311919169 ) ) ;
#44103 = CARTESIAN_POINT ( 'NONE',  ( 13.30119215211372641, 14.76984893004598476, 6.804450086558370359 ) ) ;
#44104 = CARTESIAN_POINT ( 'NONE',  ( 6.565887622018943937, 5.165301336597086568, 12.81628187352647430 ) ) ;
#44105 = CARTESIAN_POINT ( 'NONE',  ( 7.361572987183169658, 64.96726448433412315, -9.846743663894592657 ) ) ;
#44106 = CARTESIAN_POINT ( 'NONE',  ( 1.472469842513823179, 25.59226448433412315, -4.923371831947296329 ) ) ;
#44107 = CARTESIAN_POINT ( 'NONE',  ( 3.469446951953614189E-15, -10.68631465584515894, 10.88017736071110342 ) ) ;
#44108 = CARTESIAN_POINT ( 'NONE',  ( 19.38216949554541202, 40.99863466993042493, 9.382169495545424454 ) ) ;
#44110 = DIRECTION ( 'NONE',  ( -0.000000000000000000, -1.000000000000000000, -0.000000000000000000 ) ) ;
#44109 = CARTESIAN_POINT ( 'NONE',  ( 19.42250999205614548, 35.98035201082151247, -5.440088680355545492 ) ) ;
#44111 =( GEOMETRIC_REPRESENTATION_CONTEXT ( 3 ) GLOBAL_UNCERTAINTY_ASSIGNED_CONTEXT ( ( #4182 ) ) GLOBAL_UNIT_ASSIGNED_CONTEXT ( ( #71788, #11772, #58747 ) ) REPRESENTATION_CONTEXT ( 'NONE', 'WORKASPACE' ) );
#44112 = EDGE_CURVE ( 'NONE', #82054, #1778, #20626, .T. ) ;
#44113 = CARTESIAN_POINT ( 'NONE',  ( 14.99999999999997868, 80.07179676972448590, 6.250000000000000000 ) ) ;
#44114 = VECTOR ( 'NONE', #11769, 1000.000000000000000 ) ;
#44115 = CARTESIAN_POINT ( 'NONE',  ( 17.96484262340118221, 44.93868534415483396, 7.964842623401181321 ) ) ;
#44116 = CIRCLE ( 'NONE', #68062, 14.49999999999999822 ) ;
#44117 = CARTESIAN_POINT ( 'NONE',  ( 10.00000000000000178, 29.31368534415483751, 10.88017736071110342 ) ) ;
#44118 = CARTESIAN_POINT ( 'NONE',  ( 0.1532563361054100626, 65.80059781766745175, -2.638427012816831230 ) ) ;
#44119 = CARTESIAN_POINT ( 'NONE',  ( 20.88017736071110519, 50.56368534415484106, 2.639326808657452039E-16 ) ) ;
#44120 = AXIS2_PLACEMENT_3D ( 'NONE', #49121, #89088, #57107 ) ;
#44121 = UNCERTAINTY_MEASURE_WITH_UNIT (LENGTH_MEASURE( 1.000000000000000082E-05 ), #52749, 'distance_accuracy_value', 'NONE');
#44122 = CARTESIAN_POINT ( 'NONE',  ( 18.52753015748618282, 38.92559781766745175, -4.923371831947291888 ) ) ;
#44123 = CARTESIAN_POINT ( 'NONE',  ( 16.40814093676323893, 60.79030133659709634, 11.09922568453595026 ) ) ;
#44124 = CARTESIAN_POINT ( 'NONE',  ( 6.565887622018943937, 15.16530133659708568, 12.81628187352647430 ) ) ;
#44125 = ORIENTED_EDGE ( 'NONE', *, *, #46064, .F. ) ;
#44126 = CARTESIAN_POINT ( 'NONE',  ( 4.559911319644449179, 27.23035201082150536, -9.422509992056141925 ) ) ;
#44127 =( NAMED_UNIT ( * ) SI_UNIT ( $, .STERADIAN. ) SOLID_ANGLE_UNIT ( ) );
#44128 = CARTESIAN_POINT ( 'NONE',  ( 12.91533473730992121, 19.52201867748816611, 10.88017736071110164 ) ) ;
#44129 = CARTESIAN_POINT ( 'NONE',  ( 19.84674366389459621, 3.508931151000785231, 7.409399052514197653E-17 ) ) ;
#44130 = CARTESIAN_POINT ( 'NONE',  ( 22.26659068614895176, 24.72041550158063572, -7.082119434687042414 ) ) ;
#44131 = CARTESIAN_POINT ( 'NONE',  ( 18.52753015748618282, 8.925597817667451750, -4.923371831947291888 ) ) ;
#44132 = CARTESIAN_POINT ( 'NONE',  ( 3.927832320392154575, -0.03417435944610275333, 13.69797916712106733 ) ) ;
#44133 = CARTESIAN_POINT ( 'NONE',  ( -0.8801773607111008646, 43.27201867748817676, 2.915334737309923430 ) ) ;
#44134 = DIRECTION ( 'NONE',  ( 0.000000000000000000, 0.000000000000000000, 1.000000000000000000 ) ) ;
#44135 = CARTESIAN_POINT ( 'NONE',  ( 69.60148758828984228, 0.4999999999999960032, -10.00000000000000000 ) ) ;
#44137 = ORIENTED_EDGE ( 'NONE', *, *, #74390, .F. ) ;
#44136 = VECTOR ( 'NONE', #7228, 1000.000000000000000 ) ;
#44138 = CARTESIAN_POINT ( 'NONE',  ( -14.82269085861167035, 14.63595249122789177, -2.299529454047154697 ) ) ;
#44139 = CARTESIAN_POINT ( 'NONE',  ( 14.92337183194729988, 44.34226448433412315, -8.527530157486177487 ) ) ;
#44140 = VECTOR ( 'NONE', #76923, 1000.000000000000000 ) ;
#44141 = VERTEX_POINT ( 'NONE', #3661 ) ;
#44142 = ORIENTED_EDGE ( 'NONE', *, *, #97816, .F. ) ;
#44143 = CARTESIAN_POINT ( 'NONE',  ( 10.00000000000000000, 20.55374883491396787, -14.16423886937410082 ) ) ;
#44146 = EDGE_CURVE ( 'NONE', #22113, #83062, #51115, .T. ) ;
#44145 = AXIS2_PLACEMENT_3D ( 'NONE', #39080, #70556, #83593 ) ;
#44144 = CARTESIAN_POINT ( 'NONE',  ( 20.36894250292379738, 29.92874883491396432, -10.36894250292379027 ) ) ;
#44147 = CARTESIAN_POINT ( 'NONE',  ( 0.5774900079438590739, 57.64701867748817676, -5.440088680355550821 ) ) ;
#44148 = CARTESIAN_POINT ( 'NONE',  ( -0.3689425029237898834, 66.17874883491396076, -10.36894250292378850 ) ) ;
#44149 = CARTESIAN_POINT ( 'NONE',  ( -2.816281873526471635, 3.915301336597087456, -3.434112377981056508 ) ) ;
#44150 = CARTESIAN_POINT ( 'NONE',  ( 1.472469842513823179, 50.59226448433411605, -4.923371831947296329 ) ) ;
#44151 = CARTESIAN_POINT ( 'NONE',  ( -11.42361443046363512, -90.30744058745631264, 3.999999999999998224 ) ) ;
#44153 = CARTESIAN_POINT ( 'NONE',  ( 19.38216949554541202, 0.9986346699304200492, 9.382169495545424454 ) ) ;
#44152 = CARTESIAN_POINT ( 'NONE',  ( 0.5774900079438590739, 42.64701867748816966, -5.440088680355550821 ) ) ;
#44154 = CARTESIAN_POINT ( 'NONE',  ( 17.08211943468705130, 23.47041550158063572, 12.26659068614894998 ) ) ;
#44155 = CARTESIAN_POINT ( 'NONE',  ( 15.44008868035555260, 19.73035201082150536, 9.422509992056143702 ) ) ;
#44156 = CARTESIAN_POINT ( 'NONE',  ( 12.91533473730992121, 14.52201867748817143, 10.88017736071110164 ) ) ;
#44157 = FACE_OUTER_BOUND ( 'NONE', #51426, .T. ) ;
#44158 = CARTESIAN_POINT ( 'NONE',  ( 20.88017736071110164, 40.35535201082150536, 2.915334737309930979 ) ) ;
#44159 = CARTESIAN_POINT ( 'NONE',  ( 10.00000000000000178, 45.37363466993041783, 12.81628187352647608 ) ) ;
#44160 = CARTESIAN_POINT ( 'NONE',  ( 4.923371831947301658, -17.32440218233254470, 8.527530157486175710 ) ) ;
#44161 = ORIENTED_EDGE ( 'NONE', *, *, #32879, .F. ) ;
#44162 = CARTESIAN_POINT ( 'NONE',  ( 19.89220837332776526, 4.740628644642391087, 6.478736007405957231 ) ) ;
#44163 = VERTEX_POINT ( 'NONE', #64129 ) ;
#44164 = B_SPLINE_CURVE_WITH_KNOTS ( 'NONE', 3,
 ( #9176, #39694, #77175, #10169, #16195, #23713 ),
 .UNSPECIFIED., .F., .F.,
 ( 4, 2, 4 ),
 ( 3.409110551496062250E-05, 0.0004400426677367845658, 0.0008459942299586084482 ),
 .UNSPECIFIED. ) ;
#44165 = ORIENTED_EDGE ( 'NONE', *, *, #49690, .F. ) ;
#44166 = VECTOR ( 'NONE', #28160, 999.9999999999998863 ) ;
#44167 = LINE ( 'NONE', #52663, #37727 ) ;
#44168 = CARTESIAN_POINT ( 'NONE',  ( 17.08211943468705840, 45.13708216824730357, -12.26659068614894466 ) ) ;
#44170 = CARTESIAN_POINT ( 'NONE',  ( 0.1532563361054100626, 40.80059781766745886, -2.638427012816831230 ) ) ;
#44169 = CARTESIAN_POINT ( 'NONE',  ( 1.472469842513823179, 21.42559781766745175, 4.923371831947296329 ) ) ;
#44171 = CARTESIAN_POINT ( 'NONE',  ( 0.5774900079438590739, 67.64701867748817676, -5.440088680355550821 ) ) ;
#44172 = DIRECTION ( 'NONE',  ( 0.000000000000000000, 0.000000000000000000, -1.000000000000000000 ) ) ;
#44173 = CARTESIAN_POINT ( 'NONE',  ( 18.52753015748617571, 3.092264484334118269, 4.923371831947298993 ) ) ;
#44174 = CARTESIAN_POINT ( 'NONE',  ( -2.816281873526471635, 58.91530133659707502, -3.434112377981056508 ) ) ;
#44175 = CARTESIAN_POINT ( 'NONE',  ( 11.09922568453594671, 27.04030133659709989, -6.408140936763241591 ) ) ;
#44176 = VERTEX_POINT ( 'NONE', #94647 ) ;
#44177 = CARTESIAN_POINT ( 'NONE',  ( 24.16423886937410614, 34.30374883491396787, 8.672049930838204340E-16 ) ) ;
#44178 = VERTEX_POINT ( 'NONE', #26156 ) ;
#44179 = CARTESIAN_POINT ( 'NONE',  ( 22.81628187352647785, 21.62363466993041783, 6.195893100308588602E-16 ) ) ;
#44180 = ORIENTED_EDGE ( 'NONE', *, *, #22261, .T. ) ;
#44181 = CARTESIAN_POINT ( 'NONE',  ( 21.09922568453594849, 46.20696800326376064, 6.408140936763242479 ) ) ;
#44182 = ADVANCED_FACE ( 'NONE', ( #56650 ), #33125, .T. ) ;
#44183 = CARTESIAN_POINT ( 'NONE',  ( 18.52753015748618282, 38.92559781766745175, -4.923371831947291888 ) ) ;
#44184 = CARTESIAN_POINT ( 'NONE',  ( 17.96484262340118221, 9.938685344154837509, 7.964842623401181321 ) ) ;
#44185 = CARTESIAN_POINT ( 'NONE',  ( -2.816281873526471635, 63.91530133659708923, -3.434112377981056508 ) ) ;
#44186 = PLANE ( 'NONE',  #84714 ) ;
#44187 = CARTESIAN_POINT ( 'NONE',  ( 7.361572987183169658, 39.96726448433411605, -9.846743663894592657 ) ) ;
#44188 = CARTESIAN_POINT ( 'NONE',  ( 18.52753015748617571, 48.09226448433412315, 4.923371831947298993 ) ) ;
#44189 = EDGE_CURVE ( 'NONE', #2722, #19871, #34125, .T. ) ;
#44190 = CARTESIAN_POINT ( 'NONE',  ( 11.34661744925197624, 54.08985607419764818, -2.899999999999999467 ) ) ;
#44191 = DIRECTION ( 'NONE',  ( -0.000000000000000000, -1.000000000000000000, -0.000000000000000000 ) ) ;
#44192 = CARTESIAN_POINT ( 'NONE',  ( -14.88232117145532385, 15.00000000000000000, 1.875237731503040628 ) ) ;
#44193 = CARTESIAN_POINT ( 'NONE',  ( 1.274849032794317383, 27.55509018479935790, -6.500000000000010658 ) ) ;
#44194 = AXIS2_PLACEMENT_3D ( 'NONE', #39191, #22223, #14726 ) ;
#44195 = FACE_BOUND ( 'NONE', #48344, .T. ) ;
#44196 = CARTESIAN_POINT ( 'NONE',  ( 1.472469842513823179, 15.59226448433411960, -4.923371831947296329 ) ) ;
#44197 = CARTESIAN_POINT ( 'NONE',  ( 3.591859063236763294, 33.29030133659708213, -11.09922568453595026 ) ) ;
#44198 = LINE ( 'NONE', #6707, #70716 ) ;
#44199 = ADVANCED_FACE ( 'NONE', ( #57134 ), #19144, .F. ) ;
#44200 = VERTEX_POINT ( 'NONE', #52592 ) ;
#44201 = CARTESIAN_POINT ( 'NONE',  ( 14.92337183194729633, 52.67559781766745175, 8.527530157486181039 ) ) ;
#44202 = CARTESIAN_POINT ( 'NONE',  ( -14.35840480524203144, 0.5000000000000004441, 4.340070442838751319 ) ) ;
#44203 = CARTESIAN_POINT ( 'NONE',  ( 20.36894250292379738, 19.92874883491396787, -10.36894250292379027 ) ) ;
#44204 = CARTESIAN_POINT ( 'NONE',  ( 17.20831665107776587, 52.88393115100078035, 7.208316651077764980 ) ) ;
#44205 = CARTESIAN_POINT ( 'NONE',  ( 0.6178305044545838731, 49.74863466993041072, 9.382169495545420901 ) ) ;
#44207 =( NAMED_UNIT ( * ) PLANE_ANGLE_UNIT ( ) SI_UNIT ( $, .RADIAN. ) );
#44206 = CARTESIAN_POINT ( 'NONE',  ( -4.180366052181437198, 14.99999999999798206, 14.01545757926889557 ) ) ;
#44208 = CARTESIAN_POINT ( 'NONE',  ( 7.361572987183169658, -0.03273551566588185635, -9.846743663894592657 ) ) ;
#44209 = VECTOR ( 'NONE', #47801, 1000.000000000000000 ) ;
#44210 = CYLINDRICAL_SURFACE ( 'NONE', #40797, 15.00000000000000000 ) ;
#44211 = CARTESIAN_POINT ( 'NONE',  ( 18.52753015748617571, 43.09226448433412315, 4.923371831947298993 ) ) ;
#44212 = CARTESIAN_POINT ( 'NONE',  ( 17.96484262340118221, 36.18868534415484106, -7.964842623401177768 ) ) ;
#44213 = AXIS2_PLACEMENT_3D ( 'NONE', #40044, #93031, #26027 ) ;
#44214 = CARTESIAN_POINT ( 'NONE',  ( 5.076628168052704559, 35.17559781766745175, -8.527530157486179263 ) ) ;
#44215 = CIRCLE ( 'NONE', #71371, 14.49999999999999822 ) ;
#44216 = DIRECTION ( 'NONE',  ( 0.2920631208464286588, 0.8487660001727255210, 0.4407895307198632651 ) ) ;
#44217 = CARTESIAN_POINT ( 'NONE',  ( -13.07751017357372447, 15.00000000000000000, -6.263284095430686094 ) ) ;
#44218 = CARTESIAN_POINT ( 'NONE',  ( 0.5774900079438607392, 48.48035201082150536, 5.440088680355550821 ) ) ;
#44219 = ORIENTED_EDGE ( 'NONE', *, *, #85750, .T. ) ;
#44220 = CARTESIAN_POINT ( 'NONE',  ( -9.705452947461587598, 2.500000000000008438, -5.689172442861014645 ) ) ;
#44221 = CARTESIAN_POINT ( 'NONE',  ( 17.96484262340118221, 9.938685344154837509, 7.964842623401181321 ) ) ;
#44223 = CARTESIAN_POINT ( 'NONE',  ( 17.96484262340118221, 39.93868534415484106, 7.964842623401181321 ) ) ;
#44222 = CARTESIAN_POINT ( 'NONE',  ( 0.1532563361054100626, 60.80059781766744464, -2.638427012816831230 ) ) ;
#44224 = CARTESIAN_POINT ( 'NONE',  ( 1.821158202401649051, 16.16688879859530559, 6.499999999999976019 ) ) ;
#44225 = CARTESIAN_POINT ( 'NONE',  ( 20.88017736071110875, 60.77201867748817676, -2.915334737309920765 ) ) ;
#44226 = CARTESIAN_POINT ( 'NONE',  ( -13.78891971893212443, 0.5000000000000004441, 5.904717858191433244 ) ) ;
#44228 = CARTESIAN_POINT ( 'NONE',  ( 17.35999999999999943, 33.99999999999997158, 10.00000000000000000 ) ) ;
#44227 = CARTESIAN_POINT ( 'NONE',  ( 12.91533473730992121, 29.52201867748817321, 10.88017736071110164 ) ) ;
#44229 = CARTESIAN_POINT ( 'NONE',  ( 10.00000000000000178, 7.258931151000785675, 9.846743663894594434 ) ) ;
#44230 = CARTESIAN_POINT ( 'NONE',  ( 17.20831665107776587, 22.88393115100078745, 7.208316651077764980 ) ) ;
#44231 = CYLINDRICAL_SURFACE ( 'NONE', #84111, 0.2500000000000002220 ) ;
#44232 = CARTESIAN_POINT ( 'NONE',  ( 3.795296366450314540, 23.26208216824728936, 14.16423886937410082 ) ) ;
#44233 = CARTESIAN_POINT ( 'NONE',  ( 14.92337183194729988, 59.34226448433412315, -8.527530157486177487 ) ) ;
#44234 = CIRCLE ( 'NONE', #1165, 14.49999999999999822 ) ;
#44235 = CARTESIAN_POINT ( 'NONE',  ( 17.08211943468705130, 63.47041550158063927, 12.26659068614894998 ) ) ;
#44236 = DIRECTION ( 'NONE',  ( 0.000000000000000000, -1.000000000000000000, 0.000000000000000000 ) ) ;
#44237 = CARTESIAN_POINT ( 'NONE',  ( 2.917880565312948704, 7.637082168247301794, 12.26659068614894643 ) ) ;
#44238 = EDGE_CURVE ( 'NONE', #61056, #77111, #60587, .T. ) ;
#44239 = CARTESIAN_POINT ( 'NONE',  ( -0.3689425029237881626, 52.42874883491396076, 10.36894250292379027 ) ) ;
#44240 = CARTESIAN_POINT ( 'NONE',  ( 3.591859063236763294, -1.709698663402913210, -11.09922568453595026 ) ) ;
#44241 = ORIENTED_EDGE ( 'NONE', *, *, #10969, .F. ) ;
#44242 = CARTESIAN_POINT ( 'NONE',  ( 7.361572987183169658, 9.967264484334119601, -9.846743663894592657 ) ) ;
#44243 = CARTESIAN_POINT ( 'NONE',  ( 4.559911319644449179, 17.23035201082150536, -9.422509992056141925 ) ) ;
#44244 = EDGE_CURVE ( 'NONE', #6749, #1572, #78018, .T. ) ;
#44245 = CARTESIAN_POINT ( 'NONE',  ( 18.52753015748617571, 53.09226448433412315, 4.923371831947298993 ) ) ;
#44247 = CARTESIAN_POINT ( 'NONE',  ( -13.87912815710419068, 90.90967772850538609, -7.772688653987088969 ) ) ;
#44246 = CARTESIAN_POINT ( 'NONE',  ( 20.30776406404399026, 0.000000000000000000, 6.000000000000280664 ) ) ;
#44248 = CARTESIAN_POINT ( 'NONE',  ( 20.15039907845753220, 30.60158574516642815, -6.262539305110077947 ) ) ;
#44249 = AXIS2_PLACEMENT_3D ( 'NONE', #62334, #69862, #887 ) ;
#44250 =( NAMED_UNIT ( * ) SI_UNIT ( $, .STERADIAN. ) SOLID_ANGLE_UNIT ( ) );
#44251 = CARTESIAN_POINT ( 'NONE',  ( 16.40814093676324603, 22.45696800326375353, -11.09922568453594671 ) ) ;
#44252 = CARTESIAN_POINT ( 'NONE',  ( 1.472469842513823179, 25.59226448433412315, -4.923371831947296329 ) ) ;
#44253 = ORIENTED_EDGE ( 'NONE', *, *, #74171, .T. ) ;
#44254 = CARTESIAN_POINT ( 'NONE',  ( 10.00000000000000178, 2.258931151000784787, 9.846743663894594434 ) ) ;
#44255 = CARTESIAN_POINT ( 'NONE',  ( 11.35644985442049659, -65.08036738587416892, -3.750000000000000000 ) ) ;
#44256 = CARTESIAN_POINT ( 'NONE',  ( 5.500000000000000000, 11.00000000000000000, -6.000000000000000000 ) ) ;
#44257 = CARTESIAN_POINT ( 'NONE',  ( 2.035157376598822676, 12.43868534415483751, -7.964842623401177768 ) ) ;
#44258 = CARTESIAN_POINT ( 'NONE',  ( 17.08211943468705130, 43.47041550158063927, 12.26659068614894998 ) ) ;
#44259 = CARTESIAN_POINT ( 'NONE',  ( 20.88017736071110519, 65.56368534415483396, 2.639326808657452039E-16 ) ) ;
#44260 = CARTESIAN_POINT ( 'NONE',  ( 0.1532563361054082862, 21.21726448433412315, 2.638427012816831674 ) ) ;
#44261 = CARTESIAN_POINT ( 'NONE',  ( 0.5774900079438590739, 2.647018677488170990, -5.440088680355550821 ) ) ;
#44262 = CARTESIAN_POINT ( 'NONE',  ( 1.472469842513823179, 11.42559781766745175, 4.923371831947296329 ) ) ;
#44263 = CARTESIAN_POINT ( 'NONE',  ( -1.028725271592155099, -1.208271517246092823E-15, 4.540618777627624780 ) ) ;
#44264 = CARTESIAN_POINT ( 'NONE',  ( 12.63842701281683034, 42.46726448433412315, 9.846743663894596210 ) ) ;
#44265 = ADVANCED_FACE ( 'NONE', ( #82100 ), #97631, .F. ) ;
#44266 = CARTESIAN_POINT ( 'NONE',  ( 19.42250999205614548, 30.98035201082150536, -5.440088680355545492 ) ) ;
#44267 = TOROIDAL_SURFACE ( 'NONE', #57041, 14.49999999999999822, 0.5000000000000000000 ) ;
#44268 = ORIENTED_EDGE ( 'NONE', *, *, #62519, .T. ) ;
#44269 = CARTESIAN_POINT ( 'NONE',  ( -1.099225684535947600, 58.70696800326375353, -6.408140936763238038 ) ) ;
#44271 = EDGE_CURVE ( 'NONE', #42121, #94488, #45146, .T. ) ;
#44270 = FACE_OUTER_BOUND ( 'NONE', #27668, .T. ) ;
#44272 = CARTESIAN_POINT ( 'NONE',  ( 7.361572987183169658, 14.96726448433411960, -9.846743663894592657 ) ) ;
#44273 = CARTESIAN_POINT ( 'NONE',  ( 10.00000000000000178, 40.37363466993042493, 12.81628187352647608 ) ) ;
#44275 = CARTESIAN_POINT ( 'NONE',  ( 1.472469842513823179, 30.59226448433411960, -4.923371831947296329 ) ) ;
#44274 = CARTESIAN_POINT ( 'NONE',  ( 4.559911319644449179, 3.897018677488171434, 9.422509992056141925 ) ) ;
#44276 = CARTESIAN_POINT ( 'NONE',  ( 20.00000000000001066, 82.60888403405834879, 4.637569772578755689 ) ) ;
#44277 = STYLED_ITEM ( 'NONE', ( #35487 ), #89872 ) ;
#44278 = CARTESIAN_POINT ( 'NONE',  ( 0.000000000000000000, 15.00000000000000000, 0.000000000000000000 ) ) ;
#44279 = CARTESIAN_POINT ( 'NONE',  ( 2.917880565312948704, 22.63708216824730002, 12.26659068614894643 ) ) ;
#44280 = CARTESIAN_POINT ( 'NONE',  ( 22.26659068614894466, 48.88708216824730357, 7.082119434687054849 ) ) ;
#44281 = CARTESIAN_POINT ( 'NONE',  ( 17.20831665107776587, 42.88393115100077324, 7.208316651077764980 ) ) ;
#44282 = CARTESIAN_POINT ( 'NONE',  ( 32.56412365047463453, 26.99999999999998224, -9.500000000000000000 ) ) ;
#44283 = CARTESIAN_POINT ( 'NONE',  ( 15.44008868035555260, 44.73035201082151247, 9.422509992056143702 ) ) ;
#44284 = EDGE_CURVE ( 'NONE', #1757, #32864, #18035, .T. ) ;
#44285 = CARTESIAN_POINT ( 'NONE',  ( 12.91533473730993009, 66.60535201082150536, -10.88017736071109987 ) ) ;
#44286 = ORIENTED_EDGE ( 'NONE', *, *, #18061, .F. ) ;
#44287 = CARTESIAN_POINT ( 'NONE',  ( 10.00000000000000000, 52.87363466993041783, -12.81628187352647608 ) ) ;
#44288 = ORIENTED_EDGE ( 'NONE', *, *, #8687, .T. ) ;
#44289 = CARTESIAN_POINT ( 'NONE',  ( 0.5774900079438607392, 68.48035201082150536, 5.440088680355550821 ) ) ;
#44290 = ORIENTED_EDGE ( 'NONE', *, *, #25922, .F. ) ;
#44291 = CARTESIAN_POINT ( 'NONE',  ( 22.26659068614895176, 9.720415501580633943, -7.082119434687042414 ) ) ;
#44292 = CARTESIAN_POINT ( 'NONE',  ( 12.63842701281683922, 9.550597817667449974, -9.846743663894590881 ) ) ;
#44293 = CIRCLE ( 'NONE', #25194, 0.2500000000000002220 ) ;
#44294 = CARTESIAN_POINT ( 'NONE',  ( -0.1503990784575242878, 59.24884699246888431, -6.262539305110083276 ) ) ;
#44295 = ORIENTED_EDGE ( 'NONE', *, *, #75311, .F. ) ;
#44296 = CIRCLE ( 'NONE', #90609, 0.5000000000000004441 ) ;
#44297 = CARTESIAN_POINT ( 'NONE',  ( 0.5774900079438607392, 13.48035201082150358, 5.440088680355550821 ) ) ;
#44298 = VERTEX_POINT ( 'NONE', #52107 ) ;
#44299 = CARTESIAN_POINT ( 'NONE',  ( 7.084665262690076126, 39.10535201082150536, 10.88017736071109987 ) ) ;
#44300 = CARTESIAN_POINT ( 'NONE',  ( 20.15039907845753220, 55.60158574516643171, -6.262539305110077947 ) ) ;
#44301 = VERTEX_POINT ( 'NONE', #59100 ) ;
#44302 = CARTESIAN_POINT ( 'NONE',  ( 1.472469842513823179, 66.42559781766745175, 4.923371831947296329 ) ) ;
#44303 = EDGE_LOOP ( 'NONE', ( #96615, #85731, #12318, #86459, #44926, #90014 ) ) ;
#44304 = CARTESIAN_POINT ( 'NONE',  ( -0.8801773607110991993, 67.85535201082151957, -2.915334737309923874 ) ) ;
#44305 = CARTESIAN_POINT ( 'NONE',  ( 2.120353041430647068, 15.00000000000000000, -14.34413130794945523 ) ) ;
#44306 = CARTESIAN_POINT ( 'NONE',  ( -2.816281873526473856, 39.12363466993041783, 9.499525473075851096E-16 ) ) ;
#44308 = CARTESIAN_POINT ( 'NONE',  ( -0.1042174387088606602, 58.10736173766205326, 6.337391062633418670 ) ) ;
#44307 = CARTESIAN_POINT ( 'NONE',  ( 2.035157376598824452, 23.68868534415484461, 7.964842623401179544 ) ) ;
#44309 = CARTESIAN_POINT ( 'NONE',  ( 14.92337183194729633, 7.675597817667451750, 8.527530157486181039 ) ) ;
#44310 = CARTESIAN_POINT ( 'NONE',  ( 20.88017736071110164, 15.35535201082150358, 2.915334737309930979 ) ) ;
#44311 = EDGE_CURVE ( 'NONE', #59298, #69763, #53085, .T. ) ;
#44312 =( BOUNDED_SURFACE ( )  B_SPLINE_SURFACE ( 3, 2, ( 
 ( #32282, #47788, #62290 ),
 ( #86784, #85306, #47289 ),
 ( #25791, #93289, #70807 ),
 ( #1341, #2324, #9301 ),
 ( #93781, #46804, #48275 ),
 ( #41301, #64248, #78788 ),
 ( #56288, #39811, #70313 ),
 ( #55289, #10294, #71774 ),
 ( #94765, #40793, #18286 ),
 ( #48767, #1829, #79274 ),
 ( #16320, #84813, #77296 ),
 ( #39320, #69817, #31792 ),
 ( #19260, #65232, #87258 ),
 ( #18782, #3785, #65732 ),
 ( #56764, #95250, #96259 ),
 ( #79765, #64738, #4763 ),
 ( #20248, #73727, #20743 ),
 ( #4270, #81718, #28233 ) ),
 .UNSPECIFIED., .F., .F., .F. ) 
 B_SPLINE_SURFACE_WITH_KNOTS ( ( 4, 2, 2, 2, 2, 2, 2, 2, 4 ),
 ( 3, 3 ),
 ( 0.000000000000000000, 0.001371970262341174959, 0.002743940524682349918, 0.004115910787023524878, 0.005487881049364699837, 0.006859851311705874796, 0.008231821574047049755, 0.009603791836388224715, 0.01097576209872939967 ),
 ( 0.000000000000000000, 1.000000000000000000 ),
 .UNSPECIFIED. ) 
 GEOMETRIC_REPRESENTATION_ITEM ( )  RATIONAL_B_SPLINE_SURFACE ( (
 ( 1.000000000000000000, 0.7071067811865475727, 1.000000000000000000),
 ( 1.000000000000000000, 0.7072982590433614103, 1.000000000000000000),
 ( 1.000000000000000000, 0.7113498972295660971, 1.000000000000000000),
 ( 1.000000000000000000, 0.7257703676791772418, 1.000000000000000000),
 ( 1.000000000000000000, 0.7362840324263598690, 1.000000000000000000),
 ( 1.000000000000000000, 0.7606319170830569965, 1.000000000000000000),
 ( 1.000000000000000000, 0.7745485803766045674, 1.000000000000000000),
 ( 1.000000000000000000, 0.8036690257212466548, 1.000000000000000000),
 ( 1.000000000000000000, 0.8185245023542137011, 1.000000000000000000),
 ( 1.000000000000000000, 0.8475516512718134221, 1.000000000000000000),
 ( 1.000000000000000000, 0.8617420886046480710, 1.000000000000000000),
 ( 1.000000000000000000, 0.8886174597630145389, 1.000000000000000000),
 ( 1.000000000000000000, 0.9010211234293969973, 1.000000000000000000),
 ( 1.000000000000000000, 0.9233336449993967410, 1.000000000000000000),
 ( 1.000000000000000000, 0.9332564696566055806, 1.000000000000000000),
 ( 1.000000000000000000, 0.9500370447729021839, 1.000000000000000000),
 ( 1.000000000000000000, 0.9567390024732228548, 1.000000000000000000),
 ( 1.000000000000000000, 0.9611621933234234527, 1.000000000000000000) ) ) 
 REPRESENTATION_ITEM ( '' )  SURFACE ( )  );
#44313 = ORIENTED_EDGE ( 'NONE', *, *, #24514, .F. ) ;
#44314 = CARTESIAN_POINT ( 'NONE',  ( 0.6178305044545838731, 49.74863466993041072, 9.382169495545420901 ) ) ;
#44315 = CARTESIAN_POINT ( 'NONE',  ( 12.91533473730992121, 49.52201867748817676, 10.88017736071110164 ) ) ;
#44316 = CARTESIAN_POINT ( 'NONE',  ( -46.94000000000001904, 100.8832200551275662, -8.297377427090140145 ) ) ;
#44317 = CARTESIAN_POINT ( 'NONE',  ( -2.816281873526471635, 53.91530133659709634, -3.434112377981056508 ) ) ;
#44318 = CARTESIAN_POINT ( 'NONE',  ( 7.084665262690076126, 44.10535201082151247, 10.88017736071109987 ) ) ;
#44319 = CIRCLE ( 'NONE', #6013, 99.50000000000000000 ) ;
#44320 = CARTESIAN_POINT ( 'NONE',  ( 7.361572987183169658, 54.96726448433413026, -9.846743663894592657 ) ) ;
#44321 = DIRECTION ( 'NONE',  ( 8.659560562354946417E-17, 0.7071067811865465735, -0.7071067811865485719 ) ) ;
#44322 = CARTESIAN_POINT ( 'NONE',  ( 17.20831665107776587, 12.88393115100078390, 7.208316651077764980 ) ) ;
#44323 = CARTESIAN_POINT ( 'NONE',  ( 0.6178305044545838731, 9.748634669930416052, 9.382169495545420901 ) ) ;
#44325 = CARTESIAN_POINT ( 'NONE',  ( 5.076628168052703671, 61.84226448433412315, 8.527530157486179263 ) ) ;
#44324 = DIRECTION ( 'NONE',  ( -0.000000000000000000, 0.000000000000000000, 1.000000000000000000 ) ) ;
#44326 = CARTESIAN_POINT ( 'NONE',  ( 0.5774900079438590739, 37.64701867748817676, -5.440088680355550821 ) ) ;
#44327 = CARTESIAN_POINT ( 'NONE',  ( 14.92337183194729633, 52.67559781766745175, 8.527530157486181039 ) ) ;
#44328 = CARTESIAN_POINT ( 'NONE',  ( 18.52753015748617571, 3.092264484334118269, 4.923371831947298993 ) ) ;
#44330 = ORIENTED_EDGE ( 'NONE', *, *, #31257, .T. ) ;
#44329 = CARTESIAN_POINT ( 'NONE',  ( -1.099225684535947600, 3.706968003263753531, -6.408140936763238038 ) ) ;
#44331 = AXIS2_PLACEMENT_3D ( 'NONE', #28053, #29032, #52531 ) ;
#44332 = FILL_AREA_STYLE_COLOUR ( '', #41310 ) ;
#44333 = FILL_AREA_STYLE_COLOUR ( '', #66182 ) ;
#44334 = CARTESIAN_POINT ( 'NONE',  ( 2.791683348922240793, 61.63393115100079456, 7.208316651077764092 ) ) ;
#44335 = CARTESIAN_POINT ( 'NONE',  ( 22.81628187352647785, 46.62363466993041783, 6.195893100308588602E-16 ) ) ;
#44336 = CARTESIAN_POINT ( 'NONE',  ( 0.1532563361054082862, 36.21726448433410894, 2.638427012816831674 ) ) ;
#44337 = DIRECTION ( 'NONE',  ( 0.6186827199538547095, 0.6777609120375008844, 0.3973308925122679969 ) ) ;
#44338 = CARTESIAN_POINT ( 'NONE',  ( -0.8801773607111008646, 8.272018677488171434, 2.915334737309923430 ) ) ;
#44339 = CARTESIAN_POINT ( 'NONE',  ( 14.92337183194729988, 29.34226448433411960, -8.527530157486177487 ) ) ;
#44340 = EDGE_CURVE ( 'NONE', #91116, #75439, #83596, .T. ) ;
#44341 = CARTESIAN_POINT ( 'NONE',  ( 0.6081133539230648699, 18.33703382326400089, 6.500000000000005329 ) ) ;
#44342 = CARTESIAN_POINT ( 'NONE',  ( 4.559911319644449179, 7.230352010821505360, -9.422509992056141925 ) ) ;
#44343 = CARTESIAN_POINT ( 'NONE',  ( -9.886043635230025828, 89.00072246145502675, -5.688751881067946492 ) ) ;
#44344 = CARTESIAN_POINT ( 'NONE',  ( 15.44008868035555260, 14.73035201082150536, 9.422509992056143702 ) ) ;
#44346 = AXIS2_PLACEMENT_3D ( 'NONE', #87695, #50695, #65185 ) ;
#44345 = CARTESIAN_POINT ( 'NONE',  ( 20.36894250292379738, 44.92874883491396787, -10.36894250292379027 ) ) ;
#44348 = FACE_OUTER_BOUND ( 'NONE', #79909, .T. ) ;
#44347 = CARTESIAN_POINT ( 'NONE',  ( -4.164238869374099039, 56.80374883491397497, 8.674139862899312516E-16 ) ) ;
#44349 = DIRECTION ( 'NONE',  ( 0.000000000000000000, -1.000000000000000000, 0.000000000000000000 ) ) ;
#44350 = CARTESIAN_POINT ( 'NONE',  ( 12.63842701281683922, 14.55059781766744997, -9.846743663894590881 ) ) ;
#44351 = CARTESIAN_POINT ( 'NONE',  ( -2.816281873526471635, -1.084698663402913210, -3.434112377981056508 ) ) ;
#44352 = AXIS2_PLACEMENT_3D ( 'NONE', #96899, #81859, #51870 ) ;
#44353 = EDGE_LOOP ( 'NONE', ( #33553, #33717, #47966, #622, #7301, #85995, #13451, #30314 ) ) ;
#44354 = CARTESIAN_POINT ( 'NONE',  ( 0.2751277870542909176, 64.36607318730132477, -6.499999999999992006 ) ) ;
#44355 = CARTESIAN_POINT ( 'NONE',  ( 5.076628168052704559, 55.17559781766745175, -8.527530157486179263 ) ) ;
#44357 = CARTESIAN_POINT ( 'NONE',  ( 3.195792623639526653, 3.229976035794172695, -11.92686044187656336 ) ) ;
#44356 = VECTOR ( 'NONE', #29715, 1000.000000000000000 ) ;
#44358 = AXIS2_PLACEMENT_3D ( 'NONE', #62602, #17629, #38646 ) ;
#44359 = CARTESIAN_POINT ( 'NONE',  ( 5.076628168052703671, 66.84226448433412315, 8.527530157486179263 ) ) ;
#44360 = CARTESIAN_POINT ( 'NONE',  ( -0.3689425029237898834, 6.178748834913968757, -10.36894250292378850 ) ) ;
#44361 = CARTESIAN_POINT ( 'NONE',  ( 12.63842701281683922, 24.55059781766745175, -9.846743663894590881 ) ) ;
#44362 = CARTESIAN_POINT ( 'NONE',  ( 13.99999999999999822, 11.50000000000000000, 6.500000000000000888 ) ) ;
#44363 = ORIENTED_EDGE ( 'NONE', *, *, #5326, .T. ) ;
#44364 = CARTESIAN_POINT ( 'NONE',  ( 2.917880565312950480, 45.97041550158063927, -12.26659068614894821 ) ) ;
#44365 = ADVANCED_FACE ( 'NONE', ( #76084 ), #38107, .T. ) ;
#44366 = EDGE_CURVE ( 'NONE', #87849, #43677, #26028, .T. ) ;
#44367 = CARTESIAN_POINT ( 'NONE',  ( 12.63842701281683034, 7.467264484334118713, 9.846743663894596210 ) ) ;
#44369 = CARTESIAN_POINT ( 'NONE',  ( -2.258855624577434718, 0.04962891015807079781, -14.57926203528953657 ) ) ;
#44368 = FACE_OUTER_BOUND ( 'NONE', #9278, .T. ) ;
#44370 = CARTESIAN_POINT ( 'NONE',  ( 7.084665262690076126, 32.02201867748816966, -10.88017736071110164 ) ) ;
#44371 = CARTESIAN_POINT ( 'NONE',  ( 10.00000000000000178, 40.37363466993042493, 12.81628187352647608 ) ) ;
#44372 =( NAMED_UNIT ( * ) PLANE_ANGLE_UNIT ( ) SI_UNIT ( $, .RADIAN. ) );
#44373 = CARTESIAN_POINT ( 'NONE',  ( 19.38216949554541557, 37.24863466993041783, -9.382169495545420901 ) ) ;
#44374 = CARTESIAN_POINT ( 'NONE',  ( -2.816281873526473856, 59.33196800326374643, 3.434112377981055619 ) ) ;
#44375 = EDGE_LOOP ( 'NONE', ( #14454, #89639, #49472, #27206 ) ) ;
#44376 = CARTESIAN_POINT ( 'NONE',  ( 1.711636803080557767, 11.84492782695770607, -6.500000000000021316 ) ) ;
#44377 = LINE ( 'NONE', #94060, #79741 ) ;
#44378 = CARTESIAN_POINT ( 'NONE',  ( 13.79529636645031943, 35.34541550158063927, -14.16423886937409904 ) ) ;
#44379 =( NAMED_UNIT ( * ) SI_UNIT ( $, .STERADIAN. ) SOLID_ANGLE_UNIT ( ) );
#44380 = CARTESIAN_POINT ( 'NONE',  ( 4.559911319644449179, 8.897018677488171434, 9.422509992056141925 ) ) ;
#44381 = CARTESIAN_POINT ( 'NONE',  ( 7.084665262690076126, 19.10535201082150181, 10.88017736071109987 ) ) ;
#44382 = DIRECTION ( 'NONE',  ( -0.000000000000000000, 1.000000000000000000, -0.000000000000000000 ) ) ;
#44383 = PRESENTATION_STYLE_ASSIGNMENT (( #13898 ) ) ;
#44384 = CARTESIAN_POINT ( 'NONE',  ( 10.00000000000000000, 56.81368534415484106, -10.88017736071110342 ) ) ;
#44385 = CARTESIAN_POINT ( 'NONE',  ( 2.035157376598822676, 57.43868534415484106, -7.964842623401177768 ) ) ;
#44386 = CARTESIAN_POINT ( 'NONE',  ( 3.591859063236763294, 28.29030133659708568, -11.09922568453595026 ) ) ;
#44387 = DIRECTION ( 'NONE',  ( -0.000000000000000000, -1.000000000000000000, -0.000000000000000000 ) ) ;
#44388 = DIRECTION ( 'NONE',  ( 0.000000000000000000, 0.000000000000000000, 1.000000000000000000 ) ) ;
#44389 = CARTESIAN_POINT ( 'NONE',  ( 5.076628168052703671, 26.84226448433411960, 8.527530157486179263 ) ) ;
#44390 = CARTESIAN_POINT ( 'NONE',  ( 0.5774900079438607392, 53.48035201082151247, 5.440088680355550821 ) ) ;
#44391 = CARTESIAN_POINT ( 'NONE',  ( 10.00000000000000178, 20.37363466993042138, 12.81628187352647608 ) ) ;
#44392 = CARTESIAN_POINT ( 'NONE',  ( 10.00000000000000000, 11.81368534415483751, -10.88017736071110342 ) ) ;
#44393 = CARTESIAN_POINT ( 'NONE',  ( 12.63842701281683034, 37.46726448433411605, 9.846743663894596210 ) ) ;
#44394 = CARTESIAN_POINT ( 'NONE',  ( 19.38216949554541557, 42.24863466993041783, -9.382169495545420901 ) ) ;
#44395 = CARTESIAN_POINT ( 'NONE',  ( 19.84674366389459266, 13.30059781766745353, 2.638427012816836559 ) ) ;
#44396 = CARTESIAN_POINT ( 'NONE',  ( -0.3689425029237881626, 2.428748834913967869, 10.36894250292379027 ) ) ;
#44397 = LINE ( 'NONE', #6395, #86147 ) ;
#44398 = CARTESIAN_POINT ( 'NONE',  ( 4.559911319644449179, 23.89701867748817321, 9.422509992056141925 ) ) ;
#44399 = CARTESIAN_POINT ( 'NONE',  ( 24.16423886937409904, 34.09541550158064638, 3.795296366450317205 ) ) ;
#44400 = EDGE_CURVE ( 'NONE', #24676, #87709, #90077, .T. ) ;
#44401 = CARTESIAN_POINT ( 'NONE',  ( 14.92337183194729633, 47.67559781766745175, 8.527530157486181039 ) ) ;
#44402 = CARTESIAN_POINT ( 'NONE',  ( 10.00000000000000000, 31.81368534415483751, -10.88017736071110342 ) ) ;
#44403 = CARTESIAN_POINT ( 'NONE',  ( 12.91533473730993009, 11.60535201082150714, -10.88017736071109987 ) ) ;
#44404 = ORIENTED_EDGE ( 'NONE', *, *, #44925, .T. ) ;
#44405 = CARTESIAN_POINT ( 'NONE',  ( -0.8801773607110991993, 22.85535201082150181, -2.915334737309923874 ) ) ;
#44406 = CARTESIAN_POINT ( 'NONE',  ( 13.43411237798105340, 50.58196800326375353, 12.81628187352647963 ) ) ;
#44407 = CARTESIAN_POINT ( 'NONE',  ( 17.96484262340118221, 39.93868534415484106, 7.964842623401181321 ) ) ;
#44409 = CARTESIAN_POINT ( 'NONE',  ( 20.88017736071110164, 40.35535201082150536, 2.915334737309930979 ) ) ;
#44408 = FACE_OUTER_BOUND ( 'NONE', #91857, .T. ) ;
#44410 = AXIS2_PLACEMENT_3D ( 'NONE', #10001, #26952, #33456 ) ;
#44411 = ORIENTED_EDGE ( 'NONE', *, *, #74873, .F. ) ;
#44412 = CARTESIAN_POINT ( 'NONE',  ( 14.92337183194729988, 59.34226448433412315, -8.527530157486177487 ) ) ;
#44413 = CARTESIAN_POINT ( 'NONE',  ( 12.91533473730993009, 36.60535201082151247, -10.88017736071109987 ) ) ;
#44414 = CARTESIAN_POINT ( 'NONE',  ( 4.471658927162282637, -3.629165645957387554, 4.000000000000000000 ) ) ;
#44415 = DIRECTION ( 'NONE',  ( 1.000000000000000000, 0.000000000000000000, 0.000000000000000000 ) ) ;
#44416 = CARTESIAN_POINT ( 'NONE',  ( 17.08211943468705130, 53.47041550158063217, 12.26659068614894998 ) ) ;
#44417 = CARTESIAN_POINT ( 'NONE',  ( 4.559911319644449179, 47.23035201082150536, -9.422509992056141925 ) ) ;
#44418 = PLANE ( 'NONE',  #83331 ) ;
#44419 = DIRECTION ( 'NONE',  ( -0.000000000000000000, -0.000000000000000000, 1.000000000000000000 ) ) ;
#44420 = CARTESIAN_POINT ( 'NONE',  ( 17.20831665107776587, 57.88393115100078745, 7.208316651077764980 ) ) ;
#44421 = CARTESIAN_POINT ( 'NONE',  ( 10.00000000000000178, 22.25893115100078745, 9.846743663894594434 ) ) ;
#44422 = ORIENTED_EDGE ( 'NONE', *, *, #55341, .T. ) ;
#44423 = CARTESIAN_POINT ( 'NONE',  ( 14.92337183194729633, 17.67559781766745175, 8.527530157486181039 ) ) ;
#44424 = CARTESIAN_POINT ( 'NONE',  ( 6.408140936763243367, -24.20969866340290721, 11.09922568453594494 ) ) ;
#44425 = CARTESIAN_POINT ( 'NONE',  ( 20.88017736071110875, 20.77201867748816611, -2.915334737309920765 ) ) ;
#44426 = CARTESIAN_POINT ( 'NONE',  ( 12.63842701281683922, 19.55059781766745175, -9.846743663894590881 ) ) ;
#44427 = CARTESIAN_POINT ( 'NONE',  ( 17.39651004071838614, 47.93575266056826933, 6.500000000000032863 ) ) ;
#44428 = CARTESIAN_POINT ( 'NONE',  ( 22.81628187352647785, 11.62363466993042138, 6.195893100308588602E-16 ) ) ;
#44430 = CARTESIAN_POINT ( 'NONE',  ( -0.8801773607111008646, 63.27201867748817676, 2.915334737309923430 ) ) ;
#44429 = CARTESIAN_POINT ( 'NONE',  ( 2.603489959281614308, 36.58210964143329136, 6.500000000000031086 ) ) ;
#44432 = CARTESIAN_POINT ( 'NONE',  ( 21.09922568453595559, 62.04030133659709634, -6.408140936763230044 ) ) ;
#44431 = CARTESIAN_POINT ( 'NONE',  ( 19.42250999205614193, 30.14701867748817321, 5.440088680355555262 ) ) ;
#44433 = CARTESIAN_POINT ( 'NONE',  ( 22.26659068614894466, 38.88708216824731068, 7.082119434687054849 ) ) ;
#44434 = MECHANICAL_DESIGN_GEOMETRIC_PRESENTATION_REPRESENTATION (  '', ( #10892 ), #73188 ) ;
#44435 = AXIS2_PLACEMENT_3D ( 'NONE', #29526, #74546, #28057 ) ;
#44436 = CARTESIAN_POINT ( 'NONE',  ( -45.36634016833912852, 104.5847037719681936, 5.617347555694320427 ) ) ;
#44437 = VERTEX_POINT ( 'NONE', #25075 ) ;
#44438 = CARTESIAN_POINT ( 'NONE',  ( 6.565887622018943937, 18.08196800326375708, -12.81628187352647608 ) ) ;
#44439 = CARTESIAN_POINT ( 'NONE',  ( 12.91533473730992121, 4.522018677488169658, 10.88017736071110164 ) ) ;
#44440 = CARTESIAN_POINT ( 'NONE',  ( 20.88017736071110875, 45.77201867748816966, -2.915334737309920765 ) ) ;
#44441 = CARTESIAN_POINT ( 'NONE',  ( 9.879999999999988347, 26.99999999999999645, 2.900000000000000355 ) ) ;
#44442 = VERTEX_POINT ( 'NONE', #16578 ) ;
#44443 = VERTEX_POINT ( 'NONE', #24583 ) ;
#44444 = CARTESIAN_POINT ( 'NONE',  ( 10.00000000000000000, 51.81368534415484106, -10.88017736071110342 ) ) ;
#44445 = CARTESIAN_POINT ( 'NONE',  ( 17.20831665107776587, 34.13393115100078745, -7.208316651077762316 ) ) ;
#44446 = CARTESIAN_POINT ( 'NONE',  ( 17.20831665107776587, 19.13393115100078035, -7.208316651077762316 ) ) ;
#44447 = CARTESIAN_POINT ( 'NONE',  ( 5.076628168052703671, 11.84226448433411960, 8.527530157486179263 ) ) ;
#44448 = ADVANCED_FACE ( 'NONE', ( #54550 ), #33988, .F. ) ;
#44450 = CARTESIAN_POINT ( 'NONE',  ( -2.816281873526473856, 39.33196800326374643, 3.434112377981055619 ) ) ;
#44449 = CARTESIAN_POINT ( 'NONE',  ( -8.375939845167836850, 0.000000000000000000, 11.52849216984293257 ) ) ;
#44452 = DIRECTION ( 'NONE',  ( -0.000000000000000000, -1.000000000000000000, -0.000000000000000000 ) ) ;
#44451 = CARTESIAN_POINT ( 'NONE',  ( 20.88017736071110519, 65.56368534415483396, 2.639326808657452039E-16 ) ) ;
#44453 = CARTESIAN_POINT ( 'NONE',  ( 10.64411726291637450, -97.62798956704561704, 4.000000000000000000 ) ) ;
#44455 = ORIENTED_EDGE ( 'NONE', *, *, #5791, .F. ) ;
#44454 = CARTESIAN_POINT ( 'NONE',  ( 7.361572987183170547, 27.05059781766745175, 9.846743663894590881 ) ) ;
#44456 = CARTESIAN_POINT ( 'NONE',  ( -2.816281873526471635, 58.91530133659707502, -3.434112377981056508 ) ) ;
#44457 = CARTESIAN_POINT ( 'NONE',  ( 4.721516313243696139, -3.620689210586678364, 4.000000000000000000 ) ) ;
#44458 = CARTESIAN_POINT ( 'NONE',  ( 7.361572987183169658, 64.96726448433412315, -9.846743663894592657 ) ) ;
#44459 = CARTESIAN_POINT ( 'NONE',  ( 24.16423886937409904, 39.09541550158062506, 3.795296366450317205 ) ) ;
#44460 = B_SPLINE_CURVE_WITH_KNOTS ( 'NONE', 3,
 ( #98328, #14822, #37812, #60783 ),
 .UNSPECIFIED., .F., .F.,
 ( 4, 4 ),
 ( 4.878909776184769953E-19, 0.002657014572711323755 ),
 .UNSPECIFIED. ) ;
#44461 = UNCERTAINTY_MEASURE_WITH_UNIT (LENGTH_MEASURE( 1.000000000000000082E-05 ), #75827, 'distance_accuracy_value', 'NONE');
#44462 = CARTESIAN_POINT ( 'NONE',  ( -14.52844422123122747, -2.748198397366576661E-15, 1.683098224408205557 ) ) ;
#44463 = CARTESIAN_POINT ( 'NONE',  ( -2.266590686148945544, 27.22041550158063572, 7.082119434687048631 ) ) ;
#44464 = CARTESIAN_POINT ( 'NONE',  ( -2.266590686148945544, 47.22041550158063927, 7.082119434687048631 ) ) ;
#44465 = CARTESIAN_POINT ( 'NONE',  ( -0.3689425029237881626, 12.42874883491396609, 10.36894250292379027 ) ) ;
#44467 = CARTESIAN_POINT ( 'NONE',  ( -13.72545693419366764, 90.95708220729730442, -7.926564183086028059 ) ) ;
#44466 = CARTESIAN_POINT ( 'NONE',  ( 10.00000000000000178, 18.05374883491396787, 14.16423886937410082 ) ) ;
#44468 = CARTESIAN_POINT ( 'NONE',  ( 0.5774900079438590739, 42.64701867748816966, -5.440088680355550821 ) ) ;
#44469 = CARTESIAN_POINT ( 'NONE',  ( 14.64885433385999214, 0.04922511925147109862, 1.748475581354309583 ) ) ;
#44470 = CIRCLE ( 'NONE', #20500, 0.5000000000000004441 ) ;
#44471 = VERTEX_POINT ( 'NONE', #17074 ) ;
#44472 = CARTESIAN_POINT ( 'NONE',  ( 19.84674366389459266, 23.30059781766745530, 2.638427012816836559 ) ) ;
#44473 = EDGE_CURVE ( 'NONE', #39466, #7185, #20722, .T. ) ;
#44475 = CARTESIAN_POINT ( 'NONE',  ( 0.1532563361054100626, 30.80059781766744820, -2.638427012816831230 ) ) ;
#44474 = CARTESIAN_POINT ( 'NONE',  ( -46.44000000000001194, 93.00000000000000000, -9.500000000000000000 ) ) ;
#44476 = CARTESIAN_POINT ( 'NONE',  ( 19.42250999205614193, 25.14701867748817321, 5.440088680355555262 ) ) ;
#44477 = CARTESIAN_POINT ( 'NONE',  ( -2.816281873526471635, 58.91530133659707502, -3.434112377981056508 ) ) ;
#44478 = CARTESIAN_POINT ( 'NONE',  ( 5.076628168052703671, 46.84226448433412315, 8.527530157486179263 ) ) ;
#44479 = CARTESIAN_POINT ( 'NONE',  ( 19.38216949554541557, 47.24863466993041783, -9.382169495545420901 ) ) ;
#44480 = CARTESIAN_POINT ( 'NONE',  ( 10.36894250292378850, -15.07125116508603213, -10.36894250292379027 ) ) ;
#44481 = CIRCLE ( 'NONE', #84402, 15.00000000000000000 ) ;
#44482 = CARTESIAN_POINT ( 'NONE',  ( 12.91533473730993009, 36.60535201082151247, -10.88017736071109987 ) ) ;
#44483 = CARTESIAN_POINT ( 'NONE',  ( 5.076628168052704559, 45.17559781766745175, -8.527530157486179263 ) ) ;
#44484 = EDGE_CURVE ( 'NONE', #72885, #93468, #36714, .T. ) ;
#44485 = CARTESIAN_POINT ( 'NONE',  ( 6.204703633549690345, 22.84541550158062861, 14.16423886937410082 ) ) ;
#44486 = ORIENTED_EDGE ( 'NONE', *, *, #64388, .T. ) ;
#44487 = CARTESIAN_POINT ( 'NONE',  ( 17.99999999999999645, 91.28723161455539525, 8.000000000000000000 ) ) ;
#44488 = EDGE_CURVE ( 'NONE', #50168, #27600, #33476, .T. ) ;
#44489 = CARTESIAN_POINT ( 'NONE',  ( 17.96484262340118221, 66.18868534415483396, -7.964842623401177768 ) ) ;
#44490 = CARTESIAN_POINT ( 'NONE',  ( 3.420591144908583736, 14.49999999999999112, -14.60477854057961800 ) ) ;
#44491 = CARTESIAN_POINT ( 'NONE',  ( -4.164238869374099927, 57.01208216824731068, 3.795296366450308767 ) ) ;
#44492 = CARTESIAN_POINT ( 'NONE',  ( 7.361572987183170547, 62.05059781766745886, 9.846743663894590881 ) ) ;
#44493 = CARTESIAN_POINT ( 'NONE',  ( -0.8060400322138528972, 0.000000000000000000, -5.393339789881751223 ) ) ;
#44494 = CARTESIAN_POINT ( 'NONE',  ( 10.00000000000000000, 51.81368534415484106, -10.88017736071110342 ) ) ;
#44495 = CARTESIAN_POINT ( 'NONE',  ( 1.707155281725174945, 57.90189080397285437, 6.499999999999955591 ) ) ;
#44496 = STYLED_ITEM ( 'NONE', ( #37099 ), #13790 ) ;
#44497 = CARTESIAN_POINT ( 'NONE',  ( 5.440088680355556150, 24.73035201082151957, 9.422509992056138373 ) ) ;
#44498 = CARTESIAN_POINT ( 'NONE',  ( 0.5774900079438607392, 13.48035201082150358, 5.440088680355550821 ) ) ;
#44499 = CARTESIAN_POINT ( 'NONE',  ( 15.44008868035555793, 16.39701867748817321, -9.422509992056140149 ) ) ;
#44500 = CARTESIAN_POINT ( 'NONE',  ( 1.472469842513823179, 41.42559781766745886, 4.923371831947296329 ) ) ;
#44501 = CARTESIAN_POINT ( 'NONE',  ( 19.38216949554541557, 57.24863466993042493, -9.382169495545420901 ) ) ;
#44502 = CARTESIAN_POINT ( 'NONE',  ( -14.76100041229773296, 0.2306972965111885321, 2.313205896730730071 ) ) ;
#44503 = VERTEX_POINT ( 'NONE', #55557 ) ;
#44504 = CARTESIAN_POINT ( 'NONE',  ( 17.96484262340118221, 19.93868534415484106, 7.964842623401181321 ) ) ;
#44505 = CARTESIAN_POINT ( 'NONE',  ( 10.00000000000000178, 25.37363466993041783, 12.81628187352647608 ) ) ;
#44506 = CIRCLE ( 'NONE', #57269, 0.2500000000000002220 ) ;
#44507 = CARTESIAN_POINT ( 'NONE',  ( 0.1532563361054100626, 10.80059781766745175, -2.638427012816831230 ) ) ;
#44508 = CARTESIAN_POINT ( 'NONE',  ( 19.84674366389459621, 53.50893115100078745, 7.409399052514197653E-17 ) ) ;
#44509 = B_SPLINE_CURVE_WITH_KNOTS ( 'NONE', 3,
 ( #8725, #39243, #47208, #71211 ),
 .UNSPECIFIED., .F., .F.,
 ( 4, 4 ),
 ( 8.182674270850422113E-18, 0.002392975128318503269 ),
 .UNSPECIFIED. ) ;
#44510 = CARTESIAN_POINT ( 'NONE',  ( 19.42250999205614548, 35.98035201082151247, -5.440088680355545492 ) ) ;
#44511 = CARTESIAN_POINT ( 'NONE',  ( 21.09922568453595559, 12.04030133659708746, -6.408140936763230044 ) ) ;
#44513 = CARTESIAN_POINT ( 'NONE',  ( 6.432108699068924018, -88.20011490510430008, 2.500000000000000000 ) ) ;
#44512 = CARTESIAN_POINT ( 'NONE',  ( 12.91533473730993009, 51.60535201082149825, -10.88017736071109987 ) ) ;
#44514 = DIRECTION ( 'NONE',  ( -0.000000000000000000, -0.000000000000000000, -1.000000000000000000 ) ) ;
#44515 = CARTESIAN_POINT ( 'NONE',  ( 16.40814093676324603, 57.45696800326375353, -11.09922568453594671 ) ) ;
#44516 = EDGE_LOOP ( 'NONE', ( #58513, #83642, #86408, #92079, #81053, #33583 ) ) ;
#44517 = DIRECTION ( 'NONE',  ( 0.2164396139381103701, 0.000000000000000000, -0.9762960071199316969 ) ) ;
#44519 = CARTESIAN_POINT ( 'NONE',  ( -2.266590686148945544, 1.387082168247301128, -7.082119434687050408 ) ) ;
#44518 = CARTESIAN_POINT ( 'NONE',  ( 19.38216949554541557, 27.24863466993041783, -9.382169495545420901 ) ) ;
#44520 = EDGE_CURVE ( 'NONE', #76760, #96670, #9068, .T. ) ;
#44521 = CARTESIAN_POINT ( 'NONE',  ( 4.559911319644449179, 43.89701867748816966, 9.422509992056141925 ) ) ;
#44522 = CARTESIAN_POINT ( 'NONE',  ( 10.00000000000000178, 67.25893115100079456, 9.846743663894594434 ) ) ;
#44523 = CARTESIAN_POINT ( 'NONE',  ( 5.076628168052703671, 51.84226448433412315, 8.527530157486179263 ) ) ;
#44524 = CARTESIAN_POINT ( 'NONE',  ( 17.20831665107776587, 19.13393115100078035, -7.208316651077762316 ) ) ;
#44525 = CARTESIAN_POINT ( 'NONE',  ( 19.84674366389459621, 3.508931151000785231, 7.409399052514197653E-17 ) ) ;
#44526 =( NAMED_UNIT ( * ) PLANE_ANGLE_UNIT ( ) SI_UNIT ( $, .RADIAN. ) );
#44527 = CARTESIAN_POINT ( 'NONE',  ( 24.16423886937409904, 39.09541550158062506, 3.795296366450317205 ) ) ;
#44528 = CARTESIAN_POINT ( 'NONE',  ( 6.189940676892116578, 14.95037117674007021, -13.39186120659003265 ) ) ;
#44529 = MECHANICAL_DESIGN_GEOMETRIC_PRESENTATION_REPRESENTATION (  '', ( #39768 ), #73287 ) ;
#44530 = CARTESIAN_POINT ( 'NONE',  ( 8.992292137164646704, -4.149411823827444223, -3.749999999999999556 ) ) ;
#44531 = EDGE_CURVE ( 'NONE', #20984, #83910, #18667, .T. ) ;
#44532 = CARTESIAN_POINT ( 'NONE',  ( -6.857667818334720167, -50.95147662124758625, -4.000000000000000000 ) ) ;
#44533 = ORIENTED_EDGE ( 'NONE', *, *, #75097, .T. ) ;
#44534 = ORIENTED_EDGE ( 'NONE', *, *, #6237, .T. ) ;
#44535 = CARTESIAN_POINT ( 'NONE',  ( -2.266590686148945544, 56.38708216824731068, -7.082119434687050408 ) ) ;
#44536 = CARTESIAN_POINT ( 'NONE',  ( 2.917880565312950480, 60.97041550158063927, -12.26659068614894821 ) ) ;
#44537 = CARTESIAN_POINT ( 'NONE',  ( 10.00000000000000178, 32.25893115100078745, 9.846743663894594434 ) ) ;
#44538 = CARTESIAN_POINT ( 'NONE',  ( -1.099225684535947600, 24.54030133659708923, 6.408140936763237150 ) ) ;
#44539 = CARTESIAN_POINT ( 'NONE',  ( -4.431036607602381494, 14.63595249122789177, -14.33059365769917726 ) ) ;
#44541 = CARTESIAN_POINT ( 'NONE',  ( -4.164238869374098151, 1.595415501580634388, -3.795296366450310543 ) ) ;
#44540 = CARTESIAN_POINT ( 'NONE',  ( 8.879999999999995453, 41.24999999999999289, 4.250000000000000000 ) ) ;
#44542 = CARTESIAN_POINT ( 'NONE',  ( -0.8801773607111009756, 13.06368534415483929, 1.068504757029289695E-15 ) ) ;
#44543 = CARTESIAN_POINT ( 'NONE',  ( -0.3689425029237881626, 52.42874883491396076, 10.36894250292379027 ) ) ;
#44544 = CARTESIAN_POINT ( 'NONE',  ( 2.791683348922237240, 35.38393115100079456, -7.208316651077763204 ) ) ;
#44545 = DIRECTION ( 'NONE',  ( 0.000000000000000000, -1.000000000000000000, 0.000000000000000000 ) ) ;
#44546 = CARTESIAN_POINT ( 'NONE',  ( 14.92337183194729633, 22.67559781766745175, 8.527530157486181039 ) ) ;
#44547 = CARTESIAN_POINT ( 'NONE',  ( 8.879999999999991900, 69.99999999999998579, 4.000000000000000000 ) ) ;
#44548 = CARTESIAN_POINT ( 'NONE',  ( -4.923371831947292776, 16.84226448433412315, 8.527530157486181039 ) ) ;
#44549 = ORIENTED_EDGE ( 'NONE', *, *, #49046, .F. ) ;
#44550 = ORIENTED_EDGE ( 'NONE', *, *, #28799, .T. ) ;
#44551 = LINE ( 'NONE', #52545, #92464 ) ;
#44552 = VERTEX_POINT ( 'NONE', #10060 ) ;
#44553 = CARTESIAN_POINT ( 'NONE',  ( 19.84674366389459266, 48.71726448433413026, -2.638427012816827677 ) ) ;
#44555 = CARTESIAN_POINT ( 'NONE',  ( 10.00000000000000178, 44.31368534415484106, 10.88017736071110342 ) ) ;
#44554 = CARTESIAN_POINT ( 'NONE',  ( 17.96484262340118221, 14.93868534415484106, 7.964842623401181321 ) ) ;
#44557 = CARTESIAN_POINT ( 'NONE',  ( 3.591859063236763294, 23.29030133659708568, -11.09922568453595026 ) ) ;
#44556 = SURFACE_STYLE_FILL_AREA ( #23061 ) ;
#44558 = CARTESIAN_POINT ( 'NONE',  ( 22.26659068614894466, 8.887082168247300018, 7.082119434687054849 ) ) ;
#44559 = CARTESIAN_POINT ( 'NONE',  ( 19.42250999205614548, 65.98035201082151957, -5.440088680355545492 ) ) ;
#44560 = CARTESIAN_POINT ( 'NONE',  ( 21.09922568453594849, 26.20696800326375353, 6.408140936763242479 ) ) ;
#44561 = VERTEX_POINT ( 'NONE', #61565 ) ;
#44562 = CARTESIAN_POINT ( 'NONE',  ( 2.791683348922237240, 35.38393115100079456, -7.208316651077763204 ) ) ;
#44563 = CARTESIAN_POINT ( 'NONE',  ( 20.88017736071110875, 10.77201867748817143, -2.915334737309920765 ) ) ;
#44564 = EDGE_LOOP ( 'NONE', ( #49904, #81834, #52593, #62605, #28953, #18709 ) ) ;
#44565 = CARTESIAN_POINT ( 'NONE',  ( 24.16423886937410614, 64.30374883491396076, 8.672049930838204340E-16 ) ) ;
#44566 = ORIENTED_EDGE ( 'NONE', *, *, #12569, .T. ) ;
#44567 = CARTESIAN_POINT ( 'NONE',  ( 2.035157376598824452, 48.68868534415483396, 7.964842623401179544 ) ) ;
#44568 = CARTESIAN_POINT ( 'NONE',  ( 7.084665262690076126, 62.02201867748816966, -10.88017736071110164 ) ) ;
#44569 = VECTOR ( 'NONE', #27162, 1000.000000000000000 ) ;
#44571 = EDGE_CURVE ( 'NONE', #64978, #76530, #88222, .T. ) ;
#44570 = CARTESIAN_POINT ( 'NONE',  ( 0.5774900079438590739, 62.64701867748817676, -5.440088680355550821 ) ) ;
#44572 = CARTESIAN_POINT ( 'NONE',  ( 10.00000000000000178, 2.258931151000784787, 9.846743663894594434 ) ) ;
#44573 = CARTESIAN_POINT ( 'NONE',  ( 20.88017736071110164, 60.35535201082151957, 2.915334737309930979 ) ) ;
#44574 = DIRECTION ( 'NONE',  ( 1.000000000000000000, -0.000000000000000000, -0.000000000000000000 ) ) ;
#44575 = ADVANCED_FACE ( 'NONE', ( #32546 ), #31558, .F. ) ;
#44576 = CARTESIAN_POINT ( 'NONE',  ( 8.630000000000000782, -0.01512149801896540274, 4.000000000000000000 ) ) ;
#44577 = CARTESIAN_POINT ( 'NONE',  ( 19.84674366389459266, 23.71726448433412315, -2.638427012816827677 ) ) ;
#44578 = ORIENTED_EDGE ( 'NONE', *, *, #92796, .T. ) ;
#44579 = DIRECTION ( 'NONE',  ( 0.000000000000000000, 0.000000000000000000, 1.000000000000000000 ) ) ;
#44580 = LINE ( 'NONE', #607, #1446 ) ;
#44581 = CARTESIAN_POINT ( 'NONE',  ( 2.917880565312950480, 5.970415501580634832, -12.26659068614894821 ) ) ;
#44582 = ORIENTED_EDGE ( 'NONE', *, *, #37885, .T. ) ;
#44583 = CYLINDRICAL_SURFACE ( 'NONE', #50848, 0.2500000000000002220 ) ;
#44584 = FACE_OUTER_BOUND ( 'NONE', #52687, .T. ) ;
#44585 = CARTESIAN_POINT ( 'NONE',  ( 0.000000000000000000, 0.5000000000000004441, 0.000000000000000000 ) ) ;
#44586 = CARTESIAN_POINT ( 'NONE',  ( 15.44008868035555260, 9.730352010821505360, 9.422509992056143702 ) ) ;
#44587 = CARTESIAN_POINT ( 'NONE',  ( 34.56412365047463453, 26.99999999999999645, 10.00000000000000000 ) ) ;
#44588 = ORIENTED_EDGE ( 'NONE', *, *, #7044, .T. ) ;
#44589 =( BOUNDED_CURVE ( )  B_SPLINE_CURVE ( 3, ( #41362, #33800, #94818, #3837 ),
 .UNSPECIFIED., .F., .T. ) 
 B_SPLINE_CURVE_WITH_KNOTS ( ( 4, 4 ),
 ( 0.000000000000000000, 1.570796326794896558 ),
 .UNSPECIFIED. ) 
 CURVE ( )  GEOMETRIC_REPRESENTATION_ITEM ( )  RATIONAL_B_SPLINE_CURVE ( ( 1.000000000000000000, 0.8047378541243649375, 0.8047378541243649375, 1.000000000000000000 ) ) 
 REPRESENTATION_ITEM ( '' )  );
#44590 = DIRECTION ( 'NONE',  ( -1.000000000000000000, 0.000000000000000000, 0.000000000000000000 ) ) ;
#44591 = CARTESIAN_POINT ( 'NONE',  ( 1.472469842513823179, 41.42559781766745886, 4.923371831947296329 ) ) ;
#44592 = CARTESIAN_POINT ( 'NONE',  ( -13.07734668325347016, 15.00000000000000711, 6.551438809692819554 ) ) ;
#44593 = CARTESIAN_POINT ( 'NONE',  ( 16.40814093676324603, 22.45696800326375353, -11.09922568453594671 ) ) ;
#44594 = CARTESIAN_POINT ( 'NONE',  ( 17.20831665107776587, 9.133931151000787452, -7.208316651077762316 ) ) ;
#44595 = AXIS2_PLACEMENT_3D ( 'NONE', #15320, #37816, #45300 ) ;
#44596 = CARTESIAN_POINT ( 'NONE',  ( 1.042145700049398549, 29.74216108172003459, -6.499999999999841016 ) ) ;
#44597 = CARTESIAN_POINT ( 'NONE',  ( 10.00000000000000000, 19.75893115100078390, -9.846743663894594434 ) ) ;
#44598 = CARTESIAN_POINT ( 'NONE',  ( 16.40814093676323893, 0.7903013365970867898, 11.09922568453595026 ) ) ;
#44599 = CARTESIAN_POINT ( 'NONE',  ( 0.000000000000000000, -97.00000000000000000, 4.000000000000000000 ) ) ;
#44600 = EDGE_CURVE ( 'NONE', #39231, #70759, #48284, .T. ) ;
#44601 = ORIENTED_EDGE ( 'NONE', *, *, #24867, .T. ) ;
#44602 = VERTEX_POINT ( 'NONE', #38588 ) ;
#44603 = EDGE_CURVE ( 'NONE', #26347, #5105, #24406, .T. ) ;
#44604 = CARTESIAN_POINT ( 'NONE',  ( 15.44008868035555260, 24.73035201082150891, 9.422509992056143702 ) ) ;
#44605 = CARTESIAN_POINT ( 'NONE',  ( 20.36894250292379738, 24.92874883491396787, -10.36894250292379027 ) ) ;
#44606 = CARTESIAN_POINT ( 'NONE',  ( 17.20831665107776587, 24.13393115100078035, -7.208316651077762316 ) ) ;
#44607 = CARTESIAN_POINT ( 'NONE',  ( 15.44008868035555793, 51.39701867748816966, -9.422509992056140149 ) ) ;
#44608 = CARTESIAN_POINT ( 'NONE',  ( -2.816281873526471635, 33.91530133659708213, -3.434112377981056508 ) ) ;
#44609 = CARTESIAN_POINT ( 'NONE',  ( 19.42250999205614193, 10.14701867748816966, 5.440088680355555262 ) ) ;
#44610 = CARTESIAN_POINT ( 'NONE',  ( 0.6081133539230521023, 43.33703382326400089, 6.499999999999974243 ) ) ;
#44611 = CARTESIAN_POINT ( 'NONE',  ( 13.34343830728403724, 14.49999999999999112, 6.852200678592740068 ) ) ;
#44612 = AXIS2_PLACEMENT_3D ( 'NONE', #97501, #28965, #59468 ) ;
#44613 = CARTESIAN_POINT ( 'NONE',  ( 19.38216949554541202, 15.99863466993042138, 9.382169495545424454 ) ) ;
#44614 = CARTESIAN_POINT ( 'NONE',  ( 14.92337183194729988, 59.34226448433412315, -8.527530157486177487 ) ) ;
#44615 = CARTESIAN_POINT ( 'NONE',  ( 2.791683348922237240, 30.38393115100078390, -7.208316651077763204 ) ) ;
#44616 = CARTESIAN_POINT ( 'NONE',  ( 7.964842623401181321, -15.06131465584516071, 7.964842623401174215 ) ) ;
#44617 = CARTESIAN_POINT ( 'NONE',  ( 22.81628187352647785, 41.62363466993042493, 6.195893100308588602E-16 ) ) ;
#44618 = DIRECTION ( 'NONE',  ( 0.9961946980917462113, -0.08715574274765140739, 0.000000000000000000 ) ) ;
#44620 = DIRECTION ( 'NONE',  ( 0.8433914458128849434, -0.000000000000000000, 0.5372996083468249973 ) ) ;
#44619 = CARTESIAN_POINT ( 'NONE',  ( 0.5774900079438607392, 38.48035201082150536, 5.440088680355550821 ) ) ;
#44621 = AXIS2_PLACEMENT_3D ( 'NONE', #2601, #3082, #33055 ) ;
#44622 = FACE_OUTER_BOUND ( 'NONE', #51095, .T. ) ;
#44623 = CARTESIAN_POINT ( 'NONE',  ( -0.8801773607110991993, 67.85535201082151957, -2.915334737309923874 ) ) ;
#44624 = CARTESIAN_POINT ( 'NONE',  ( -0.8801773607111008646, 43.27201867748817676, 2.915334737309923430 ) ) ;
#44625 = CARTESIAN_POINT ( 'NONE',  ( -0.8801773607111009756, 38.06368534415484106, 1.068504757029289695E-15 ) ) ;
#44626 = CARTESIAN_POINT ( 'NONE',  ( 10.00000000000000000, 59.75893115100078745, -9.846743663894594434 ) ) ;
#44627 = CARTESIAN_POINT ( 'NONE',  ( 12.91533473730992121, 59.52201867748816966, 10.88017736071110164 ) ) ;
#44628 = EDGE_CURVE ( 'NONE', #35322, #93263, #69576, .T. ) ;
#44629 = CARTESIAN_POINT ( 'NONE',  ( 10.00000000000000000, 44.75893115100078745, -9.846743663894594434 ) ) ;
#44630 = CARTESIAN_POINT ( 'NONE',  ( 4.559911319644449179, 12.23035201082150536, -9.422509992056141925 ) ) ;
#44631 = CARTESIAN_POINT ( 'NONE',  ( 19.38216949554541557, 12.24863466993041961, -9.382169495545420901 ) ) ;
#44632 = VERTEX_POINT ( 'NONE', #8579 ) ;
#44633 = CARTESIAN_POINT ( 'NONE',  ( 7.084665262690076126, 22.02201867748817321, -10.88017736071110164 ) ) ;
#44634 = SURFACE_STYLE_USAGE ( .BOTH. , #29615 ) ;
#44635 = ADVANCED_FACE ( 'NONE', ( #69087 ), #85684, .T. ) ;
#44636 = CARTESIAN_POINT ( 'NONE',  ( 4.559911319644449179, 3.897018677488170990, 9.422509992056141925 ) ) ;
#44637 = CARTESIAN_POINT ( 'NONE',  ( 0.5774900079438607392, 33.48035201082150536, 5.440088680355550821 ) ) ;
#44638 = CARTESIAN_POINT ( 'NONE',  ( 12.63842701281683922, 4.550597817667451750, -9.846743663894590881 ) ) ;
#44639 = CARTESIAN_POINT ( 'NONE',  ( -2.266590686148945544, 32.22041550158063927, 7.082119434687048631 ) ) ;
#44640 = CARTESIAN_POINT ( 'NONE',  ( 14.92337183194729988, 9.342264484334119601, -8.527530157486177487 ) ) ;
#44641 = CARTESIAN_POINT ( 'NONE',  ( 7.084665262690076126, 52.02201867748816255, -10.88017736071110164 ) ) ;
#44642 = LINE ( 'NONE', #52633, #80984 ) ;
#44643 = CARTESIAN_POINT ( 'NONE',  ( 13.79529636645030344, 3.262082168247301350, 14.16423886937410614 ) ) ;
#44644 = ORIENTED_EDGE ( 'NONE', *, *, #63120, .T. ) ;
#44645 = CARTESIAN_POINT ( 'NONE',  ( -46.94000000000001194, 103.0000000000000000, 5.997726559847112782 ) ) ;
#44646 = CARTESIAN_POINT ( 'NONE',  ( 0.1532563361054100626, 55.80059781766745175, -2.638427012816831230 ) ) ;
#44647 = ORIENTED_EDGE ( 'NONE', *, *, #26992, .T. ) ;
#44648 = ORIENTED_EDGE ( 'NONE', *, *, #50981, .T. ) ;
#44649 = CARTESIAN_POINT ( 'NONE',  ( 20.36894250292379738, 24.92874883491396787, -10.36894250292379027 ) ) ;
#44650 = CARTESIAN_POINT ( 'NONE',  ( 13.79529636645031943, 25.34541550158063572, -14.16423886937409904 ) ) ;
#44651 = CARTESIAN_POINT ( 'NONE',  ( -0.8801773607110991993, 62.85535201082150536, -2.915334737309923874 ) ) ;
#44652 = CARTESIAN_POINT ( 'NONE',  ( 0.5774900079438607392, 3.480352010821504916, 5.440088680355550821 ) ) ;
#44653 = CARTESIAN_POINT ( 'NONE',  ( 22.81628187352648496, 1.831968003263753753, -3.434112377981050290 ) ) ;
#44654 = CARTESIAN_POINT ( 'NONE',  ( 0.1532563361054082862, 46.21726448433411605, 2.638427012816831674 ) ) ;
#44655 = CARTESIAN_POINT ( 'NONE',  ( -10.85644721466729123, -98.10785618530077556, 3.999999999999093614 ) ) ;
#44657 = CARTESIAN_POINT ( 'NONE',  ( 0.6178305044545818747, 8.498634669930421381, -9.382169495545419124 ) ) ;
#44656 = CARTESIAN_POINT ( 'NONE',  ( -0.8801773607111009756, 43.06368534415484106, 1.068504757029289695E-15 ) ) ;
#44658 = CARTESIAN_POINT ( 'NONE',  ( 17.08211943468705130, 13.47041550158063572, 12.26659068614894998 ) ) ;
#44659 = CARTESIAN_POINT ( 'NONE',  ( 20.88017736071110164, 10.35535201082150714, 2.915334737309930979 ) ) ;
#44660 = CARTESIAN_POINT ( 'NONE',  ( 10.00000000000000178, 14.31368534415483929, 10.88017736071110342 ) ) ;
#44661 = CARTESIAN_POINT ( 'NONE',  ( 20.15039907845753220, 17.62777174578612716, -6.262539305110077947 ) ) ;
#44662 = CARTESIAN_POINT ( 'NONE',  ( 2.035157376598824452, 38.68868534415483396, 7.964842623401179544 ) ) ;
#44663 = CARTESIAN_POINT ( 'NONE',  ( 2.638427012816835227, -22.53273551566587685, 9.846743663894590881 ) ) ;
#44664 = VERTEX_POINT ( 'NONE', #62055 ) ;
#44665 = DIRECTION ( 'NONE',  ( -0.9681476403781067441, 0.000000000000000000, -0.2503800040544454375 ) ) ;
#44666 = ORIENTED_EDGE ( 'NONE', *, *, #38242, .F. ) ;
#44667 = CARTESIAN_POINT ( 'NONE',  ( 5.076628168052703671, 31.84226448433412315, 8.527530157486179263 ) ) ;
#44668 = VECTOR ( 'NONE', #65327, 1000.000000000000000 ) ;
#44669 = ORIENTED_EDGE ( 'NONE', *, *, #24173, .F. ) ;
#44670 = DIRECTION ( 'NONE',  ( 1.483861936729427615E-16, -1.000000000000000000, 0.000000000000000000 ) ) ;
#44672 = CARTESIAN_POINT ( 'NONE',  ( 0.5774900079438590739, 2.647018677488171434, -5.440088680355550821 ) ) ;
#44671 = CARTESIAN_POINT ( 'NONE',  ( 24.16423886937409904, 49.09541550158063217, 3.795296366450317205 ) ) ;
#44674 = CARTESIAN_POINT ( 'NONE',  ( 12.63842701281683034, 42.46726448433412315, 9.846743663894596210 ) ) ;
#44673 = CARTESIAN_POINT ( 'NONE',  ( 19.84674366389459266, 28.30059781766745886, 2.638427012816836559 ) ) ;
#44675 = DIRECTION ( 'NONE',  ( 0.08715574274766037244, 0.9961946980917453232, -0.000000000000000000 ) ) ;
#44676 = COLOUR_RGB ( '', 0.31764706, 0.68627451, 0.89019608) ;
#44677 = CARTESIAN_POINT ( 'NONE',  ( 15.44008868035555793, 61.39701867748817676, -9.422509992056140149 ) ) ;
#44678 = CARTESIAN_POINT ( 'NONE',  ( 11.09922568453595026, 16.20696800326376064, 6.408140936763232709 ) ) ;
#44679 = ORIENTED_EDGE ( 'NONE', *, *, #39686, .F. ) ;
#44680 = CARTESIAN_POINT ( 'NONE',  ( 13.79529636645030344, 28.26208216824729647, 14.16423886937410614 ) ) ;
#44681 = CARTESIAN_POINT ( 'NONE',  ( 3.591859063236761518, 24.95696800326375353, 11.09922568453594849 ) ) ;
#44682 = VERTEX_POINT ( 'NONE', #34012 ) ;
#44683 = CARTESIAN_POINT ( 'NONE',  ( 3.591859063236763294, 63.29030133659708923, -11.09922568453595026 ) ) ;
#44684 = CARTESIAN_POINT ( 'NONE',  ( 20.88017736071110519, 25.56368534415483751, 2.639326808657452039E-16 ) ) ;
#44685 = CARTESIAN_POINT ( 'NONE',  ( 0.1532563361054100626, 35.80059781766745175, -2.638427012816831230 ) ) ;
#44686 = CARTESIAN_POINT ( 'NONE',  ( 2.035157376598822676, 32.43868534415483396, -7.964842623401177768 ) ) ;
#44687 = CARTESIAN_POINT ( 'NONE',  ( -2.816281873526473856, 64.12363466993042493, 9.499525473075851096E-16 ) ) ;
#44688 = CYLINDRICAL_SURFACE ( 'NONE', #60718, 0.5000000000000004441 ) ;
#44689 = CARTESIAN_POINT ( 'NONE',  ( 2.791683348922237240, 40.38393115100078035, -7.208316651077763204 ) ) ;
#44690 = CARTESIAN_POINT ( 'NONE',  ( 7.361572987183169658, 49.96726448433410894, -9.846743663894592657 ) ) ;
#44691 = ADVANCED_FACE ( 'NONE', ( #72508 ), #71772, .F. ) ;
#44693 = ORIENTED_EDGE ( 'NONE', *, *, #27032, .T. ) ;
#44692 = CARTESIAN_POINT ( 'NONE',  ( -7.750000000000000000, 41.24999999999999289, -6.250000000000000000 ) ) ;
#44694 = DIRECTION ( 'NONE',  ( -0.7253743710122820820, 0.000000000000000000, -0.6883545756937599069 ) ) ;
#44695 = CARTESIAN_POINT ( 'NONE',  ( -0.7166339456633684657, -0.03417435944610275333, 15.98010739087745868 ) ) ;
#44696 = CARTESIAN_POINT ( 'NONE',  ( 17.39651004071842522, 19.08210964143329491, -6.499999999999992895 ) ) ;
#44697 = DIRECTION ( 'NONE',  ( 0.000000000000000000, 0.000000000000000000, -1.000000000000000000 ) ) ;
#44698 = CARTESIAN_POINT ( 'NONE',  ( 12.63842701281683922, 14.55059781766744997, -9.846743663894590881 ) ) ;
#44699 = CARTESIAN_POINT ( 'NONE',  ( 34.56412365047464874, 11.99999999999999645, 7.000000000000000000 ) ) ;
#44700 = ORIENTED_EDGE ( 'NONE', *, *, #20467, .F. ) ;
#44701 = CARTESIAN_POINT ( 'NONE',  ( 14.92337183194729988, 59.34226448433412315, -8.527530157486177487 ) ) ;
#44702 = CARTESIAN_POINT ( 'NONE',  ( 7.361572987183170547, 37.05059781766744464, 9.846743663894590881 ) ) ;
#44703 = CARTESIAN_POINT ( 'NONE',  ( 24.16423886937409904, 34.09541550158064638, 3.795296366450317205 ) ) ;
#44704 = CARTESIAN_POINT ( 'NONE',  ( 1.472469842513823179, 40.59226448433411605, -4.923371831947296329 ) ) ;
#44705 = CARTESIAN_POINT ( 'NONE',  ( 13.43411237798106583, 52.66530133659708213, -12.81628187352647252 ) ) ;
#44707 =( LENGTH_UNIT ( ) NAMED_UNIT ( * ) SI_UNIT ( .MILLI., .METRE. ) );
#44706 = CARTESIAN_POINT ( 'NONE',  ( 10.00000000000000178, 70.00000000000000000, 0.000000000000000000 ) ) ;
#44708 = CARTESIAN_POINT ( 'NONE',  ( 17.20831665107776587, 9.133931151000787452, -7.208316651077762316 ) ) ;
#44709 = CARTESIAN_POINT ( 'NONE',  ( 13.79529636645030344, 3.262082168247301350, 14.16423886937410614 ) ) ;
#44710 = CARTESIAN_POINT ( 'NONE',  ( 14.92337183194729988, 54.34226448433412315, -8.527530157486177487 ) ) ;
#44711 = CARTESIAN_POINT ( 'NONE',  ( 4.559911319644449179, 42.23035201082151247, -9.422509992056141925 ) ) ;
#44712 = CARTESIAN_POINT ( 'NONE',  ( 14.92337183194729633, 42.67559781766745886, 8.527530157486181039 ) ) ;
#44713 = SHAPE_DEFINITION_REPRESENTATION ( #97154, #51695 ) ;
#44714 = CARTESIAN_POINT ( 'NONE',  ( -5.279540384298797129, 0.000000000000000000, 1.365381980696670716 ) ) ;
#44715 = EDGE_CURVE ( 'NONE', #9889, #41155, #51511, .T. ) ;
#44716 = CARTESIAN_POINT ( 'NONE',  ( 15.44008868035555260, 49.73035201082150536, 9.422509992056143702 ) ) ;
#44717 = ORIENTED_EDGE ( 'NONE', *, *, #47408, .F. ) ;
#44718 = EDGE_CURVE ( 'NONE', #38990, #71871, #54455, .T. ) ;
#44719 = LINE ( 'NONE', #1225, #90464 ) ;
#44720 = CARTESIAN_POINT ( 'NONE',  ( 17.96484262340118221, 11.18868534415483929, -7.964842623401177768 ) ) ;
#44722 = CARTESIAN_POINT ( 'NONE',  ( -0.8801773607111008646, 38.27201867748816255, 2.915334737309923430 ) ) ;
#44721 = CARTESIAN_POINT ( 'NONE',  ( 14.92337183194729988, 64.34226448433412315, -8.527530157486177487 ) ) ;
#44723 = CARTESIAN_POINT ( 'NONE',  ( 10.58981376305288613, 15.00000000000000000, -9.535111140613709679 ) ) ;
#44724 = CARTESIAN_POINT ( 'NONE',  ( 10.00000000000000000, 66.81368534415484817, -10.88017736071110342 ) ) ;
#44725 = CARTESIAN_POINT ( 'NONE',  ( 6.879999999999995453, 43.00000000000000000, -6.250000000000000000 ) ) ;
#44727 = CARTESIAN_POINT ( 'NONE',  ( 0.000000000000000000, 15.00000000000000000, 0.000000000000000000 ) ) ;
#44726 = CARTESIAN_POINT ( 'NONE',  ( 19.42250999205614548, 35.98035201082151247, -5.440088680355545492 ) ) ;
#44728 = CARTESIAN_POINT ( 'NONE',  ( 17.20831665107776587, 7.883931151000784787, 7.208316651077764980 ) ) ;
#44729 = CARTESIAN_POINT ( 'NONE',  ( 0.1532563361054100626, 20.80059781766744464, -2.638427012816831230 ) ) ;
#44730 = CARTESIAN_POINT ( 'NONE',  ( -1.780824192092587577, 14.49999999999999112, 14.89391369643518637 ) ) ;
#44731 = CARTESIAN_POINT ( 'NONE',  ( -5.204170427930421283E-15, 20.55374883491398208, -14.16423886937410082 ) ) ;
#44732 = CARTESIAN_POINT ( 'NONE',  ( 18.52753015748618282, 58.92559781766745886, -4.923371831947291888 ) ) ;
#44733 = AXIS2_PLACEMENT_3D ( 'NONE', #30168, #83683, #15198 ) ;
#44734 = CARTESIAN_POINT ( 'NONE',  ( 24.16423886937410614, 64.30374883491396076, 8.672049930838204340E-16 ) ) ;
#44735 = CARTESIAN_POINT ( 'NONE',  ( -4.164238869374098151, 16.59541550158063927, -3.795296366450310543 ) ) ;
#44736 = CARTESIAN_POINT ( 'NONE',  ( 24.16423886937410614, 54.51208216824730357, -3.795296366450302550 ) ) ;
#44737 = CARTESIAN_POINT ( 'NONE',  ( 20.88017736071110519, 5.563685344154837509, 2.639326808657452039E-16 ) ) ;
#44738 = ORIENTED_EDGE ( 'NONE', *, *, #38127, .T. ) ;
#44739 = CARTESIAN_POINT ( 'NONE',  ( 2.791683348922240793, 26.63393115100078745, 7.208316651077764092 ) ) ;
#44740 = CARTESIAN_POINT ( 'NONE',  ( 4.559911319644449179, 18.89701867748817321, 9.422509992056141925 ) ) ;
#44741 = CARTESIAN_POINT ( 'NONE',  ( 7.361572987183170547, 52.05059781766745175, 9.846743663894590881 ) ) ;
#44742 = DIRECTION ( 'NONE',  ( 0.000000000000000000, 0.000000000000000000, 1.000000000000000000 ) ) ;
#44743 = DIRECTION ( 'NONE',  ( 1.000000000000000000, 0.000000000000000000, 0.000000000000000000 ) ) ;
#44744 = CARTESIAN_POINT ( 'NONE',  ( -1.099225684535947600, 39.54030133659708923, 6.408140936763237150 ) ) ;
#44745 = CARTESIAN_POINT ( 'NONE',  ( 12.63842701281683034, 47.46726448433412315, 9.846743663894596210 ) ) ;
#44746 = ORIENTED_EDGE ( 'NONE', *, *, #4039, .T. ) ;
#44747 = CARTESIAN_POINT ( 'NONE',  ( 19.84674366389459266, 13.71726448433411782, -2.638427012816827677 ) ) ;
#44748 = CARTESIAN_POINT ( 'NONE',  ( 11.18126922403858003, -92.99194761433179224, -3.750000000000000000 ) ) ;
#44749 = CARTESIAN_POINT ( 'NONE',  ( 0.000000000000000000, 14.49999999999999822, 0.000000000000000000 ) ) ;
#44750 = CARTESIAN_POINT ( 'NONE',  ( 20.88017736071110164, 10.35535201082150714, 2.915334737309930979 ) ) ;
#44751 = CARTESIAN_POINT ( 'NONE',  ( 13.79529636645030344, 53.26208216824730357, 14.16423886937410614 ) ) ;
#44752 = CARTESIAN_POINT ( 'NONE',  ( 12.91533473730993009, 46.60535201082150536, -10.88017736071109987 ) ) ;
#44753 = CARTESIAN_POINT ( 'NONE',  ( 15.44008868035555793, 61.39701867748817676, -9.422509992056140149 ) ) ;
#44754 = EDGE_CURVE ( 'NONE', #85704, #17506, #8477, .T. ) ;
#44755 = CARTESIAN_POINT ( 'NONE',  ( 0.1532563361054100626, 20.80059781766744464, -2.638427012816831230 ) ) ;
#44756 = CARTESIAN_POINT ( 'NONE',  ( -0.8801773607111008646, 8.272018677488171434, 2.915334737309923430 ) ) ;
#44757 = CARTESIAN_POINT ( 'NONE',  ( 12.63842701281683034, 12.46726448433411782, 9.846743663894596210 ) ) ;
#44758 = DIRECTION ( 'NONE',  ( -0.000000000000000000, -1.000000000000000000, -0.000000000000000000 ) ) ;
#44759 = CARTESIAN_POINT ( 'NONE',  ( 5.076628168052703671, 56.84226448433412315, 8.527530157486179263 ) ) ;
#44760 = EDGE_CURVE ( 'NONE', #32525, #60007, #23348, .T. ) ;
#44761 = CARTESIAN_POINT ( 'NONE',  ( -0.8801773607111009756, 33.06368534415484106, 1.068504757029289695E-15 ) ) ;
#44762 = ORIENTED_EDGE ( 'NONE', *, *, #4215, .T. ) ;
#44763 = CARTESIAN_POINT ( 'NONE',  ( 0.6178305044545838731, 64.74863466993043914, 9.382169495545420901 ) ) ;
#44764 = LINE ( 'NONE', #60752, #12527 ) ;
#44765 = CARTESIAN_POINT ( 'NONE',  ( 2.791683348922237240, 15.38393115100078212, -7.208316651077763204 ) ) ;
#44766 = CARTESIAN_POINT ( 'NONE',  ( 16.40814093676324603, 37.45696800326376064, -11.09922568453594671 ) ) ;
#44768 = CARTESIAN_POINT ( 'NONE',  ( 10.00000000000000000, 34.75893115100078745, -9.846743663894594434 ) ) ;
#44767 = CARTESIAN_POINT ( 'NONE',  ( 0.5774900079438590739, 12.64701867748817321, -5.440088680355550821 ) ) ;
#44769 = CARTESIAN_POINT ( 'NONE',  ( 0.1532563361054100626, 0.8005978176674514168, -2.638427012816831230 ) ) ;
#44770 = CARTESIAN_POINT ( 'NONE',  ( 20.36894250292379382, 33.67874883491396076, 10.36894250292379205 ) ) ;
#44771 = CARTESIAN_POINT ( 'NONE',  ( -4.164238869374099039, 41.80374883491397497, 8.674139862899312516E-16 ) ) ;
#44772 = CARTESIAN_POINT ( 'NONE',  ( 7.361572987183169658, 54.96726448433413026, -9.846743663894592657 ) ) ;
#44773 = LINE ( 'NONE', #13796, #29940 ) ;
#44774 = CARTESIAN_POINT ( 'NONE',  ( 0.5774900079438607392, 33.48035201082150536, 5.440088680355550821 ) ) ;
#44775 = CARTESIAN_POINT ( 'NONE',  ( 18.52753015748617571, 3.092264484334118269, 4.923371831947298993 ) ) ;
#44776 = DIRECTION ( 'NONE',  ( 0.000000000000000000, 1.000000000000000000, 0.000000000000000000 ) ) ;
#44777 = VERTEX_POINT ( 'NONE', #53972 ) ;
#44778 = CARTESIAN_POINT ( 'NONE',  ( -2.816281873526471635, 63.91530133659708923, -3.434112377981056508 ) ) ;
#44779 = EDGE_LOOP ( 'NONE', ( #92267, #3002, #14350, #36649 ) ) ;
#44780 = CARTESIAN_POINT ( 'NONE',  ( 12.91533473730993009, 66.60535201082150536, -10.88017736071109987 ) ) ;
#44781 = VERTEX_POINT ( 'NONE', #31941 ) ;
#44782 = CARTESIAN_POINT ( 'NONE',  ( -4.164238869374098151, 11.59541550158063217, -3.795296366450310543 ) ) ;
#44783 = CARTESIAN_POINT ( 'NONE',  ( 19.84674366389459621, 13.50893115100078568, 7.409399052514197653E-17 ) ) ;
#44784 = CARTESIAN_POINT ( 'NONE',  ( 7.084665262690076126, 29.10535201082150181, 10.88017736071109987 ) ) ;
#44785 = CARTESIAN_POINT ( 'NONE',  ( 2.094539387258905538, 0.2439618909456068852, -6.442855573511589995 ) ) ;
#44786 = ORIENTED_EDGE ( 'NONE', *, *, #29437, .F. ) ;
#44787 = AXIS2_PLACEMENT_3D ( 'NONE', #34169, #2739, #11687 ) ;
#44788 = CARTESIAN_POINT ( 'NONE',  ( 2.035157376598822676, 22.43868534415483396, -7.964842623401177768 ) ) ;
#44789 = EDGE_LOOP ( 'NONE', ( #93146, #5550, #3985, #89116 ) ) ;
#44790 = VECTOR ( 'NONE', #57413, 1000.000000000000000 ) ;
#44791 = CARTESIAN_POINT ( 'NONE',  ( 20.03932841506542673, 55.62161441960502373, -6.397827110479002322 ) ) ;
#44792 = EDGE_LOOP ( 'NONE', ( #76784, #96448, #2013, #8095, #92420, #7148, #60130, #93235 ) ) ;
#44793 = ORIENTED_EDGE ( 'NONE', *, *, #33985, .F. ) ;
#44794 = CARTESIAN_POINT ( 'NONE',  ( 2.035157376598824452, 68.68868534415484817, 7.964842623401179544 ) ) ;
#44795 = CARTESIAN_POINT ( 'NONE',  ( 13.96521320569122437, 0.04922511925147349254, 4.755935267939266353 ) ) ;
#44797 = CARTESIAN_POINT ( 'NONE',  ( 19.88701968852526747, 6.794273331840863683, 6.480634945678607650 ) ) ;
#44796 = CARTESIAN_POINT ( 'NONE',  ( 4.559911319644449179, 17.23035201082150536, -9.422509992056141925 ) ) ;
#44798 = CARTESIAN_POINT ( 'NONE',  ( 5.076628168052703671, 1.842264484334118047, 8.527530157486179263 ) ) ;
#44799 = CIRCLE ( 'NONE', #35010, 14.49999999999999822 ) ;
#44800 = CARTESIAN_POINT ( 'NONE',  ( 4.559911319644449179, 18.89701867748817321, 9.422509992056141925 ) ) ;
#44801 = EDGE_CURVE ( 'NONE', #52823, #19862, #92387, .T. ) ;
#44802 = VERTEX_POINT ( 'NONE', #9458 ) ;
#44803 = CARTESIAN_POINT ( 'NONE',  ( 19.38216949554541557, 52.24863466993041072, -9.382169495545420901 ) ) ;
#44804 = CARTESIAN_POINT ( 'NONE',  ( 0.5774900079438590739, 37.64701867748817676, -5.440088680355550821 ) ) ;
#44805 = DIRECTION ( 'NONE',  ( -0.000000000000000000, 1.000000000000000000, -0.000000000000000000 ) ) ;
#44806 = CARTESIAN_POINT ( 'NONE',  ( -2.816281873526473856, 49.12363466993042493, 9.499525473075851096E-16 ) ) ;
#44807 = CARTESIAN_POINT ( 'NONE',  ( -0.8801773607111009756, 43.06368534415484106, 1.068504757029289695E-15 ) ) ;
#44808 = CARTESIAN_POINT ( 'NONE',  ( -2.816281873526473856, 4.331968003263754419, 3.434112377981055619 ) ) ;
#44809 = LINE ( 'NONE', #62774, #17967 ) ;
#44810 = CARTESIAN_POINT ( 'NONE',  ( 5.076628168052704559, 15.17559781766745175, -8.527530157486179263 ) ) ;
#44811 = CARTESIAN_POINT ( 'NONE',  ( -2.614810775378867191, 35.00346125376525919, 9.500000000000000000 ) ) ;
#44812 = CARTESIAN_POINT ( 'NONE',  ( 19.38216949554541202, 0.9986346699304200492, 9.382169495545424454 ) ) ;
#44813 = DIRECTION ( 'NONE',  ( 0.000000000000000000, -1.000000000000000000, 0.000000000000000000 ) ) ;
#44814 = CARTESIAN_POINT ( 'NONE',  ( 10.00000000000000000, 41.81368534415484106, -10.88017736071110342 ) ) ;
#44815 = CARTESIAN_POINT ( 'NONE',  ( 18.52753015748617571, 48.09226448433412315, 4.923371831947298993 ) ) ;
#44816 = COLOUR_RGB ( '', 0.08235294, 0.09019608, 0.10196078) ;
#44817 = SURFACE_SIDE_STYLE ('',( #21348 ) ) ;
#44818 = CARTESIAN_POINT ( 'NONE',  ( 5.076628168052704559, 10.17559781766745175, -8.527530157486179263 ) ) ;
#44820 = EDGE_LOOP ( 'NONE', ( #30886, #46078, #15605, #27115 ) ) ;
#44819 = CARTESIAN_POINT ( 'NONE',  ( 5.076628168052703671, 66.84226448433412315, 8.527530157486179263 ) ) ;
#44821 =( NAMED_UNIT ( * ) SI_UNIT ( $, .STERADIAN. ) SOLID_ANGLE_UNIT ( ) );
#44822 = CARTESIAN_POINT ( 'NONE',  ( 12.63842701281683034, 62.46726448433410894, 9.846743663894596210 ) ) ;
#44823 = VECTOR ( 'NONE', #96747, 1000.000000000000000 ) ;
#44824 = EDGE_CURVE ( 'NONE', #3422, #44200, #25470, .T. ) ;
#44825 = CARTESIAN_POINT ( 'NONE',  ( 4.395712687474492952, -0.8323168403830496498, -2.500000000000000888 ) ) ;
#44826 = CARTESIAN_POINT ( 'NONE',  ( 15.44008868035555793, 6.397018677488171434, -9.422509992056140149 ) ) ;
#44827 = CARTESIAN_POINT ( 'NONE',  ( 1.472469842513823179, 51.42559781766745886, 4.923371831947296329 ) ) ;
#44828 = DIRECTION ( 'NONE',  ( -0.000000000000000000, 0.000000000000000000, 1.000000000000000000 ) ) ;
#44829 = EDGE_CURVE ( 'NONE', #23534, #6552, #84481, .T. ) ;
#44830 = CARTESIAN_POINT ( 'NONE',  ( 0.5774900079438590739, 2.647018677488171434, -5.440088680355550821 ) ) ;
#44831 = DIRECTION ( 'NONE',  ( -0.000000000000000000, -0.000000000000000000, -1.000000000000000000 ) ) ;
#44832 = CARTESIAN_POINT ( 'NONE',  ( 7.084665262690076126, 19.10535201082150181, 10.88017736071109987 ) ) ;
#44833 = EDGE_CURVE ( 'NONE', #49656, #79731, #84963, .T. ) ;
#44834 = CARTESIAN_POINT ( 'NONE',  ( 13.79529636645031943, 55.34541550158062506, -14.16423886937409904 ) ) ;
#44835 = CARTESIAN_POINT ( 'NONE',  ( -4.164238869374099927, 67.01208216824728936, 3.795296366450308767 ) ) ;
#44836 = CARTESIAN_POINT ( 'NONE',  ( 2.791683348922237240, 5.383931151000785675, -7.208316651077763204 ) ) ;
#44837 = CARTESIAN_POINT ( 'NONE',  ( 1.472469842513823179, 25.59226448433412315, -4.923371831947296329 ) ) ;
#44838 = CARTESIAN_POINT ( 'NONE',  ( -2.816281873526473856, 14.12363466993041961, 9.499525473075851096E-16 ) ) ;
#44839 = VERTEX_POINT ( 'NONE', #15982 ) ;
#44840 = ORIENTED_EDGE ( 'NONE', *, *, #57607, .F. ) ;
#44841 = CARTESIAN_POINT ( 'NONE',  ( 0.3093388210927633941, 14.49999999999999822, 14.99680997725065978 ) ) ;
#44842 = CARTESIAN_POINT ( 'NONE',  ( 0.1532563361054083140, 61.00893115100078745, 1.131784320476157264E-15 ) ) ;
#44843 = CARTESIAN_POINT ( 'NONE',  ( 5.963430220938279902, 3.021642702460851204, -10.32896413005680181 ) ) ;
#44844 = FACE_OUTER_BOUND ( 'NONE', #86255, .T. ) ;
#44845 = CARTESIAN_POINT ( 'NONE',  ( 24.16423886937410614, 9.303748834913967869, 8.672049930838204340E-16 ) ) ;
#44846 = AXIS2_PLACEMENT_3D ( 'NONE', #6029, #51019, #19054 ) ;
#44847 = CARTESIAN_POINT ( 'NONE',  ( 17.20831665107776587, 27.88393115100078390, 7.208316651077764980 ) ) ;
#44848 = CARTESIAN_POINT ( 'NONE',  ( 0.2751277870542967463, 0.000000000000000000, 6.500000000000000888 ) ) ;
#44849 = ORIENTED_EDGE ( 'NONE', *, *, #24772, .T. ) ;
#44850 = CARTESIAN_POINT ( 'NONE',  ( 22.26659068614895176, 34.72041550158063927, -7.082119434687042414 ) ) ;
#44851 = CARTESIAN_POINT ( 'NONE',  ( 17.20831665107776587, 12.88393115100078390, 7.208316651077764980 ) ) ;
#44853 = DIRECTION ( 'NONE',  ( 0.000000000000000000, 1.000000000000000000, 0.000000000000000000 ) ) ;
#44852 = CYLINDRICAL_SURFACE ( 'NONE', #91409, 0.5000000000000004441 ) ;
#44854 = CARTESIAN_POINT ( 'NONE',  ( 10.00000000000000000, 31.81368534415483751, -10.88017736071110342 ) ) ;
#44855 = CARTESIAN_POINT ( 'NONE',  ( 3.591859063236763294, 43.29030133659708923, -11.09922568453595026 ) ) ;
#44856 = CARTESIAN_POINT ( 'NONE',  ( 0.5774900079438590739, 7.647018677488171434, -5.440088680355550821 ) ) ;
#44857 = AXIS2_PLACEMENT_3D ( 'NONE', #83259, #59260, #66772 ) ;
#44858 = CARTESIAN_POINT ( 'NONE',  ( 21.09922568453594849, 31.20696800326375353, 6.408140936763242479 ) ) ;
#44859 =( NAMED_UNIT ( * ) PLANE_ANGLE_UNIT ( ) SI_UNIT ( $, .RADIAN. ) );
#44860 = ORIENTED_EDGE ( 'NONE', *, *, #90416, .T. ) ;
#44861 = CARTESIAN_POINT ( 'NONE',  ( -13.69999999999999751, 99.99999999999998579, -8.000000000000000000 ) ) ;
#44862 = VECTOR ( 'NONE', #32465, 1000.000000000000000 ) ;
#44863 = CARTESIAN_POINT ( 'NONE',  ( -11.10136736363520527, 14.95077488074852745, -9.716261771425058313 ) ) ;
#44864 = CARTESIAN_POINT ( 'NONE',  ( -0.3689425029237898834, 36.17874883491396787, -10.36894250292378850 ) ) ;
#44865 = CARTESIAN_POINT ( 'NONE',  ( 2.035157376598822676, 7.438685344154837509, -7.964842623401177768 ) ) ;
#44866 = CARTESIAN_POINT ( 'NONE',  ( 19.42250999205614548, 25.98035201082150891, -5.440088680355545492 ) ) ;
#44867 = CARTESIAN_POINT ( 'NONE',  ( -13.14228782657345462, 0.3640475087720987379, 7.230509711182144805 ) ) ;
#44868 = CARTESIAN_POINT ( 'NONE',  ( -7.750000000000000000, 80.32179676972448590, -4.250000000000000000 ) ) ;
#44869 = CARTESIAN_POINT ( 'NONE',  ( 4.559911319644449179, 48.89701867748817676, 9.422509992056141925 ) ) ;
#44870 = CARTESIAN_POINT ( 'NONE',  ( 20.88017736071110519, 65.56368534415483396, 2.639326808657452039E-16 ) ) ;
#44871 = CARTESIAN_POINT ( 'NONE',  ( 13.43411237798105340, 25.58196800326374998, 12.81628187352647963 ) ) ;
#44872 = CARTESIAN_POINT ( 'NONE',  ( -2.827051895225887179, 0.2301501044984908817, 14.67071941139710312 ) ) ;
#44873 = CARTESIAN_POINT ( 'NONE',  ( -3.420591144908390113, 14.49999999999999112, -14.60477854057966063 ) ) ;
#44874 = CARTESIAN_POINT ( 'NONE',  ( 0.1532563361054083140, 26.00893115100078745, 1.131784320476157264E-15 ) ) ;
#44875 = CARTESIAN_POINT ( 'NONE',  ( 7.084665262690076126, 57.02201867748817676, -10.88017736071110164 ) ) ;
#44876 = EDGE_CURVE ( 'NONE', #35320, #95857, #52789, .T. ) ;
#44877 = CARTESIAN_POINT ( 'NONE',  ( 19.38216949554541557, 12.24863466993041961, -9.382169495545420901 ) ) ;
#44878 = CARTESIAN_POINT ( 'NONE',  ( 2.791683348922240793, 1.633931151000784565, 7.208316651077764092 ) ) ;
#44879 = CARTESIAN_POINT ( 'NONE',  ( 12.91533473730993009, 11.60535201082150536, -10.88017736071109987 ) ) ;
#44880 = CARTESIAN_POINT ( 'NONE',  ( 0.1532563361054100626, 35.80059781766745175, -2.638427012816831230 ) ) ;
#44881 = CARTESIAN_POINT ( 'NONE',  ( -2.816281873526473856, 59.12363466993042493, 9.499525473075851096E-16 ) ) ;
#44882 = CARTESIAN_POINT ( 'NONE',  ( 18.52753015748618282, 13.92559781766745175, -4.923371831947291888 ) ) ;
#44883 = CARTESIAN_POINT ( 'NONE',  ( -0.3689425029237898834, 1.178748834913967869, -10.36894250292378850 ) ) ;
#44884 = CARTESIAN_POINT ( 'NONE',  ( 0.000000000000000000, 15.00000000000000000, 0.000000000000000000 ) ) ;
#44885 = CARTESIAN_POINT ( 'NONE',  ( 15.44008868035555793, 31.39701867748817676, -9.422509992056140149 ) ) ;
#44886 = SURFACE_STYLE_FILL_AREA ( #14416 ) ;
#44887 = CARTESIAN_POINT ( 'NONE',  ( 2.791683348922240793, 46.63393115100077324, 7.208316651077764092 ) ) ;
#44888 = CARTESIAN_POINT ( 'NONE',  ( 0.5774900079438607392, 33.48035201082150536, 5.440088680355550821 ) ) ;
#44889 = CARTESIAN_POINT ( 'NONE',  ( 0.5774900079438590739, 12.64701867748817321, -5.440088680355550821 ) ) ;
#44890 = ORIENTED_EDGE ( 'NONE', *, *, #39564, .T. ) ;
#44891 = VECTOR ( 'NONE', #77807, 1000.000000000000000 ) ;
#44892 = CARTESIAN_POINT ( 'NONE',  ( 15.44008868035555793, 31.39701867748817676, -9.422509992056140149 ) ) ;
#44893 = AXIS2_PLACEMENT_3D ( 'NONE', #86909, #25448, #85939 ) ;
#44894 = CARTESIAN_POINT ( 'NONE',  ( -2.816281873526473856, 49.33196800326374643, 3.434112377981055619 ) ) ;
#44895 = CARTESIAN_POINT ( 'NONE',  ( 12.91533473730992121, 49.52201867748817676, 10.88017736071110164 ) ) ;
#44897 = CARTESIAN_POINT ( 'NONE',  ( 17.96484262340118221, 41.18868534415484106, -7.964842623401177768 ) ) ;
#44896 = SURFACE_SIDE_STYLE ('',( #60890 ) ) ;
#44898 = ORIENTED_EDGE ( 'NONE', *, *, #9194, .F. ) ;
#44899 = CARTESIAN_POINT ( 'NONE',  ( 19.84674366389459266, 58.71726448433411605, -2.638427012816827677 ) ) ;
#44900 = CARTESIAN_POINT ( 'NONE',  ( 10.00000000000000000, 41.81368534415484106, -10.88017736071110342 ) ) ;
#44901 = CARTESIAN_POINT ( 'NONE',  ( 7.185087194272973932, -80.58596676771932721, 4.000000000000000000 ) ) ;
#44902 = AXIS2_PLACEMENT_3D ( 'NONE', #78436, #48429, #10441 ) ;
#44903 =( NAMED_UNIT ( * ) PLANE_ANGLE_UNIT ( ) SI_UNIT ( $, .RADIAN. ) );
#44904 = CARTESIAN_POINT ( 'NONE',  ( 8.879999999999991900, 20.99999999999999645, 0.000000000000000000 ) ) ;
#44905 = CARTESIAN_POINT ( 'NONE',  ( 6.204703633549690345, 45.76208216824729647, -14.16423886937410259 ) ) ;
#44906 = CARTESIAN_POINT ( 'NONE',  ( 17.96484262340118221, 51.18868534415483396, -7.964842623401177768 ) ) ;
#44907 = PLANE ( 'NONE',  #22190 ) ;
#44908 = CARTESIAN_POINT ( 'NONE',  ( 17.20831665107776587, 64.13393115100079456, -7.208316651077762316 ) ) ;
#44909 = DIRECTION ( 'NONE',  ( -0.000000000000000000, -1.000000000000000000, -0.000000000000000000 ) ) ;
#44910 = CARTESIAN_POINT ( 'NONE',  ( 1.472469842513823179, 35.59226448433412315, -4.923371831947296329 ) ) ;
#44911 = ORIENTED_EDGE ( 'NONE', *, *, #19140, .F. ) ;
#44912 = CARTESIAN_POINT ( 'NONE',  ( 19.84674366389459621, 38.50893115100078745, 7.409399052514197653E-17 ) ) ;
#44913 = CARTESIAN_POINT ( 'NONE',  ( -9.382169495545413795, -20.25136533006958217, 9.382169495545428006 ) ) ;
#44914 = CARTESIAN_POINT ( 'NONE',  ( 19.42250999205614548, 25.98035201082150891, -5.440088680355545492 ) ) ;
#44915 = CARTESIAN_POINT ( 'NONE',  ( 19.84674366389459266, 28.30059781766745886, 2.638427012816836559 ) ) ;
#44916 = CARTESIAN_POINT ( 'NONE',  ( 3.591859063236763294, 23.29030133659708568, -11.09922568453595026 ) ) ;
#44918 = CARTESIAN_POINT ( 'NONE',  ( 7.084665262690076126, 64.10535201082150536, 10.88017736071109987 ) ) ;
#44917 = CARTESIAN_POINT ( 'NONE',  ( 3.166711953933263768, 0.000000000000000000, -4.439566422914428045 ) ) ;
#44920 = CARTESIAN_POINT ( 'NONE',  ( 4.559911319644449179, 3.897018677488170990, 9.422509992056141925 ) ) ;
#44919 = CARTESIAN_POINT ( 'NONE',  ( 7.084665262690076126, 39.10535201082150536, 10.88017736071109987 ) ) ;
#44921 = CARTESIAN_POINT ( 'NONE',  ( 22.26659068614894466, 43.88708216824729647, 7.082119434687054849 ) ) ;
#44922 = ADVANCED_FACE ( 'NONE', ( #47936 ), #94248, .T. ) ;
#44923 = COLOUR_RGB ( '', 0.40784314, 0.44705882, 0.49803922) ;
#44924 = CARTESIAN_POINT ( 'NONE',  ( 0.000000000000000000, 80.32179676972448590, -4.000000000000000000 ) ) ;
#44925 = EDGE_CURVE ( 'NONE', #65472, #83178, #521, .T. ) ;
#44926 = ORIENTED_EDGE ( 'NONE', *, *, #11446, .T. ) ;
#44927 = CARTESIAN_POINT ( 'NONE',  ( 10.00000000000000000, 17.87363466993041783, -12.81628187352647608 ) ) ;
#44928 = CARTESIAN_POINT ( 'NONE',  ( 4.559911319644449179, 7.230352010821504471, -9.422509992056141925 ) ) ;
#44929 = CARTESIAN_POINT ( 'NONE',  ( 2.035157376598824452, 53.68868534415484817, 7.964842623401179544 ) ) ;
#44930 = AXIS2_PLACEMENT_3D ( 'NONE', #537, #44013, #98041 ) ;
#44931 = CARTESIAN_POINT ( 'NONE',  ( 0.4278561937608483801, 0.000000000000000000, -5.436428395565743088 ) ) ;
#44932 = ORIENTED_EDGE ( 'NONE', *, *, #14425, .T. ) ;
#44933 = CARTESIAN_POINT ( 'NONE',  ( 15.44008868035555793, 51.39701867748816966, -9.422509992056140149 ) ) ;
#44934 = CIRCLE ( 'NONE', #75284, 0.2500000000000002220 ) ;
#44935 = CARTESIAN_POINT ( 'NONE',  ( 19.84674366389459266, 38.71726448433412315, -2.638427012816827677 ) ) ;
#44936 = ADVANCED_FACE ( 'NONE', ( #46469 ), #32007, .T. ) ;
#44937 = CARTESIAN_POINT ( 'NONE',  ( 7.361572987183170547, 22.05059781766745530, 9.846743663894590881 ) ) ;
#44938 = CARTESIAN_POINT ( 'NONE',  ( 10.00000000000000000, 14.75893115100078568, -9.846743663894594434 ) ) ;
#44940 = CARTESIAN_POINT ( 'NONE',  ( 13.43411237798105340, 40.58196800326375353, 12.81628187352647963 ) ) ;
#44939 = CARTESIAN_POINT ( 'NONE',  ( 14.82269085861167568, 14.63595249122790598, 2.299529454047060550 ) ) ;
#44942 = LINE ( 'NONE', #7466, #10010 ) ;
#44941 = CARTESIAN_POINT ( 'NONE',  ( 17.20831665107776587, 9.133931151000787452, -7.208316651077762316 ) ) ;
#44943 = CARTESIAN_POINT ( 'NONE',  ( 8.629999999999995453, 40.99999999999999289, 6.500000000000000888 ) ) ;
#44945 = ORIENTED_EDGE ( 'NONE', *, *, #14029, .T. ) ;
#44944 = CARTESIAN_POINT ( 'NONE',  ( 14.92337183194729988, 34.34226448433411605, -8.527530157486177487 ) ) ;
#44946 = CARTESIAN_POINT ( 'NONE',  ( 3.591859063236761518, 59.95696800326375353, 11.09922568453594849 ) ) ;
#44947 = DIRECTION ( 'NONE',  ( -0.000000000000000000, -1.000000000000000000, -0.000000000000000000 ) ) ;
#44949 = EDGE_CURVE ( 'NONE', #48124, #18106, #28803, .T. ) ;
#44948 = CARTESIAN_POINT ( 'NONE',  ( 6.565887622018943937, 15.16530133659708568, 12.81628187352647430 ) ) ;
#44950 = CARTESIAN_POINT ( 'NONE',  ( 7.084665262690076126, 52.02201867748816255, -10.88017736071110164 ) ) ;
#44951 = CARTESIAN_POINT ( 'NONE',  ( 13.79529636645031943, 35.34541550158063927, -14.16423886937409904 ) ) ;
#44952 = CARTESIAN_POINT ( 'NONE',  ( 2.377183314879979026, 40.78593319516822646, -6.500000000000005329 ) ) ;
#44953 = EDGE_CURVE ( 'NONE', #87334, #11994, #994, .T. ) ;
#44954 = CARTESIAN_POINT ( 'NONE',  ( -2.266590686148945544, 32.22041550158063927, 7.082119434687048631 ) ) ;
#44955 = B_SPLINE_CURVE_WITH_KNOTS ( 'NONE', 3,
 ( #81344, #80364, #72845, #43826, #5365, #35844 ),
 .UNSPECIFIED., .F., .F.,
 ( 4, 2, 4 ),
 ( 0.0002800206007755490657, 0.0006862260317144062332, 0.001092431462653263401 ),
 .UNSPECIFIED. ) ;
#44956 = CARTESIAN_POINT ( 'NONE',  ( 6.204703633549690345, 50.76208216824730357, -14.16423886937410259 ) ) ;
#44957 = CARTESIAN_POINT ( 'NONE',  ( 2.917880565312948704, 7.637082168247301794, 12.26659068614894643 ) ) ;
#44959 = CARTESIAN_POINT ( 'NONE',  ( -5.999999999999994671, 43.00000000000000000, -6.250000000000000000 ) ) ;
#44958 = CARTESIAN_POINT ( 'NONE',  ( 10.00000000000000000, 15.55374883491396787, -14.16423886937410082 ) ) ;
#44960 = CARTESIAN_POINT ( 'NONE',  ( 2.035157376598824452, 48.68868534415483396, 7.964842623401179544 ) ) ;
#44961 = CARTESIAN_POINT ( 'NONE',  ( 6.533420211785746723, -50.31490269211863620, -2.750000000000000000 ) ) ;
#44962 = CARTESIAN_POINT ( 'NONE',  ( 12.63842701281683922, 24.55059781766745175, -9.846743663894590881 ) ) ;
#44964 = CARTESIAN_POINT ( 'NONE',  ( 0.1532563361054082862, 31.21726448433412315, 2.638427012816831674 ) ) ;
#44963 = CARTESIAN_POINT ( 'NONE',  ( 4.559911319644449179, 68.89701867748817676, 9.422509992056141925 ) ) ;
#44965 = CIRCLE ( 'NONE', #3456, 19.99999999999999645 ) ;
#44966 = CARTESIAN_POINT ( 'NONE',  ( 4.559911319644449179, 28.89701867748817321, 9.422509992056141925 ) ) ;
#44967 = CARTESIAN_POINT ( 'NONE',  ( 21.09922568453594849, 61.20696800326376064, 6.408140936763242479 ) ) ;
#44968 = CARTESIAN_POINT ( 'NONE',  ( 17.20831665107776587, 64.13393115100079456, -7.208316651077762316 ) ) ;
#44969 =( NAMED_UNIT ( * ) SI_UNIT ( $, .STERADIAN. ) SOLID_ANGLE_UNIT ( ) );
#44970 = CARTESIAN_POINT ( 'NONE',  ( 16.40814093676323893, 35.79030133659708923, 11.09922568453595026 ) ) ;
#44971 = CARTESIAN_POINT ( 'NONE',  ( 10.36894250292379027, -26.32125116508603568, 10.36894250292378672 ) ) ;
#44972 = CARTESIAN_POINT ( 'NONE',  ( 10.00000000000000000, 41.81368534415484106, -10.88017736071110342 ) ) ;
#44973 = CARTESIAN_POINT ( 'NONE',  ( 14.92337183194729988, 54.34226448433412315, -8.527530157486177487 ) ) ;
#44974 = AXIS2_PLACEMENT_3D ( 'NONE', #86332, #17836, #33309 ) ;
#44975 = CARTESIAN_POINT ( 'NONE',  ( -4.164238869374098151, 21.59541550158063217, -3.795296366450310543 ) ) ;
#44976 = ORIENTED_EDGE ( 'NONE', *, *, #52091, .F. ) ;
#44977 = CARTESIAN_POINT ( 'NONE',  ( -0.3689425029237898834, 1.178748834913967869, -10.36894250292378850 ) ) ;
#44978 = CARTESIAN_POINT ( 'NONE',  ( 20.88017736071110875, 65.77201867748817676, -2.915334737309920765 ) ) ;
#44979 = CARTESIAN_POINT ( 'NONE',  ( 24.16423886937410614, 64.51208216824728936, -3.795296366450302550 ) ) ;
#44980 = CARTESIAN_POINT ( 'NONE',  ( 21.09922568453594849, 1.206968003263753531, 6.408140936763242479 ) ) ;
#44981 = DIRECTION ( 'NONE',  ( 0.000000000000000000, 1.000000000000000000, 0.000000000000000000 ) ) ;
#44982 = CARTESIAN_POINT ( 'NONE',  ( -0.8801773607111009756, 53.06368534415484106, 1.068504757029289695E-15 ) ) ;
#44983 = DIRECTION ( 'NONE',  ( 0.000000000000000000, 1.000000000000000000, 0.000000000000000000 ) ) ;
#44984 = CARTESIAN_POINT ( 'NONE',  ( 2.917880565312950480, 55.97041550158063217, -12.26659068614894821 ) ) ;
#44985 = CARTESIAN_POINT ( 'NONE',  ( 5.440088680355556150, 29.73035201082152668, 9.422509992056138373 ) ) ;
#44986 = CARTESIAN_POINT ( 'NONE',  ( 12.91533473730993009, 11.60535201082150536, -10.88017736071109987 ) ) ;
#44987 = CARTESIAN_POINT ( 'NONE',  ( 2.035157376598824452, 18.68868534415484106, 7.964842623401179544 ) ) ;
#44988 = CARTESIAN_POINT ( 'NONE',  ( 14.92337183194729633, 62.67559781766745886, 8.527530157486181039 ) ) ;
#44989 = CARTESIAN_POINT ( 'NONE',  ( 19.38216949554541202, 55.99863466993041072, 9.382169495545424454 ) ) ;
#44990 = LINE ( 'NONE', #31462, #74314 ) ;
#44991 = ORIENTED_EDGE ( 'NONE', *, *, #32163, .T. ) ;
#44992 = CARTESIAN_POINT ( 'NONE',  ( 15.44008868035555260, 19.73035201082150536, 9.422509992056143702 ) ) ;
#44993 = EDGE_CURVE ( 'NONE', #33828, #75926, #40463, .T. ) ;
#44994 = CARTESIAN_POINT ( 'NONE',  ( 19.38216949554541557, 17.24863466993041783, -9.382169495545420901 ) ) ;
#44995 = LINE ( 'NONE', #52499, #14623 ) ;
#44996 = VECTOR ( 'NONE', #8019, 1000.000000000000000 ) ;
#44997 =( GEOMETRIC_REPRESENTATION_CONTEXT ( 3 ) GLOBAL_UNCERTAINTY_ASSIGNED_CONTEXT ( ( #17481 ) ) GLOBAL_UNIT_ASSIGNED_CONTEXT ( ( #34309, #26826, #57811 ) ) REPRESENTATION_CONTEXT ( 'NONE', 'WORKASPACE' ) );
#44998 = CARTESIAN_POINT ( 'NONE',  ( 2.791683348922237240, 45.38393115100079456, -7.208316651077763204 ) ) ;
#44999 = CARTESIAN_POINT ( 'NONE',  ( 7.084665262690076126, 39.10535201082150536, 10.88017736071109987 ) ) ;
#45000 = CARTESIAN_POINT ( 'NONE',  ( 6.565887622018943937, 23.08196800326375708, -12.81628187352647608 ) ) ;
#45002 = DIRECTION ( 'NONE',  ( 0.000000000000000000, 1.000000000000000000, 0.000000000000000000 ) ) ;
#45001 = CARTESIAN_POINT ( 'NONE',  ( -0.8801773607110991993, 42.85535201082150536, -2.915334737309923874 ) ) ;
#45003 = DIRECTION ( 'NONE',  ( 1.000000000000000000, 0.000000000000000000, 0.000000000000000000 ) ) ;
#45004 = CARTESIAN_POINT ( 'NONE',  ( 6.565887622018943937, 48.08196800326375353, -12.81628187352647608 ) ) ;
#45005 = VERTEX_POINT ( 'NONE', #70962 ) ;
#45006 = CARTESIAN_POINT ( 'NONE',  ( 20.88017736071110164, 45.35535201082149115, 2.915334737309930979 ) ) ;
#45008 = CARTESIAN_POINT ( 'NONE',  ( 6.204703633549690345, 5.762082168247301794, -14.16423886937410259 ) ) ;
#45007 = CARTESIAN_POINT ( 'NONE',  ( 10.00000000000000178, 35.37363466993042493, 12.81628187352647608 ) ) ;
#45009 = CARTESIAN_POINT ( 'NONE',  ( 20.88017736071110875, 45.77201867748816966, -2.915334737309920765 ) ) ;
#45010 = CARTESIAN_POINT ( 'NONE',  ( 18.52753015748618282, 63.92559781766745886, -4.923371831947291888 ) ) ;
#45011 = CARTESIAN_POINT ( 'NONE',  ( 4.219999999999999751, 37.00000000000000000, 3.750000000000000000 ) ) ;
#45012 = CARTESIAN_POINT ( 'NONE',  ( 18.52753015748617571, 23.09226448433411960, 4.923371831947298993 ) ) ;
#45013 = CARTESIAN_POINT ( 'NONE',  ( 18.52753015748617571, 13.09226448433411960, 4.923371831947298993 ) ) ;
#45014 = CARTESIAN_POINT ( 'NONE',  ( -8.000000000000000000, 40.74999999999999289, -3.750000000000000000 ) ) ;
#45015 = CARTESIAN_POINT ( 'NONE',  ( 20.36894250292379738, 49.92874883491396787, -10.36894250292379027 ) ) ;
#45016 = AXIS2_PLACEMENT_3D ( 'NONE', #34606, #49608, #18645 ) ;
#45017 = CARTESIAN_POINT ( 'NONE',  ( 20.00000000000000711, 79.40087001978915282, 4.500000000000000888 ) ) ;
#45018 = CARTESIAN_POINT ( 'NONE',  ( 8.880000000000002558, -0.01511739988658945127, -3.750000000000000888 ) ) ;
#45019 = CARTESIAN_POINT ( 'NONE',  ( -7.124934413296625912, -78.83349193436581004, -3.750000000000000888 ) ) ;
#45020 = ORIENTED_EDGE ( 'NONE', *, *, #48004, .T. ) ;
#45021 = CARTESIAN_POINT ( 'NONE',  ( -4.164238869374099927, 67.01208216824728936, 3.795296366450308767 ) ) ;
#45022 = CARTESIAN_POINT ( 'NONE',  ( 24.16423886937410614, 59.51208216824728936, -3.795296366450302550 ) ) ;
#45023 = CARTESIAN_POINT ( 'NONE',  ( 1.472469842513823179, 36.42559781766745175, 4.923371831947296329 ) ) ;
#45024 = CARTESIAN_POINT ( 'NONE',  ( 10.00000000000000178, 45.37363466993041783, 12.81628187352647608 ) ) ;
#45026 = CARTESIAN_POINT ( 'NONE',  ( 10.00000000000000000, 10.55374883491396787, -14.16423886937410082 ) ) ;
#45025 = CARTESIAN_POINT ( 'NONE',  ( 2.258648100792295832, 0.04922511925147383949, -14.57890972981273769 ) ) ;
#45027 = CARTESIAN_POINT ( 'NONE',  ( 17.96484262340118221, 16.18868534415483396, -7.964842623401177768 ) ) ;
#45028 = CARTESIAN_POINT ( 'NONE',  ( 2.917880565312948704, 62.63708216824730357, 12.26659068614894643 ) ) ;
#45029 = CARTESIAN_POINT ( 'NONE',  ( 5.076628168052703671, 46.84226448433412315, 8.527530157486179263 ) ) ;
#45030 = DIRECTION ( 'NONE',  ( 1.000000000000000000, 0.000000000000000000, 0.000000000000000000 ) ) ;
#45031 = CARTESIAN_POINT ( 'NONE',  ( 7.361572987183170547, 27.05059781766745175, 9.846743663894590881 ) ) ;
#45032 = CARTESIAN_POINT ( 'NONE',  ( 0.000000000000000000, 14.49999999999999822, 0.000000000000000000 ) ) ;
#45033 = CARTESIAN_POINT ( 'NONE',  ( -9.846743663894596210, 20.80059781766745175, -2.638427012816824124 ) ) ;
#45034 = ORIENTED_EDGE ( 'NONE', *, *, #70557, .F. ) ;
#45035 = EDGE_LOOP ( 'NONE', ( #80700, #47656, #13156, #37967 ) ) ;
#45037 = EDGE_CURVE ( 'NONE', #33071, #41488, #69731, .T. ) ;
#45036 = SURFACE_STYLE_FILL_AREA ( #15069 ) ;
#45038 = ORIENTED_EDGE ( 'NONE', *, *, #74963, .T. ) ;
#45039 = CARTESIAN_POINT ( 'NONE',  ( 6.204703633549690345, 20.76208216824730357, -14.16423886937410259 ) ) ;
#45041 = CARTESIAN_POINT ( 'NONE',  ( 7.084665262690076126, 42.02201867748816966, -10.88017736071110164 ) ) ;
#45040 = CARTESIAN_POINT ( 'NONE',  ( 19.42250999205614548, 35.98035201082151247, -5.440088680355545492 ) ) ;
#45043 = CARTESIAN_POINT ( 'NONE',  ( 6.565887622018943937, 35.16530133659708923, 12.81628187352647430 ) ) ;
#45042 = CARTESIAN_POINT ( 'NONE',  ( 18.52753015748617571, 58.09226448433411605, 4.923371831947298993 ) ) ;
#45044 = CARTESIAN_POINT ( 'NONE',  ( 24.16423886937410614, 9.303748834913967869, 8.672049930838204340E-16 ) ) ;
#45045 = EDGE_CURVE ( 'NONE', #75802, #69260, #76479, .T. ) ;
#45046 = EDGE_CURVE ( 'NONE', #15789, #70022, #42274, .T. ) ;
#45047 = CARTESIAN_POINT ( 'NONE',  ( 3.591859063236763294, 33.29030133659708213, -11.09922568453595026 ) ) ;
#45048 = EDGE_CURVE ( 'NONE', #38087, #40514, #41245, .T. ) ;
#45049 = VERTEX_POINT ( 'NONE', #71452 ) ;
#45050 = CARTESIAN_POINT ( 'NONE',  ( 12.63842701281683034, 47.46726448433412315, 9.846743663894596210 ) ) ;
#45051 = CARTESIAN_POINT ( 'NONE',  ( 10.00000000000000178, 4.313685344154837509, 10.88017736071110342 ) ) ;
#45052 = ORIENTED_EDGE ( 'NONE', *, *, #25575, .F. ) ;
#45053 = CARTESIAN_POINT ( 'NONE',  ( 2.035157376598822676, 12.43868534415483751, -7.964842623401177768 ) ) ;
#45054 = VERTEX_POINT ( 'NONE', #94426 ) ;
#45055 = CARTESIAN_POINT ( 'NONE',  ( 19.42250999205614548, 65.98035201082151957, -5.440088680355545492 ) ) ;
#45056 = CARTESIAN_POINT ( 'NONE',  ( 17.96484262340118221, 56.18868534415484817, -7.964842623401177768 ) ) ;
#45057 = CARTESIAN_POINT ( 'NONE',  ( 17.96484262340118221, 66.18868534415483396, -7.964842623401177768 ) ) ;
#45058 = CYLINDRICAL_SURFACE ( 'NONE', #18441, 0.2500000000000002220 ) ;
#45059 = CARTESIAN_POINT ( 'NONE',  ( 15.44008868035555260, 54.73035201082150536, 9.422509992056143702 ) ) ;
#45060 = EDGE_CURVE ( 'NONE', #69579, #40063, #10447, .T. ) ;
#45061 = CARTESIAN_POINT ( 'NONE',  ( -46.94000000000001194, 100.6164469615930841, 8.719320056954199316 ) ) ;
#45062 = LINE ( 'NONE', #7084, #75855 ) ;
#45065 = ORIENTED_EDGE ( 'NONE', *, *, #20687, .T. ) ;
#45064 = AXIS2_PLACEMENT_3D ( 'NONE', #27716, #20724, #51214 ) ;
#45063 = CARTESIAN_POINT ( 'NONE',  ( 11.18664512644303599, -81.61943089664755746, 4.000000000000000888 ) ) ;
#45066 = CARTESIAN_POINT ( 'NONE',  ( 5.076628168052704559, 45.17559781766745175, -8.527530157486179263 ) ) ;
#45067 = VERTEX_POINT ( 'NONE', #41944 ) ;
#45068 = CARTESIAN_POINT ( 'NONE',  ( 2.621477372531582528, -0.03417435944610275333, 15.77990027919563154 ) ) ;
#45069 = PRESENTATION_STYLE_ASSIGNMENT (( #46072 ) ) ;
#45070 = MECHANICAL_DESIGN_GEOMETRIC_PRESENTATION_REPRESENTATION (  '', ( #80191 ), #92961 ) ;
#45071 = AXIS2_PLACEMENT_3D ( 'NONE', #2687, #79141, #10652 ) ;
#45072 = ADVANCED_FACE ( 'NONE', ( #25941 ), #35399, .T. ) ;
#45073 = COLOUR_RGB ( '', 0.72549020, 0.75294118, 0.79215686) ;
#45074 = CARTESIAN_POINT ( 'NONE',  ( 17.08211943468705840, 5.137082168247300906, -12.26659068614894466 ) ) ;
#45075 = EDGE_LOOP ( 'NONE', ( #37813, #25264, #43168, #39994 ) ) ;
#45076 = FACE_OUTER_BOUND ( 'NONE', #56618, .T. ) ;
#45077 = CARTESIAN_POINT ( 'NONE',  ( 17.96484262340118221, 11.18868534415484106, -7.964842623401177768 ) ) ;
#45078 = CARTESIAN_POINT ( 'NONE',  ( 17.75000000000000355, 73.00000000000001421, -6.500000000000000888 ) ) ;
#45080 = ORIENTED_EDGE ( 'NONE', *, *, #59954, .F. ) ;
#45079 = CARTESIAN_POINT ( 'NONE',  ( 22.81628187352647785, 46.41530133659708213, 3.434112377981063169 ) ) ;
#45081 = CARTESIAN_POINT ( 'NONE',  ( 19.88565890683628723, 62.71691075486300804, -6.480892540919839462 ) ) ;
#45082 = CARTESIAN_POINT ( 'NONE',  ( 0.1532563361054082862, 46.21726448433411605, 2.638427012816831674 ) ) ;
#45083 = CARTESIAN_POINT ( 'NONE',  ( 17.74999999999999645, 91.00000000000000000, 8.000000000000000000 ) ) ;
#45084 = CARTESIAN_POINT ( 'NONE',  ( 10.00000000000000178, 20.37363466993042138, 12.81628187352647608 ) ) ;
#45085 = CARTESIAN_POINT ( 'NONE',  ( 2.791683348922237240, 25.38393115100078390, -7.208316651077763204 ) ) ;
#45086 = DIRECTION ( 'NONE',  ( -1.000000000000000000, 0.000000000000000000, 0.000000000000000000 ) ) ;
#45087 = CARTESIAN_POINT ( 'NONE',  ( 16.40814093676324603, 2.456968003263753531, -11.09922568453594671 ) ) ;
#45088 = EDGE_CURVE ( 'NONE', #92052, #2779, #2989, .T. ) ;
#45089 = CARTESIAN_POINT ( 'NONE',  ( 5.418184704451244116, 0.000000000000000000, -0.6173241701923083413 ) ) ;
#45090 = ORIENTED_EDGE ( 'NONE', *, *, #28363, .T. ) ;
#45091 = CARTESIAN_POINT ( 'NONE',  ( 17.96484262340118221, 19.93868534415484106, 7.964842623401181321 ) ) ;
#45092 = CARTESIAN_POINT ( 'NONE',  ( 6.204703633549690345, 20.76208216824730357, -14.16423886937410259 ) ) ;
#45093 = CARTESIAN_POINT ( 'NONE',  ( 14.92337183194729988, 29.34226448433411960, -8.527530157486177487 ) ) ;
#45094 = CARTESIAN_POINT ( 'NONE',  ( 10.00000000000000000, -0.2410688489992152128, -9.846743663894594434 ) ) ;
#45095 = CARTESIAN_POINT ( 'NONE',  ( 10.00000000000000000, 37.87363466993041783, -12.81628187352647608 ) ) ;
#45096 = CARTESIAN_POINT ( 'NONE',  ( 10.00000000000000000, 11.81368534415483751, -10.88017736071110342 ) ) ;
#45097 = DIRECTION ( 'NONE',  ( -0.000000000000000000, -1.000000000000000000, -0.000000000000000000 ) ) ;
#45098 = TOROIDAL_SURFACE ( 'NONE', #2034, 14.49999999999999822, 0.5000000000000000000 ) ;
#45099 = CARTESIAN_POINT ( 'NONE',  ( 19.38216949554541557, 7.248634669930421381, -9.382169495545420901 ) ) ;
#45100 = CARTESIAN_POINT ( 'NONE',  ( 19.84674366389459266, 23.30059781766745530, 2.638427012816836559 ) ) ;
#45101 = CARTESIAN_POINT ( 'NONE',  ( 2.915334737309921209, -13.39464798917849109, -10.88017736071110164 ) ) ;
#45102 = CARTESIAN_POINT ( 'NONE',  ( 16.40814093676324603, 32.45696800326375353, -11.09922568453594671 ) ) ;
#45103 = LINE ( 'NONE', #6620, #70789 ) ;
#45105 = DIRECTION ( 'NONE',  ( 0.000000000000000000, 1.000000000000000000, 0.000000000000000000 ) ) ;
#45104 = CARTESIAN_POINT ( 'NONE',  ( -0.8801773607110991993, 37.85535201082151247, -2.915334737309923874 ) ) ;
#45106 = FACE_OUTER_BOUND ( 'NONE', #13185, .T. ) ;
#45107 = CARTESIAN_POINT ( 'NONE',  ( 19.72487221294571569, 20.71833443783938122, -6.499999999999990230 ) ) ;
#45108 = CARTESIAN_POINT ( 'NONE',  ( 17.96484262340118221, 41.18868534415484106, -7.964842623401177768 ) ) ;
#45110 = CARTESIAN_POINT ( 'NONE',  ( 4.559911319644449179, 47.23035201082150536, -9.422509992056141925 ) ) ;
#45109 = TOROIDAL_SURFACE ( 'NONE', #13135, 14.49999999999999822, 0.5000000000000000000 ) ;
#45111 = CARTESIAN_POINT ( 'NONE',  ( 7.361572987183170547, 62.05059781766745886, 9.846743663894590881 ) ) ;
#45112 = CARTESIAN_POINT ( 'NONE',  ( 17.96484262340118221, 61.18868534415482685, -7.964842623401177768 ) ) ;
#45113 = CARTESIAN_POINT ( 'NONE',  ( 2.791683348922240793, 56.63393115100078035, 7.208316651077764092 ) ) ;
#45115 = LINE ( 'NONE', #27282, #46306 ) ;
#45114 = CARTESIAN_POINT ( 'NONE',  ( 19.42250999205614193, 5.147018677488171434, 5.440088680355555262 ) ) ;
#45116 = CARTESIAN_POINT ( 'NONE',  ( 6.565887622018943937, 8.081968003263751754, -12.81628187352647608 ) ) ;
#45117 = EDGE_LOOP ( 'NONE', ( #10630, #13574, #91200, #68446 ) ) ;
#45118 = CARTESIAN_POINT ( 'NONE',  ( 0.5774900079438590739, 22.64701867748817321, -5.440088680355550821 ) ) ;
#45119 = CARTESIAN_POINT ( 'NONE',  ( 14.47650479471827722, 14.49999999999999112, -3.928206833722049929 ) ) ;
#45120 = CARTESIAN_POINT ( 'NONE',  ( 12.91533473730992121, 4.522018677488169658, 10.88017736071110164 ) ) ;
#45121 = CARTESIAN_POINT ( 'NONE',  ( 7.084665262690076126, 34.10535201082151247, 10.88017736071109987 ) ) ;
#45122 = CARTESIAN_POINT ( 'NONE',  ( 19.42250999205614548, 65.98035201082151957, -5.440088680355545492 ) ) ;
#45123 = CARTESIAN_POINT ( 'NONE',  ( -4.164238869374099039, 31.80374883491396432, 8.674139862899312516E-16 ) ) ;
#45124 = EDGE_CURVE ( 'NONE', #83062, #34693, #87895, .T. ) ;
#45125 = CARTESIAN_POINT ( 'NONE',  ( 0.1532563361054100626, 25.80059781766744820, -2.638427012816831230 ) ) ;
#45126 = CARTESIAN_POINT ( 'NONE',  ( 15.44008868035555260, 44.73035201082151247, 9.422509992056143702 ) ) ;
#45127 = CARTESIAN_POINT ( 'NONE',  ( 69.60148758828984228, 0.4999999999999958922, -9.500000000000000000 ) ) ;
#45128 = CARTESIAN_POINT ( 'NONE',  ( -2.266590686148945544, 7.220415501580634832, 7.082119434687048631 ) ) ;
#45129 = ADVANCED_FACE ( 'NONE', ( #4437 ), #97493, .T. ) ;
#45130 = EDGE_LOOP ( 'NONE', ( #50171, #66076, #5324, #75641 ) ) ;
#45131 = VECTOR ( 'NONE', #12611, 1000.000000000000000 ) ;
#45132 = CARTESIAN_POINT ( 'NONE',  ( -14.82269085861172364, 14.49999999999999112, -2.299529454047143595 ) ) ;
#45133 = CARTESIAN_POINT ( 'NONE',  ( 5.076628168052703671, 56.84226448433412315, 8.527530157486179263 ) ) ;
#45134 = EDGE_LOOP ( 'NONE', ( #35077, #39386, #29470, #74189 ) ) ;
#45135 = ORIENTED_EDGE ( 'NONE', *, *, #3915, .F. ) ;
#45136 = CARTESIAN_POINT ( 'NONE',  ( 22.26659068614895176, 24.72041550158063572, -7.082119434687042414 ) ) ;
#45137 = CARTESIAN_POINT ( 'NONE',  ( 10.00000000000000178, 23.05374883491397142, 14.16423886937410082 ) ) ;
#45138 = CARTESIAN_POINT ( 'NONE',  ( 19.42250999205614548, 65.98035201082151957, -5.440088680355545492 ) ) ;
#45139 = CARTESIAN_POINT ( 'NONE',  ( 17.08211943468705840, 65.13708216824730357, -12.26659068614894466 ) ) ;
#45140 = CARTESIAN_POINT ( 'NONE',  ( 7.361572987183170547, 52.05059781766745175, 9.846743663894590881 ) ) ;
#45141 = CARTESIAN_POINT ( 'NONE',  ( -10.57481851842510778, -40.44832046089882738, 4.000000000000000000 ) ) ;
#45143 = CARTESIAN_POINT ( 'NONE',  ( -1.099225684535947600, 14.54030133659708568, 6.408140936763237150 ) ) ;
#45142 = CARTESIAN_POINT ( 'NONE',  ( 12.91533473730993009, 51.60535201082149825, -10.88017736071109987 ) ) ;
#45144 = CARTESIAN_POINT ( 'NONE',  ( 13.79529636645030344, 18.26208216824730002, 14.16423886937410614 ) ) ;
#45145 = CARTESIAN_POINT ( 'NONE',  ( 4.559911319644449179, 17.23035201082150536, -9.422509992056141925 ) ) ;
#45146 = CIRCLE ( 'NONE', #96261, 15.00000000000000000 ) ;
#45147 = AXIS2_PLACEMENT_3D ( 'NONE', #23206, #15214, #74197 ) ;
#45148 = CARTESIAN_POINT ( 'NONE',  ( 0.5774900079438607392, 23.48035201082150536, 5.440088680355550821 ) ) ;
#45149 = CARTESIAN_POINT ( 'NONE',  ( -1.926860441876562247, 2.453790035174471473, -3.195792623639530650 ) ) ;
#45150 = CARTESIAN_POINT ( 'NONE',  ( 7.084665262690076126, 52.02201867748816255, -10.88017736071110164 ) ) ;
#45151 = CIRCLE ( 'NONE', #35586, 14.49999999999999822 ) ;
#45152 = CARTESIAN_POINT ( 'NONE',  ( 3.469446951953614189E-15, -27.74106884899921255, 9.846743663894594434 ) ) ;
#45153 = ORIENTED_EDGE ( 'NONE', *, *, #59281, .T. ) ;
#45154 = DIRECTION ( 'NONE',  ( 0.000000000000000000, -0.000000000000000000, -1.000000000000000000 ) ) ;
#45155 = VECTOR ( 'NONE', #22379, 1000.000000000000114 ) ;
#45156 = VERTEX_POINT ( 'NONE', #19910 ) ;
#45157 = SURFACE_SIDE_STYLE ('',( #29648 ) ) ;
#45158 = DIRECTION ( 'NONE',  ( -0.000000000000000000, -0.000000000000000000, 1.000000000000000000 ) ) ;
#45159 = VERTEX_POINT ( 'NONE', #79436 ) ;
#45160 = DIRECTION ( 'NONE',  ( 0.000000000000000000, -1.000000000000000000, 0.000000000000000000 ) ) ;
#45162 = CARTESIAN_POINT ( 'NONE',  ( 20.36894250292379382, 58.67874883491396076, 10.36894250292379205 ) ) ;
#45161 = CARTESIAN_POINT ( 'NONE',  ( 17.08211943468705840, 65.13708216824730357, -12.26659068614894466 ) ) ;
#45164 = CARTESIAN_POINT ( 'NONE',  ( 5.076628168052703671, 61.84226448433412315, 8.527530157486179263 ) ) ;
#45163 = CARTESIAN_POINT ( 'NONE',  ( 0.1532563361054083140, 26.00893115100078745, 1.131784320476157264E-15 ) ) ;
#45165 = CARTESIAN_POINT ( 'NONE',  ( 20.32896413005680714, 50.57879003517447103, -5.963430220938276349 ) ) ;
#45166 = CARTESIAN_POINT ( 'NONE',  ( 19.72487221294571214, 44.78217586085236945, 6.499999999999993783 ) ) ;
#45167 = CARTESIAN_POINT ( 'NONE',  ( 17.96484262340118221, 66.18868534415483396, -7.964842623401177768 ) ) ;
#45168 = EDGE_CURVE ( 'NONE', #42904, #18090, #86351, .T. ) ;
#45169 = CARTESIAN_POINT ( 'NONE',  ( 12.81628187352647252, 16.83196800326375708, -3.434112377981059172 ) ) ;
#45170 = ADVANCED_FACE ( 'NONE', ( #71926 ), #48436, .T. ) ;
#45171 = ORIENTED_EDGE ( 'NONE', *, *, #49895, .F. ) ;
#45172 = CARTESIAN_POINT ( 'NONE',  ( 22.26659068614894466, 38.88708216824731068, 7.082119434687054849 ) ) ;
#45173 = ORIENTED_EDGE ( 'NONE', *, *, #71254, .T. ) ;
#45174 = CARTESIAN_POINT ( 'NONE',  ( -4.164238869374099927, 37.01208216824731068, 3.795296366450308767 ) ) ;
#45175 = ORIENTED_EDGE ( 'NONE', *, *, #63242, .F. ) ;
#45176 = VECTOR ( 'NONE', #84479, 1000.000000000000114 ) ;
#45177 = CARTESIAN_POINT ( 'NONE',  ( 21.09922568453595559, 52.04030133659708923, -6.408140936763230044 ) ) ;
#45178 = CARTESIAN_POINT ( 'NONE',  ( 10.00000000000000178, 24.31368534415484106, 10.88017736071110342 ) ) ;
#45179 = CARTESIAN_POINT ( 'NONE',  ( 1.472469842513823179, 45.59226448433412315, -4.923371831947296329 ) ) ;
#45180 = CARTESIAN_POINT ( 'NONE',  ( 10.00000000000000000, 31.81368534415483751, -10.88017736071110342 ) ) ;
#45181 =( BOUNDED_CURVE ( )  B_SPLINE_CURVE ( 2, ( #14206, #75182, #82025, #51034, #89038, #97061, #19557, #13535, #43049 ),
 .UNSPECIFIED., .F., .T. ) 
 B_SPLINE_CURVE_WITH_KNOTS ( ( 3, 2, 2, 2, 3 ),
 ( 0.4758552226545170183, 0.4761904761904762196, 0.4821428571428571508, 0.4880952380952381375, 0.4884304916311972833 ),
 .UNSPECIFIED. ) 
 CURVE ( )  GEOMETRIC_REPRESENTATION_ITEM ( )  RATIONAL_B_SPLINE_CURVE ( ( 0.9963778908391753841, 0.9980808541467917072, 1.000000000000000000, 0.9659258262890683122, 1.000000000000000000, 0.9659258262890683122, 1.000000000000000000, 0.9980808541467920403, 0.9963778908391759392 ) ) 
 REPRESENTATION_ITEM ( '' )  );
#45182 = CARTESIAN_POINT ( 'NONE',  ( 16.40814093676323893, 60.79030133659709634, 11.09922568453595026 ) ) ;
#45183 = DIRECTION ( 'NONE',  ( -0.000000000000000000, -0.000000000000000000, -1.000000000000000000 ) ) ;
#45184 = CARTESIAN_POINT ( 'NONE',  ( 14.92337183194729633, 57.67559781766745886, 8.527530157486181039 ) ) ;
#45185 = CARTESIAN_POINT ( 'NONE',  ( 18.52753015748617571, 53.09226448433412315, 4.923371831947298993 ) ) ;
#45186 =( BOUNDED_SURFACE ( )  B_SPLINE_SURFACE ( 1, 2, ( 
 ( #97100, #66571, #68060, #90056, #13569, #37073, #75553, #89568, #28571, #14577, #30039, #52067, #20586, #60047, #74561, #83554, #76043, #90545, #21077, #15077, #82061, #60547, #51071, #51575, #7069, #97592, #45546, #53038, #6077, #29052, #81563, #44056, #21579, #43562, #75054, #37569, #22077, #82562, #14078, #68554, #44558, #52552, #45044, #83056, #91040, #22569, #38062, #28070, #58567, #89072, #13070, #74060, #5593, #36070, #54513, #39042, #31999, #85026, #93008, #47016, #78507, #91546, #46527, #85521, #31517, #53532, #61034, #69046, #31025, #23561, #84046, #580, #61521, #55518, #25032, #9518, #69536, #70029, #24041, #1049, #10020, #54029, #30533, #23063, #86017, #38551, #62505, #84541, #92031, #2045, #16038, #8051, #40018, #77506, #55003, #17530, #47997, #40521, #15566, #46050, #86, #17032, #47510, #62016, #76536, #9020, #92516, #70522, #78011, #32506, #16539, #77027, #8541, #39537, #1553, #24542, #63004, #93506, #48491, #11480, #49967, #2540, #41012, #41997, #63498, #25524, #10499, #49468, #32996, #64951, #19477, #65452, #3026, #48983, #27460, #72958, #33474, #72461, #94973, #78994, #79492, #88460, #95479, #3995, #34460, #80473, #71512, #19961, #50456, #26967, #57468, #79974, #80962, #42474, #87961, #12462, #11971, #71018, #4487, #34954, #95977, #63971, #57953, #33961, #26475, #94000, #86986, #10992, #56010, #94483, #87476, #86514, #18011, #26001, #56496, #18495, #41513, #71979, #3504, #18991, #64466, #56973, #42967, #82933, #44433, #35947, #51451, #43445, #96477, #60421, #13447, #83430, #73448, #81449, #28929, #81937, #14451, #65950, #59926, #21452, #75429, #66443, #29916, #51949, #89935, #50954, #90915, #5475, #44921, #6943, #96977, #97965, #20963, #28451, #12950, #97464, #27950, #73946, #59433, #29421, #58442, #90414, #89450, #74936, #37449, #36947, #74431, #98461, #21956, #22445, #52435, #52918, #6437, #67940, #4974, #67446, #20465, #36452, #43934, #5959, #58948, #66944, #35454, #82434, #13959, #88956, #76899, #455, #92396, #62377, #76417, #53410, #1427, #54882, #38920, #7446, #16415, #61399, #70400, #62883, #23921, #83918, #1919, #68926, #46410, #15447, #15920, #929, #46892, #69408, #32378, #77383, #45928, #69907, #8896, #98956, #8414, #93380, #16907, #7932, #84902, #31391, #22943, #23435, #24907, #39412, #31880, #92883, #24416, #38428, #55390, #14949, #85394, #37944, #30905, #47382, #53914, #45418, #39897, #91910, #84423, #68434, #61891, #54390, #30412, #77881, #9393, #75922, #60913, #91417, #27337, #71863, #26356, #3872, #48370, #94362, #18380, #10875, #34336, #64345, #71391, #64832, #42358, #95350, #17886 ),
 ( #11356, #86384, #3375, #72833, #85891, #26848, #57344, #80352, #78377, #34836, #87357, #33836, #25881, #56857, #17405, #87838, #18871, #78875, #56382, #10383, #40402, #4371, #86871, #47873, #9898, #25401, #94855, #48859, #19356, #70896, #49840, #49352, #11849, #40888, #65329, #79855, #41876, #93875, #95855, #2904, #2413, #32872, #33354, #72340, #63850, #79368, #55887, #41397, #63371, #96358, #43813, #13829, #12341, #74812, #5353, #89811, #90294, #51821, #89328, #14328, #36826, #6816, #6318, #37332, #21332, #44310, #19840, #82307, #35330, #51326, #27829, #97342, #50329, #42846, #58315, #36326, #88342, #67317, #97842, #52314, #88831, #35831, #44800, #59802, #20342, #28815, #81810, #65824, #66317, #75304, #29307, #59313, #21831, #82806, #50839, #67822, #98338, #57833, #80841, #81332, #73330, #96853, #4856, #12828, #28329, #58819, #43326, #73819, #20838, #13329, #5833, #74308, #66819, #84309, #68807, #70285, #15809, #69296, #46776, #91291, #38310, #61285, #53794, #77269, #8298, #15325, #8780, #85280, #39297, #60791, #46294, #337, #61771, #76782, #23809, #38797, #9276, #22326, #76298, #16295, #91794, #83304, #90800, #98834, #22813, #53294, #14829, #30288, #83802, #16786, #54761, #69788, #30781, #817, #31271, #23314, #39786, #45807, #60307, #52801, #47261, #68314, #92286, #7815, #54270, #31768, #84786, #37821, #1317, #62262, #92768, #77761, #29796, #45305, #75800, #7318, #24295, #88584, #58080, #72589, #62758, #50098, #42123, #73574, #20092, #50596, #95604, #11120, #89083, #95097, #4123, #93262, #27590, #24786, #79618, #42604, #81088, #32256, #35080, #35590, #96106, #34586, #58581, #12589, #51084, #43089, #81575, #65579, #5099, #55261, #66078, #41638, #27090, #80101, #65080, #72104, #57102, #96606, #3631, #34098, #28083, #57593, #87598, #80603, #20597, #64589, #26605, #13082, #43577, #88090, #85776, #4618, #49588, #1801, #17286, #12101, #19109, #49117, #11606, #19603, #73082, #75067, #60057, #7079, #29552, #30544, #37581, #44066, #30051, #68074, #59073, #67584, #75566, #98601, #52562, #53545, #45559, #14587, #91557, #83568, #23076, #45056, #83067, #91051, #13582, #76057, #37085, #98093, #60560, #90066, #14088, #22578, #74573, #90558, #61044, #74070, #15088, #53049, #68566, #66584, #84058, #7586, #22087, #82574, #38075, #5602, #97, #15579, #67077, #44568, #6087, #28582, #36081, #6573, #97111, #89577, #36589, #21088, #51586, #82072, #97604, #29065, #59573, #21590, #52081, #55527, #39551, #70040, #92044, #86024, #46539, #40030, #70532, #77040, #85531, #1065, #16051, #23572, #47026, #592, #54041, #77517, #17043, #69056, #47522 ) ),
 .UNSPECIFIED., .F., .F., .T. ) 
 B_SPLINE_SURFACE_WITH_KNOTS ( ( 2, 2 ),
 ( 3, 2, 2, 2, 2, 2, 2, 2, 2, 2, 2, 2, 2, 2, 2, 2, 2, 2, 2, 2, 2, 2, 2, 2, 2, 2, 2, 2, 2, 2, 2, 2, 2, 2, 2, 2, 2, 2, 2, 2, 2, 2, 2, 2, 2, 2, 2, 2, 2, 2, 2, 2, 2, 2, 2, 2, 2, 2, 2, 2, 2, 2, 2, 2, 2, 2, 2, 2, 2, 2, 2, 2, 2, 2, 2, 2, 2, 2, 2, 2, 2, 2, 2, 2, 2, 2, 2, 2, 2, 2, 2, 2, 2, 2, 2, 2, 2, 2, 2, 2, 2, 2, 2, 2, 2, 2, 2, 2, 2, 2, 2, 2, 2, 2, 2, 2, 2, 2, 2, 2, 2, 2, 2, 2, 2, 2, 2, 2, 2, 2, 2, 2, 2, 2, 2, 2, 2, 2, 2, 2, 2, 2, 2, 2, 2, 2, 2, 2, 2, 2, 2, 2, 2, 2, 2, 2, 2, 2, 2, 2, 2, 2, 3 ),
 ( 0.000000000000000000, 1.000000000000000000 ),
 ( 0.000000000000000000, 0.005952380952380952051, 0.01190476190476190410, 0.01785714285714285615, 0.02380952380952380820, 0.02976190476190476025, 0.03571428571428571230, 0.04166666666666666435, 0.04761904761904761640, 0.05357142857142856845, 0.05952380952380952051, 0.06547619047619047949, 0.07142857142857142461, 0.07738095238095238360, 0.08333333333333332871, 0.08928571428571428770, 0.09523809523809523281, 0.1011904761904761918, 0.1071428571428571369, 0.1130952380952380959, 0.1190476190476190410, 0.1250000000000000000, 0.1309523809523809590, 0.1369047619047619180, 0.1428571428571428492, 0.1488095238095238082, 0.1547619047619047672, 0.1607142857142857262, 0.1666666666666666574, 0.1726190476190476164, 0.1785714285714285754, 0.1845238095238095344, 0.1904761904761904656, 0.1964285714285714246, 0.2023809523809523836, 0.2083333333333333426, 0.2142857142857142738, 0.2202380952380952328, 0.2261904761904761918, 0.2321428571428571508, 0.2380952380952380820, 0.2440476190476190410, 0.2500000000000000000, 0.2559523809523809312, 0.2619047619047619180, 0.2678571428571428492, 0.2738095238095238360, 0.2797619047619047672, 0.2857142857142856984, 0.2916666666666666852, 0.2976190476190476164, 0.3035714285714285476, 0.3095238095238095344, 0.3154761904761904656, 0.3214285714285714524, 0.3273809523809523836, 0.3333333333333333148, 0.3392857142857143016, 0.3452380952380952328, 0.3511904761904761640, 0.3571428571428571508, 0.3630952380952380820, 0.3690476190476190688, 0.3750000000000000000, 0.3809523809523809312, 0.3869047619047619180, 0.3928571428571428492, 0.3988095238095238360, 0.4047619047619047672, 0.4107142857142856984, 0.4166666666666666852, 0.4226190476190476164, 0.4285714285714285476, 0.4345238095238095344, 0.4404761904761904656, 0.4464285714285714524, 0.4523809523809523836, 0.4583333333333333148, 0.4642857142857143016, 0.4702380952380952328, 0.4761904761904761640, 0.4821428571428571508, 0.4880952380952380820, 0.4940476190476190688, 0.5000000000000000000, 0.5059523809523809312, 0.5119047619047618625, 0.5178571428571429047, 0.5238095238095238360, 0.5297619047619047672, 0.5357142857142856984, 0.5416666666666666297, 0.5476190476190476719, 0.5535714285714286031, 0.5595238095238095344, 0.5654761904761904656, 0.5714285714285713969, 0.5773809523809523281, 0.5833333333333333703, 0.5892857142857143016, 0.5952380952380952328, 0.6011904761904761640, 0.6071428571428570953, 0.6130952380952381375, 0.6190476190476190688, 0.6250000000000000000, 0.6309523809523809312, 0.6369047619047618625, 0.6428571428571429047, 0.6488095238095238360, 0.6547619047619047672, 0.6607142857142856984, 0.6666666666666666297, 0.6726190476190476719, 0.6785714285714286031, 0.6845238095238095344, 0.6904761904761904656, 0.6964285714285713969, 0.7023809523809523281, 0.7083333333333333703, 0.7142857142857143016, 0.7202380952380952328, 0.7261904761904761640, 0.7321428571428570953, 0.7380952380952381375, 0.7440476190476190688, 0.7500000000000000000, 0.7559523809523809312, 0.7619047619047618625, 0.7678571428571429047, 0.7738095238095238360, 0.7797619047619047672, 0.7857142857142856984, 0.7916666666666666297, 0.7976190476190476719, 0.8035714285714286031, 0.8095238095238095344, 0.8154761904761904656, 0.8214285714285713969, 0.8273809523809523281, 0.8333333333333333703, 0.8392857142857143016, 0.8452380952380952328, 0.8511904761904761640, 0.8571428571428570953, 0.8630952380952381375, 0.8690476190476190688, 0.8750000000000000000, 0.8809523809523809312, 0.8869047619047618625, 0.8928571428571429047, 0.8988095238095238360, 0.9047619047619047672, 0.9107142857142856984, 0.9166666666666666297, 0.9226190476190476719, 0.9285714285714286031, 0.9345238095238095344, 0.9404761904761904656, 0.9464285714285713969, 0.9523809523809523281, 0.9583333333333333703, 0.9642857142857143016 ),
 .UNSPECIFIED. ) 
 GEOMETRIC_REPRESENTATION_ITEM ( )  RATIONAL_B_SPLINE_SURFACE ( (
 ( 1.000000000000000000, 0.9659258262890683122, 1.000000000000000000, 0.9659258262890683122, 1.000000000000000000, 0.9659258262890683122, 1.000000000000000000, 0.9659258262890683122, 1.000000000000000000, 0.9659258262890683122, 1.000000000000000000, 0.9659258262890683122, 1.000000000000000000, 0.9659258262890683122, 1.000000000000000000, 0.9659258262890683122, 1.000000000000000000, 0.9659258262890683122, 1.000000000000000000, 0.9659258262890683122, 1.000000000000000000, 0.9659258262890683122, 1.000000000000000000, 0.9659258262890683122, 1.000000000000000000, 0.9659258262890683122, 1.000000000000000000, 0.9659258262890683122, 1.000000000000000000, 0.9659258262890683122, 1.000000000000000000, 0.9659258262890683122, 1.000000000000000000, 0.9659258262890683122, 1.000000000000000000, 0.9659258262890683122, 1.000000000000000000, 0.9659258262890683122, 1.000000000000000000, 0.9659258262890683122, 1.000000000000000000, 0.9659258262890683122, 1.000000000000000000, 0.9659258262890683122, 1.000000000000000000, 0.9659258262890683122, 1.000000000000000000, 0.9659258262890683122, 1.000000000000000000, 0.9659258262890683122, 1.000000000000000000, 0.9659258262890683122, 1.000000000000000000, 0.9659258262890683122, 1.000000000000000000, 0.9659258262890683122, 1.000000000000000000, 0.9659258262890683122, 1.000000000000000000, 0.9659258262890683122, 1.000000000000000000, 0.9659258262890683122, 1.000000000000000000, 0.9659258262890683122, 1.000000000000000000, 0.9659258262890683122, 1.000000000000000000, 0.9659258262890683122, 1.000000000000000000, 0.9659258262890683122, 1.000000000000000000, 0.9659258262890683122, 1.000000000000000000, 0.9659258262890683122, 1.000000000000000000, 0.9659258262890683122, 1.000000000000000000, 0.9659258262890683122, 1.000000000000000000, 0.9659258262890683122, 1.000000000000000000, 0.9659258262890683122, 1.000000000000000000, 0.9659258262890683122, 1.000000000000000000, 0.9659258262890683122, 1.000000000000000000, 0.9659258262890683122, 1.000000000000000000, 0.9659258262890683122, 1.000000000000000000, 0.9659258262890683122, 1.000000000000000000, 0.9659258262890683122, 1.000000000000000000, 0.9659258262890683122, 1.000000000000000000, 0.9659258262890683122, 1.000000000000000000, 0.9659258262890683122, 1.000000000000000000, 0.9659258262890683122, 1.000000000000000000, 0.9659258262890683122, 1.000000000000000000, 0.9659258262890683122, 1.000000000000000000, 0.9659258262890683122, 1.000000000000000000, 0.9659258262890683122, 1.000000000000000000, 0.9659258262890683122, 1.000000000000000000, 0.9659258262890683122, 1.000000000000000000, 0.9659258262890683122, 1.000000000000000000, 0.9659258262890683122, 1.000000000000000000, 0.9659258262890683122, 1.000000000000000000, 0.9659258262890683122, 1.000000000000000000, 0.9659258262890683122, 1.000000000000000000, 0.9659258262890683122, 1.000000000000000000, 0.9659258262890683122, 1.000000000000000000, 0.9659258262890683122, 1.000000000000000000, 0.9659258262890683122, 1.000000000000000000, 0.9659258262890683122, 1.000000000000000000, 0.9659258262890683122, 1.000000000000000000, 0.9659258262890683122, 1.000000000000000000, 0.9659258262890683122, 1.000000000000000000, 0.9659258262890683122, 1.000000000000000000, 0.9659258262890683122, 1.000000000000000000, 0.9659258262890683122, 1.000000000000000000, 0.9659258262890683122, 1.000000000000000000, 0.9659258262890683122, 1.000000000000000000, 0.9659258262890683122, 1.000000000000000000, 0.9659258262890683122, 1.000000000000000000, 0.9659258262890683122, 1.000000000000000000, 0.9659258262890683122, 1.000000000000000000, 0.9659258262890683122, 1.000000000000000000, 0.9659258262890683122, 1.000000000000000000, 0.9659258262890683122, 1.000000000000000000, 0.9659258262890683122, 1.000000000000000000, 0.9659258262890683122, 1.000000000000000000, 0.9659258262890683122, 1.000000000000000000, 0.9659258262890683122, 1.000000000000000000, 0.9659258262890683122, 1.000000000000000000, 0.9659258262890683122, 1.000000000000000000, 0.9659258262890683122, 1.000000000000000000, 0.9659258262890683122, 1.000000000000000000, 0.9659258262890683122, 1.000000000000000000, 0.9659258262890683122, 1.000000000000000000, 0.9659258262890683122, 1.000000000000000000, 0.9659258262890683122, 1.000000000000000000, 0.9659258262890683122, 1.000000000000000000, 0.9659258262890683122, 1.000000000000000000, 0.9659258262890683122, 1.000000000000000000, 0.9659258262890683122, 1.000000000000000000, 0.9659258262890683122, 1.000000000000000000, 0.9659258262890683122, 1.000000000000000000, 0.9659258262890683122, 1.000000000000000000, 0.9659258262890683122, 1.000000000000000000, 0.9659258262890683122, 1.000000000000000000, 0.9659258262890683122, 1.000000000000000000, 0.9659258262890683122, 1.000000000000000000, 0.9659258262890683122, 1.000000000000000000, 0.9659258262890683122, 1.000000000000000000, 0.9659258262890683122, 1.000000000000000000, 0.9659258262890683122, 1.000000000000000000, 0.9659258262890683122, 1.000000000000000000, 0.9659258262890683122, 1.000000000000000000, 0.9659258262890683122, 1.000000000000000000, 0.9659258262890683122, 1.000000000000000000, 0.9659258262890683122, 1.000000000000000000, 0.9659258262890683122, 1.000000000000000000, 0.9659258262890683122, 1.000000000000000000, 0.9659258262890683122, 1.000000000000000000, 0.9659258262890683122, 1.000000000000000000, 0.9659258262890683122, 1.000000000000000000, 0.9659258262890683122, 1.000000000000000000, 0.9659258262890683122, 1.000000000000000000, 0.9659258262890683122, 1.000000000000000000, 0.9659258262890683122, 1.000000000000000000, 0.9659258262890683122, 1.000000000000000000, 0.9659258262890683122, 1.000000000000000000, 0.9659258262890683122, 1.000000000000000000, 0.9659258262890683122, 1.000000000000000000, 0.9659258262890683122, 1.000000000000000000, 0.9659258262890683122, 1.000000000000000000, 0.9659258262890683122, 1.000000000000000000, 0.9659258262890683122, 1.000000000000000000, 0.9659258262890683122, 1.000000000000000000, 0.9659258262890683122, 1.000000000000000000, 0.9659258262890683122, 1.000000000000000000, 0.9659258262890683122, 1.000000000000000000, 0.9659258262890683122, 1.000000000000000000, 0.9659258262890683122, 1.000000000000000000, 0.9659258262890683122, 1.000000000000000000, 0.9659258262890683122, 1.000000000000000000, 0.9659258262890683122, 1.000000000000000000, 0.9659258262890683122, 1.000000000000000000, 0.9659258262890683122, 1.000000000000000000, 0.9659258262890683122, 1.000000000000000000, 0.9659258262890683122, 1.000000000000000000, 0.9659258262890683122, 1.000000000000000000, 0.9659258262890683122, 1.000000000000000000, 0.9659258262890683122, 1.000000000000000000, 0.9659258262890683122, 1.000000000000000000, 0.9659258262890683122, 1.000000000000000000, 0.9659258262890683122, 1.000000000000000000, 0.9659258262890683122, 1.000000000000000000, 0.9659258262890683122, 1.000000000000000000, 0.9659258262890683122, 1.000000000000000000, 0.9659258262890683122, 1.000000000000000000, 0.9659258262890683122, 1.000000000000000000, 0.9659258262890683122, 1.000000000000000000, 0.9659258262890683122, 1.000000000000000000, 0.9659258262890683122, 1.000000000000000000, 0.9659258262890683122, 1.000000000000000000, 0.9659258262890683122, 1.000000000000000000, 0.9659258262890683122, 1.000000000000000000, 0.9659258262890683122, 1.000000000000000000),
 ( 1.000000000000000000, 0.9659258262890683122, 1.000000000000000000, 0.9659258262890683122, 1.000000000000000000, 0.9659258262890683122, 1.000000000000000000, 0.9659258262890683122, 1.000000000000000000, 0.9659258262890683122, 1.000000000000000000, 0.9659258262890683122, 1.000000000000000000, 0.9659258262890683122, 1.000000000000000000, 0.9659258262890683122, 1.000000000000000000, 0.9659258262890683122, 1.000000000000000000, 0.9659258262890683122, 1.000000000000000000, 0.9659258262890683122, 1.000000000000000000, 0.9659258262890683122, 1.000000000000000000, 0.9659258262890683122, 1.000000000000000000, 0.9659258262890683122, 1.000000000000000000, 0.9659258262890683122, 1.000000000000000000, 0.9659258262890683122, 1.000000000000000000, 0.9659258262890683122, 1.000000000000000000, 0.9659258262890683122, 1.000000000000000000, 0.9659258262890683122, 1.000000000000000000, 0.9659258262890683122, 1.000000000000000000, 0.9659258262890683122, 1.000000000000000000, 0.9659258262890683122, 1.000000000000000000, 0.9659258262890683122, 1.000000000000000000, 0.9659258262890683122, 1.000000000000000000, 0.9659258262890683122, 1.000000000000000000, 0.9659258262890683122, 1.000000000000000000, 0.9659258262890683122, 1.000000000000000000, 0.9659258262890683122, 1.000000000000000000, 0.9659258262890683122, 1.000000000000000000, 0.9659258262890683122, 1.000000000000000000, 0.9659258262890683122, 1.000000000000000000, 0.9659258262890683122, 1.000000000000000000, 0.9659258262890683122, 1.000000000000000000, 0.9659258262890683122, 1.000000000000000000, 0.9659258262890683122, 1.000000000000000000, 0.9659258262890683122, 1.000000000000000000, 0.9659258262890683122, 1.000000000000000000, 0.9659258262890683122, 1.000000000000000000, 0.9659258262890683122, 1.000000000000000000, 0.9659258262890683122, 1.000000000000000000, 0.9659258262890683122, 1.000000000000000000, 0.9659258262890683122, 1.000000000000000000, 0.9659258262890683122, 1.000000000000000000, 0.9659258262890683122, 1.000000000000000000, 0.9659258262890683122, 1.000000000000000000, 0.9659258262890683122, 1.000000000000000000, 0.9659258262890683122, 1.000000000000000000, 0.9659258262890683122, 1.000000000000000000, 0.9659258262890683122, 1.000000000000000000, 0.9659258262890683122, 1.000000000000000000, 0.9659258262890683122, 1.000000000000000000, 0.9659258262890683122, 1.000000000000000000, 0.9659258262890683122, 1.000000000000000000, 0.9659258262890683122, 1.000000000000000000, 0.9659258262890683122, 1.000000000000000000, 0.9659258262890683122, 1.000000000000000000, 0.9659258262890683122, 1.000000000000000000, 0.9659258262890683122, 1.000000000000000000, 0.9659258262890683122, 1.000000000000000000, 0.9659258262890683122, 1.000000000000000000, 0.9659258262890683122, 1.000000000000000000, 0.9659258262890683122, 1.000000000000000000, 0.9659258262890683122, 1.000000000000000000, 0.9659258262890683122, 1.000000000000000000, 0.9659258262890683122, 1.000000000000000000, 0.9659258262890683122, 1.000000000000000000, 0.9659258262890683122, 1.000000000000000000, 0.9659258262890683122, 1.000000000000000000, 0.9659258262890683122, 1.000000000000000000, 0.9659258262890683122, 1.000000000000000000, 0.9659258262890683122, 1.000000000000000000, 0.9659258262890683122, 1.000000000000000000, 0.9659258262890683122, 1.000000000000000000, 0.9659258262890683122, 1.000000000000000000, 0.9659258262890683122, 1.000000000000000000, 0.9659258262890683122, 1.000000000000000000, 0.9659258262890683122, 1.000000000000000000, 0.9659258262890683122, 1.000000000000000000, 0.9659258262890683122, 1.000000000000000000, 0.9659258262890683122, 1.000000000000000000, 0.9659258262890683122, 1.000000000000000000, 0.9659258262890683122, 1.000000000000000000, 0.9659258262890683122, 1.000000000000000000, 0.9659258262890683122, 1.000000000000000000, 0.9659258262890683122, 1.000000000000000000, 0.9659258262890683122, 1.000000000000000000, 0.9659258262890683122, 1.000000000000000000, 0.9659258262890683122, 1.000000000000000000, 0.9659258262890683122, 1.000000000000000000, 0.9659258262890683122, 1.000000000000000000, 0.9659258262890683122, 1.000000000000000000, 0.9659258262890683122, 1.000000000000000000, 0.9659258262890683122, 1.000000000000000000, 0.9659258262890683122, 1.000000000000000000, 0.9659258262890683122, 1.000000000000000000, 0.9659258262890683122, 1.000000000000000000, 0.9659258262890683122, 1.000000000000000000, 0.9659258262890683122, 1.000000000000000000, 0.9659258262890683122, 1.000000000000000000, 0.9659258262890683122, 1.000000000000000000, 0.9659258262890683122, 1.000000000000000000, 0.9659258262890683122, 1.000000000000000000, 0.9659258262890683122, 1.000000000000000000, 0.9659258262890683122, 1.000000000000000000, 0.9659258262890683122, 1.000000000000000000, 0.9659258262890683122, 1.000000000000000000, 0.9659258262890683122, 1.000000000000000000, 0.9659258262890683122, 1.000000000000000000, 0.9659258262890683122, 1.000000000000000000, 0.9659258262890683122, 1.000000000000000000, 0.9659258262890683122, 1.000000000000000000, 0.9659258262890683122, 1.000000000000000000, 0.9659258262890683122, 1.000000000000000000, 0.9659258262890683122, 1.000000000000000000, 0.9659258262890683122, 1.000000000000000000, 0.9659258262890683122, 1.000000000000000000, 0.9659258262890683122, 1.000000000000000000, 0.9659258262890683122, 1.000000000000000000, 0.9659258262890683122, 1.000000000000000000, 0.9659258262890683122, 1.000000000000000000, 0.9659258262890683122, 1.000000000000000000, 0.9659258262890683122, 1.000000000000000000, 0.9659258262890683122, 1.000000000000000000, 0.9659258262890683122, 1.000000000000000000, 0.9659258262890683122, 1.000000000000000000, 0.9659258262890683122, 1.000000000000000000, 0.9659258262890683122, 1.000000000000000000, 0.9659258262890683122, 1.000000000000000000, 0.9659258262890683122, 1.000000000000000000, 0.9659258262890683122, 1.000000000000000000, 0.9659258262890683122, 1.000000000000000000, 0.9659258262890683122, 1.000000000000000000, 0.9659258262890683122, 1.000000000000000000, 0.9659258262890683122, 1.000000000000000000, 0.9659258262890683122, 1.000000000000000000, 0.9659258262890683122, 1.000000000000000000, 0.9659258262890683122, 1.000000000000000000, 0.9659258262890683122, 1.000000000000000000, 0.9659258262890683122, 1.000000000000000000, 0.9659258262890683122, 1.000000000000000000, 0.9659258262890683122, 1.000000000000000000, 0.9659258262890683122, 1.000000000000000000, 0.9659258262890683122, 1.000000000000000000, 0.9659258262890683122, 1.000000000000000000, 0.9659258262890683122, 1.000000000000000000, 0.9659258262890683122, 1.000000000000000000, 0.9659258262890683122, 1.000000000000000000, 0.9659258262890683122, 1.000000000000000000, 0.9659258262890683122, 1.000000000000000000, 0.9659258262890683122, 1.000000000000000000, 0.9659258262890683122, 1.000000000000000000, 0.9659258262890683122, 1.000000000000000000, 0.9659258262890683122, 1.000000000000000000, 0.9659258262890683122, 1.000000000000000000, 0.9659258262890683122, 1.000000000000000000, 0.9659258262890683122, 1.000000000000000000, 0.9659258262890683122, 1.000000000000000000, 0.9659258262890683122, 1.000000000000000000, 0.9659258262890683122, 1.000000000000000000, 0.9659258262890683122, 1.000000000000000000, 0.9659258262890683122, 1.000000000000000000, 0.9659258262890683122, 1.000000000000000000) ) ) 
 REPRESENTATION_ITEM ( '' )  SURFACE ( )  );
#45188 = VERTEX_POINT ( 'NONE', #80911 ) ;
#45187 = CARTESIAN_POINT ( 'NONE',  ( 7.264948169187460003, 0.2306972965111908080, -13.05597881399718929 ) ) ;
#45189 = CIRCLE ( 'NONE', #49970, 15.00000000000000000 ) ;
#45190 = CARTESIAN_POINT ( 'NONE',  ( -3.384479038598405154, 14.76984929998922347, 14.55223509985375863 ) ) ;
#45191 = CARTESIAN_POINT ( 'NONE',  ( 1.087200977609890096, 0.000000000000000000, 5.343763529286935210 ) ) ;
#45192 = PRESENTATION_STYLE_ASSIGNMENT (( #91179 ) ) ;
#45193 = ORIENTED_EDGE ( 'NONE', *, *, #80725, .T. ) ;
#45194 = CARTESIAN_POINT ( 'NONE',  ( 12.26500600480481040, 44.99999999999999289, 0.000000000000000000 ) ) ;
#45195 = CARTESIAN_POINT ( 'NONE',  ( 17.20831665107776587, 37.88393115100078745, 7.208316651077764980 ) ) ;
#45196 = DIRECTION ( 'NONE',  ( 0.08715574274765112983, 0.9961946980917461003, 0.000000000000000000 ) ) ;
#45197 = CARTESIAN_POINT ( 'NONE',  ( 67.06412365047464164, 26.99999999999998224, 9.500000000000000000 ) ) ;
#45198 = EDGE_CURVE ( 'NONE', #41466, #11855, #60782, .T. ) ;
#45199 = DIRECTION ( 'NONE',  ( 1.000000000000000000, 0.000000000000000000, 0.000000000000000000 ) ) ;
#45200 = ORIENTED_EDGE ( 'NONE', *, *, #65693, .T. ) ;
#45201 = CARTESIAN_POINT ( 'NONE',  ( 18.52753015748617571, 53.09226448433412315, 4.923371831947298993 ) ) ;
#45202 = CARTESIAN_POINT ( 'NONE',  ( 0.2751277870542875315, 65.30223176428830811, 6.499999999999984901 ) ) ;
#45203 = CARTESIAN_POINT ( 'NONE',  ( 17.20831665107776587, 44.13393115100078745, -7.208316651077762316 ) ) ;
#45204 = CARTESIAN_POINT ( 'NONE',  ( 20.36894250292379382, 28.67874883491396787, 10.36894250292379205 ) ) ;
#45205 = CARTESIAN_POINT ( 'NONE',  ( 14.92337183194729633, 42.67559781766745886, 8.527530157486181039 ) ) ;
#45206 = CARTESIAN_POINT ( 'NONE',  ( 22.81628187352647785, 56.62363466993042493, 6.195893100308588602E-16 ) ) ;
#45207 = FACE_OUTER_BOUND ( 'NONE', #79826, .T. ) ;
#45208 = CARTESIAN_POINT ( 'NONE',  ( 1.472469842513823179, 6.425597817667451750, 4.923371831947296329 ) ) ;
#45209 = CARTESIAN_POINT ( 'NONE',  ( 21.92686044187656336, 46.97997603579418069, 3.195792623639536423 ) ) ;
#45210 = CARTESIAN_POINT ( 'NONE',  ( 1.472469842513823179, 45.59226448433412315, -4.923371831947296329 ) ) ;
#45211 = CARTESIAN_POINT ( 'NONE',  ( 20.88017736071110164, 60.35535201082151957, 2.915334737309930979 ) ) ;
#45212 = CARTESIAN_POINT ( 'NONE',  ( 2.791683348922237240, 40.38393115100078035, -7.208316651077763204 ) ) ;
#45213 = DIRECTION ( 'NONE',  ( -0.000000000000000000, 0.000000000000000000, 1.000000000000000000 ) ) ;
#45214 = CARTESIAN_POINT ( 'NONE',  ( 10.00000000000000000, 51.81368534415484106, -10.88017736071110342 ) ) ;
#45215 = AXIS2_PLACEMENT_3D ( 'NONE', #1066, #31530, #70533 ) ;
#45216 = ORIENTED_EDGE ( 'NONE', *, *, #86362, .T. ) ;
#45217 = LINE ( 'NONE', #46209, #93622 ) ;
#45218 = CARTESIAN_POINT ( 'NONE',  ( 20.88017736071110519, 15.56368534415483751, 2.639326808657452039E-16 ) ) ;
#45220 = CARTESIAN_POINT ( 'NONE',  ( 19.42250999205614193, 45.14701867748817676, 5.440088680355555262 ) ) ;
#45219 = CARTESIAN_POINT ( 'NONE',  ( 10.00000000000000178, 0.3736346699304200492, 12.81628187352647608 ) ) ;
#45221 = CARTESIAN_POINT ( 'NONE',  ( 19.84674366389459266, 13.71726448433411782, -2.638427012816827677 ) ) ;
#45222 = CARTESIAN_POINT ( 'NONE',  ( -46.34323875807881166, 103.6109741468810483, -6.190393423093146552 ) ) ;
#45224 = FACE_OUTER_BOUND ( 'NONE', #20830, .T. ) ;
#45223 = CARTESIAN_POINT ( 'NONE',  ( 17.96484262340118221, 34.93868534415482685, 7.964842623401181321 ) ) ;
#45225 = CARTESIAN_POINT ( 'NONE',  ( 18.52753015748618282, 8.925597817667451750, -4.923371831947291888 ) ) ;
#45226 = CARTESIAN_POINT ( 'NONE',  ( 19.84674366389459266, 33.30059781766744464, 2.638427012816836559 ) ) ;
#45227 = VECTOR ( 'NONE', #88847, 1000.000000000000000 ) ;
#45228 = CARTESIAN_POINT ( 'NONE',  ( -14.16423886937410437, 21.59541550158063927, -3.795296366450299885 ) ) ;
#45229 = CARTESIAN_POINT ( 'NONE',  ( 5.076628168052703671, 66.84226448433412315, 8.527530157486179263 ) ) ;
#45230 = CARTESIAN_POINT ( 'NONE',  ( 15.44008868035555793, 6.397018677488171434, -9.422509992056140149 ) ) ;
#45231 = FILL_AREA_STYLE ('',( #52728 ) ) ;
#45232 = CARTESIAN_POINT ( 'NONE',  ( 22.26659068614894466, 23.88708216824730357, 7.082119434687054849 ) ) ;
#45233 = CARTESIAN_POINT ( 'NONE',  ( 22.26659068614895176, 44.72041550158063927, -7.082119434687042414 ) ) ;
#45234 = FILL_AREA_STYLE_COLOUR ( '', #88787 ) ;
#45235 = B_SPLINE_CURVE_WITH_KNOTS ( 'NONE', 3,
 ( #675, #17141, #40122, #24143, #23164, #24637 ),
 .UNSPECIFIED., .F., .F.,
 ( 4, 2, 4 ),
 ( 0.0002800392683662262074, 0.0006862448819792434616, 0.001092450495592260824 ),
 .UNSPECIFIED. ) ;
#45236 = ORIENTED_EDGE ( 'NONE', *, *, #34055, .T. ) ;
#45237 = CARTESIAN_POINT ( 'NONE',  ( 19.84674366389459266, 28.71726448433411960, -2.638427012816827677 ) ) ;
#45238 = CARTESIAN_POINT ( 'NONE',  ( -0.8801773607110991993, 32.85535201082151247, -2.915334737309923874 ) ) ;
#45239 = CARTESIAN_POINT ( 'NONE',  ( 19.84674366389459266, 48.30059781766745175, 2.638427012816836559 ) ) ;
#45241 = CARTESIAN_POINT ( 'NONE',  ( 19.72487221294571569, 47.80223176428831522, -6.499999999999982236 ) ) ;
#45240 = CARTESIAN_POINT ( 'NONE',  ( 24.16423886937410614, 9.303748834913967869, 8.672049930838204340E-16 ) ) ;
#45242 = LINE ( 'NONE', #7258, #40767 ) ;
#45243 = FILL_AREA_STYLE ('',( #14770 ) ) ;
#45244 = CARTESIAN_POINT ( 'NONE',  ( 10.00000000000000178, 40.37363466993042493, 12.81628187352647608 ) ) ;
#45245 = CARTESIAN_POINT ( 'NONE',  ( 1.472469842513823179, 35.59226448433412315, -4.923371831947296329 ) ) ;
#45246 = VERTEX_POINT ( 'NONE', #79915 ) ;
#45247 = CARTESIAN_POINT ( 'NONE',  ( 18.52753015748618282, 13.92559781766745175, -4.923371831947291888 ) ) ;
#45248 = CARTESIAN_POINT ( 'NONE',  ( 10.64413412520849000, -97.62783346105426574, -4.000000000000000000 ) ) ;
#45249 = CARTESIAN_POINT ( 'NONE',  ( 19.80448550324508261, 16.82703681773341131, 6.500000000002789768 ) ) ;
#45250 = CARTESIAN_POINT ( 'NONE',  ( 15.44008868035555793, 6.397018677488171434, -9.422509992056140149 ) ) ;
#45251 = CARTESIAN_POINT ( 'NONE',  ( 2.917880565312950480, 50.97041550158064638, -12.26659068614894821 ) ) ;
#45252 = CARTESIAN_POINT ( 'NONE',  ( -4.164238869374098151, 1.595415501580634388, -3.795296366450310543 ) ) ;
#45253 = CARTESIAN_POINT ( 'NONE',  ( -12.11353679309445219, 0.04962889481943084935, 8.421373815019547848 ) ) ;
#45254 = CARTESIAN_POINT ( 'NONE',  ( 19.84674366389459266, 28.71726448433411960, -2.638427012816827677 ) ) ;
#45255 = CARTESIAN_POINT ( 'NONE',  ( 0.5774900079438607392, 3.480352010821504027, 5.440088680355550821 ) ) ;
#45256 = CARTESIAN_POINT ( 'NONE',  ( 17.20831665107776587, 44.13393115100078745, -7.208316651077762316 ) ) ;
#45257 =( NAMED_UNIT ( * ) SI_UNIT ( $, .STERADIAN. ) SOLID_ANGLE_UNIT ( ) );
#45258 = CARTESIAN_POINT ( 'NONE',  ( 7.361572987183170547, 52.05059781766745175, 9.846743663894590881 ) ) ;
#45259 = EDGE_CURVE ( 'NONE', #45656, #26776, #34403, .T. ) ;
#45260 = AXIS2_PLACEMENT_3D ( 'NONE', #25697, #70205, #17214 ) ;
#45261 = EDGE_CURVE ( 'NONE', #60216, #46867, #76697, .T. ) ;
#45262 = CARTESIAN_POINT ( 'NONE',  ( -0.8801773607111008646, 33.27201867748817676, 2.915334737309923430 ) ) ;
#45263 = UNCERTAINTY_MEASURE_WITH_UNIT (LENGTH_MEASURE( 1.000000000000000082E-05 ), #11799, 'distance_accuracy_value', 'NONE');
#45264 = ORIENTED_EDGE ( 'NONE', *, *, #28572, .T. ) ;
#45265 = CARTESIAN_POINT ( 'NONE',  ( 3.591859063236763294, 53.29030133659708923, -11.09922568453595026 ) ) ;
#45266 = CARTESIAN_POINT ( 'NONE',  ( 0.000000000000000000, 14.49999999999999822, 0.000000000000000000 ) ) ;
#45267 = CARTESIAN_POINT ( 'NONE',  ( 19.84674366389459266, 8.717264484334116048, -2.638427012816827677 ) ) ;
#45268 = CARTESIAN_POINT ( 'NONE',  ( -1.099225684535947600, 59.54030133659708923, 6.408140936763237150 ) ) ;
#45270 = CARTESIAN_POINT ( 'NONE',  ( 19.84674366389459266, 43.30059781766744464, 2.638427012816836559 ) ) ;
#45269 = CARTESIAN_POINT ( 'NONE',  ( 15.44008868035555793, 6.397018677488171434, -9.422509992056140149 ) ) ;
#45271 = LINE ( 'NONE', #75766, #39059 ) ;
#45272 = DIRECTION ( 'NONE',  ( -0.000000000000000000, -0.000000000000000000, 1.000000000000000000 ) ) ;
#45273 = CARTESIAN_POINT ( 'NONE',  ( 20.36894250292379738, 34.92874883491396076, -10.36894250292379027 ) ) ;
#45274 = CARTESIAN_POINT ( 'NONE',  ( 13.79529636645030344, 43.26208216824730357, 14.16423886937410614 ) ) ;
#45275 = CARTESIAN_POINT ( 'NONE',  ( 17.20831665107776587, 59.13393115100078745, -7.208316651077762316 ) ) ;
#45276 = CARTESIAN_POINT ( 'NONE',  ( 17.41414817163570916, 33.99863903001855903, 9.761180582272331208 ) ) ;
#45277 = CARTESIAN_POINT ( 'NONE',  ( 10.00000000000000000, 56.81368534415484106, -10.88017736071110342 ) ) ;
#45278 = CARTESIAN_POINT ( 'NONE',  ( 0.1532563361054082862, 6.217264484334118713, 2.638427012816831674 ) ) ;
#45279 = PRESENTATION_STYLE_ASSIGNMENT (( #45783 ) ) ;
#45280 = ORIENTED_EDGE ( 'NONE', *, *, #74271, .T. ) ;
#45281 = CARTESIAN_POINT ( 'NONE',  ( 22.81628187352648496, 61.83196800326376774, -3.434112377981050290 ) ) ;
#45282 = ORIENTED_EDGE ( 'NONE', *, *, #4099, .T. ) ;
#45283 = CARTESIAN_POINT ( 'NONE',  ( -0.8801773607111008646, 68.27201867748817676, 2.915334737309923430 ) ) ;
#45284 = ORIENTED_EDGE ( 'NONE', *, *, #69793, .F. ) ;
#45285 = CARTESIAN_POINT ( 'NONE',  ( 22.26659068614894466, 8.887082168247300018, 7.082119434687054849 ) ) ;
#45286 = CARTESIAN_POINT ( 'NONE',  ( 18.52753015748617571, 8.092264484334117824, 4.923371831947298993 ) ) ;
#45287 = CARTESIAN_POINT ( 'NONE',  ( -0.8801773607111009756, 28.06368534415484106, 1.068504757029289695E-15 ) ) ;
#45288 = CARTESIAN_POINT ( 'NONE',  ( 7.313705784284532996, 0.3639312656126381662, 13.09617149020750837 ) ) ;
#45289 = ORIENTED_EDGE ( 'NONE', *, *, #61081, .F. ) ;
#45290 = CARTESIAN_POINT ( 'NONE',  ( -0.8801773607110991993, 22.85535201082150181, -2.915334737309923874 ) ) ;
#45291 = ADVANCED_FACE ( 'NONE', ( #64892 ), #17950, .F. ) ;
#45292 = TOROIDAL_SURFACE ( 'NONE', #13312, 14.49999999999999822, 0.5000000000000000000 ) ;
#45293 = EDGE_CURVE ( 'NONE', #49707, #89457, #49414, .T. ) ;
#45294 = ORIENTED_EDGE ( 'NONE', *, *, #86840, .F. ) ;
#45295 = CARTESIAN_POINT ( 'NONE',  ( -0.8801773607110991993, 32.85535201082151247, -2.915334737309923874 ) ) ;
#45296 = FACE_OUTER_BOUND ( 'NONE', #65201, .T. ) ;
#45297 = PRESENTATION_LAYER_ASSIGNMENT (  '', '', ( #26108 ) ) ;
#45298 = ORIENTED_EDGE ( 'NONE', *, *, #80851, .T. ) ;
#45299 = CARTESIAN_POINT ( 'NONE',  ( 3.591859063236761518, 19.95696800326375353, 11.09922568453594849 ) ) ;
#45300 = DIRECTION ( 'NONE',  ( 0.000000000000000000, 0.000000000000000000, 1.000000000000000000 ) ) ;
#45301 = CARTESIAN_POINT ( 'NONE',  ( 12.91533473730993009, 61.60535201082150536, -10.88017736071109987 ) ) ;
#45302 = DIRECTION ( 'NONE',  ( 0.000000000000000000, 1.000000000000000000, 0.000000000000000000 ) ) ;
#45303 = DIRECTION ( 'NONE',  ( 0.7132504491541897806, 0.000000000000000000, -0.7009092642998425715 ) ) ;
#45304 = CARTESIAN_POINT ( 'NONE',  ( 10.00000000000000000, 14.75893115100078568, -9.846743663894594434 ) ) ;
#45305 = CARTESIAN_POINT ( 'NONE',  ( -0.8801773607110991993, 37.85535201082151247, -2.915334737309923874 ) ) ;
#45306 = ORIENTED_EDGE ( 'NONE', *, *, #97575, .T. ) ;
#45307 = ORIENTED_EDGE ( 'NONE', *, *, #13086, .F. ) ;
#45308 = DIRECTION ( 'NONE',  ( 0.000000000000000000, 1.000000000000000000, 0.000000000000000000 ) ) ;
#45309 = CARTESIAN_POINT ( 'NONE',  ( 20.88017736071110164, 40.35535201082150536, 2.915334737309930979 ) ) ;
#45310 = CARTESIAN_POINT ( 'NONE',  ( -46.94000000000014694, 103.2291249090730787, -5.913062993056311889 ) ) ;
#45311 = CARTESIAN_POINT ( 'NONE',  ( 22.81628187352648496, 56.83196800326374643, -3.434112377981050290 ) ) ;
#45312 = CARTESIAN_POINT ( 'NONE',  ( 19.42250999205614548, 60.98035201082151247, -5.440088680355545492 ) ) ;
#45313 = CARTESIAN_POINT ( 'NONE',  ( 22.81628187352647785, 1.623634669930420271, 6.195893100308588602E-16 ) ) ;
#45314 = CARTESIAN_POINT ( 'NONE',  ( 1.472469842513823179, 21.42559781766745175, 4.923371831947296329 ) ) ;
#45315 = CARTESIAN_POINT ( 'NONE',  ( -2.816281873526471635, 48.91530133659708213, -3.434112377981056508 ) ) ;
#45316 = DIRECTION ( 'NONE',  ( 0.000000000000000000, 0.000000000000000000, 1.000000000000000000 ) ) ;
#45317 = CARTESIAN_POINT ( 'NONE',  ( 19.84674366389459266, 8.300597817667451750, 2.638427012816836559 ) ) ;
#45318 = CARTESIAN_POINT ( 'NONE',  ( 19.38216949554541202, 5.998634669930420493, 9.382169495545424454 ) ) ;
#45320 = DIRECTION ( 'NONE',  ( 0.000000000000000000, 0.000000000000000000, -1.000000000000000000 ) ) ;
#45319 =( NAMED_UNIT ( * ) PLANE_ANGLE_UNIT ( ) SI_UNIT ( $, .RADIAN. ) );
#45321 = CARTESIAN_POINT ( 'NONE',  ( 20.88017736071110164, 40.35535201082150536, 2.915334737309930979 ) ) ;
#45322 = CARTESIAN_POINT ( 'NONE',  ( 2.791683348922240793, 51.63393115100078745, 7.208316651077764092 ) ) ;
#45323 = DIRECTION ( 'NONE',  ( 0.000000000000000000, 0.000000000000000000, 1.000000000000000000 ) ) ;
#45324 = ADVANCED_FACE ( 'NONE', ( #20908 ), #81884, .T. ) ;
#45325 = CARTESIAN_POINT ( 'NONE',  ( 2.791683348922240793, 21.63393115100078745, 7.208316651077764092 ) ) ;
#45326 = CARTESIAN_POINT ( 'NONE',  ( 0.1532563361054100626, 5.800597817667452638, -2.638427012816831230 ) ) ;
#45328 = ORIENTED_EDGE ( 'NONE', *, *, #49422, .T. ) ;
#45327 = CARTESIAN_POINT ( 'NONE',  ( 22.81628187352647785, 6.415301336597088344, 3.434112377981063169 ) ) ;
#45329 = CARTESIAN_POINT ( 'NONE',  ( 10.00000000000000000, 1.813685344154837731, -10.88017736071110342 ) ) ;
#45330 = CYLINDRICAL_SURFACE ( 'NONE', #27869, 0.5000000000000004441 ) ;
#45331 = CARTESIAN_POINT ( 'NONE',  ( 4.669733657687698880, -13.81599790086176682, -2.499999999999999112 ) ) ;
#45332 = CARTESIAN_POINT ( 'NONE',  ( -4.164238869374099039, 66.80374883491396076, 8.674139862899312516E-16 ) ) ;
#45333 = CARTESIAN_POINT ( 'NONE',  ( 0.1532563361054082862, 46.21726448433411605, 2.638427012816831674 ) ) ;
#45334 = DIRECTION ( 'NONE',  ( -0.9890158633619157147, 0.000000000000000000, -0.1478094111296180124 ) ) ;
#45335 = CARTESIAN_POINT ( 'NONE',  ( 19.42250999205614548, 5.980352010821504471, -5.440088680355545492 ) ) ;
#45336 = CARTESIAN_POINT ( 'NONE',  ( 1.959929470562270959, 6.502578601053488505, 5.767676674365833200 ) ) ;
#45337 = CARTESIAN_POINT ( 'NONE',  ( 4.559911319644449179, 38.89701867748817676, 9.422509992056141925 ) ) ;
#45338 = CARTESIAN_POINT ( 'NONE',  ( 24.16423886937409904, 44.09541550158063927, 3.795296366450317205 ) ) ;
#45340 = CARTESIAN_POINT ( 'NONE',  ( -19.89999999999999858, 0.000000000000000000, 7.750000000000000000 ) ) ;
#45339 = CARTESIAN_POINT ( 'NONE',  ( 2.917880565312950480, 60.97041550158063927, -12.26659068614894821 ) ) ;
#45341 = CARTESIAN_POINT ( 'NONE',  ( 2.791683348922240793, 6.633931151000785675, 7.208316651077764092 ) ) ;
#45342 = CARTESIAN_POINT ( 'NONE',  ( 17.20831665107776587, 27.88393115100078390, 7.208316651077764980 ) ) ;
#45343 = CARTESIAN_POINT ( 'NONE',  ( 22.81628187352647785, 16.41530133659708923, 3.434112377981063169 ) ) ;
#45344 = CARTESIAN_POINT ( 'NONE',  ( -7.750000000000000000, 83.99999999999994316, -4.000000000000000000 ) ) ;
#45345 = CARTESIAN_POINT ( 'NONE',  ( 9.399392868737743711, 4.718572659598065102E-16, 11.04089732309480532 ) ) ;
#45346 = CARTESIAN_POINT ( 'NONE',  ( -8.468261785982759804, -9.345432893194818291, -4.000000000000000000 ) ) ;
#45347 = CARTESIAN_POINT ( 'NONE',  ( 13.79529636645030344, 8.262082168247300018, 14.16423886937410614 ) ) ;
#45348 = CARTESIAN_POINT ( 'NONE',  ( 0.1532563361054100626, 30.80059781766744820, -2.638427012816831230 ) ) ;
#45349 = CARTESIAN_POINT ( 'NONE',  ( -0.1503990784575328643, 70.00000000000000000, 6.262539305110068177 ) ) ;
#45350 = PRESENTATION_LAYER_ASSIGNMENT (  '', '', ( #32574 ) ) ;
#45351 = CARTESIAN_POINT ( 'NONE',  ( 24.16423886937410614, 39.51208216824731068, -3.795296366450302550 ) ) ;
#45352 = CARTESIAN_POINT ( 'NONE',  ( 12.63842701281683922, 9.550597817667449974, -9.846743663894590881 ) ) ;
#45354 = DIRECTION ( 'NONE',  ( 0.000000000000000000, 0.000000000000000000, 1.000000000000000000 ) ) ;
#45353 = CARTESIAN_POINT ( 'NONE',  ( 3.166711953933172286, 0.000000000000000000, 4.439566422914491994 ) ) ;
#45355 = CARTESIAN_POINT ( 'NONE',  ( 4.559911319644449179, 28.89701867748817321, 9.422509992056141925 ) ) ;
#45356 = CARTESIAN_POINT ( 'NONE',  ( 16.40814093676323893, 50.79030133659708923, 11.09922568453595026 ) ) ;
#45357 = CARTESIAN_POINT ( 'NONE',  ( -0.8801773607110991993, 2.855352010821504471, -2.915334737309923874 ) ) ;
#45358 = CARTESIAN_POINT ( 'NONE',  ( -2.816281873526473856, 34.33196800326376064, 3.434112377981055619 ) ) ;
#45359 = CARTESIAN_POINT ( 'NONE',  ( 14.92337183194729988, 4.342264484334117824, -8.527530157486177487 ) ) ;
#45360 = ORIENTED_EDGE ( 'NONE', *, *, #7540, .F. ) ;
#45361 = AXIS2_PLACEMENT_3D ( 'NONE', #73619, #12138, #95647 ) ;
#45362 = FACE_OUTER_BOUND ( 'NONE', #68440, .T. ) ;
#45363 = CARTESIAN_POINT ( 'NONE',  ( -14.75001642003105040, 0.04962894700187112096, -0.3071237627331344089 ) ) ;
#45364 = CARTESIAN_POINT ( 'NONE',  ( -4.164238869374099039, 36.80374883491396787, 8.674139862899312516E-16 ) ) ;
#45365 = CARTESIAN_POINT ( 'NONE',  ( 13.79529636645030344, 18.26208216824730002, 14.16423886937410614 ) ) ;
#45366 = CARTESIAN_POINT ( 'NONE',  ( 10.00000000000000000, 1.813685344154837731, -10.88017736071110342 ) ) ;
#45367 = CARTESIAN_POINT ( 'NONE',  ( -0.8801773607111008646, 38.27201867748816255, 2.915334737309923430 ) ) ;
#45368 = DIRECTION ( 'NONE',  ( 1.000000000000000000, 1.257402221000611116E-16, -0.000000000000000000 ) ) ;
#45369 = DIRECTION ( 'NONE',  ( -0.000000000000000000, -1.000000000000000000, -0.000000000000000000 ) ) ;
#45370 = CARTESIAN_POINT ( 'NONE',  ( 2.035157376598822676, 52.43868534415483396, -7.964842623401177768 ) ) ;
#45371 = CARTESIAN_POINT ( 'NONE',  ( 7.084665262690076126, 67.02201867748817676, -10.88017736071110164 ) ) ;
#45372 = CARTESIAN_POINT ( 'NONE',  ( 19.38216949554541557, 27.24863466993041783, -9.382169495545420901 ) ) ;
#45373 = FACE_OUTER_BOUND ( 'NONE', #73684, .T. ) ;
#45374 = CARTESIAN_POINT ( 'NONE',  ( -3.384800920123979484, 14.76930270348881180, -14.55270344038012453 ) ) ;
#45375 = CARTESIAN_POINT ( 'NONE',  ( 0.1532563361054082862, 31.21726448433412315, 2.638427012816831674 ) ) ;
#45376 = EDGE_CURVE ( 'NONE', #26206, #86034, #82881, .T. ) ;
#45377 = CARTESIAN_POINT ( 'NONE',  ( 21.09922568453594849, 21.20696800326375353, 6.408140936763242479 ) ) ;
#45378 = CARTESIAN_POINT ( 'NONE',  ( -0.8801773607111009756, 43.06368534415484106, 1.068504757029289695E-15 ) ) ;
#45379 = CARTESIAN_POINT ( 'NONE',  ( 4.559911319644449179, 12.23035201082150536, -9.422509992056141925 ) ) ;
#45380 = CARTESIAN_POINT ( 'NONE',  ( 2.791683348922240793, 41.63393115100078745, 7.208316651077764092 ) ) ;
#45381 = DIRECTION ( 'NONE',  ( -1.000000000000000000, 0.000000000000000000, 0.000000000000000000 ) ) ;
#45382 = CARTESIAN_POINT ( 'NONE',  ( 12.63842701281683034, 12.46726448433411782, 9.846743663894596210 ) ) ;
#45383 = CARTESIAN_POINT ( 'NONE',  ( 2.917880565312950480, 5.970415501580634832, -12.26659068614894821 ) ) ;
#45384 = FACE_OUTER_BOUND ( 'NONE', #18502, .T. ) ;
#45385 = CARTESIAN_POINT ( 'NONE',  ( 4.559911319644449179, 37.23035201082150536, -9.422509992056141925 ) ) ;
#45386 = CARTESIAN_POINT ( 'NONE',  ( 12.91533473730992121, 4.522018677488169658, 10.88017736071110164 ) ) ;
#45387 = CARTESIAN_POINT ( 'NONE',  ( 10.00000000000000000, 26.81368534415484106, -10.88017736071110342 ) ) ;
#45388 = CARTESIAN_POINT ( 'NONE',  ( 4.559911319644449179, 12.23035201082150714, -9.422509992056141925 ) ) ;
#45389 = ORIENTED_EDGE ( 'NONE', *, *, #79926, .F. ) ;
#45390 = EDGE_CURVE ( 'NONE', #54861, #54024, #90362, .T. ) ;
#45391 = CARTESIAN_POINT ( 'NONE',  ( 20.88017736071110519, 20.56368534415484106, 2.639326808657452039E-16 ) ) ;
#45392 = CARTESIAN_POINT ( 'NONE',  ( 22.81628187352647785, 41.41530133659708923, 3.434112377981063169 ) ) ;
#45393 = CARTESIAN_POINT ( 'NONE',  ( 4.559911319644449179, 43.89701867748816966, 9.422509992056141925 ) ) ;
#45394 = CARTESIAN_POINT ( 'NONE',  ( 20.88017736071110519, 55.56368534415484817, 2.639326808657452039E-16 ) ) ;
#45395 = ORIENTED_EDGE ( 'NONE', *, *, #35903, .F. ) ;
#45396 = CARTESIAN_POINT ( 'NONE',  ( 17.96484262340118221, 34.93868534415482685, 7.964842623401181321 ) ) ;
#45397 = CARTESIAN_POINT ( 'NONE',  ( 7.184035427668765017, -73.16388022040806050, 4.000000000000000000 ) ) ;
#45398 = EDGE_CURVE ( 'NONE', #16419, #76530, #51397, .T. ) ;
#45399 = CARTESIAN_POINT ( 'NONE',  ( 0.1077916266722768468, 37.24062864464240619, -6.478736007406001640 ) ) ;
#45400 = CARTESIAN_POINT ( 'NONE',  ( -2.266590686148945544, 41.38708216824729647, -7.082119434687050408 ) ) ;
#45401 = CARTESIAN_POINT ( 'NONE',  ( 17.20831665107776587, 2.883931151000785231, 7.208316651077764980 ) ) ;
#45402 = CARTESIAN_POINT ( 'NONE',  ( 5.279540384298776701, 0.000000000000000000, 1.365381980696741548 ) ) ;
#45403 = CARTESIAN_POINT ( 'NONE',  ( 0.000000000000000000, 15.00000000000000000, 0.000000000000000000 ) ) ;
#45404 = CARTESIAN_POINT ( 'NONE',  ( 17.20831665107776587, 59.13393115100078745, -7.208316651077762316 ) ) ;
#45405 = CARTESIAN_POINT ( 'NONE',  ( -14.16722289976678617, 0.5000000000000004441, -4.928467845925704083 ) ) ;
#45406 = CARTESIAN_POINT ( 'NONE',  ( 19.84674366389459266, 38.71726448433412315, -2.638427012816827677 ) ) ;
#45407 = EDGE_CURVE ( 'NONE', #65307, #88822, #11245, .T. ) ;
#45408 = ORIENTED_EDGE ( 'NONE', *, *, #98249, .F. ) ;
#45409 = CARTESIAN_POINT ( 'NONE',  ( 5.076628168052703671, 36.84226448433412315, 8.527530157486179263 ) ) ;
#45410 = CARTESIAN_POINT ( 'NONE',  ( -6.408140936763246032, -16.70969866340291077, -11.09922568453594316 ) ) ;
#45411 = CARTESIAN_POINT ( 'NONE',  ( -0.8801773607111009756, 23.06368534415484106, 1.068504757029289695E-15 ) ) ;
#45412 = CARTESIAN_POINT ( 'NONE',  ( 10.00000000000000000, 44.75893115100078745, -9.846743663894594434 ) ) ;
#45413 = CARTESIAN_POINT ( 'NONE',  ( 16.40814093676323893, 15.79030133659708746, 11.09922568453595026 ) ) ;
#45415 = CARTESIAN_POINT ( 'NONE',  ( 15.44008868035555793, 56.39701867748817676, -9.422509992056140149 ) ) ;
#45414 = FACE_OUTER_BOUND ( 'NONE', #89320, .T. ) ;
#45417 = FILL_AREA_STYLE_COLOUR ( '', #49767 ) ;
#45416 = CARTESIAN_POINT ( 'NONE',  ( 10.00000000000000178, 39.31368534415484106, 10.88017736071110342 ) ) ;
#45418 = CARTESIAN_POINT ( 'NONE',  ( -0.3689425029237881626, 62.42874883491396787, 10.36894250292379027 ) ) ;
#45419 = CARTESIAN_POINT ( 'NONE',  ( -2.253458813454140675, 12.77999999999999936, 9.500000000000000000 ) ) ;
#45420 = EDGE_LOOP ( 'NONE', ( #7591, #62429, #87347, #72010 ) ) ;
#45421 = AXIS2_PLACEMENT_3D ( 'NONE', #25931, #31446, #92934 ) ;
#45422 = CARTESIAN_POINT ( 'NONE',  ( 6.565887622018943937, 13.08196800326374998, -12.81628187352647608 ) ) ;
#45423 = CARTESIAN_POINT ( 'NONE',  ( -0.8801773607111008646, 13.27201867748817143, 2.915334737309923430 ) ) ;
#45424 = CARTESIAN_POINT ( 'NONE',  ( 12.91533473730992121, 44.52201867748816966, 10.88017736071110164 ) ) ;
#45425 = CARTESIAN_POINT ( 'NONE',  ( -14.29730467489530632, 4.415605380435452030E-16, -2.416004766803409254 ) ) ;
#45426 = AXIS2_PLACEMENT_3D ( 'NONE', #42530, #81503, #13008 ) ;
#45427 = ORIENTED_EDGE ( 'NONE', *, *, #93804, .F. ) ;
#45428 = CARTESIAN_POINT ( 'NONE',  ( -12.21238578216017245, -2.320870275476780957E-16, 8.049595036947042814 ) ) ;
#45429 = EDGE_CURVE ( 'NONE', #13614, #1450, #43148, .T. ) ;
#45430 = CARTESIAN_POINT ( 'NONE',  ( 20.88017736071110519, 60.56368534415484106, 2.639326808657452039E-16 ) ) ;
#45431 = STYLED_ITEM ( 'NONE', ( #10300 ), #42960 ) ;
#45432 = CARTESIAN_POINT ( 'NONE',  ( 5.076628168052703671, 41.84226448433411605, 8.527530157486179263 ) ) ;
#45433 = CARTESIAN_POINT ( 'NONE',  ( 18.52753015748617571, 18.09226448433411960, 4.923371831947298993 ) ) ;
#45434 = CARTESIAN_POINT ( 'NONE',  ( 19.84674366389459266, 8.717264484334116048, -2.638427012816827677 ) ) ;
#45435 = CARTESIAN_POINT ( 'NONE',  ( 0.1957200283969098564, 40.25733960839544778, 6.499999999999992006 ) ) ;
#45436 = PLANE ( 'NONE',  #2180 ) ;
#45437 = EDGE_CURVE ( 'NONE', #59690, #84144, #60367, .T. ) ;
#45439 = CARTESIAN_POINT ( 'NONE',  ( -8.209432707284749497, 14.49999999999999112, -12.55409154915501269 ) ) ;
#45438 = CARTESIAN_POINT ( 'NONE',  ( 0.1532563361054100626, 10.80059781766745175, -2.638427012816831230 ) ) ;
#45440 = CARTESIAN_POINT ( 'NONE',  ( 7.079515573063599021, -88.00917032380691296, -4.000000000000000000 ) ) ;
#45442 = ORIENTED_EDGE ( 'NONE', *, *, #3312, .T. ) ;
#45441 = CARTESIAN_POINT ( 'NONE',  ( 1.472469842513823179, 31.42559781766745530, 4.923371831947296329 ) ) ;
#45443 = CARTESIAN_POINT ( 'NONE',  ( 9.742785792574933268, 3.034700295649320534, -5.625000000000003553 ) ) ;
#45444 = CARTESIAN_POINT ( 'NONE',  ( 19.38216949554541557, 17.24863466993041783, -9.382169495545420901 ) ) ;
#45445 = TOROIDAL_SURFACE ( 'NONE', #3997, 14.49999999999999822, 0.5000000000000000000 ) ;
#45446 = CARTESIAN_POINT ( 'NONE',  ( 0.5774900079438590739, 57.64701867748817676, -5.440088680355550821 ) ) ;
#45447 = CARTESIAN_POINT ( 'NONE',  ( -2.266590686148945544, 32.22041550158063927, 7.082119434687048631 ) ) ;
#45448 = UNCERTAINTY_MEASURE_WITH_UNIT (LENGTH_MEASURE( 1.000000000000000082E-05 ), #4806, 'distance_accuracy_value', 'NONE');
#45449 = CARTESIAN_POINT ( 'NONE',  ( -11.88860330016272471, 90.28199325633934791, 6.828299344291659523 ) ) ;
#45450 = CARTESIAN_POINT ( 'NONE',  ( 10.00000000000000000, 35.55374883491396787, -14.16423886937410082 ) ) ;
#45451 = EDGE_CURVE ( 'NONE', #91405, #22543, #98409, .T. ) ;
#45452 = CARTESIAN_POINT ( 'NONE',  ( -0.3689425029237881626, 57.42874883491397497, 10.36894250292379027 ) ) ;
#45453 = CARTESIAN_POINT ( 'NONE',  ( 24.16423886937409904, 9.095415501580633943, 3.795296366450317205 ) ) ;
#45455 = CARTESIAN_POINT ( 'NONE',  ( -2.815433093576914736, 14.49999999999999112, -14.73340885523760413 ) ) ;
#45454 = CARTESIAN_POINT ( 'NONE',  ( -0.3689425029237881626, 32.42874883491395366, 10.36894250292379027 ) ) ;
#45456 = CARTESIAN_POINT ( 'NONE',  ( 0.5774900079438590739, 52.64701867748817676, -5.440088680355550821 ) ) ;
#45457 = CARTESIAN_POINT ( 'NONE',  ( 4.380000000000000782, -0.01592157648205478476, -2.750000000000000000 ) ) ;
#45458 =( BOUNDED_CURVE ( )  B_SPLINE_CURVE ( 2, ( #72443, #70998, #19944, #79474, #87458, #3486, #94465, #57936, #64447 ),
 .UNSPECIFIED., .F., .F. ) 
 B_SPLINE_CURVE_WITH_KNOTS ( ( 3, 2, 2, 2, 3 ),
 ( 0.8687123655116599785, 0.8690476190476190688, 0.8750000000000000000, 0.8809523809523809312, 0.8812876344883400215 ),
 .UNSPECIFIED. ) 
 CURVE ( )  GEOMETRIC_REPRESENTATION_ITEM ( )  RATIONAL_B_SPLINE_CURVE ( ( 0.9963778908391764944, 0.9980808541467923733, 1.000000000000000000, 0.9659258262890683122, 1.000000000000000000, 0.9659258262890683122, 1.000000000000000000, 0.9980808541467922623, 0.9963778908391764944 ) ) 
 REPRESENTATION_ITEM ( '' )  );
#45460 = CARTESIAN_POINT ( 'NONE',  ( 18.52753015748618282, 38.92559781766745175, -4.923371831947291888 ) ) ;
#45459 = CARTESIAN_POINT ( 'NONE',  ( 7.084665262690076126, 69.10535201082151957, 10.88017736071109987 ) ) ;
#45461 = CARTESIAN_POINT ( 'NONE',  ( 19.42250999205614193, 30.14701867748817321, 5.440088680355555262 ) ) ;
#45462 = CARTESIAN_POINT ( 'NONE',  ( -2.816281873526473856, 59.12363466993042493, 9.499525473075851096E-16 ) ) ;
#45463 = CARTESIAN_POINT ( 'NONE',  ( 2.791683348922240793, 61.63393115100079456, 7.208316651077764092 ) ) ;
#45464 = CARTESIAN_POINT ( 'NONE',  ( 11.48952521350825151, 15.00000000000000000, -8.845383562535966249 ) ) ;
#45465 = CARTESIAN_POINT ( 'NONE',  ( 5.076628168052704559, 30.17559781766745175, -8.527530157486179263 ) ) ;
#45466 = CARTESIAN_POINT ( 'NONE',  ( 13.43411237798106583, 52.66530133659708213, -12.81628187352647252 ) ) ;
#45467 = CARTESIAN_POINT ( 'NONE',  ( -12.26659068614895354, -18.61291783175269288, -7.082119434687038861 ) ) ;
#45468 = CARTESIAN_POINT ( 'NONE',  ( 15.44008868035555793, 46.39701867748817676, -9.422509992056140149 ) ) ;
#45469 = CARTESIAN_POINT ( 'NONE',  ( 19.84674366389459266, 48.30059781766745175, 2.638427012816836559 ) ) ;
#45470 = CARTESIAN_POINT ( 'NONE',  ( 24.16423886937410614, 34.30374883491396787, 8.672049930838204340E-16 ) ) ;
#45471 = ORIENTED_EDGE ( 'NONE', *, *, #49470, .T. ) ;
#45472 = LINE ( 'NONE', #81994, #36371 ) ;
#45473 = CARTESIAN_POINT ( 'NONE',  ( 4.559911319644449179, 62.23035201082150536, -9.422509992056141925 ) ) ;
#45474 = CARTESIAN_POINT ( 'NONE',  ( 7.084665262690076126, 67.02201867748817676, -10.88017736071110164 ) ) ;
#45475 = CARTESIAN_POINT ( 'NONE',  ( 20.36894250292379382, 58.67874883491396076, 10.36894250292379205 ) ) ;
#45476 = CARTESIAN_POINT ( 'NONE',  ( 6.565887622018943937, 13.08196800326374998, -12.81628187352647608 ) ) ;
#45477 = CARTESIAN_POINT ( 'NONE',  ( 5.991992585808519678, 15.00000000000000000, 13.20401548210297271 ) ) ;
#45478 = CARTESIAN_POINT ( 'NONE',  ( 20.88017736071110164, 55.35535201082149825, 2.915334737309930979 ) ) ;
#45479 = CARTESIAN_POINT ( 'NONE',  ( 7.551349515323185990, -0.03417435944610275333, -12.08468537022906020 ) ) ;
#45480 = CYLINDRICAL_SURFACE ( 'NONE', #22862, 0.2500000000000002220 ) ;
#45481 = CARTESIAN_POINT ( 'NONE',  ( 6.204703633549690345, 52.84541550158062506, 14.16423886937410082 ) ) ;
#45482 = CARTESIAN_POINT ( 'NONE',  ( 3.469446951953614189E-15, 24.31368534415484461, 10.88017736071110342 ) ) ;
#45483 = CARTESIAN_POINT ( 'NONE',  ( 17.96484262340118221, 14.93868534415483751, 7.964842623401181321 ) ) ;
#45484 = CARTESIAN_POINT ( 'NONE',  ( 17.96484262340118221, 29.93868534415484106, 7.964842623401181321 ) ) ;
#45485 = CARTESIAN_POINT ( 'NONE',  ( 1.472469842513823179, 61.42559781766745175, 4.923371831947296329 ) ) ;
#45486 = CARTESIAN_POINT ( 'NONE',  ( 16.40814093676323893, 50.79030133659708923, 11.09922568453595026 ) ) ;
#45487 = DIRECTION ( 'NONE',  ( -0.000000000000000000, -1.000000000000000000, -0.000000000000000000 ) ) ;
#45488 = ORIENTED_EDGE ( 'NONE', *, *, #9620, .F. ) ;
#45489 = CARTESIAN_POINT ( 'NONE',  ( 7.084665262690076126, 19.10535201082150181, 10.88017736071109987 ) ) ;
#45490 = EDGE_CURVE ( 'NONE', #94289, #53120, #29865, .T. ) ;
#45491 = CARTESIAN_POINT ( 'NONE',  ( 3.591859063236763294, 23.29030133659708568, -11.09922568453595026 ) ) ;
#45492 = DIRECTION ( 'NONE',  ( 1.000000000000000000, 0.000000000000000000, 0.000000000000000000 ) ) ;
#45493 =( GEOMETRIC_REPRESENTATION_CONTEXT ( 3 ) GLOBAL_UNCERTAINTY_ASSIGNED_CONTEXT ( ( #13481 ) ) GLOBAL_UNIT_ASSIGNED_CONTEXT ( ( #48766, #77789, #71773 ) ) REPRESENTATION_CONTEXT ( 'NONE', 'WORKASPACE' ) );
#45494 = CARTESIAN_POINT ( 'NONE',  ( 5.076628168052703671, 46.84226448433412315, 8.527530157486179263 ) ) ;
#45495 = EDGE_CURVE ( 'NONE', #23012, #97173, #6886, .T. ) ;
#45496 = CARTESIAN_POINT ( 'NONE',  ( 4.559911319644449179, 37.23035201082150536, -9.422509992056141925 ) ) ;
#45497 =( GEOMETRIC_REPRESENTATION_CONTEXT ( 3 ) GLOBAL_UNCERTAINTY_ASSIGNED_CONTEXT ( ( #11504 ) ) GLOBAL_UNIT_ASSIGNED_CONTEXT ( ( #29322, #5370, #73347 ) ) REPRESENTATION_CONTEXT ( 'NONE', 'WORKASPACE' ) );
#45498 = CARTESIAN_POINT ( 'NONE',  ( 6.565887622018943937, 28.08196800326375353, -12.81628187352647608 ) ) ;
#45500 = DIRECTION ( 'NONE',  ( 0.000000000000000000, -1.000000000000000000, 0.000000000000000000 ) ) ;
#45499 = CARTESIAN_POINT ( 'NONE',  ( 2.035157376598824452, 48.68868534415483396, 7.964842623401179544 ) ) ;
#45501 = CARTESIAN_POINT ( 'NONE',  ( 19.72487221294570858, 70.00000000000000000, -6.000000000000000000 ) ) ;
#45502 = CARTESIAN_POINT ( 'NONE',  ( -1.099225684535947600, 48.70696800326375353, -6.408140936763238038 ) ) ;
#45503 = ORIENTED_EDGE ( 'NONE', *, *, #63879, .F. ) ;
#45504 = B_SPLINE_CURVE_WITH_KNOTS ( 'NONE', 3,
 ( #89922, #35933, #96964, #58934 ),
 .UNSPECIFIED., .F., .F.,
 ( 4, 4 ),
 ( 0.000000000000000000, 0.002392975128318479416 ),
 .UNSPECIFIED. ) ;
#45505 = CARTESIAN_POINT ( 'NONE',  ( 19.42250999205614193, 55.14701867748817676, 5.440088680355555262 ) ) ;
#45507 = CARTESIAN_POINT ( 'NONE',  ( -0.3689425029237881626, 2.428748834913967869, 10.36894250292379027 ) ) ;
#45506 = CARTESIAN_POINT ( 'NONE',  ( -2.816281873526471635, 33.91530133659708213, -3.434112377981056508 ) ) ;
#45508 = CARTESIAN_POINT ( 'NONE',  ( 0.1532563361054082862, 6.217264484334118713, 2.638427012816831674 ) ) ;
#45509 = CARTESIAN_POINT ( 'NONE',  ( 20.36894250292379738, 49.92874883491396787, -10.36894250292379027 ) ) ;
#45510 = DIRECTION ( 'NONE',  ( 1.000000000000000000, 0.000000000000000000, 0.000000000000000000 ) ) ;
#45511 = CARTESIAN_POINT ( 'NONE',  ( 19.84674366389459621, 13.50893115100078568, 7.409399052514197653E-17 ) ) ;
#45512 = CARTESIAN_POINT ( 'NONE',  ( 0.1532563361054100626, 0.8005978176674514168, -2.638427012816831230 ) ) ;
#45513 = CARTESIAN_POINT ( 'NONE',  ( 2.588169541918969419, 0.4578369456018643868, -6.498696640609835207 ) ) ;
#45514 = CARTESIAN_POINT ( 'NONE',  ( 2.917880565312948704, 47.63708216824730357, 12.26659068614894643 ) ) ;
#45515 = EDGE_CURVE ( 'NONE', #13300, #20878, #59128, .T. ) ;
#45516 = CARTESIAN_POINT ( 'NONE',  ( 18.72515096720570327, 16.07228050351031712, -6.499999999999992006 ) ) ;
#45517 = CARTESIAN_POINT ( 'NONE',  ( 7.084665262690076126, 2.022018677488170990, -10.88017736071110164 ) ) ;
#45518 = CARTESIAN_POINT ( 'NONE',  ( -7.116171662378945051, -80.69120418497870162, -3.749999999999193534 ) ) ;
#45519 = VERTEX_POINT ( 'NONE', #75371 ) ;
#45520 = CARTESIAN_POINT ( 'NONE',  ( -0.8801773607111009756, 3.063685344154838397, 1.068504757029289695E-15 ) ) ;
#45521 = CARTESIAN_POINT ( 'NONE',  ( -2.266590686148945544, 66.38708216824730357, -7.082119434687050408 ) ) ;
#45522 = CARTESIAN_POINT ( 'NONE',  ( 14.92337183194729988, 49.34226448433411605, -8.527530157486177487 ) ) ;
#45523 = TOROIDAL_SURFACE ( 'NONE', #90259, 2.250000000000001332, 0.2500000000000000000 ) ;
#45524 = ADVANCED_FACE ( 'NONE', ( #36397 ), #68384, .F. ) ;
#45525 = CARTESIAN_POINT ( 'NONE',  ( -2.816281873526471635, 43.91530133659708923, -3.434112377981056508 ) ) ;
#45526 = DIRECTION ( 'NONE',  ( -3.463895836830488406E-14, 0.000000000000000000, 1.000000000000000000 ) ) ;
#45528 = CARTESIAN_POINT ( 'NONE',  ( -0.3689425029237898834, 11.17874883491396787, -10.36894250292378850 ) ) ;
#45527 = CARTESIAN_POINT ( 'NONE',  ( 0.000000000000000000, 0.000000000000000000, 0.000000000000000000 ) ) ;
#45529 = CARTESIAN_POINT ( 'NONE',  ( 19.42250999205614548, 15.98035201082150714, -5.440088680355545492 ) ) ;
#45530 = CARTESIAN_POINT ( 'NONE',  ( 20.88017736071110164, 10.35535201082150714, 2.915334737309930979 ) ) ;
#45531 = CARTESIAN_POINT ( 'NONE',  ( 7.361572987183169658, 44.96726448433412315, -9.846743663894592657 ) ) ;
#45532 = CARTESIAN_POINT ( 'NONE',  ( -6.869455772996959197, 15.00000000000000000, -14.44603661281848517 ) ) ;
#45533 = CARTESIAN_POINT ( 'NONE',  ( 12.63842701281683034, 27.46726448433411250, 9.846743663894596210 ) ) ;
#45534 = EDGE_CURVE ( 'NONE', #47321, #86750, #78346, .T. ) ;
#45535 = CARTESIAN_POINT ( 'NONE',  ( 0.5774900079438590739, 32.64701867748816966, -5.440088680355550821 ) ) ;
#45536 = CARTESIAN_POINT ( 'NONE',  ( -9.846743663894590881, 16.21726448433411960, 2.638427012816840111 ) ) ;
#45537 = ORIENTED_EDGE ( 'NONE', *, *, #13242, .T. ) ;
#45538 = ORIENTED_EDGE ( 'NONE', *, *, #97672, .F. ) ;
#45539 = ORIENTED_EDGE ( 'NONE', *, *, #81939, .F. ) ;
#45540 = CARTESIAN_POINT ( 'NONE',  ( 2.791683348922237240, 55.38393115100078745, -7.208316651077763204 ) ) ;
#45541 = CARTESIAN_POINT ( 'NONE',  ( 24.16423886937410614, 19.51208216824729647, -3.795296366450302550 ) ) ;
#45543 = CARTESIAN_POINT ( 'NONE',  ( -0.8801773607111008646, 33.27201867748817676, 2.915334737309923430 ) ) ;
#45542 = CARTESIAN_POINT ( 'NONE',  ( 12.91533473730993009, 31.60535201082150891, -10.88017736071109987 ) ) ;
#45545 = CARTESIAN_POINT ( 'NONE',  ( 13.43411237798106583, 32.66530133659708213, -12.81628187352647252 ) ) ;
#45544 = CARTESIAN_POINT ( 'NONE',  ( 1.472469842513823179, 61.42559781766745175, 4.923371831947296329 ) ) ;
#45546 = CARTESIAN_POINT ( 'NONE',  ( 2.917880565312950480, 5.970415501580634832, -12.26659068614894821 ) ) ;
#45547 = CIRCLE ( 'NONE', #40763, 1.000000000000007772 ) ;
#45548 = CARTESIAN_POINT ( 'NONE',  ( -0.8801773607111008646, 63.27201867748817676, 2.915334737309923430 ) ) ;
#45549 = CIRCLE ( 'NONE', #18428, 0.09999999999999982514 ) ;
#45550 = CARTESIAN_POINT ( 'NONE',  ( -2.816281873526473856, 49.12363466993042493, 9.499525473075851096E-16 ) ) ;
#45551 = ORIENTED_EDGE ( 'NONE', *, *, #78331, .F. ) ;
#45552 = CARTESIAN_POINT ( 'NONE',  ( 18.52753015748618282, 43.92559781766745175, -4.923371831947291888 ) ) ;
#45553 = CARTESIAN_POINT ( 'NONE',  ( 2.035157376598824452, 8.688685344154839285, 7.964842623401179544 ) ) ;
#45554 = VERTEX_POINT ( 'NONE', #73892 ) ;
#45555 = CARTESIAN_POINT ( 'NONE',  ( -8.000000000000000000, 40.99999999999999289, -6.500000000000000888 ) ) ;
#45556 = CARTESIAN_POINT ( 'NONE',  ( 12.91533473730992121, 19.52201867748816611, 10.88017736071110164 ) ) ;
#45557 = ORIENTED_EDGE ( 'NONE', *, *, #40621, .T. ) ;
#45558 = CARTESIAN_POINT ( 'NONE',  ( 0.5774900079438607392, 63.48035201082149825, 5.440088680355550821 ) ) ;
#45559 = CARTESIAN_POINT ( 'NONE',  ( 19.42250999205614193, 55.14701867748817676, 5.440088680355555262 ) ) ;
#45560 = CARTESIAN_POINT ( 'NONE',  ( 7.084665262690076126, 62.02201867748816966, -10.88017736071110164 ) ) ;
#45561 = CARTESIAN_POINT ( 'NONE',  ( 10.00000000000000000, -0.2410688489992152128, -9.846743663894594434 ) ) ;
#45562 = CARTESIAN_POINT ( 'NONE',  ( 12.91533473730992121, 54.52201867748816255, 10.88017736071110164 ) ) ;
#45563 = FACE_OUTER_BOUND ( 'NONE', #28353, .T. ) ;
#45564 = EDGE_CURVE ( 'NONE', #65197, #91549, #71919, .T. ) ;
#45565 = CARTESIAN_POINT ( 'NONE',  ( -46.93999999999942219, 101.0602049476338777, 8.583117191026476078 ) ) ;
#45566 = CARTESIAN_POINT ( 'NONE',  ( 11.04397247052727238, -89.88416767676933716, 4.000000000000000888 ) ) ;
#45567 = CARTESIAN_POINT ( 'NONE',  ( 18.52753015748618282, 38.92559781766745175, -4.923371831947291888 ) ) ;
#45568 = ORIENTED_EDGE ( 'NONE', *, *, #68407, .F. ) ;
#45569 = CARTESIAN_POINT ( 'NONE',  ( 2.791683348922237240, 65.38393115100078035, -7.208316651077763204 ) ) ;
#45570 = AXIS2_PLACEMENT_3D ( 'NONE', #42260, #43228, #58212 ) ;
#45571 = FACE_OUTER_BOUND ( 'NONE', #1942, .T. ) ;
#45572 =( BOUNDED_SURFACE ( )  B_SPLINE_SURFACE ( 1, 2, ( 
 ( #56597, #80075, #41118, #79594, #19086, #49563, #81061, #73548, #5074, #35560, #25618, #87088, #18114, #79092, #33577, #18598, #49091, #41611, #57079, #72080, #3606, #72561, #76027, #37554, #22552, #29035, #30023, #97083, #20569, #68044, #90525, #36560, #38047, #82542, #37054, #14558, #59047, #6061, #59544, #51556, #98570, #53022, #66554, #13054, #90039, #89056, #28054, #52051, #67049, #29523, #14059, #28554, #22060, #7558, #44542, #52534, #96578, #67553, #60529, #58549, #89551, #21061, #82042, #74042, #91019, #98064, #5577, #75038, #45529, #45027, #51054, #75534, #6544, #97572, #81544, #43548, #36052, #83537, #13554, #60030, #44040, #74541, #15056, #83042, #21562, #7050, #77493, #24527, #55503, #25015, #17514, #68539, #69521, #84030, #54986, #1036, #31497, #77011, #2029, #92014, #8523, #15550, #39521, #47980, #62986, #30516, #70013, #39026, #61019, #24029, #86003, #78490, #69030, #31011, #1539, #62000, #32491, #16525, #565, #31983, #62489, #85505, #10004, #61507, #23544, #92993, #92499, #93492, #47000, #54016, #17015, #47493, #77996, #70, #54497, #8036, #9501, #85012, #91531, #84525, #9005, #53518, #16022, #40003, #70505, #23046, #46035, #76520, #38534, #46511, #40997, #88446, #19946, #11957, #63482, #78976, #19462, #48966, #93986, #25508, #71494, #50441, #80459, #65438, #71965, #72944, #3009, #55995, #42462, #34444, #79476, #80946, #26458, #79959, #57454, #33458, #10975, #3488, #94467, #4474, #95962, #10486, #86495, #33945, #32978, #71002, #94956, #41496, #72445, #56957, #63955, #64935, #40506, #87460, #95463, #2525, #11463, #34940, #17995, #25984, #56481, #86967, #48477, #27444, #41981, #18481, #18975, #64449, #87947, #49453, #49954, #3975, #26954, #57938, #42952, #35438, #37434, #50939, #44417, #96962, #81433, #14435, #6419, #58426, #96461, #21435, #67424, #98445, #67924, #60406, #12444, #13431, #27933, #97949, #43917, #74415, #20946, #44906, #35932, #51433, #88940, #82416, #90902, #6927, #73431, #13940, #81923, #4958, #66928, #29901, #5944, #52902, #65933, #12937, #36435, #20449, #5460, #66429, #29406, #89921, #75408, #28434, #43431, #22430, #90399, #97448, #51932, #73932, #58932, #89432, #28913, #59415, #74921, #36932, #59909, #52418, #21938, #82917, #77371, #46879, #1907, #22925, #37928, #68912, #39882, #68417, #69394, #76885, #8882, #46397, #60898, #31379, #32362, #39400, #15907, #8398, #38907, #54377, #16891, #916, #1413, #98940, #61877, #47370, #75907, #84890, #92382, #440, #23908, #31866, #45912, #53394, #69893, #24400, #16397, #7432, #62365, #30893, #91397, #62869, #92870, #15434, #54868, #84408, #83904 ),
 ( #85379, #76401, #91896, #77868, #38412, #9379, #70388, #7916, #30394, #93365, #61387, #14934, #24893, #23421, #83413, #45401, #53900, #49337, #34823, #41382, #79837, #95839, #94840, #57328, #17390, #25388, #86370, #78860, #32857, #87822, #56843, #63356, #71849, #4357, #3858, #65313, #34318, #3359, #56365, #85878, #47859, #78365, #80335, #93860, #18364, #63835, #19342, #10372, #94349, #2400, #26342, #55377, #49825, #9884, #87342, #25868, #40384, #10861, #72817, #42342, #55871, #17871, #18857, #86858, #11834, #33822, #48354, #11342, #41862, #72325, #70883, #64328, #40873, #64816, #95335, #71378, #2890, #26834, #33341, #48843, #79354, #22185, #98699, #53161, #30148, #60657, #7683, #29170, #76645, #8166, #193, #51691, #67181, #38176, #37197, #82170, #13683, #59671, #38657, #68666, #53653, #60163, #61149, #90163, #44169, #30640, #22680, #67688, #69162, #14693, #68180, #45664, #21693, #98197, #90659, #82673, #91658, #84172, #97704, #74677, #52666, #19826, #57820, #83168, #29654, #91156, #45163, #52179, #83666, #27322, #75667, #15184, #88328, #76161, #23176, #6189, #14189, #44673, #75167, #36693, #15677, #46162, #6677, #7178, #37681, #48111, #48604, #78625, #47631, #1666, #31137, #61630, #23674, #25636, #39157, #32618, #85142, #69647, #2656, #93618, #46636, #84649, #9637, #55630, #86621, #56126, #79108, #686, #32115, #16152, #86130, #62613, #40631, #17152, #18132, #92149, #71129, #10620, #41132, #9137, #55116, #33108, #92630, #63603, #17643, #10136, #94108, #54136, #70635, #39653, #1171, #77138, #8647, #70145, #31631, #62122, #24153, #93120, #54621, #16650, #47122, #77622, #78127, #24647, #85634, #40135, #2163, #63116, #25153, #50086, #58565, #41627, #13068, #80089, #64086, #71620, #42113, #3616, #12579, #26118, #49102, #65566, #35067, #89070, #11108, #56610, #57092, #28068, #87099, #57580, #65068, #96092, #34572, #79605, #19588, #20584, #27574, #4108, #95594, #27079, #42590, #5087, #88076, #88572, #18613, #80590, #35574, #94601, #73070, #12085, #87586, #4606, #20076, #34085, #72092, #58069, #43077, #50581, #64576, #81076, #19098, #95085, #51069, #73563, #26590, #66065, #72575, #49579, #96593, #81561, #3131, #33591, #11594, #84, #7067, #13567, #98588, #37567, #28569, #37071, #45042, #5591, #30531, #51573, #36068, #43560, #7574, #74058, #21075, #14575, #52550, #60545, #82059, #6075, #36576, #98081, #45544, #97590, #67064, #29050, #61032, #91544, #44054, #59557, #75551, #14076, #38060, #90543, #74559, #68058, #30037, #91038, #53530, #29540, #90054, #53036, #60045, #76041, #21577, #22075, #59062, #52065, #6561, #67569, #22567 ) ),
 .UNSPECIFIED., .F., .F., .F. ) 
 B_SPLINE_SURFACE_WITH_KNOTS ( ( 2, 2 ),
 ( 3, 2, 2, 2, 2, 2, 2, 2, 2, 2, 2, 2, 2, 2, 2, 2, 2, 2, 2, 2, 2, 2, 2, 2, 2, 2, 2, 2, 2, 2, 2, 2, 2, 2, 2, 2, 2, 2, 2, 2, 2, 2, 2, 2, 2, 2, 2, 2, 2, 2, 2, 2, 2, 2, 2, 2, 2, 2, 2, 2, 2, 2, 2, 2, 2, 2, 2, 2, 2, 2, 2, 2, 2, 2, 2, 2, 2, 2, 2, 2, 2, 2, 2, 2, 2, 2, 2, 2, 2, 2, 2, 2, 2, 2, 2, 2, 2, 2, 2, 2, 2, 2, 2, 2, 2, 2, 2, 2, 2, 2, 2, 2, 2, 2, 2, 2, 2, 2, 2, 2, 2, 2, 2, 2, 2, 2, 2, 2, 2, 2, 2, 2, 2, 2, 2, 2, 2, 2, 2, 2, 2, 2, 2, 2, 2, 2, 2, 2, 2, 2, 2, 2, 2, 2, 2, 2, 2, 2, 2, 2, 2, 2, 3 ),
 ( 0.000000000000000000, 1.000000000000000000 ),
 ( 0.000000000000000000, 0.005952380952380952051, 0.01190476190476190410, 0.01785714285714285615, 0.02380952380952380820, 0.02976190476190476025, 0.03571428571428571230, 0.04166666666666666435, 0.04761904761904761640, 0.05357142857142856845, 0.05952380952380952051, 0.06547619047619047949, 0.07142857142857142461, 0.07738095238095238360, 0.08333333333333332871, 0.08928571428571428770, 0.09523809523809523281, 0.1011904761904761918, 0.1071428571428571369, 0.1130952380952380959, 0.1190476190476190410, 0.1250000000000000000, 0.1309523809523809590, 0.1369047619047619180, 0.1428571428571428492, 0.1488095238095238082, 0.1547619047619047672, 0.1607142857142857262, 0.1666666666666666574, 0.1726190476190476164, 0.1785714285714285754, 0.1845238095238095344, 0.1904761904761904656, 0.1964285714285714246, 0.2023809523809523836, 0.2083333333333333426, 0.2142857142857142738, 0.2202380952380952328, 0.2261904761904761918, 0.2321428571428571508, 0.2380952380952380820, 0.2440476190476190410, 0.2500000000000000000, 0.2559523809523809312, 0.2619047619047619180, 0.2678571428571428492, 0.2738095238095238360, 0.2797619047619047672, 0.2857142857142856984, 0.2916666666666666852, 0.2976190476190476164, 0.3035714285714285476, 0.3095238095238095344, 0.3154761904761904656, 0.3214285714285714524, 0.3273809523809523836, 0.3333333333333333148, 0.3392857142857143016, 0.3452380952380952328, 0.3511904761904761640, 0.3571428571428571508, 0.3630952380952380820, 0.3690476190476190688, 0.3750000000000000000, 0.3809523809523809312, 0.3869047619047619180, 0.3928571428571428492, 0.3988095238095238360, 0.4047619047619047672, 0.4107142857142856984, 0.4166666666666666852, 0.4226190476190476164, 0.4285714285714285476, 0.4345238095238095344, 0.4404761904761904656, 0.4464285714285714524, 0.4523809523809523836, 0.4583333333333333148, 0.4642857142857143016, 0.4702380952380952328, 0.4761904761904761640, 0.4821428571428571508, 0.4880952380952380820, 0.4940476190476190688, 0.5000000000000000000, 0.5059523809523809312, 0.5119047619047618625, 0.5178571428571429047, 0.5238095238095238360, 0.5297619047619047672, 0.5357142857142856984, 0.5416666666666666297, 0.5476190476190476719, 0.5535714285714286031, 0.5595238095238095344, 0.5654761904761904656, 0.5714285714285713969, 0.5773809523809523281, 0.5833333333333333703, 0.5892857142857143016, 0.5952380952380952328, 0.6011904761904761640, 0.6071428571428570953, 0.6130952380952381375, 0.6190476190476190688, 0.6250000000000000000, 0.6309523809523809312, 0.6369047619047618625, 0.6428571428571429047, 0.6488095238095238360, 0.6547619047619047672, 0.6607142857142856984, 0.6666666666666666297, 0.6726190476190476719, 0.6785714285714286031, 0.6845238095238095344, 0.6904761904761904656, 0.6964285714285713969, 0.7023809523809523281, 0.7083333333333333703, 0.7142857142857143016, 0.7202380952380952328, 0.7261904761904761640, 0.7321428571428570953, 0.7380952380952381375, 0.7440476190476190688, 0.7500000000000000000, 0.7559523809523809312, 0.7619047619047618625, 0.7678571428571429047, 0.7738095238095238360, 0.7797619047619047672, 0.7857142857142856984, 0.7916666666666666297, 0.7976190476190476719, 0.8035714285714286031, 0.8095238095238095344, 0.8154761904761904656, 0.8214285714285713969, 0.8273809523809523281, 0.8333333333333333703, 0.8392857142857143016, 0.8452380952380952328, 0.8511904761904761640, 0.8571428571428570953, 0.8630952380952381375, 0.8690476190476190688, 0.8750000000000000000, 0.8809523809523809312, 0.8869047619047618625, 0.8928571428571429047, 0.8988095238095238360, 0.9047619047619047672, 0.9107142857142856984, 0.9166666666666666297, 0.9226190476190476719, 0.9285714285714286031, 0.9345238095238095344, 0.9404761904761904656, 0.9464285714285713969, 0.9523809523809523281, 0.9583333333333333703, 0.9642857142857143016 ),
 .UNSPECIFIED. ) 
 GEOMETRIC_REPRESENTATION_ITEM ( )  RATIONAL_B_SPLINE_SURFACE ( (
 ( 1.000000000000000000, 0.9659258262890683122, 1.000000000000000000, 0.9659258262890683122, 1.000000000000000000, 0.9659258262890683122, 1.000000000000000000, 0.9659258262890683122, 1.000000000000000000, 0.9659258262890683122, 1.000000000000000000, 0.9659258262890683122, 1.000000000000000000, 0.9659258262890683122, 1.000000000000000000, 0.9659258262890683122, 1.000000000000000000, 0.9659258262890683122, 1.000000000000000000, 0.9659258262890683122, 1.000000000000000000, 0.9659258262890683122, 1.000000000000000000, 0.9659258262890683122, 1.000000000000000000, 0.9659258262890683122, 1.000000000000000000, 0.9659258262890683122, 1.000000000000000000, 0.9659258262890683122, 1.000000000000000000, 0.9659258262890683122, 1.000000000000000000, 0.9659258262890683122, 1.000000000000000000, 0.9659258262890683122, 1.000000000000000000, 0.9659258262890683122, 1.000000000000000000, 0.9659258262890683122, 1.000000000000000000, 0.9659258262890683122, 1.000000000000000000, 0.9659258262890683122, 1.000000000000000000, 0.9659258262890683122, 1.000000000000000000, 0.9659258262890683122, 1.000000000000000000, 0.9659258262890683122, 1.000000000000000000, 0.9659258262890683122, 1.000000000000000000, 0.9659258262890683122, 1.000000000000000000, 0.9659258262890683122, 1.000000000000000000, 0.9659258262890683122, 1.000000000000000000, 0.9659258262890683122, 1.000000000000000000, 0.9659258262890683122, 1.000000000000000000, 0.9659258262890683122, 1.000000000000000000, 0.9659258262890683122, 1.000000000000000000, 0.9659258262890683122, 1.000000000000000000, 0.9659258262890683122, 1.000000000000000000, 0.9659258262890683122, 1.000000000000000000, 0.9659258262890683122, 1.000000000000000000, 0.9659258262890683122, 1.000000000000000000, 0.9659258262890683122, 1.000000000000000000, 0.9659258262890683122, 1.000000000000000000, 0.9659258262890683122, 1.000000000000000000, 0.9659258262890683122, 1.000000000000000000, 0.9659258262890683122, 1.000000000000000000, 0.9659258262890683122, 1.000000000000000000, 0.9659258262890683122, 1.000000000000000000, 0.9659258262890683122, 1.000000000000000000, 0.9659258262890683122, 1.000000000000000000, 0.9659258262890683122, 1.000000000000000000, 0.9659258262890683122, 1.000000000000000000, 0.9659258262890683122, 1.000000000000000000, 0.9659258262890683122, 1.000000000000000000, 0.9659258262890683122, 1.000000000000000000, 0.9659258262890683122, 1.000000000000000000, 0.9659258262890683122, 1.000000000000000000, 0.9659258262890683122, 1.000000000000000000, 0.9659258262890683122, 1.000000000000000000, 0.9659258262890683122, 1.000000000000000000, 0.9659258262890683122, 1.000000000000000000, 0.9659258262890683122, 1.000000000000000000, 0.9659258262890683122, 1.000000000000000000, 0.9659258262890683122, 1.000000000000000000, 0.9659258262890683122, 1.000000000000000000, 0.9659258262890683122, 1.000000000000000000, 0.9659258262890683122, 1.000000000000000000, 0.9659258262890683122, 1.000000000000000000, 0.9659258262890683122, 1.000000000000000000, 0.9659258262890683122, 1.000000000000000000, 0.9659258262890683122, 1.000000000000000000, 0.9659258262890683122, 1.000000000000000000, 0.9659258262890683122, 1.000000000000000000, 0.9659258262890683122, 1.000000000000000000, 0.9659258262890683122, 1.000000000000000000, 0.9659258262890683122, 1.000000000000000000, 0.9659258262890683122, 1.000000000000000000, 0.9659258262890683122, 1.000000000000000000, 0.9659258262890683122, 1.000000000000000000, 0.9659258262890683122, 1.000000000000000000, 0.9659258262890683122, 1.000000000000000000, 0.9659258262890683122, 1.000000000000000000, 0.9659258262890683122, 1.000000000000000000, 0.9659258262890683122, 1.000000000000000000, 0.9659258262890683122, 1.000000000000000000, 0.9659258262890683122, 1.000000000000000000, 0.9659258262890683122, 1.000000000000000000, 0.9659258262890683122, 1.000000000000000000, 0.9659258262890683122, 1.000000000000000000, 0.9659258262890683122, 1.000000000000000000, 0.9659258262890683122, 1.000000000000000000, 0.9659258262890683122, 1.000000000000000000, 0.9659258262890683122, 1.000000000000000000, 0.9659258262890683122, 1.000000000000000000, 0.9659258262890683122, 1.000000000000000000, 0.9659258262890683122, 1.000000000000000000, 0.9659258262890683122, 1.000000000000000000, 0.9659258262890683122, 1.000000000000000000, 0.9659258262890683122, 1.000000000000000000, 0.9659258262890683122, 1.000000000000000000, 0.9659258262890683122, 1.000000000000000000, 0.9659258262890683122, 1.000000000000000000, 0.9659258262890683122, 1.000000000000000000, 0.9659258262890683122, 1.000000000000000000, 0.9659258262890683122, 1.000000000000000000, 0.9659258262890683122, 1.000000000000000000, 0.9659258262890683122, 1.000000000000000000, 0.9659258262890683122, 1.000000000000000000, 0.9659258262890683122, 1.000000000000000000, 0.9659258262890683122, 1.000000000000000000, 0.9659258262890683122, 1.000000000000000000, 0.9659258262890683122, 1.000000000000000000, 0.9659258262890683122, 1.000000000000000000, 0.9659258262890683122, 1.000000000000000000, 0.9659258262890683122, 1.000000000000000000, 0.9659258262890683122, 1.000000000000000000, 0.9659258262890683122, 1.000000000000000000, 0.9659258262890683122, 1.000000000000000000, 0.9659258262890683122, 1.000000000000000000, 0.9659258262890683122, 1.000000000000000000, 0.9659258262890683122, 1.000000000000000000, 0.9659258262890683122, 1.000000000000000000, 0.9659258262890683122, 1.000000000000000000, 0.9659258262890683122, 1.000000000000000000, 0.9659258262890683122, 1.000000000000000000, 0.9659258262890683122, 1.000000000000000000, 0.9659258262890683122, 1.000000000000000000, 0.9659258262890683122, 1.000000000000000000, 0.9659258262890683122, 1.000000000000000000, 0.9659258262890683122, 1.000000000000000000, 0.9659258262890683122, 1.000000000000000000, 0.9659258262890683122, 1.000000000000000000, 0.9659258262890683122, 1.000000000000000000, 0.9659258262890683122, 1.000000000000000000, 0.9659258262890683122, 1.000000000000000000, 0.9659258262890683122, 1.000000000000000000, 0.9659258262890683122, 1.000000000000000000, 0.9659258262890683122, 1.000000000000000000, 0.9659258262890683122, 1.000000000000000000, 0.9659258262890683122, 1.000000000000000000, 0.9659258262890683122, 1.000000000000000000, 0.9659258262890683122, 1.000000000000000000, 0.9659258262890683122, 1.000000000000000000, 0.9659258262890683122, 1.000000000000000000, 0.9659258262890683122, 1.000000000000000000, 0.9659258262890683122, 1.000000000000000000, 0.9659258262890683122, 1.000000000000000000, 0.9659258262890683122, 1.000000000000000000, 0.9659258262890683122, 1.000000000000000000, 0.9659258262890683122, 1.000000000000000000, 0.9659258262890683122, 1.000000000000000000, 0.9659258262890683122, 1.000000000000000000, 0.9659258262890683122, 1.000000000000000000, 0.9659258262890683122, 1.000000000000000000, 0.9659258262890683122, 1.000000000000000000, 0.9659258262890683122, 1.000000000000000000, 0.9659258262890683122, 1.000000000000000000, 0.9659258262890683122, 1.000000000000000000, 0.9659258262890683122, 1.000000000000000000, 0.9659258262890683122, 1.000000000000000000, 0.9659258262890683122, 1.000000000000000000, 0.9659258262890683122, 1.000000000000000000, 0.9659258262890683122, 1.000000000000000000, 0.9659258262890683122, 1.000000000000000000, 0.9659258262890683122, 1.000000000000000000),
 ( 1.000000000000000000, 0.9659258262890683122, 1.000000000000000000, 0.9659258262890683122, 1.000000000000000000, 0.9659258262890683122, 1.000000000000000000, 0.9659258262890683122, 1.000000000000000000, 0.9659258262890683122, 1.000000000000000000, 0.9659258262890683122, 1.000000000000000000, 0.9659258262890683122, 1.000000000000000000, 0.9659258262890683122, 1.000000000000000000, 0.9659258262890683122, 1.000000000000000000, 0.9659258262890683122, 1.000000000000000000, 0.9659258262890683122, 1.000000000000000000, 0.9659258262890683122, 1.000000000000000000, 0.9659258262890683122, 1.000000000000000000, 0.9659258262890683122, 1.000000000000000000, 0.9659258262890683122, 1.000000000000000000, 0.9659258262890683122, 1.000000000000000000, 0.9659258262890683122, 1.000000000000000000, 0.9659258262890683122, 1.000000000000000000, 0.9659258262890683122, 1.000000000000000000, 0.9659258262890683122, 1.000000000000000000, 0.9659258262890683122, 1.000000000000000000, 0.9659258262890683122, 1.000000000000000000, 0.9659258262890683122, 1.000000000000000000, 0.9659258262890683122, 1.000000000000000000, 0.9659258262890683122, 1.000000000000000000, 0.9659258262890683122, 1.000000000000000000, 0.9659258262890683122, 1.000000000000000000, 0.9659258262890683122, 1.000000000000000000, 0.9659258262890683122, 1.000000000000000000, 0.9659258262890683122, 1.000000000000000000, 0.9659258262890683122, 1.000000000000000000, 0.9659258262890683122, 1.000000000000000000, 0.9659258262890683122, 1.000000000000000000, 0.9659258262890683122, 1.000000000000000000, 0.9659258262890683122, 1.000000000000000000, 0.9659258262890683122, 1.000000000000000000, 0.9659258262890683122, 1.000000000000000000, 0.9659258262890683122, 1.000000000000000000, 0.9659258262890683122, 1.000000000000000000, 0.9659258262890683122, 1.000000000000000000, 0.9659258262890683122, 1.000000000000000000, 0.9659258262890683122, 1.000000000000000000, 0.9659258262890683122, 1.000000000000000000, 0.9659258262890683122, 1.000000000000000000, 0.9659258262890683122, 1.000000000000000000, 0.9659258262890683122, 1.000000000000000000, 0.9659258262890683122, 1.000000000000000000, 0.9659258262890683122, 1.000000000000000000, 0.9659258262890683122, 1.000000000000000000, 0.9659258262890683122, 1.000000000000000000, 0.9659258262890683122, 1.000000000000000000, 0.9659258262890683122, 1.000000000000000000, 0.9659258262890683122, 1.000000000000000000, 0.9659258262890683122, 1.000000000000000000, 0.9659258262890683122, 1.000000000000000000, 0.9659258262890683122, 1.000000000000000000, 0.9659258262890683122, 1.000000000000000000, 0.9659258262890683122, 1.000000000000000000, 0.9659258262890683122, 1.000000000000000000, 0.9659258262890683122, 1.000000000000000000, 0.9659258262890683122, 1.000000000000000000, 0.9659258262890683122, 1.000000000000000000, 0.9659258262890683122, 1.000000000000000000, 0.9659258262890683122, 1.000000000000000000, 0.9659258262890683122, 1.000000000000000000, 0.9659258262890683122, 1.000000000000000000, 0.9659258262890683122, 1.000000000000000000, 0.9659258262890683122, 1.000000000000000000, 0.9659258262890683122, 1.000000000000000000, 0.9659258262890683122, 1.000000000000000000, 0.9659258262890683122, 1.000000000000000000, 0.9659258262890683122, 1.000000000000000000, 0.9659258262890683122, 1.000000000000000000, 0.9659258262890683122, 1.000000000000000000, 0.9659258262890683122, 1.000000000000000000, 0.9659258262890683122, 1.000000000000000000, 0.9659258262890683122, 1.000000000000000000, 0.9659258262890683122, 1.000000000000000000, 0.9659258262890683122, 1.000000000000000000, 0.9659258262890683122, 1.000000000000000000, 0.9659258262890683122, 1.000000000000000000, 0.9659258262890683122, 1.000000000000000000, 0.9659258262890683122, 1.000000000000000000, 0.9659258262890683122, 1.000000000000000000, 0.9659258262890683122, 1.000000000000000000, 0.9659258262890683122, 1.000000000000000000, 0.9659258262890683122, 1.000000000000000000, 0.9659258262890683122, 1.000000000000000000, 0.9659258262890683122, 1.000000000000000000, 0.9659258262890683122, 1.000000000000000000, 0.9659258262890683122, 1.000000000000000000, 0.9659258262890683122, 1.000000000000000000, 0.9659258262890683122, 1.000000000000000000, 0.9659258262890683122, 1.000000000000000000, 0.9659258262890683122, 1.000000000000000000, 0.9659258262890683122, 1.000000000000000000, 0.9659258262890683122, 1.000000000000000000, 0.9659258262890683122, 1.000000000000000000, 0.9659258262890683122, 1.000000000000000000, 0.9659258262890683122, 1.000000000000000000, 0.9659258262890683122, 1.000000000000000000, 0.9659258262890683122, 1.000000000000000000, 0.9659258262890683122, 1.000000000000000000, 0.9659258262890683122, 1.000000000000000000, 0.9659258262890683122, 1.000000000000000000, 0.9659258262890683122, 1.000000000000000000, 0.9659258262890683122, 1.000000000000000000, 0.9659258262890683122, 1.000000000000000000, 0.9659258262890683122, 1.000000000000000000, 0.9659258262890683122, 1.000000000000000000, 0.9659258262890683122, 1.000000000000000000, 0.9659258262890683122, 1.000000000000000000, 0.9659258262890683122, 1.000000000000000000, 0.9659258262890683122, 1.000000000000000000, 0.9659258262890683122, 1.000000000000000000, 0.9659258262890683122, 1.000000000000000000, 0.9659258262890683122, 1.000000000000000000, 0.9659258262890683122, 1.000000000000000000, 0.9659258262890683122, 1.000000000000000000, 0.9659258262890683122, 1.000000000000000000, 0.9659258262890683122, 1.000000000000000000, 0.9659258262890683122, 1.000000000000000000, 0.9659258262890683122, 1.000000000000000000, 0.9659258262890683122, 1.000000000000000000, 0.9659258262890683122, 1.000000000000000000, 0.9659258262890683122, 1.000000000000000000, 0.9659258262890683122, 1.000000000000000000, 0.9659258262890683122, 1.000000000000000000, 0.9659258262890683122, 1.000000000000000000, 0.9659258262890683122, 1.000000000000000000, 0.9659258262890683122, 1.000000000000000000, 0.9659258262890683122, 1.000000000000000000, 0.9659258262890683122, 1.000000000000000000, 0.9659258262890683122, 1.000000000000000000, 0.9659258262890683122, 1.000000000000000000, 0.9659258262890683122, 1.000000000000000000, 0.9659258262890683122, 1.000000000000000000, 0.9659258262890683122, 1.000000000000000000, 0.9659258262890683122, 1.000000000000000000, 0.9659258262890683122, 1.000000000000000000, 0.9659258262890683122, 1.000000000000000000, 0.9659258262890683122, 1.000000000000000000, 0.9659258262890683122, 1.000000000000000000, 0.9659258262890683122, 1.000000000000000000, 0.9659258262890683122, 1.000000000000000000, 0.9659258262890683122, 1.000000000000000000, 0.9659258262890683122, 1.000000000000000000, 0.9659258262890683122, 1.000000000000000000, 0.9659258262890683122, 1.000000000000000000, 0.9659258262890683122, 1.000000000000000000, 0.9659258262890683122, 1.000000000000000000, 0.9659258262890683122, 1.000000000000000000, 0.9659258262890683122, 1.000000000000000000, 0.9659258262890683122, 1.000000000000000000, 0.9659258262890683122, 1.000000000000000000, 0.9659258262890683122, 1.000000000000000000, 0.9659258262890683122, 1.000000000000000000, 0.9659258262890683122, 1.000000000000000000, 0.9659258262890683122, 1.000000000000000000, 0.9659258262890683122, 1.000000000000000000, 0.9659258262890683122, 1.000000000000000000, 0.9659258262890683122, 1.000000000000000000) ) ) 
 REPRESENTATION_ITEM ( '' )  SURFACE ( )  );
#45573 = CARTESIAN_POINT ( 'NONE',  ( 10.00000000000000178, 8.053748834913967869, 14.16423886937410082 ) ) ;
#45574 = CARTESIAN_POINT ( 'NONE',  ( 9.050000000000002487, 99.99999999999998579, -8.525133428036873795 ) ) ;
#45575 = CARTESIAN_POINT ( 'NONE',  ( -46.94000000000001194, 93.00000000000000000, 9.000000000000000000 ) ) ;
#45576 = CARTESIAN_POINT ( 'NONE',  ( 12.91533473730993009, 6.605352010821504471, -10.88017736071109987 ) ) ;
#45577 = DIRECTION ( 'NONE',  ( -2.107602052970795044E-16, 1.000000000000000000, 0.000000000000000000 ) ) ;
#45579 = ORIENTED_EDGE ( 'NONE', *, *, #26477, .T. ) ;
#45578 = CARTESIAN_POINT ( 'NONE',  ( 16.40814093676324603, 47.45696800326375353, -11.09922568453594671 ) ) ;
#45580 = DIRECTION ( 'NONE',  ( 1.000000000000000000, -8.673617379884027583E-16, 0.000000000000000000 ) ) ;
#45581 = CARTESIAN_POINT ( 'NONE',  ( 1.472469842513823179, 50.59226448433411605, -4.923371831947296329 ) ) ;
#45582 = CARTESIAN_POINT ( 'NONE',  ( 0.1532563361054100626, 0.8005978176674514168, -2.638427012816831230 ) ) ;
#45583 = CARTESIAN_POINT ( 'NONE',  ( 22.81628187352647785, 16.41530133659708923, 3.434112377981063169 ) ) ;
#45584 = CARTESIAN_POINT ( 'NONE',  ( 18.52753015748617571, 18.09226448433411960, 4.923371831947298993 ) ) ;
#45585 = CARTESIAN_POINT ( 'NONE',  ( 1.274849032794294290, 63.57228050351031357, 6.499999999999979572 ) ) ;
#45586 = CARTESIAN_POINT ( 'NONE',  ( 19.38216949554541202, 20.99863466993042138, 9.382169495545424454 ) ) ;
#45587 = CARTESIAN_POINT ( 'NONE',  ( 2.603489959281060973, 26.58210964143323096, 6.499999999999401368 ) ) ;
#45588 = CARTESIAN_POINT ( 'NONE',  ( 2.791683348922237240, 5.383931151000785675, -7.208316651077763204 ) ) ;
#45589 = ORIENTED_EDGE ( 'NONE', *, *, #80948, .F. ) ;
#45590 = ORIENTED_EDGE ( 'NONE', *, *, #73141, .T. ) ;
#45591 = CARTESIAN_POINT ( 'NONE',  ( 20.88017736071110164, 20.35535201082150891, 2.915334737309930979 ) ) ;
#45592 = CARTESIAN_POINT ( 'NONE',  ( 17.08211943468705130, 18.47041550158063572, 12.26659068614894998 ) ) ;
#45593 = CARTESIAN_POINT ( 'NONE',  ( 2.791683348922237240, 45.38393115100079456, -7.208316651077763204 ) ) ;
#45594 = CARTESIAN_POINT ( 'NONE',  ( 2.791683348922237240, 5.383931151000785675, -7.208316651077763204 ) ) ;
#45596 = CARTESIAN_POINT ( 'NONE',  ( 6.879999999999995453, 79.82179676972448590, -6.500000000000000888 ) ) ;
#45595 = CARTESIAN_POINT ( 'NONE',  ( -1.099225684535947600, 39.54030133659708923, 6.408140936763237150 ) ) ;
#45597 = CARTESIAN_POINT ( 'NONE',  ( 10.00000000000000178, 9.313685344154839285, 10.88017736071110342 ) ) ;
#45598 = LINE ( 'NONE', #92087, #19872 ) ;
#45599 = CARTESIAN_POINT ( 'NONE',  ( 10.00000000000000178, 15.37363466993042138, 12.81628187352647608 ) ) ;
#45600 = CARTESIAN_POINT ( 'NONE',  ( 13.43411237798106583, 12.66530133659708746, -12.81628187352647252 ) ) ;
#45601 = CARTESIAN_POINT ( 'NONE',  ( 0.1532563361054100626, 30.80059781766744820, -2.638427012816831230 ) ) ;
#45602 = CARTESIAN_POINT ( 'NONE',  ( -10.88017736071110164, -12.14464798917849642, -2.915334737309917212 ) ) ;
#45603 = CARTESIAN_POINT ( 'NONE',  ( 0.6178305044545818747, 33.49863466993042493, -9.382169495545419124 ) ) ;
#45604 = LINE ( 'NONE', #30096, #57981 ) ;
#45605 = ADVANCED_FACE ( 'NONE', ( #66388 ), #52870, .T. ) ;
#45607 = LINE ( 'NONE', #51133, #30404 ) ;
#45606 = CARTESIAN_POINT ( 'NONE',  ( 7.084665262690076126, 44.10535201082151247, 10.88017736071109987 ) ) ;
#45608 = PRESENTATION_LAYER_ASSIGNMENT (  '', '', ( #75938 ) ) ;
#45609 = DIRECTION ( 'NONE',  ( 0.000000000000000000, -1.000000000000000000, 0.000000000000000000 ) ) ;
#45610 = CARTESIAN_POINT ( 'NONE',  ( 17.96484262340118221, 66.18868534415483396, -7.964842623401177768 ) ) ;
#45611 = CARTESIAN_POINT ( 'NONE',  ( 20.88017736071110164, 35.35535201082150536, 2.915334737309930979 ) ) ;
#45612 = CARTESIAN_POINT ( 'NONE',  ( -0.8801773607111009756, 48.06368534415484817, 1.068504757029289695E-15 ) ) ;
#45613 = CARTESIAN_POINT ( 'NONE',  ( 2.791683348922237240, 60.38393115100078745, -7.208316651077763204 ) ) ;
#45614 = CARTESIAN_POINT ( 'NONE',  ( -7.109031286574684749, 0.04962885628204312394, -12.92745085449648101 ) ) ;
#45615 = CIRCLE ( 'NONE', #23304, 14.49999999999999822 ) ;
#45616 = EDGE_CURVE ( 'NONE', #40405, #35851, #63977, .T. ) ;
#45617 = EDGE_CURVE ( 'NONE', #43266, #54617, #78407, .T. ) ;
#45618 = CARTESIAN_POINT ( 'NONE',  ( 0.1532563361054100626, 45.80059781766745886, -2.638427012816831230 ) ) ;
#45620 = PLANE ( 'NONE',  #70295 ) ;
#45619 = CARTESIAN_POINT ( 'NONE',  ( 7.084665262690076126, 4.105352010821503583, 10.88017736071109987 ) ) ;
#45621 = CARTESIAN_POINT ( 'NONE',  ( 22.81628187352648496, 11.83196800326375531, -3.434112377981050290 ) ) ;
#45622 = ORIENTED_EDGE ( 'NONE', *, *, #93597, .F. ) ;
#45623 = CARTESIAN_POINT ( 'NONE',  ( 0.5774900079438607392, 33.48035201082150536, 5.440088680355550821 ) ) ;
#45625 =( LENGTH_UNIT ( ) NAMED_UNIT ( * ) SI_UNIT ( .MILLI., .METRE. ) );
#45624 = CARTESIAN_POINT ( 'NONE',  ( 1.472469842513823179, 65.59226448433412315, -4.923371831947296329 ) ) ;
#45626 = CARTESIAN_POINT ( 'NONE',  ( 17.96484262340118221, 4.938685344154837509, 7.964842623401181321 ) ) ;
#45627 = CARTESIAN_POINT ( 'NONE',  ( 7.084665262690076126, 24.10535201082150181, 10.88017736071109987 ) ) ;
#45628 = CARTESIAN_POINT ( 'NONE',  ( 24.16423886937409904, 34.09541550158064638, 3.795296366450317205 ) ) ;
#45629 = CARTESIAN_POINT ( 'NONE',  ( 14.92337183194729633, 32.67559781766745175, 8.527530157486181039 ) ) ;
#45630 = CARTESIAN_POINT ( 'NONE',  ( 12.91533473730993009, 41.60535201082149825, -10.88017736071109987 ) ) ;
#45631 = CARTESIAN_POINT ( 'NONE',  ( 22.26659068614895176, 9.720415501580633943, -7.082119434687042414 ) ) ;
#45632 = TOROIDAL_SURFACE ( 'NONE', #24884, 14.49999999999999822, 0.5000000000000000000 ) ;
#45633 = CARTESIAN_POINT ( 'NONE',  ( -46.83212803583222694, 103.4681393821014836, 5.836481404741387102 ) ) ;
#45634 = CARTESIAN_POINT ( 'NONE',  ( 19.84674366389459266, 58.71726448433411605, -2.638427012816827677 ) ) ;
#45635 = AXIS2_PLACEMENT_3D ( 'NONE', #73312, #6305, #96834 ) ;
#45636 = ORIENTED_EDGE ( 'NONE', *, *, #43684, .F. ) ;
#45637 = ORIENTED_EDGE ( 'NONE', *, *, #85395, .T. ) ;
#45638 = CIRCLE ( 'NONE', #28073, 14.49999999999999822 ) ;
#45639 = CARTESIAN_POINT ( 'NONE',  ( -0.3689425029237898834, 31.17874883491396787, -10.36894250292378850 ) ) ;
#45640 = CARTESIAN_POINT ( 'NONE',  ( 10.00000000000000178, 28.05374883491396787, 14.16423886937410082 ) ) ;
#45641 = CARTESIAN_POINT ( 'NONE',  ( 10.00000000000000000, 4.758931151000784787, -9.846743663894594434 ) ) ;
#45642 = EDGE_CURVE ( 'NONE', #28421, #18735, #41672, .T. ) ;
#45643 = CARTESIAN_POINT ( 'NONE',  ( -0.3689425029237881626, 62.42874883491396787, 10.36894250292379027 ) ) ;
#45644 = CARTESIAN_POINT ( 'NONE',  ( 18.52753015748618282, 53.92559781766745175, -4.923371831947291888 ) ) ;
#45645 = CARTESIAN_POINT ( 'NONE',  ( -8.647950603528085978, -15.58161425315045534, 4.000000000000000000 ) ) ;
#45647 = CARTESIAN_POINT ( 'NONE',  ( 19.38216949554541557, 22.24863466993041428, -9.382169495545420901 ) ) ;
#45646 = CARTESIAN_POINT ( 'NONE',  ( 4.559911319644449179, 47.23035201082150536, -9.422509992056141925 ) ) ;
#45648 = CARTESIAN_POINT ( 'NONE',  ( 20.36894250292379382, 13.67874883491396965, 10.36894250292379205 ) ) ;
#45649 = CARTESIAN_POINT ( 'NONE',  ( 12.91533473730992121, 14.52201867748817143, 10.88017736071110164 ) ) ;
#45650 = VECTOR ( 'NONE', #56626, 1000.000000000000000 ) ;
#45651 = CARTESIAN_POINT ( 'NONE',  ( 19.42250999205614548, 35.98035201082151247, -5.440088680355545492 ) ) ;
#45652 =( NAMED_UNIT ( * ) SI_UNIT ( $, .STERADIAN. ) SOLID_ANGLE_UNIT ( ) );
#45653 = CARTESIAN_POINT ( 'NONE',  ( -0.8801773607111008646, 53.27201867748816966, 2.915334737309923430 ) ) ;
#45654 = EDGE_CURVE ( 'NONE', #18045, #57285, #8789, .T. ) ;
#45655 = CARTESIAN_POINT ( 'NONE',  ( -7.208316651077756099, -18.36606884899920900, 7.208316651077766757 ) ) ;
#45656 = VERTEX_POINT ( 'NONE', #91864 ) ;
#45657 = CARTESIAN_POINT ( 'NONE',  ( 0.1034006766821536916, 15.00000000000000000, -14.49963131600461352 ) ) ;
#45658 = ORIENTED_EDGE ( 'NONE', *, *, #26632, .T. ) ;
#45659 = CARTESIAN_POINT ( 'NONE',  ( -6.000000000000014211, 79.82179676972448590, -6.500000000000000888 ) ) ;
#45660 = EDGE_LOOP ( 'NONE', ( #32710, #65028, #83095, #15811, #27925, #90821, #69507, #90085, #29287, #55154, #98663, #27588, #35001, #41738, #5451, #24020, #70969, #65717, #53896, #76327, #35192, #15496, #79201, #26979, #216, #30954, #75913, #44669, #27470, #19025, #82340, #12010 ) ) ;
#45661 = CARTESIAN_POINT ( 'NONE',  ( -0.7375392941519193224, 0.3639308982088595434, 14.98185688723474129 ) ) ;
#45663 = CARTESIAN_POINT ( 'NONE',  ( 2.917880565312950480, 60.97041550158063927, -12.26659068614894821 ) ) ;
#45662 = CARTESIAN_POINT ( 'NONE',  ( 20.36894250292379382, 63.67874883491396787, 10.36894250292379205 ) ) ;
#45665 = CARTESIAN_POINT ( 'NONE',  ( 18.52753015748618282, 53.92559781766745175, -4.923371831947291888 ) ) ;
#45664 = CARTESIAN_POINT ( 'NONE',  ( 17.20831665107776587, 22.88393115100078745, 7.208316651077764980 ) ) ;
#45666 = DIRECTION ( 'NONE',  ( 0.1132032137679039180, 0.000000000000000000, 0.9935718556765877896 ) ) ;
#45667 = DIRECTION ( 'NONE',  ( -0.000000000000000000, -1.000000000000000000, -0.000000000000000000 ) ) ;
#45668 = CARTESIAN_POINT ( 'NONE',  ( 19.84674366389459266, 8.717264484334116048, -2.638427012816827677 ) ) ;
#45669 = CIRCLE ( 'NONE', #40890, 14.49999999999999822 ) ;
#45670 = CARTESIAN_POINT ( 'NONE',  ( -11.09922568453594316, 19.54030133659709279, 6.408140936763246920 ) ) ;
#45671 = ORIENTED_EDGE ( 'NONE', *, *, #4569, .T. ) ;
#45672 = CARTESIAN_POINT ( 'NONE',  ( 17.08211943468705130, 33.47041550158063927, 12.26659068614894998 ) ) ;
#45673 = CARTESIAN_POINT ( 'NONE',  ( 24.16423886937409904, 39.09541550158062506, 3.795296366450317205 ) ) ;
#45674 = VERTEX_POINT ( 'NONE', #17355 ) ;
#45675 = CARTESIAN_POINT ( 'NONE',  ( -1.099225684535947600, 59.54030133659708923, 6.408140936763237150 ) ) ;
#45676 = CARTESIAN_POINT ( 'NONE',  ( 10.00000000000000000, 21.81368534415484106, -10.88017736071110342 ) ) ;
#45677 = CARTESIAN_POINT ( 'NONE',  ( 7.361572987183169658, 44.96726448433412315, -9.846743663894592657 ) ) ;
#45678 = CARTESIAN_POINT ( 'NONE',  ( 4.559911319644449179, 22.23035201082150536, -9.422509992056141925 ) ) ;
#45679 = CARTESIAN_POINT ( 'NONE',  ( -1.099225684535947600, 63.70696800326376774, -6.408140936763238038 ) ) ;
#45680 = DIRECTION ( 'NONE',  ( 0.000000000000000000, 1.000000000000000000, 0.000000000000000000 ) ) ;
#45681 = CARTESIAN_POINT ( 'NONE',  ( 2.791683348922237240, 60.38393115100078745, -7.208316651077763204 ) ) ;
#45682 = CARTESIAN_POINT ( 'NONE',  ( 10.00000000000000000, 49.75893115100078745, -9.846743663894594434 ) ) ;
#45683 = CIRCLE ( 'NONE', #7365, 15.00000000000000000 ) ;
#45684 = AXIS2_PLACEMENT_3D ( 'NONE', #3168, #64617, #5132 ) ;
#45685 = LINE ( 'NONE', #60676, #37732 ) ;
#45686 = DIRECTION ( 'NONE',  ( 1.000000000000000000, 0.000000000000000000, 0.000000000000000000 ) ) ;
#45687 = DIRECTION ( 'NONE',  ( 1.000000000000000000, 3.828355257328124777E-15, 0.000000000000000000 ) ) ;
#45688 = ORIENTED_EDGE ( 'NONE', *, *, #96782, .F. ) ;
#45689 = FILL_AREA_STYLE ('',( #15210 ) ) ;
#45690 = CARTESIAN_POINT ( 'NONE',  ( 12.63842701281683034, 32.46726448433412315, 9.846743663894596210 ) ) ;
#45691 = CARTESIAN_POINT ( 'NONE',  ( -12.07856007377833407, 3.961594683405543780E-16, 8.022367888854752493 ) ) ;
#45692 = CARTESIAN_POINT ( 'NONE',  ( 21.09922568453595559, 37.04030133659708923, -6.408140936763230044 ) ) ;
#45693 = FACE_OUTER_BOUND ( 'NONE', #29166, .T. ) ;
#45694 = CARTESIAN_POINT ( 'NONE',  ( -0.03743638938522799581, 39.25197528031018379, -6.399506433553962204 ) ) ;
#45695 = ORIENTED_EDGE ( 'NONE', *, *, #34109, .T. ) ;
#45696 = CARTESIAN_POINT ( 'NONE',  ( 14.92337183194729988, 64.34226448433412315, -8.527530157486177487 ) ) ;
#45697 = DIRECTION ( 'NONE',  ( 0.000000000000000000, 1.000000000000000000, 0.000000000000000000 ) ) ;
#45698 = CARTESIAN_POINT ( 'NONE',  ( 0.1532563361054100626, 40.80059781766745886, -2.638427012816831230 ) ) ;
#45699 = CARTESIAN_POINT ( 'NONE',  ( -4.164238869374098151, 36.59541550158063217, -3.795296366450310543 ) ) ;
#45700 = CARTESIAN_POINT ( 'NONE',  ( 2.791683348922237240, 55.38393115100078745, -7.208316651077763204 ) ) ;
#45701 = CARTESIAN_POINT ( 'NONE',  ( -9.402796353261225093, 14.49999999999999112, 11.68706210897757281 ) ) ;
#45702 = CARTESIAN_POINT ( 'NONE',  ( 2.791683348922237240, 0.3839311510007847872, -7.208316651077763204 ) ) ;
#45703 =( LENGTH_UNIT ( ) NAMED_UNIT ( * ) SI_UNIT ( .MILLI., .METRE. ) );
#45704 = EDGE_CURVE ( 'NONE', #5362, #1078, #76774, .T. ) ;
#45705 = CARTESIAN_POINT ( 'NONE',  ( 10.00000000000000000, 49.75893115100078745, -9.846743663894594434 ) ) ;
#45706 = CARTESIAN_POINT ( 'NONE',  ( 17.96484262340118221, 56.18868534415484817, -7.964842623401177768 ) ) ;
#45707 = AXIS2_PLACEMENT_3D ( 'NONE', #13857, #44337, #50361 ) ;
#45708 = CARTESIAN_POINT ( 'NONE',  ( 1.472469842513823179, 46.42559781766745175, 4.923371831947296329 ) ) ;
#45709 = APPLICATION_PROTOCOL_DEFINITION ( 'draft international standard', 'automotive_design', 1998, #4669 ) ;
#45710 = CARTESIAN_POINT ( 'NONE',  ( 13.75801628063878645, 4.006593314786880238E-16, 4.578972376164555769 ) ) ;
#45711 =( GEOMETRIC_REPRESENTATION_CONTEXT ( 3 ) GLOBAL_UNCERTAINTY_ASSIGNED_CONTEXT ( ( #10210 ) ) GLOBAL_UNIT_ASSIGNED_CONTEXT ( ( #67804, #10253, #87216 ) ) REPRESENTATION_CONTEXT ( 'NONE', 'WORKASPACE' ) );
#45712 = VERTEX_POINT ( 'NONE', #85841 ) ;
#45713 = CARTESIAN_POINT ( 'NONE',  ( 2.035157376598824452, 48.68868534415483396, 7.964842623401179544 ) ) ;
#45714 = ORIENTED_EDGE ( 'NONE', *, *, #71907, .F. ) ;
#45715 = DIRECTION ( 'NONE',  ( 0.4305110968083047940, 0.000000000000000000, -0.9025852843498560762 ) ) ;
#45716 = CARTESIAN_POINT ( 'NONE',  ( 20.88017736071110519, 35.56368534415484106, 2.639326808657452039E-16 ) ) ;
#45718 = CARTESIAN_POINT ( 'NONE',  ( 0.5774900079438607392, 58.48035201082151247, 5.440088680355550821 ) ) ;
#45717 = CARTESIAN_POINT ( 'NONE',  ( -2.816281873526473856, 4.331968003263754419, 3.434112377981055619 ) ) ;
#45719 = DIRECTION ( 'NONE',  ( -0.000000000000000000, -1.000000000000000000, -0.000000000000000000 ) ) ;
#45720 = CARTESIAN_POINT ( 'NONE',  ( 18.52753015748618282, 13.92559781766745175, -4.923371831947291888 ) ) ;
#45721 = SURFACE_STYLE_FILL_AREA ( #30698 ) ;
#45723 = CARTESIAN_POINT ( 'NONE',  ( -7.199999999999996625, 99.99999999999998579, 8.000000000000000000 ) ) ;
#45722 = CARTESIAN_POINT ( 'NONE',  ( 4.559911319644449179, 43.89701867748816966, 9.422509992056141925 ) ) ;
#45724 = CARTESIAN_POINT ( 'NONE',  ( 10.00000000000000000, 9.758931151000785675, -9.846743663894594434 ) ) ;
#45725 = CARTESIAN_POINT ( 'NONE',  ( 17.20831665107776587, 37.88393115100078745, 7.208316651077764980 ) ) ;
#45726 = CARTESIAN_POINT ( 'NONE',  ( 19.88565890683628012, 57.71691075486304356, -6.480892540919849232 ) ) ;
#45727 = CARTESIAN_POINT ( 'NONE',  ( 7.082119434687047743, 20.13708216824730712, -12.26659068614894821 ) ) ;
#45728 = CARTESIAN_POINT ( 'NONE',  ( -2.816281873526471635, -1.084698663402913210, -3.434112377981056508 ) ) ;
#45729 = EDGE_CURVE ( 'NONE', #63731, #74051, #47329, .T. ) ;
#45730 = CARTESIAN_POINT ( 'NONE',  ( 6.204703633549690345, 60.76208216824730357, -14.16423886937410259 ) ) ;
#45731 = CARTESIAN_POINT ( 'NONE',  ( 9.898881779040729967, 0.000000000000000000, -10.25059215482576214 ) ) ;
#45732 = CARTESIAN_POINT ( 'NONE',  ( 24.16423886937410614, 19.51208216824729647, -3.795296366450302550 ) ) ;
#45733 = AXIS2_PLACEMENT_3D ( 'NONE', #21962, #75437, #60429 ) ;
#45734 = CARTESIAN_POINT ( 'NONE',  ( 17.08211943468705130, 48.47041550158063927, 12.26659068614894998 ) ) ;
#45735 = VECTOR ( 'NONE', #12362, 999.9999999999998863 ) ;
#45736 = CARTESIAN_POINT ( 'NONE',  ( 12.63842701281683034, 12.46726448433411782, 9.846743663894596210 ) ) ;
#45737 = CARTESIAN_POINT ( 'NONE',  ( 2.035157376598822676, 2.438685344154837953, -7.964842623401177768 ) ) ;
#45738 = ADVANCED_FACE ( 'NONE', ( #91363 ), #77830, .F. ) ;
#45739 = VERTEX_POINT ( 'NONE', #9342 ) ;
#45740 = CARTESIAN_POINT ( 'NONE',  ( 18.52753015748617571, 28.09226448433411960, 4.923371831947298993 ) ) ;
#45741 = CARTESIAN_POINT ( 'NONE',  ( -0.8801773607111009756, 33.06368534415484106, 1.068504757029289695E-15 ) ) ;
#45742 = CARTESIAN_POINT ( 'NONE',  ( 14.92337183194729988, 44.34226448433412315, -8.527530157486177487 ) ) ;
#45744 = DIRECTION ( 'NONE',  ( -0.000000000000000000, 0.000000000000000000, -1.000000000000000000 ) ) ;
#45743 = CARTESIAN_POINT ( 'NONE',  ( 10.00000000000000178, 3.053748834913967425, 14.16423886937410082 ) ) ;
#45745 = FACE_OUTER_BOUND ( 'NONE', #62649, .T. ) ;
#45746 = ADVANCED_FACE ( 'NONE', ( #31834 ), #30858, .F. ) ;
#45747 = CARTESIAN_POINT ( 'NONE',  ( 12.63842701281683922, 14.55059781766744997, -9.846743663894590881 ) ) ;
#45748 = CARTESIAN_POINT ( 'NONE',  ( 3.591859063236763294, 33.29030133659708213, -11.09922568453595026 ) ) ;
#45749 = CARTESIAN_POINT ( 'NONE',  ( 7.361572987183169658, 44.96726448433412315, -9.846743663894592657 ) ) ;
#45750 = ORIENTED_EDGE ( 'NONE', *, *, #46498, .F. ) ;
#45751 = CARTESIAN_POINT ( 'NONE',  ( 12.63842701281683034, 27.46726448433411250, 9.846743663894596210 ) ) ;
#45752 = CARTESIAN_POINT ( 'NONE',  ( 10.72174155808380647, -40.27583460510356161, -3.999999999992825739 ) ) ;
#45753 = CARTESIAN_POINT ( 'NONE',  ( -11.96291822454869802, 4.725512573308054359E-16, -8.193813980849247613 ) ) ;
#45754 = CARTESIAN_POINT ( 'NONE',  ( 24.16423886937410614, 54.30374883491396787, 8.672049930838204340E-16 ) ) ;
#45755 = LINE ( 'NONE', #77223, #23478 ) ;
#45756 =( NAMED_UNIT ( * ) PLANE_ANGLE_UNIT ( ) SI_UNIT ( $, .RADIAN. ) );
#45757 = B_SPLINE_CURVE_WITH_KNOTS ( 'NONE', 3,
 ( #28347, #81348, #7714, #65346, #91689, #42375 ),
 .UNSPECIFIED., .F., .F.,
 ( 4, 2, 4 ),
 ( 0.0002800138956522161475, 0.0006862192609926581061, 0.001092424626333100010 ),
 .UNSPECIFIED. ) ;
#45758 = CARTESIAN_POINT ( 'NONE',  ( 14.92337183194729988, 34.34226448433411605, -8.527530157486177487 ) ) ;
#45759 = CARTESIAN_POINT ( 'NONE',  ( 20.88017736071110875, 5.772018677488170546, -2.915334737309920765 ) ) ;
#45760 = CARTESIAN_POINT ( 'NONE',  ( 0.1532563361054100626, 45.80059781766745886, -2.638427012816831230 ) ) ;
#45761 = CARTESIAN_POINT ( 'NONE',  ( 17.39651004071841811, 2.935752660568277328, 6.500000000000002665 ) ) ;
#45762 = CARTESIAN_POINT ( 'NONE',  ( 0.1532563361054082862, 51.21726448433412315, 2.638427012816831674 ) ) ;
#45763 = PRESENTATION_LAYER_ASSIGNMENT (  '', '', ( #1091 ) ) ;
#45764 = CARTESIAN_POINT ( 'NONE',  ( 20.88017736071110875, 55.77201867748816966, -2.915334737309920765 ) ) ;
#45765 = B_SPLINE_CURVE_WITH_KNOTS ( 'NONE', 3,
 ( #29577, #98627, #67609, #51615 ),
 .UNSPECIFIED., .F., .F.,
 ( 4, 4 ),
 ( 5.421010862427522170E-20, 0.002657014572711345439 ),
 .UNSPECIFIED. ) ;
#45766 = ORIENTED_EDGE ( 'NONE', *, *, #11405, .F. ) ;
#45767 = VERTEX_POINT ( 'NONE', #1869 ) ;
#45768 = CARTESIAN_POINT ( 'NONE',  ( 0.6178305044545818747, 53.49863466993041072, -9.382169495545419124 ) ) ;
#45769 = DIRECTION ( 'NONE',  ( -0.9961946980917462113, 0.08715574274765114371, 0.000000000000000000 ) ) ;
#45770 = CARTESIAN_POINT ( 'NONE',  ( 12.63842701281683034, 7.467264484334118713, 9.846743663894596210 ) ) ;
#45771 = CARTESIAN_POINT ( 'NONE',  ( 6.565887622018943937, 53.08196800326374643, -12.81628187352647608 ) ) ;
#45773 = CARTESIAN_POINT ( 'NONE',  ( 2.791683348922240793, 51.63393115100078745, 7.208316651077764092 ) ) ;
#45772 = CARTESIAN_POINT ( 'NONE',  ( -0.3689425029237898834, 66.17874883491396076, -10.36894250292378850 ) ) ;
#45774 = CARTESIAN_POINT ( 'NONE',  ( 0.000000000000000000, 99.74999999999998579, 8.000000000000000000 ) ) ;
#45775 = CARTESIAN_POINT ( 'NONE',  ( 6.204703633549690345, 27.84541550158063217, 14.16423886937410082 ) ) ;
#45776 = STYLED_ITEM ( 'NONE', ( #22427 ), #30522 ) ;
#45777 = CARTESIAN_POINT ( 'NONE',  ( 24.16423886937409904, 64.09541550158064638, 3.795296366450317205 ) ) ;
#45778 = CARTESIAN_POINT ( 'NONE',  ( 1.472469842513823179, 50.59226448433411605, -4.923371831947296329 ) ) ;
#45779 = CARTESIAN_POINT ( 'NONE',  ( 4.323020469702378854, -6.401304200487259344, -2.500000000000000888 ) ) ;
#45780 = CARTESIAN_POINT ( 'NONE',  ( 0.5774900079438590739, 47.64701867748817676, -5.440088680355550821 ) ) ;
#45781 = EDGE_CURVE ( 'NONE', #67494, #44632, #56020, .T. ) ;
#45782 = CARTESIAN_POINT ( 'NONE',  ( -0.8801773607111009756, 68.06368534415484817, 1.068504757029289695E-15 ) ) ;
#45783 = SURFACE_STYLE_USAGE ( .BOTH. , #15783 ) ;
#45784 = EDGE_LOOP ( 'NONE', ( #14160, #33466, #38800, #20797 ) ) ;
#45785 = CARTESIAN_POINT ( 'NONE',  ( 16.40814093676323893, 60.79030133659709634, 11.09922568453595026 ) ) ;
#45786 =( BOUNDED_CURVE ( )  B_SPLINE_CURVE ( 2, ( #42339, #58806, #96341, #27816, #12813, #72322, #97329, #58301, #43312 ),
 .UNSPECIFIED., .F., .F. ) 
 B_SPLINE_CURVE_WITH_KNOTS ( ( 3, 2, 2, 2, 3 ),
 ( 0.8320003743640370653, 0.8333333333333333703, 0.8392857142857143016, 0.8452380952380952328, 0.8465710542073914269 ),
 .UNSPECIFIED. ) 
 CURVE ( )  GEOMETRIC_REPRESENTATION_ITEM ( )  RATIONAL_B_SPLINE_CURVE ( ( 0.9881565478350742282, 0.9923695281211498687, 1.000000000000000000, 0.9659258262890683122, 1.000000000000000000, 0.9659258262890683122, 1.000000000000000000, 0.9923695281211504238, 0.9881565478350748943 ) ) 
 REPRESENTATION_ITEM ( '' )  );
#45787 = ORIENTED_EDGE ( 'NONE', *, *, #21581, .T. ) ;
#45788 = CARTESIAN_POINT ( 'NONE',  ( 19.84674366389459266, 8.300597817667451750, 2.638427012816836559 ) ) ;
#45789 = ORIENTED_EDGE ( 'NONE', *, *, #86386, .T. ) ;
#45790 = CARTESIAN_POINT ( 'NONE',  ( 10.00000000000000000, 25.55374883491396787, -14.16423886937410082 ) ) ;
#45791 = CARTESIAN_POINT ( 'NONE',  ( 10.00000000000000000, 19.75893115100078390, -9.846743663894594434 ) ) ;
#45792 = CARTESIAN_POINT ( 'NONE',  ( 19.42250999205614548, 25.98035201082150891, -5.440088680355545492 ) ) ;
#45793 = AXIS2_PLACEMENT_3D ( 'NONE', #70828, #2341, #92331 ) ;
#45794 = VERTEX_POINT ( 'NONE', #93330 ) ;
#45795 = CARTESIAN_POINT ( 'NONE',  ( 17.96484262340118221, 24.93868534415484461, 7.964842623401181321 ) ) ;
#45796 = VECTOR ( 'NONE', #39676, 1000.000000000000000 ) ;
#45797 = ORIENTED_EDGE ( 'NONE', *, *, #6438, .T. ) ;
#45798 = CARTESIAN_POINT ( 'NONE',  ( 15.44008868035555260, 34.73035201082151247, 9.422509992056143702 ) ) ;
#45799 = CARTESIAN_POINT ( 'NONE',  ( 20.15039907845753220, 46.74884699246888431, 6.262539305110077947 ) ) ;
#45800 = EDGE_LOOP ( 'NONE', ( #11148, #42369, #75239, #26909 ) ) ;
#45801 = EDGE_LOOP ( 'NONE', ( #44679, #98401, #12608, #34311 ) ) ;
#45802 = CARTESIAN_POINT ( 'NONE',  ( 21.09922568453595559, 22.04030133659708923, -6.408140936763230044 ) ) ;
#45803 = CARTESIAN_POINT ( 'NONE',  ( 1.472469842513823179, 15.59226448433411960, -4.923371831947296329 ) ) ;
#45804 = CYLINDRICAL_SURFACE ( 'NONE', #88105, 15.00000000000000000 ) ;
#45805 = CARTESIAN_POINT ( 'NONE',  ( 2.815433093577012880, 14.49999999999999112, 14.73340885523758281 ) ) ;
#45806 = CARTESIAN_POINT ( 'NONE',  ( 17.20831665107776587, 19.13393115100078035, -7.208316651077762316 ) ) ;
#45807 = CARTESIAN_POINT ( 'NONE',  ( 12.91533473730992121, 34.52201867748817676, 10.88017736071110164 ) ) ;
#45808 = MECHANICAL_DESIGN_GEOMETRIC_PRESENTATION_REPRESENTATION (  '', ( #79340 ), #13906 ) ;
#45809 = AXIS2_PLACEMENT_3D ( 'NONE', #25920, #47429, #32424 ) ;
#45810 = VECTOR ( 'NONE', #28542, 1000.000000000000114 ) ;
#45811 = ORIENTED_EDGE ( 'NONE', *, *, #50588, .F. ) ;
#45812 = AXIS2_PLACEMENT_3D ( 'NONE', #49509, #3549, #57016 ) ;
#45813 = PLANE ( 'NONE',  #8797 ) ;
#45814 = CARTESIAN_POINT ( 'NONE',  ( 17.96484262340118221, 59.93868534415484106, 7.964842623401181321 ) ) ;
#45815 = CARTESIAN_POINT ( 'NONE',  ( -46.48621475366246614, 103.4032225623660821, -6.318809327474250281 ) ) ;
#45816 = CARTESIAN_POINT ( 'NONE',  ( -2.816281873526473856, 54.33196800326376064, 3.434112377981055619 ) ) ;
#45817 = CARTESIAN_POINT ( 'NONE',  ( 12.91533473730992121, 64.52201867748817676, 10.88017736071110164 ) ) ;
#45818 = CARTESIAN_POINT ( 'NONE',  ( 6.565887622018943937, -1.918031996736246692, -12.81628187352647608 ) ) ;
#45819 = B_SPLINE_CURVE_WITH_KNOTS ( 'NONE', 3,
 ( #72056, #74019, #11554, #81034 ),
 .UNSPECIFIED., .F., .F.,
 ( 4, 4 ),
 ( 0.000000000000000000, 0.002392975128318533193 ),
 .UNSPECIFIED. ) ;
#45820 = DIRECTION ( 'NONE',  ( 0.000000000000000000, 0.000000000000000000, -1.000000000000000000 ) ) ;
#45821 = CARTESIAN_POINT ( 'NONE',  ( 10.00000000000000000, 29.75893115100078745, -9.846743663894594434 ) ) ;
#45822 = CARTESIAN_POINT ( 'NONE',  ( 22.81628187352648496, 56.83196800326374643, -3.434112377981050290 ) ) ;
#45823 = DIRECTION ( 'NONE',  ( -0.000000000000000000, -1.000000000000000000, -0.000000000000000000 ) ) ;
#45824 = CARTESIAN_POINT ( 'NONE',  ( 7.361572987183169658, 9.967264484334119601, -9.846743663894592657 ) ) ;
#45825 = CARTESIAN_POINT ( 'NONE',  ( 22.81628187352647785, 26.41530133659708923, 3.434112377981063169 ) ) ;
#45826 = CARTESIAN_POINT ( 'NONE',  ( 15.00000000000000000, 0.000000000000000000, -6.500000000000000888 ) ) ;
#45827 = CARTESIAN_POINT ( 'NONE',  ( 17.96484262340118221, 36.18868534415484106, -7.964842623401177768 ) ) ;
#45828 = CARTESIAN_POINT ( 'NONE',  ( 2.791683348922237240, 60.38393115100078745, -7.208316651077763204 ) ) ;
#45829 = CARTESIAN_POINT ( 'NONE',  ( 0.000000000000000000, 15.00000000000000000, 0.000000000000000000 ) ) ;
#45830 = EDGE_CURVE ( 'NONE', #86107, #69763, #40094, .T. ) ;
#45831 = CARTESIAN_POINT ( 'NONE',  ( 0.1532563361054082862, 21.21726448433412315, 2.638427012816831674 ) ) ;
#45832 = CARTESIAN_POINT ( 'NONE',  ( 7.361572987183170547, 7.050597817667451750, 9.846743663894590881 ) ) ;
#45833 = CARTESIAN_POINT ( 'NONE',  ( 17.96484262340118221, 9.938685344154837509, 7.964842623401181321 ) ) ;
#45835 = ORIENTED_EDGE ( 'NONE', *, *, #57984, .F. ) ;
#45834 = CARTESIAN_POINT ( 'NONE',  ( 0.6178305044545818747, 13.49863466993041783, -9.382169495545419124 ) ) ;
#45836 = VECTOR ( 'NONE', #80419, 1000.000000000000114 ) ;
#45837 =( LENGTH_UNIT ( ) NAMED_UNIT ( * ) SI_UNIT ( .MILLI., .METRE. ) );
#45838 = DIRECTION ( 'NONE',  ( -0.04361938736532633420, 0.000000000000000000, -0.9990482215818581313 ) ) ;
#45839 = CARTESIAN_POINT ( 'NONE',  ( 4.572805492040462383, -6.390838093309134216, -2.750000000000000000 ) ) ;
#45840 = CARTESIAN_POINT ( 'NONE',  ( 4.559911319644449179, 3.897018677488171434, 9.422509992056141925 ) ) ;
#45841 = CARTESIAN_POINT ( 'NONE',  ( 17.20831665107776587, 47.88393115100078745, 7.208316651077764980 ) ) ;
#45842 = CARTESIAN_POINT ( 'NONE',  ( -0.1503990784575242878, 49.24884699246889141, -6.262539305110083276 ) ) ;
#45843 = CARTESIAN_POINT ( 'NONE',  ( -4.164238869374099927, 67.01208216824728936, 3.795296366450308767 ) ) ;
#45844 = CARTESIAN_POINT ( 'NONE',  ( 19.72487221294570858, 64.78217586085237656, 6.499999999999992895 ) ) ;
#45845 = CARTESIAN_POINT ( 'NONE',  ( 2.035157376598822676, 32.43868534415483396, -7.964842623401177768 ) ) ;
#45847 = LINE ( 'NONE', #75840, #65446 ) ;
#45846 = CARTESIAN_POINT ( 'NONE',  ( 13.79529636645031943, 65.34541550158063217, -14.16423886937409904 ) ) ;
#45848 = CARTESIAN_POINT ( 'NONE',  ( 14.92337183194729633, 7.675597817667451750, 8.527530157486181039 ) ) ;
#45849 = CARTESIAN_POINT ( 'NONE',  ( 17.20831665107776587, 22.88393115100078745, 7.208316651077764980 ) ) ;
#45850 = CARTESIAN_POINT ( 'NONE',  ( 0.6178305044545838731, 14.74863466993041783, 9.382169495545420901 ) ) ;
#45851 = CARTESIAN_POINT ( 'NONE',  ( -0.1503990784575260087, 24.24884699246888786, -6.262539305110081500 ) ) ;
#45852 = CARTESIAN_POINT ( 'NONE',  ( -7.750000002551292511, -0.02148553728220452957, -4.000000000000000000 ) ) ;
#45853 = CARTESIAN_POINT ( 'NONE',  ( 2.917880565312948704, 7.637082168247301794, 12.26659068614894643 ) ) ;
#45854 = CARTESIAN_POINT ( 'NONE',  ( 2.791683348922240793, 31.63393115100078745, 7.208316651077764092 ) ) ;
#45855 = EDGE_CURVE ( 'NONE', #44471, #15375, #8849, .T. ) ;
#45856 = VERTEX_POINT ( 'NONE', #47824 ) ;
#45857 = CARTESIAN_POINT ( 'NONE',  ( -0.3689425029237881626, 47.42874883491396787, 10.36894250292379027 ) ) ;
#45858 = VECTOR ( 'NONE', #51726, 1000.000000000000114 ) ;
#45859 = CARTESIAN_POINT ( 'NONE',  ( 0.1532563361054082862, 11.21726448433411605, 2.638427012816831674 ) ) ;
#45861 = LINE ( 'NONE', #53852, #94975 ) ;
#45860 = CARTESIAN_POINT ( 'NONE',  ( 5.500000000000000000, 60.50000000000000000, 5.000000000000000000 ) ) ;
#45862 = CARTESIAN_POINT ( 'NONE',  ( 4.559911319644449179, 38.89701867748817676, 9.422509992056141925 ) ) ;
#45863 = CARTESIAN_POINT ( 'NONE',  ( 13.43411237798106583, 52.66530133659708213, -12.81628187352647252 ) ) ;
#45864 = EDGE_CURVE ( 'NONE', #70611, #63731, #95987, .T. ) ;
#45865 = CARTESIAN_POINT ( 'NONE',  ( -0.8801773607111009756, 13.06368534415483929, 1.068504757029289695E-15 ) ) ;
#45866 = CARTESIAN_POINT ( 'NONE',  ( 3.591859063236761518, 44.95696800326376064, 11.09922568453594849 ) ) ;
#45867 = CARTESIAN_POINT ( 'NONE',  ( 14.92337183194729633, 62.67559781766745886, 8.527530157486181039 ) ) ;
#45868 = FACE_OUTER_BOUND ( 'NONE', #89652, .T. ) ;
#45869 = ORIENTED_EDGE ( 'NONE', *, *, #53411, .T. ) ;
#45870 = FILL_AREA_STYLE_COLOUR ( '', #34065 ) ;
#45871 = CARTESIAN_POINT ( 'NONE',  ( -4.289191146912808207E-15, 8.868033628982656680, -11.25000000000000178 ) ) ;
#45872 = CARTESIAN_POINT ( 'NONE',  ( 13.79529636645031943, 45.34541550158062506, -14.16423886937409904 ) ) ;
#45873 = CARTESIAN_POINT ( 'NONE',  ( 6.204703633549690345, 20.76208216824730357, -14.16423886937410259 ) ) ;
#45874 =( NAMED_UNIT ( * ) SI_UNIT ( $, .STERADIAN. ) SOLID_ANGLE_UNIT ( ) );
#45875 = AXIS2_PLACEMENT_3D ( 'NONE', #83310, #69794, #54763 ) ;
#45876 = CARTESIAN_POINT ( 'NONE',  ( 19.42250999205614548, 35.98035201082151247, -5.440088680355545492 ) ) ;
#45877 = CARTESIAN_POINT ( 'NONE',  ( -14.99847009497950800, 14.49999999999999112, -0.2142307401082109986 ) ) ;
#45878 = CARTESIAN_POINT ( 'NONE',  ( 6.000000000000000000, 61.50000000000000711, 6.000000000000000000 ) ) ;
#45879 = CARTESIAN_POINT ( 'NONE',  ( 17.20831665107776587, 2.883931151000785231, 7.208316651077764980 ) ) ;
#45880 = CARTESIAN_POINT ( 'NONE',  ( 7.084665262690076126, 59.10535201082150536, 10.88017736071109987 ) ) ;
#45881 = CARTESIAN_POINT ( 'NONE',  ( 3.591859063236763294, 23.29030133659708568, -11.09922568453595026 ) ) ;
#45882 = CARTESIAN_POINT ( 'NONE',  ( 17.39651004071843232, 17.93575266056828355, 6.499999999999984013 ) ) ;
#45883 = CARTESIAN_POINT ( 'NONE',  ( -8.731067818237029599, 3.287123368507813836, 8.731067818237043809 ) ) ;
#45884 = CARTESIAN_POINT ( 'NONE',  ( 0.1532563361054083140, 31.00893115100078390, 1.131784320476157264E-15 ) ) ;
#45885 = AXIS2_PLACEMENT_3D ( 'NONE', #33455, #63952, #86963 ) ;
#45886 = CARTESIAN_POINT ( 'NONE',  ( 12.91533473730992121, 9.522018677488171434, 10.88017736071110164 ) ) ;
#45887 = AXIS2_PLACEMENT_3D ( 'NONE', #57803, #96822, #41366 ) ;
#45888 = CARTESIAN_POINT ( 'NONE',  ( 13.43411237798105340, 20.58196800326374643, 12.81628187352647963 ) ) ;
#45890 = EDGE_CURVE ( 'NONE', #8159, #31701, #17143, .T. ) ;
#45889 = CARTESIAN_POINT ( 'NONE',  ( 5.076628168052704559, 15.17559781766745175, -8.527530157486179263 ) ) ;
#45891 = CARTESIAN_POINT ( 'NONE',  ( 0.5774900079438607392, 8.480352010821505360, 5.440088680355550821 ) ) ;
#45892 = CARTESIAN_POINT ( 'NONE',  ( 19.84674366389459266, 43.30059781766744464, 2.638427012816836559 ) ) ;
#45893 = CARTESIAN_POINT ( 'NONE',  ( 16.40814093676323893, 55.79030133659708923, 11.09922568453595026 ) ) ;
#45895 = CARTESIAN_POINT ( 'NONE',  ( -2.266590686148945544, 2.220415501580634388, 7.082119434687048631 ) ) ;
#45894 = CARTESIAN_POINT ( 'NONE',  ( 2.791683348922237240, 15.38393115100078212, -7.208316651077763204 ) ) ;
#45896 = CARTESIAN_POINT ( 'NONE',  ( 22.26659068614894466, 8.887082168247300018, 7.082119434687054849 ) ) ;
#45897 = FACE_OUTER_BOUND ( 'NONE', #20194, .T. ) ;
#45898 = CARTESIAN_POINT ( 'NONE',  ( 7.084665262690076126, 32.02201867748816966, -10.88017736071110164 ) ) ;
#45900 = CARTESIAN_POINT ( 'NONE',  ( -4.164238869374098151, 41.59541550158061796, -3.795296366450310543 ) ) ;
#45899 = CARTESIAN_POINT ( 'NONE',  ( -0.8801773607111009756, 18.06368534415484106, 1.068504757029289695E-15 ) ) ;
#45901 = CARTESIAN_POINT ( 'NONE',  ( 15.44008868035555793, 36.39701867748816966, -9.422509992056140149 ) ) ;
#45902 = CARTESIAN_POINT ( 'NONE',  ( 19.42250999205614193, 15.14701867748817143, 5.440088680355555262 ) ) ;
#45903 = VERTEX_POINT ( 'NONE', #86330 ) ;
#45904 = CARTESIAN_POINT ( 'NONE',  ( 20.88017736071110164, 45.35535201082149115, 2.915334737309930979 ) ) ;
#45905 = CARTESIAN_POINT ( 'NONE',  ( 22.81628187352647785, 61.62363466993041783, 6.195893100308588602E-16 ) ) ;
#45906 = CARTESIAN_POINT ( 'NONE',  ( 20.88017736071110164, 50.35535201082151247, 2.915334737309930979 ) ) ;
#45907 = CARTESIAN_POINT ( 'NONE',  ( 10.00000000000000000, 56.81368534415484106, -10.88017736071110342 ) ) ;
#45908 = VERTEX_POINT ( 'NONE', #80792 ) ;
#45909 = CARTESIAN_POINT ( 'NONE',  ( 10.00000000000000178, 49.31368534415484106, 10.88017736071110342 ) ) ;
#45910 = CARTESIAN_POINT ( 'NONE',  ( 6.910361961229144256, -84.29457034759302303, 3.999999999998390177 ) ) ;
#45911 = CARTESIAN_POINT ( 'NONE',  ( -4.164238869374099039, 46.80374883491397497, 8.674139862899312516E-16 ) ) ;
#45912 = CARTESIAN_POINT ( 'NONE',  ( 15.44008868035555793, 66.39701867748817676, -9.422509992056140149 ) ) ;
#45913 = CARTESIAN_POINT ( 'NONE',  ( 0.2751277870542910842, 52.28217586085238366, -6.499999999999992006 ) ) ;
#45914 = CARTESIAN_POINT ( 'NONE',  ( -4.511864039100093926, -13.83704418182126972, -4.000000000000000888 ) ) ;
#45915 = CARTESIAN_POINT ( 'NONE',  ( 5.076628168052704559, 60.17559781766745175, -8.527530157486179263 ) ) ;
#45916 = SURFACE_SIDE_STYLE ('',( #91403 ) ) ;
#45917 = CARTESIAN_POINT ( 'NONE',  ( 1.472469842513823179, 31.42559781766745530, 4.923371831947296329 ) ) ;
#45918 = ORIENTED_EDGE ( 'NONE', *, *, #65518, .F. ) ;
#45919 = CARTESIAN_POINT ( 'NONE',  ( 5.076628168052703671, 31.84226448433412315, 8.527530157486179263 ) ) ;
#45920 = CARTESIAN_POINT ( 'NONE',  ( 11.09922568453594671, -7.959698663402909879, -6.408140936763241591 ) ) ;
#45921 = CARTESIAN_POINT ( 'NONE',  ( 20.88017736071110519, 35.56368534415484106, 2.639326808657452039E-16 ) ) ;
#45922 = CARTESIAN_POINT ( 'NONE',  ( 17.20831665107776587, 39.13393115100079456, -7.208316651077762316 ) ) ;
#45923 = CARTESIAN_POINT ( 'NONE',  ( 0.6178305044545818747, 23.49863466993041783, -9.382169495545419124 ) ) ;
#45925 = CARTESIAN_POINT ( 'NONE',  ( 12.91533473730993009, 56.60535201082151247, -10.88017736071109987 ) ) ;
#45924 = CARTESIAN_POINT ( 'NONE',  ( 10.00000000000000000, 66.81368534415484817, -10.88017736071110342 ) ) ;
#45927 = CARTESIAN_POINT ( 'NONE',  ( 19.42250999205614548, 5.980352010821504471, -5.440088680355545492 ) ) ;
#45926 = CARTESIAN_POINT ( 'NONE',  ( 0.5774900079438590739, 42.64701867748816966, -5.440088680355550821 ) ) ;
#45928 = CARTESIAN_POINT ( 'NONE',  ( -2.266590686148945544, 57.22041550158063217, 7.082119434687048631 ) ) ;
#45929 = CARTESIAN_POINT ( 'NONE',  ( -2.816281873526471635, 23.91530133659708568, -3.434112377981056508 ) ) ;
#45930 = DIRECTION ( 'NONE',  ( 1.257568779154408793E-17, 1.000000000000000000, -0.000000000000000000 ) ) ;
#45931 = ORIENTED_EDGE ( 'NONE', *, *, #58025, .F. ) ;
#45932 = CARTESIAN_POINT ( 'NONE',  ( -2.816281873526473856, 9.123634669930421381, 9.499525473075851096E-16 ) ) ;
#45933 = CARTESIAN_POINT ( 'NONE',  ( 0.5774900079438607392, 23.48035201082150536, 5.440088680355550821 ) ) ;
#45934 = CARTESIAN_POINT ( 'NONE',  ( 17.96484262340118221, 66.18868534415483396, -7.964842623401177768 ) ) ;
#45935 = ORIENTED_EDGE ( 'NONE', *, *, #98486, .T. ) ;
#45936 = AXIS2_PLACEMENT_3D ( 'NONE', #97698, #38170, #68657 ) ;
#45937 = B_SPLINE_CURVE_WITH_KNOTS ( 'NONE', 3,
 ( #90986, #83994, #6511, #37017, #52989, #76490 ),
 .UNSPECIFIED., .F., .F.,
 ( 4, 2, 4 ),
 ( 0.000000000000000000, 0.0002565770811490933789, 0.0005131541622981867579 ),
 .UNSPECIFIED. ) ;
#45938 = CARTESIAN_POINT ( 'NONE',  ( 12.91533473730993009, 61.60535201082150536, -10.88017736071109987 ) ) ;
#45939 = CARTESIAN_POINT ( 'NONE',  ( 7.361572987183169658, 49.96726448433410894, -9.846743663894592657 ) ) ;
#45940 = CARTESIAN_POINT ( 'NONE',  ( 1.472469842513823179, 26.42559781766745175, 4.923371831947296329 ) ) ;
#45941 = CARTESIAN_POINT ( 'NONE',  ( 14.92337183194729633, 27.67559781766745530, 8.527530157486181039 ) ) ;
#45942 = DIRECTION ( 'NONE',  ( 0.000000000000000000, 0.000000000000000000, 1.000000000000000000 ) ) ;
#45944 = CARTESIAN_POINT ( 'NONE',  ( 13.43411237798106583, 42.66530133659707502, -12.81628187352647252 ) ) ;
#45943 = DIRECTION ( 'NONE',  ( -0.000000000000000000, -0.000000000000000000, -1.000000000000000000 ) ) ;
#45945 = EDGE_CURVE ( 'NONE', #33986, #9878, #54528, .T. ) ;
#45947 = FACE_OUTER_BOUND ( 'NONE', #14689, .T. ) ;
#45946 = CARTESIAN_POINT ( 'NONE',  ( 10.00000000000000000, 14.75893115100078568, -9.846743663894594434 ) ) ;
#45948 = PLANE ( 'NONE',  #77693 ) ;
#45950 = ORIENTED_EDGE ( 'NONE', *, *, #93444, .T. ) ;
#45949 = CARTESIAN_POINT ( 'NONE',  ( 5.076628168052704559, 30.17559781766745175, -8.527530157486179263 ) ) ;
#45951 = CIRCLE ( 'NONE', #97075, 14.49999999999999822 ) ;
#45952 = B_SPLINE_CURVE_WITH_KNOTS ( 'NONE', 3,
 ( #94782, #27263, #57273, #88760, #42285, #48786, #19769, #27758, #34766, #88266, #79295, #4292, #33763, #26775, #41803, #87767, #64271, #49283, #73260, #26282, #56783, #86804 ),
 .UNSPECIFIED., .F., .F.,
 ( 4, 2, 2, 2, 2, 2, 2, 2, 2, 2, 4 ),
 ( 0.000000000000000000, 0.005577058028141766884, 0.01115411605628353377, 0.02230823211256706753, 0.04461646422513413507, 0.05577058028141766016, 0.06692469633770119219, 0.07807881239398470341, 0.08365587042212647984, 0.08644439943619736111, 0.08923292845026822850 ),
 .UNSPECIFIED. ) ;
#45953 = CARTESIAN_POINT ( 'NONE',  ( 11.24999999999999822, 2.559852905346091223, 0.8418318073276112035 ) ) ;
#45954 = CARTESIAN_POINT ( 'NONE',  ( 10.00000000000000000, 17.87363466993041783, -12.81628187352647608 ) ) ;
#45955 = CARTESIAN_POINT ( 'NONE',  ( 2.035157376598822676, 47.43868534415484817, -7.964842623401177768 ) ) ;
#45956 = CARTESIAN_POINT ( 'NONE',  ( -4.164238869374099039, 31.80374883491396432, 8.674139862899312516E-16 ) ) ;
#45957 = CARTESIAN_POINT ( 'NONE',  ( 1.383448333479218473, 42.37718327197428181, -6.499999999999959144 ) ) ;
#45958 = CARTESIAN_POINT ( 'NONE',  ( 17.08211943468705840, 25.13708216824730357, -12.26659068614894466 ) ) ;
#45959 = CARTESIAN_POINT ( 'NONE',  ( -4.164238869374099927, 57.01208216824731068, 3.795296366450308767 ) ) ;
#45960 = CARTESIAN_POINT ( 'NONE',  ( 17.08211943468705840, 15.13708216824730179, -12.26659068614894466 ) ) ;
#45962 = CARTESIAN_POINT ( 'NONE',  ( -13.51649600052862610, 90.98605788696677621, -7.975941444417872894 ) ) ;
#45961 = CARTESIAN_POINT ( 'NONE',  ( 13.79529636645031943, 30.34541550158063927, -14.16423886937409904 ) ) ;
#45963 = CARTESIAN_POINT ( 'NONE',  ( -0.8801773607110991993, 52.85535201082151247, -2.915334737309923874 ) ) ;
#45964 = CARTESIAN_POINT ( 'NONE',  ( 19.72487221294571214, 24.78217586085238011, 6.499999999999993783 ) ) ;
#45966 = CARTESIAN_POINT ( 'NONE',  ( 14.92337183194729633, 47.67559781766745175, 8.527530157486181039 ) ) ;
#45965 = CARTESIAN_POINT ( 'NONE',  ( 6.599999999999995204, -97.00000000000000000, -4.000000000000000000 ) ) ;
#45967 = CARTESIAN_POINT ( 'NONE',  ( 4.559911319644449179, 18.89701867748817321, 9.422509992056141925 ) ) ;
#45968 = CARTESIAN_POINT ( 'NONE',  ( 5.302565485995484273, 0.000000000000000000, 1.273033341818867736 ) ) ;
#45969 = CARTESIAN_POINT ( 'NONE',  ( 12.63842701281683034, 62.46726448433410894, 9.846743663894596210 ) ) ;
#45970 = CARTESIAN_POINT ( 'NONE',  ( 14.49154782522701446, 0.04962890019108410350, -2.766288502466956345 ) ) ;
#45971 = CARTESIAN_POINT ( 'NONE',  ( 17.20831665107776587, 22.88393115100078745, 7.208316651077764980 ) ) ;
#45972 = CARTESIAN_POINT ( 'NONE',  ( 10.00000000000000178, 55.37363466993042493, 12.81628187352647608 ) ) ;
#45973 = CARTESIAN_POINT ( 'NONE',  ( 14.16423886937410437, -0.9045844984193566196, 3.795296366450304770 ) ) ;
#45974 = CARTESIAN_POINT ( 'NONE',  ( 12.63842701281683034, 47.46726448433412315, 9.846743663894596210 ) ) ;
#45975 = CARTESIAN_POINT ( 'NONE',  ( 0.1532563361054100626, 55.80059781766745175, -2.638427012816831230 ) ) ;
#45976 = CARTESIAN_POINT ( 'NONE',  ( 17.08211943468705840, 40.13708216824731068, -12.26659068614894466 ) ) ;
#45977 = EDGE_CURVE ( 'NONE', #35759, #8190, #85131, .T. ) ;
#45978 = ORIENTED_EDGE ( 'NONE', *, *, #32736, .F. ) ;
#45979 = CARTESIAN_POINT ( 'NONE',  ( 20.36894250292379382, 8.678748834913967869, 10.36894250292379205 ) ) ;
#45980 = CARTESIAN_POINT ( 'NONE',  ( -0.8801773607110991993, 62.85535201082150536, -2.915334737309923874 ) ) ;
#45981 = CARTESIAN_POINT ( 'NONE',  ( 19.72487221294571214, 44.78217586085236945, 6.499999999999993783 ) ) ;
#45982 = CARTESIAN_POINT ( 'NONE',  ( 24.16423886937410614, 64.30374883491396076, 8.672049930838204340E-16 ) ) ;
#45983 = CARTESIAN_POINT ( 'NONE',  ( 22.81628187352647785, 16.41530133659708923, 3.434112377981063169 ) ) ;
#45984 = CARTESIAN_POINT ( 'NONE',  ( 12.80781515976310203, -0.03417435944610275333, 6.246788841744411513 ) ) ;
#45985 = CARTESIAN_POINT ( 'NONE',  ( 10.00000000000000178, 2.258931151000784787, 9.846743663894594434 ) ) ;
#45986 = CARTESIAN_POINT ( 'NONE',  ( -0.1049300847420639449, 27.21697413083879624, -6.336235997365760930 ) ) ;
#45987 = DIRECTION ( 'NONE',  ( 0.009903002720634835818, -0.9999509640662961329, 0.000000000000000000 ) ) ;
#45988 = CARTESIAN_POINT ( 'NONE',  ( -2.816281873526471635, 33.91530133659708213, -3.434112377981056508 ) ) ;
#45989 = CARTESIAN_POINT ( 'NONE',  ( -0.3689425029237881626, 62.42874883491396787, 10.36894250292379027 ) ) ;
#45990 = CARTESIAN_POINT ( 'NONE',  ( -14.88585913059880284, 0.2301501830257628445, -1.278057234794063302 ) ) ;
#45991 = CARTESIAN_POINT ( 'NONE',  ( 0.5774900079438590739, 17.64701867748817321, -5.440088680355550821 ) ) ;
#45992 = CARTESIAN_POINT ( 'NONE',  ( -0.8801773607111009756, 23.06368534415484106, 1.068504757029289695E-15 ) ) ;
#45993 = CARTESIAN_POINT ( 'NONE',  ( 18.52753015748618282, 53.92559781766745175, -4.923371831947291888 ) ) ;
#45994 = CARTESIAN_POINT ( 'NONE',  ( 2.791683348922237240, 60.38393115100078745, -7.208316651077763204 ) ) ;
#45995 = CARTESIAN_POINT ( 'NONE',  ( 13.43411237798106583, 52.66530133659708213, -12.81628187352647252 ) ) ;
#45996 = CARTESIAN_POINT ( 'NONE',  ( -1.820328553599931842, 0.000000000000000000, 5.140449258537799437 ) ) ;
#45997 = ORIENTED_EDGE ( 'NONE', *, *, #33913, .F. ) ;
#45998 = CARTESIAN_POINT ( 'NONE',  ( 4.559911319644449179, 17.23035201082150536, -9.422509992056141925 ) ) ;
#45999 = CARTESIAN_POINT ( 'NONE',  ( 6.565887622018943937, 15.16530133659708568, 12.81628187352647430 ) ) ;
#46000 = DIRECTION ( 'NONE',  ( -5.818595309480553908E-17, -1.000000000000000000, -0.000000000000000000 ) ) ;
#46001 = AXIS2_PLACEMENT_3D ( 'NONE', #42572, #48587, #26574 ) ;
#46002 = CARTESIAN_POINT ( 'NONE',  ( 7.361572987183169658, 44.96726448433412315, -9.846743663894592657 ) ) ;
#46003 = CARTESIAN_POINT ( 'NONE',  ( 20.88017736071110519, 55.56368534415484817, 2.639326808657452039E-16 ) ) ;
#46004 = CARTESIAN_POINT ( 'NONE',  ( 22.81628187352647785, 21.62363466993041783, 6.195893100308588602E-16 ) ) ;
#46006 = CARTESIAN_POINT ( 'NONE',  ( 18.72515096720568906, 15.05509018479935612, 6.500000000000002665 ) ) ;
#46005 = CARTESIAN_POINT ( 'NONE',  ( 7.084665262690076126, 54.10535201082151247, 10.88017736071109987 ) ) ;
#46007 = FACE_OUTER_BOUND ( 'NONE', #62250, .T. ) ;
#46008 = CARTESIAN_POINT ( 'NONE',  ( 22.81628187352648496, 56.83196800326374643, -3.434112377981050290 ) ) ;
#46009 = ORIENTED_EDGE ( 'NONE', *, *, #18553, .T. ) ;
#46010 = DIRECTION ( 'NONE',  ( -0.6225146366376129725, 0.000000000000000000, -0.7826081568524190235 ) ) ;
#46011 = CARTESIAN_POINT ( 'NONE',  ( -16.94999999999999574, 99.74999999999998579, -8.000000000000000000 ) ) ;
#46012 = CARTESIAN_POINT ( 'NONE',  ( 12.91533473730992121, 44.52201867748816966, 10.88017736071110164 ) ) ;
#46014 = CARTESIAN_POINT ( 'NONE',  ( -4.164238869374098151, 16.59541550158063927, -3.795296366450310543 ) ) ;
#46013 = CARTESIAN_POINT ( 'NONE',  ( -2.816281873526473856, 44.33196800326375353, 3.434112377981055619 ) ) ;
#46015 = MECHANICAL_DESIGN_GEOMETRIC_PRESENTATION_REPRESENTATION (  '', ( #47644 ), #41247 ) ;
#46016 = LINE ( 'NONE', #76505, #44996 ) ;
#46017 = CARTESIAN_POINT ( 'NONE',  ( 1.472469842513823179, 25.59226448433412315, -4.923371831947296329 ) ) ;
#46018 = EDGE_CURVE ( 'NONE', #92377, #35492, #41825, .T. ) ;
#46019 = CARTESIAN_POINT ( 'NONE',  ( 14.92337183194729633, 7.675597817667451750, 8.527530157486181039 ) ) ;
#46020 = CARTESIAN_POINT ( 'NONE',  ( 9.399392868737814766, 15.00000000000000000, -11.04089732309474314 ) ) ;
#46021 = CARTESIAN_POINT ( 'NONE',  ( -0.3689425029237881626, 42.42874883491396787, 10.36894250292379027 ) ) ;
#46022 = PRESENTATION_STYLE_ASSIGNMENT (( #54973 ) ) ;
#46023 = ADVANCED_FACE ( 'NONE', ( #64290 ), #32816, .F. ) ;
#46024 = CARTESIAN_POINT ( 'NONE',  ( 10.00000000000000178, 14.31368534415483751, 10.88017736071110342 ) ) ;
#46025 = CARTESIAN_POINT ( 'NONE',  ( -7.287642027973244119, -86.26866148728002770, -4.000000000000000000 ) ) ;
#46026 =( GEOMETRIC_REPRESENTATION_CONTEXT ( 3 ) GLOBAL_UNCERTAINTY_ASSIGNED_CONTEXT ( ( #70239 ) ) GLOBAL_UNIT_ASSIGNED_CONTEXT ( ( #33948, #25511, #86500 ) ) REPRESENTATION_CONTEXT ( 'NONE', 'WORKASPACE' ) );
#46027 = ORIENTED_EDGE ( 'NONE', *, *, #53329, .T. ) ;
#46028 = EDGE_LOOP ( 'NONE', ( #96540, #67862, #92125, #76439 ) ) ;
#46029 = CARTESIAN_POINT ( 'NONE',  ( 7.084665262690076126, 7.022018677488170546, -10.88017736071110164 ) ) ;
#46030 = CARTESIAN_POINT ( 'NONE',  ( 15.44008868035555260, 4.730352010821505360, 9.422509992056143702 ) ) ;
#46031 = CARTESIAN_POINT ( 'NONE',  ( 17.20831665107776587, 39.13393115100079456, -7.208316651077762316 ) ) ;
#46032 = CARTESIAN_POINT ( 'NONE',  ( 6.565887622018943937, 33.08196800326374643, -12.81628187352647608 ) ) ;
#46034 = CARTESIAN_POINT ( 'NONE',  ( 2.917880565312950480, 10.97041550158063572, -12.26659068614894821 ) ) ;
#46033 = CARTESIAN_POINT ( 'NONE',  ( 1.707155281725155849, 22.90189080397288635, 6.499999999999955591 ) ) ;
#46035 = CARTESIAN_POINT ( 'NONE',  ( 4.559911319644449179, 32.23035201082150536, -9.422509992056141925 ) ) ;
#46036 = CARTESIAN_POINT ( 'NONE',  ( 20.36894250292379382, 63.67874883491396787, 10.36894250292379205 ) ) ;
#46037 = CARTESIAN_POINT ( 'NONE',  ( 14.92337183194729633, 37.67559781766745175, 8.527530157486181039 ) ) ;
#46038 = CARTESIAN_POINT ( 'NONE',  ( 18.39792806157246119, 44.52224192338639597, 6.500000000000077272 ) ) ;
#46039 = CARTESIAN_POINT ( 'NONE',  ( 0.1532563361054083140, 21.00893115100078745, 1.131784320476157264E-15 ) ) ;
#46040 = B_SPLINE_CURVE_WITH_KNOTS ( 'NONE', 3,
 ( #98307, #52278, #22784, #37788, #98806, #67785, #82274, #68772, #30254, #29761, #83769, #44276, #304, #60269 ),
 .UNSPECIFIED., .F., .F.,
 ( 4, 2, 2, 2, 2, 2, 4 ),
 ( 0.000000000000000000, 0.004797171936611957510, 0.007195757904917936265, 0.009594343873223915020, 0.01199292984152989378, 0.01439151580983587253, 0.01918868774644783004 ),
 .UNSPECIFIED. ) ;
#46041 = CARTESIAN_POINT ( 'NONE',  ( 1.472469842513823179, 0.5922644843341181575, -4.923371831947296329 ) ) ;
#46042 = CARTESIAN_POINT ( 'NONE',  ( 9.846743663894594434, 28.50893115100078390, -2.168404344971008868E-15 ) ) ;
#46043 = VERTEX_POINT ( 'NONE', #95803 ) ;
#46044 = CARTESIAN_POINT ( 'NONE',  ( 11.62719953690064933, 14.49999999999999822, -9.476720473301794456 ) ) ;
#46045 = ORIENTED_EDGE ( 'NONE', *, *, #33966, .T. ) ;
#46046 = CARTESIAN_POINT ( 'NONE',  ( 0.1532563361054083140, 61.00893115100078745, 1.131784320476157264E-15 ) ) ;
#46048 = CARTESIAN_POINT ( 'NONE',  ( 20.88017736071110164, 40.35535201082150536, 2.915334737309930979 ) ) ;
#46047 = CARTESIAN_POINT ( 'NONE',  ( 20.88017736071110875, 30.77201867748816966, -2.915334737309920765 ) ) ;
#46049 = CARTESIAN_POINT ( 'NONE',  ( 22.81628187352648496, 31.83196800326375353, -3.434112377981050290 ) ) ;
#46050 = CARTESIAN_POINT ( 'NONE',  ( -0.3689425029237898834, 21.17874883491396432, -10.36894250292378850 ) ) ;
#46051 = CARTESIAN_POINT ( 'NONE',  ( 13.43411237798105340, 50.58196800326375353, 12.81628187352647963 ) ) ;
#46052 = VERTEX_POINT ( 'NONE', #57781 ) ;
#46053 = CARTESIAN_POINT ( 'NONE',  ( 5.076628168052703671, 46.84226448433412315, 8.527530157486179263 ) ) ;
#46054 = CARTESIAN_POINT ( 'NONE',  ( 12.91533473730993009, 16.60535201082150891, -10.88017736071109987 ) ) ;
#46055 = ORIENTED_EDGE ( 'NONE', *, *, #69387, .F. ) ;
#46056 = CARTESIAN_POINT ( 'NONE',  ( 17.96484262340118221, 19.93868534415484106, 7.964842623401181321 ) ) ;
#46057 = VERTEX_POINT ( 'NONE', #73281 ) ;
#46058 = CARTESIAN_POINT ( 'NONE',  ( 12.91533473730993009, 56.60535201082151247, -10.88017736071109987 ) ) ;
#46059 = CARTESIAN_POINT ( 'NONE',  ( -0.8801773607111009756, 63.06368534415484106, 1.068504757029289695E-15 ) ) ;
#46060 =( BOUNDED_CURVE ( )  B_SPLINE_CURVE ( 2, ( #56506, #46656, #1188, #701, #19003, #31647, #70163, #79987, #62137 ),
 .UNSPECIFIED., .F., .F. ) 
 B_SPLINE_CURVE_WITH_KNOTS ( ( 3, 2, 2, 2, 3 ),
 ( 0.01156950836880285202, 0.01190476190476197349, 0.01785714285714290472, 0.02380952380952383596, 0.02414477734548295743 ),
 .UNSPECIFIED. ) 
 CURVE ( )  GEOMETRIC_REPRESENTATION_ITEM ( )  RATIONAL_B_SPLINE_CURVE ( ( 0.9963778908391762723, 0.9980808541467921513, 1.000000000000000000, 0.9659258262890683122, 1.000000000000000000, 0.9659258262890683122, 1.000000000000000000, 0.9980808541467921513, 0.9963778908391762723 ) ) 
 REPRESENTATION_ITEM ( '' )  );
#46061 = CARTESIAN_POINT ( 'NONE',  ( -7.750000000000000000, 0.000000000000000000, 3.750000000000000000 ) ) ;
#46062 = CARTESIAN_POINT ( 'NONE',  ( -0.8801773607110991993, 47.85535201082150536, -2.915334737309923874 ) ) ;
#46063 = CARTESIAN_POINT ( 'NONE',  ( -0.1503990784575247319, 52.22266099184918176, -6.262539305110083276 ) ) ;
#46064 = EDGE_CURVE ( 'NONE', #44503, #41466, #87300, .T. ) ;
#46065 = CARTESIAN_POINT ( 'NONE',  ( -46.94000000000001194, 100.7103534007538883, 8.569772222592094479 ) ) ;
#46068 = ORIENTED_EDGE ( 'NONE', *, *, #98045, .T. ) ;
#46067 = PRESENTATION_LAYER_ASSIGNMENT (  '', '', ( #89159 ) ) ;
#46066 = DIRECTION ( 'NONE',  ( -1.000000000000000000, 0.000000000000000000, 0.000000000000000000 ) ) ;
#46069 = CARTESIAN_POINT ( 'NONE',  ( 19.84674366389459621, 38.50893115100078745, 7.409399052514197653E-17 ) ) ;
#46070 = ORIENTED_EDGE ( 'NONE', *, *, #19318, .T. ) ;
#46071 = FACE_OUTER_BOUND ( 'NONE', #1099, .T. ) ;
#46072 = SURFACE_STYLE_USAGE ( .BOTH. , #61550 ) ;
#46073 = CARTESIAN_POINT ( 'NONE',  ( 24.16423886937410614, 24.30374883491396787, 8.672049930838204340E-16 ) ) ;
#46074 = CARTESIAN_POINT ( 'NONE',  ( -49.20731707317072079, 39.36585365853652974, -8.000000000000000000 ) ) ;
#46075 = CARTESIAN_POINT ( 'NONE',  ( 19.72487221294570858, 70.00000000000000000, 6.000000000000000000 ) ) ;
#46076 = CARTESIAN_POINT ( 'NONE',  ( 7.084665262690076126, 14.10535201082150358, 10.88017736071109987 ) ) ;
#46078 = ORIENTED_EDGE ( 'NONE', *, *, #32851, .F. ) ;
#46077 = CARTESIAN_POINT ( 'NONE',  ( 10.00000000000000000, 37.87363466993041783, -12.81628187352647608 ) ) ;
#46079 = CARTESIAN_POINT ( 'NONE',  ( -11.64999999999999680, 98.49999999999998579, -8.000000000000000000 ) ) ;
#46080 = CARTESIAN_POINT ( 'NONE',  ( 17.20831665107776587, 2.883931151000785231, 7.208316651077764980 ) ) ;
#46081 = CARTESIAN_POINT ( 'NONE',  ( 13.43411237798105340, 25.58196800326374998, 12.81628187352647963 ) ) ;
#46082 = CARTESIAN_POINT ( 'NONE',  ( 10.00000000000000000, 19.75893115100078390, -9.846743663894594434 ) ) ;
#46083 = COLOUR_RGB ( '', 0.09019608, 0.27058824, 0.51372549) ;
#46084 = CARTESIAN_POINT ( 'NONE',  ( 19.72487221294570858, 0.000000000000000000, -6.500000000000000888 ) ) ;
#46085 = CARTESIAN_POINT ( 'NONE',  ( 10.00000000000000178, 17.25893115100078745, 9.846743663894594434 ) ) ;
#46086 = CARTESIAN_POINT ( 'NONE',  ( -2.816281873526471635, 13.91530133659708746, -3.434112377981056508 ) ) ;
#46087 = AXIS2_PLACEMENT_3D ( 'NONE', #28557, #74045, #45030 ) ;
#46088 = CARTESIAN_POINT ( 'NONE',  ( 8.879999999999991900, 27.04366094290857347, -2.958578643762691307 ) ) ;
#46089 = CARTESIAN_POINT ( 'NONE',  ( 1.472469842513823179, 1.425597817667451528, 4.923371831947296329 ) ) ;
#46090 = EDGE_CURVE ( 'NONE', #51581, #37077, #4024, .T. ) ;
#46091 = VERTEX_POINT ( 'NONE', #33784 ) ;
#46092 = VERTEX_POINT ( 'NONE', #94802 ) ;
#46093 = CARTESIAN_POINT ( 'NONE',  ( 4.559911319644449179, 27.23035201082150536, -9.422509992056141925 ) ) ;
#46094 = CARTESIAN_POINT ( 'NONE',  ( 20.36894250292379382, 23.67874883491397142, 10.36894250292379205 ) ) ;
#46095 = CARTESIAN_POINT ( 'NONE',  ( 14.92337183194729633, 47.67559781766745175, 8.527530157486181039 ) ) ;
#46096 = CARTESIAN_POINT ( 'NONE',  ( 10.00000000000000000, 66.81368534415484817, -10.88017736071110342 ) ) ;
#46098 = CARTESIAN_POINT ( 'NONE',  ( -6.982525766139714207, -88.11956320875633253, -2.750000000000000444 ) ) ;
#46097 = CARTESIAN_POINT ( 'NONE',  ( -1.099225684535947600, 34.54030133659708923, 6.408140936763237150 ) ) ;
#46099 = CARTESIAN_POINT ( 'NONE',  ( 0.5774900079438607392, 8.480352010821505360, 5.440088680355550821 ) ) ;
#46100 = ADVANCED_FACE ( 'NONE', ( #56804 ), #38458, .F. ) ;
#46101 = CARTESIAN_POINT ( 'NONE',  ( -14.35840480524197815, 0.3639308199838639513, -4.340070442839035536 ) ) ;
#46102 = CARTESIAN_POINT ( 'NONE',  ( 19.38216949554541202, 10.99863466993042138, 9.382169495545424454 ) ) ;
#46103 = VECTOR ( 'NONE', #47723, 1000.000000000000000 ) ;
#46104 = CARTESIAN_POINT ( 'NONE',  ( 0.6178305044545838731, 4.748634669930420493, 9.382169495545420901 ) ) ;
#46105 = CARTESIAN_POINT ( 'NONE',  ( 10.00000000000000178, 27.25893115100078390, 9.846743663894594434 ) ) ;
#46106 = CARTESIAN_POINT ( 'NONE',  ( -5.440088680355558814, -17.76964798917849109, -9.422509992056136596 ) ) ;
#46107 = CARTESIAN_POINT ( 'NONE',  ( -2.816281873526471635, 28.91530133659708213, -3.434112377981056508 ) ) ;
#46108 = SURFACE_STYLE_FILL_AREA ( #22625 ) ;
#46110 = CARTESIAN_POINT ( 'NONE',  ( 1.274849032794292736, 62.55509018479936145, -6.499999999999977796 ) ) ;
#46109 = CARTESIAN_POINT ( 'NONE',  ( 15.44008868035555793, 51.39701867748816966, -9.422509992056140149 ) ) ;
#46111 = DIRECTION ( 'NONE',  ( 0.8788171126619711560, 0.000000000000000000, -0.4771587602595978028 ) ) ;
#46112 = CARTESIAN_POINT ( 'NONE',  ( 0.5774900079438607392, 68.48035201082150536, 5.440088680355550821 ) ) ;
#46113 = CARTESIAN_POINT ( 'NONE',  ( -0.8801773607110991993, 42.85535201082150536, -2.915334737309923874 ) ) ;
#46114 = CARTESIAN_POINT ( 'NONE',  ( 7.084665262690076126, 39.10535201082150536, 10.88017736071109987 ) ) ;
#46115 = LINE ( 'NONE', #21646, #58443 ) ;
#46116 = LINE ( 'NONE', #76603, #93895 ) ;
#46117 = CARTESIAN_POINT ( 'NONE',  ( 14.92337183194729633, 57.67559781766745886, 8.527530157486181039 ) ) ;
#46119 = DIRECTION ( 'NONE',  ( 0.1822355254921448620, 0.000000000000000000, 0.9832549075639551717 ) ) ;
#46118 = CARTESIAN_POINT ( 'NONE',  ( 20.88017736071110875, 5.772018677488170546, -2.915334737309920765 ) ) ;
#46120 = CARTESIAN_POINT ( 'NONE',  ( 21.09922568453595559, 7.040301336597086568, -6.408140936763230044 ) ) ;
#46121 = ORIENTED_EDGE ( 'NONE', *, *, #68033, .F. ) ;
#46122 = CARTESIAN_POINT ( 'NONE',  ( 7.084665262690076126, 42.02201867748816966, -10.88017736071110164 ) ) ;
#46124 = DIRECTION ( 'NONE',  ( 0.9969173337331278528, 0.000000000000000000, 0.07845909572784538766 ) ) ;
#46123 = CARTESIAN_POINT ( 'NONE',  ( 12.63842701281683034, 62.46726448433410894, 9.846743663894596210 ) ) ;
#46125 = CARTESIAN_POINT ( 'NONE',  ( 20.88017736071110875, 10.77201867748817143, -2.915334737309920765 ) ) ;
#46126 = CARTESIAN_POINT ( 'NONE',  ( -0.8801773607110991993, 32.85535201082151247, -2.915334737309923874 ) ) ;
#46127 = CARTESIAN_POINT ( 'NONE',  ( 2.917880565312948704, 42.63708216824729647, 12.26659068614894643 ) ) ;
#46128 = CARTESIAN_POINT ( 'NONE',  ( 18.52753015748617571, 33.09226448433411605, 4.923371831947298993 ) ) ;
#46129 = CARTESIAN_POINT ( 'NONE',  ( -0.8801773607110991993, 52.85535201082151247, -2.915334737309923874 ) ) ;
#46130 = CARTESIAN_POINT ( 'NONE',  ( -18.89999999999999147, 99.74999999999998579, 8.000000000000000000 ) ) ;
#46131 = SURFACE_STYLE_USAGE ( .BOTH. , #98672 ) ;
#46132 = ADVANCED_FACE ( 'NONE', ( #79803 ), #52263, .F. ) ;
#46133 = CARTESIAN_POINT ( 'NONE',  ( 5.817157072110800797, 0.5000000000000004441, -13.82608706751086558 ) ) ;
#46134 = CARTESIAN_POINT ( 'NONE',  ( 0.1532563361054082862, 61.21726448433412315, 2.638427012816831674 ) ) ;
#46135 = ORIENTED_EDGE ( 'NONE', *, *, #81136, .F. ) ;
#46136 = ORIENTED_EDGE ( 'NONE', *, *, #32334, .F. ) ;
#46137 = CARTESIAN_POINT ( 'NONE',  ( 13.79529636645031943, 35.34541550158063927, -14.16423886937409904 ) ) ;
#46138 = CARTESIAN_POINT ( 'NONE',  ( -0.3689425029237881626, 27.42874883491397142, 10.36894250292379027 ) ) ;
#46139 = CARTESIAN_POINT ( 'NONE',  ( 17.20831665107776587, 4.133931151000785675, -7.208316651077762316 ) ) ;
#46140 = CARTESIAN_POINT ( 'NONE',  ( 13.43411237798105340, 10.58196800326375353, 12.81628187352647963 ) ) ;
#46141 = DIRECTION ( 'NONE',  ( -1.509903313490212895E-14, 0.000000000000000000, 1.000000000000000000 ) ) ;
#46142 = CARTESIAN_POINT ( 'NONE',  ( -11.33063469435185233, -84.07074358190932628, 4.000000000000000000 ) ) ;
#46144 = CARTESIAN_POINT ( 'NONE',  ( 3.591859063236763294, 23.29030133659708568, -11.09922568453595026 ) ) ;
#46143 = CARTESIAN_POINT ( 'NONE',  ( 20.88017736071110519, 60.56368534415484106, 2.639326808657452039E-16 ) ) ;
#46145 = CARTESIAN_POINT ( 'NONE',  ( 22.26659068614895176, 24.72041550158063572, -7.082119434687042414 ) ) ;
#46146 = CARTESIAN_POINT ( 'NONE',  ( 20.88017736071110519, 10.56368534415483929, 2.639326808657452039E-16 ) ) ;
#46147 = CARTESIAN_POINT ( 'NONE',  ( -0.8801773607111008646, 33.27201867748817676, 2.915334737309923430 ) ) ;
#46148 = LINE ( 'NONE', #23663, #36373 ) ;
#46149 = CARTESIAN_POINT ( 'NONE',  ( 20.88017736071110519, 50.56368534415484106, 2.639326808657452039E-16 ) ) ;
#46150 = EDGE_CURVE ( 'NONE', #26347, #43655, #2700, .T. ) ;
#46151 = VECTOR ( 'NONE', #49661, 1000.000000000000000 ) ;
#46152 = CARTESIAN_POINT ( 'NONE',  ( 19.38216949554541557, 52.24863466993041072, -9.382169495545420901 ) ) ;
#46153 = CARTESIAN_POINT ( 'NONE',  ( -7.208316651077756099, -28.36606884899921610, 7.208316651077766757 ) ) ;
#46154 = ORIENTED_EDGE ( 'NONE', *, *, #68670, .F. ) ;
#46155 = FACE_OUTER_BOUND ( 'NONE', #91772, .T. ) ;
#46156 = ORIENTED_EDGE ( 'NONE', *, *, #1307, .T. ) ;
#46157 = CARTESIAN_POINT ( 'NONE',  ( -3.750000000000000000, 36.75000000000000000, 2.750000000000000000 ) ) ;
#46158 = ORIENTED_EDGE ( 'NONE', *, *, #1387, .F. ) ;
#46159 = CARTESIAN_POINT ( 'NONE',  ( 0.000000000000000000, 15.00000000000000000, 0.000000000000000000 ) ) ;
#46161 = CARTESIAN_POINT ( 'NONE',  ( 22.26659068614894466, 63.88708216824730357, 7.082119434687054849 ) ) ;
#46160 = CARTESIAN_POINT ( 'NONE',  ( 2.917880565312948704, 57.63708216824731068, 12.26659068614894643 ) ) ;
#46163 = CARTESIAN_POINT ( 'NONE',  ( 12.63842701281683922, 59.55059781766744464, -9.846743663894590881 ) ) ;
#46162 = CARTESIAN_POINT ( 'NONE',  ( 17.20831665107776587, 29.13393115100078390, -7.208316651077762316 ) ) ;
#46164 = STYLED_ITEM ( 'NONE', ( #96589 ), #60234 ) ;
#46166 = CARTESIAN_POINT ( 'NONE',  ( 7.361572987183169658, 9.967264484334119601, -9.846743663894592657 ) ) ;
#46165 = AXIS2_PLACEMENT_3D ( 'NONE', #63254, #10274, #1806 ) ;
#46167 = CARTESIAN_POINT ( 'NONE',  ( 10.00000000000000178, 0.3736346699304200492, 12.81628187352647608 ) ) ;
#46168 = CARTESIAN_POINT ( 'NONE',  ( 3.434112377981060948, 20.58196800326374643, 12.81628187352647430 ) ) ;
#46169 = VERTEX_POINT ( 'NONE', #67270 ) ;
#46170 = ADVANCED_FACE ( 'NONE', ( #59756 ), #71987, .T. ) ;
#46171 = CARTESIAN_POINT ( 'NONE',  ( -4.164238869374098151, 36.59541550158063217, -3.795296366450310543 ) ) ;
#46172 = CARTESIAN_POINT ( 'NONE',  ( 17.08211943468705130, 38.47041550158063217, 12.26659068614894998 ) ) ;
#46173 = ORIENTED_EDGE ( 'NONE', *, *, #77246, .F. ) ;
#46174 = CARTESIAN_POINT ( 'NONE',  ( 13.43411237798105340, 55.58196800326374643, 12.81628187352647963 ) ) ;
#46175 = CARTESIAN_POINT ( 'NONE',  ( 20.88017736071110875, 25.77201867748816966, -2.915334737309920765 ) ) ;
#46176 = CARTESIAN_POINT ( 'NONE',  ( 19.84674366389459621, 48.50893115100078745, 7.409399052514197653E-17 ) ) ;
#46177 = CARTESIAN_POINT ( 'NONE',  ( 15.44008868035555793, 21.39701867748817321, -9.422509992056140149 ) ) ;
#46178 = CARTESIAN_POINT ( 'NONE',  ( 5.076628168052704559, 50.17559781766745886, -8.527530157486179263 ) ) ;
#46179 = CARTESIAN_POINT ( 'NONE',  ( 17.20831665107776587, 47.88393115100078745, 7.208316651077764980 ) ) ;
#46180 = COLOUR_RGB ( '', 0.09019608, 0.27058824, 0.51372549) ;
#46181 = EDGE_CURVE ( 'NONE', #20106, #20819, #35279, .T. ) ;
#46183 = ORIENTED_EDGE ( 'NONE', *, *, #60667, .T. ) ;
#46182 = CARTESIAN_POINT ( 'NONE',  ( 18.00000000000001776, 4.625929269271493211E-15, 6.250000000000000000 ) ) ;
#46184 = CARTESIAN_POINT ( 'NONE',  ( 19.72487221294570858, 31.86607318730074567, 6.500000000000000888 ) ) ;
#46185 = CARTESIAN_POINT ( 'NONE',  ( 2.791683348922240793, 1.633931151000784565, 7.208316651077764092 ) ) ;
#46186 = LINE ( 'NONE', #37223, #24438 ) ;
#46187 = ORIENTED_EDGE ( 'NONE', *, *, #55600, .F. ) ;
#46188 = CARTESIAN_POINT ( 'NONE',  ( 8.880000001785997910, -0.01162444801712644513, 4.000000000009423573 ) ) ;
#46189 = CARTESIAN_POINT ( 'NONE',  ( 10.00000000000000000, 24.75893115100078745, -9.846743663894594434 ) ) ;
#46190 = EDGE_CURVE ( 'NONE', #32127, #83513, #72004, .T. ) ;
#46191 = CARTESIAN_POINT ( 'NONE',  ( 3.969999999999999751, 36.75000000000000000, -2.500000000000000000 ) ) ;
#46192 = CARTESIAN_POINT ( 'NONE',  ( 22.81628187352647785, 41.62363466993042493, 6.195893100308588602E-16 ) ) ;
#46193 = CYLINDRICAL_SURFACE ( 'NONE', #41958, 0.5000000000000004441 ) ;
#46194 = PLANE ( 'NONE',  #81049 ) ;
#46195 = ORIENTED_EDGE ( 'NONE', *, *, #11246, .F. ) ;
#46196 = CARTESIAN_POINT ( 'NONE',  ( 2.791683348922237240, 65.38393115100078035, -7.208316651077763204 ) ) ;
#46197 = CARTESIAN_POINT ( 'NONE',  ( 19.84674366389459266, 58.71726448433411605, -2.638427012816827677 ) ) ;
#46198 = CARTESIAN_POINT ( 'NONE',  ( 20.36894250292379738, 29.92874883491396432, -10.36894250292379027 ) ) ;
#46199 = CARTESIAN_POINT ( 'NONE',  ( 2.791683348922240793, 56.63393115100078035, 7.208316651077764092 ) ) ;
#46200 = CARTESIAN_POINT ( 'NONE',  ( -13.21236992757665973, -0.03417435944610275333, -5.338143956176898186 ) ) ;
#46201 = CARTESIAN_POINT ( 'NONE',  ( 7.361572987183170547, 7.050597817667451750, 9.846743663894590881 ) ) ;
#46202 = CARTESIAN_POINT ( 'NONE',  ( 0.6178305044545838731, 49.74863466993041072, 9.382169495545420901 ) ) ;
#46203 = CARTESIAN_POINT ( 'NONE',  ( 6.204703633549690345, 2.845415501580634388, 14.16423886937410082 ) ) ;
#46204 = CARTESIAN_POINT ( 'NONE',  ( 0.1532563361054082862, 51.21726448433412315, 2.638427012816831674 ) ) ;
#46205 = CARTESIAN_POINT ( 'NONE',  ( 10.00000000000000178, 54.31368534415484106, 10.88017736071110342 ) ) ;
#46206 = DIRECTION ( 'NONE',  ( -0.000000000000000000, -0.000000000000000000, -1.000000000000000000 ) ) ;
#46207 = EDGE_CURVE ( 'NONE', #73080, #48374, #54421, .T. ) ;
#46208 = VERTEX_POINT ( 'NONE', #14782 ) ;
#46209 = CARTESIAN_POINT ( 'NONE',  ( -1.780824192092292924, 15.00000000000000000, -14.89391369643515795 ) ) ;
#46210 = CARTESIAN_POINT ( 'NONE',  ( 7.084665262690076126, 32.02201867748816966, -10.88017736071110164 ) ) ;
#46212 = CARTESIAN_POINT ( 'NONE',  ( 7.084665262690076126, 54.10535201082151247, 10.88017736071109987 ) ) ;
#46211 = CARTESIAN_POINT ( 'NONE',  ( -1.099225684535947600, -0.4596986634029132657, 6.408140936763237150 ) ) ;
#46213 = EDGE_CURVE ( 'NONE', #24676, #8841, #4804, .T. ) ;
#46214 = B_SPLINE_CURVE_WITH_KNOTS ( 'NONE', 3,
 ( #47314, #93809, #77814, #25339, #66759, #50262 ),
 .UNSPECIFIED., .F., .F.,
 ( 4, 2, 4 ),
 ( 3.409110551494646689E-05, 0.0004400426677367928058, 0.0008459942299586391311 ),
 .UNSPECIFIED. ) ;
#46215 = CARTESIAN_POINT ( 'NONE',  ( 0.000000000000000000, 14.49999999999999822, 0.000000000000000000 ) ) ;
#46216 = CARTESIAN_POINT ( 'NONE',  ( -46.48608351833326680, 103.4078159519480806, -6.315430899466240255 ) ) ;
#46218 = DIRECTION ( 'NONE',  ( -1.000000000000000000, 2.081668171172167567E-14, 0.000000000000000000 ) ) ;
#46217 = CARTESIAN_POINT ( 'NONE',  ( -0.8801773607110991993, 37.85535201082151247, -2.915334737309923874 ) ) ;
#46219 = CARTESIAN_POINT ( 'NONE',  ( 19.84674366389459266, 13.30059781766745353, 2.638427012816836559 ) ) ;
#46220 = CARTESIAN_POINT ( 'NONE',  ( 0.1532563361054100626, 40.80059781766745886, -2.638427012816831230 ) ) ;
#46221 = CYLINDRICAL_SURFACE ( 'NONE', #79245, 0.5000000000000004441 ) ;
#46222 = CARTESIAN_POINT ( 'NONE',  ( 12.26659068614894466, 19.72041550158062861, -7.082119434687053960 ) ) ;
#46223 = CARTESIAN_POINT ( 'NONE',  ( 10.00000000000000000, 64.75893115100078035, -9.846743663894594434 ) ) ;
#46225 = SURFACE_STYLE_USAGE ( .BOTH. , #62185 ) ;
#46224 = CARTESIAN_POINT ( 'NONE',  ( 2.035157376598822676, 12.43868534415483751, -7.964842623401177768 ) ) ;
#46226 = DIRECTION ( 'NONE',  ( -0.5905099943842175847, -0.8070303256584298035, 0.000000000000000000 ) ) ;
#46227 = CARTESIAN_POINT ( 'NONE',  ( 20.36894250292379382, 28.67874883491396787, 10.36894250292379205 ) ) ;
#46228 = CARTESIAN_POINT ( 'NONE',  ( 24.16423886937409904, 49.09541550158063217, 3.795296366450317205 ) ) ;
#46229 = CARTESIAN_POINT ( 'NONE',  ( 19.84674366389459266, 33.71726448433410894, -2.638427012816827677 ) ) ;
#46230 = CARTESIAN_POINT ( 'NONE',  ( 0.1532563361054100626, 20.80059781766744464, -2.638427012816831230 ) ) ;
#46231 = CARTESIAN_POINT ( 'NONE',  ( 17.96484262340118221, 6.188685344154836621, -7.964842623401177768 ) ) ;
#46232 = ORIENTED_EDGE ( 'NONE', *, *, #5791, .T. ) ;
#46233 = CARTESIAN_POINT ( 'NONE',  ( 0.1532563361054082862, 31.21726448433412315, 2.638427012816831674 ) ) ;
#46234 = CARTESIAN_POINT ( 'NONE',  ( 10.00000000000000178, 24.31368534415484106, 10.88017736071110342 ) ) ;
#46235 = CARTESIAN_POINT ( 'NONE',  ( 0.1532563361054083140, 61.00893115100078745, 1.131784320476157264E-15 ) ) ;
#46236 = CARTESIAN_POINT ( 'NONE',  ( 20.36894250292379738, 4.928748834913967869, -10.36894250292379027 ) ) ;
#46237 = DIRECTION ( 'NONE',  ( -1.257568779154408793E-17, -1.000000000000000000, 0.000000000000000000 ) ) ;
#46238 = CARTESIAN_POINT ( 'NONE',  ( 7.361572987183170547, 7.050597817667451750, 9.846743663894590881 ) ) ;
#46239 = CARTESIAN_POINT ( 'NONE',  ( 10.00000000000000000, 42.87363466993042493, -12.81628187352647608 ) ) ;
#46240 = CARTESIAN_POINT ( 'NONE',  ( 5.076628168052703671, 36.84226448433412315, 8.527530157486179263 ) ) ;
#46241 = ORIENTED_EDGE ( 'NONE', *, *, #79926, .T. ) ;
#46242 = CARTESIAN_POINT ( 'NONE',  ( 12.63842701281683922, 24.55059781766745175, -9.846743663894590881 ) ) ;
#46243 = CARTESIAN_POINT ( 'NONE',  ( 11.18665108219126125, -81.61837458707562121, -4.000000000000000000 ) ) ;
#46244 = CARTESIAN_POINT ( 'NONE',  ( -46.61731745958343254, 101.4415013874591835, -8.301784926884796079 ) ) ;
#46245 = AXIS2_PLACEMENT_3D ( 'NONE', #43878, #89881, #50400 ) ;
#46246 = CARTESIAN_POINT ( 'NONE',  ( 6.204703633549690345, 52.84541550158062506, 14.16423886937410082 ) ) ;
#46247 = CARTESIAN_POINT ( 'NONE',  ( 0.5774900079438607392, 53.48035201082151247, 5.440088680355550821 ) ) ;
#46248 =( NAMED_UNIT ( * ) PLANE_ANGLE_UNIT ( ) SI_UNIT ( $, .RADIAN. ) );
#46249 = CARTESIAN_POINT ( 'NONE',  ( 0.1532563361054082862, 41.21726448433411605, 2.638427012816831674 ) ) ;
#46250 = CARTESIAN_POINT ( 'NONE',  ( 7.084665262690076126, 4.105352010821503583, 10.88017736071109987 ) ) ;
#46251 =( NAMED_UNIT ( * ) SI_UNIT ( $, .STERADIAN. ) SOLID_ANGLE_UNIT ( ) );
#46252 = CARTESIAN_POINT ( 'NONE',  ( 0.1532563361054100626, 45.80059781766745886, -2.638427012816831230 ) ) ;
#46253 = AXIS2_PLACEMENT_3D ( 'NONE', #94937, #55480, #2987 ) ;
#46254 = CARTESIAN_POINT ( 'NONE',  ( -0.8801773607111009756, 53.06368534415484106, 1.068504757029289695E-15 ) ) ;
#46255 = EDGE_CURVE ( 'NONE', #97016, #91796, #98256, .T. ) ;
#46256 = CARTESIAN_POINT ( 'NONE',  ( 10.00000000000000000, -0.2410688489992152128, -9.846743663894594434 ) ) ;
#46257 = VERTEX_POINT ( 'NONE', #43276 ) ;
#46258 = ORIENTED_EDGE ( 'NONE', *, *, #39088, .F. ) ;
#46259 = DIRECTION ( 'NONE',  ( 0.000000000000000000, -1.000000000000000000, 0.000000000000000000 ) ) ;
#46260 = DIRECTION ( 'NONE',  ( -1.000000000000000000, 0.000000000000000000, 0.000000000000000000 ) ) ;
#46261 = CARTESIAN_POINT ( 'NONE',  ( 0.1532563361054100626, 10.80059781766745175, -2.638427012816831230 ) ) ;
#46262 = CARTESIAN_POINT ( 'NONE',  ( -1.099225684535947600, 54.54030133659708923, 6.408140936763237150 ) ) ;
#46264 = CARTESIAN_POINT ( 'NONE',  ( 14.92337183194729633, 42.67559781766745886, 8.527530157486181039 ) ) ;
#46263 = CARTESIAN_POINT ( 'NONE',  ( 17.96484262340118221, 9.938685344154839285, 7.964842623401181321 ) ) ;
#46265 = DIRECTION ( 'NONE',  ( 0.000000000000000000, 0.000000000000000000, 1.000000000000000000 ) ) ;
#46266 = CARTESIAN_POINT ( 'NONE',  ( -4.164238869374099927, 27.01208216824730357, 3.795296366450308767 ) ) ;
#46267 = CARTESIAN_POINT ( 'NONE',  ( 13.79529636645030344, 63.26208216824730357, 14.16423886937410614 ) ) ;
#46268 = CARTESIAN_POINT ( 'NONE',  ( 12.63842701281683034, 62.46726448433410894, 9.846743663894596210 ) ) ;
#46269 = CARTESIAN_POINT ( 'NONE',  ( -11.62112565934141983, 15.00000000000000888, -8.881879596174913516 ) ) ;
#46270 = CARTESIAN_POINT ( 'NONE',  ( 7.084665262690076126, 57.02201867748817676, -10.88017736071110164 ) ) ;
#46271 = CARTESIAN_POINT ( 'NONE',  ( 18.52753015748618282, 3.925597817667451306, -4.923371831947291888 ) ) ;
#46272 = CARTESIAN_POINT ( 'NONE',  ( -3.522141228719769757, -0.8488377518989214110, 4.000000000000402345 ) ) ;
#46273 = ORIENTED_EDGE ( 'NONE', *, *, #61415, .F. ) ;
#46274 = LINE ( 'NONE', #39275, #21965 ) ;
#46275 = ORIENTED_EDGE ( 'NONE', *, *, #87293, .T. ) ;
#46276 = CARTESIAN_POINT ( 'NONE',  ( 12.63842701281683034, 7.467264484334118713, 9.846743663894596210 ) ) ;
#46277 = ORIENTED_EDGE ( 'NONE', *, *, #81288, .F. ) ;
#46278 = CARTESIAN_POINT ( 'NONE',  ( 22.26659068614894466, 18.88708216824730002, 7.082119434687054849 ) ) ;
#46279 = CARTESIAN_POINT ( 'NONE',  ( 12.63842701281683034, 22.46726448433411605, 9.846743663894596210 ) ) ;
#46280 = CARTESIAN_POINT ( 'NONE',  ( 19.42250999205614548, 35.98035201082151247, -5.440088680355545492 ) ) ;
#46281 =( NAMED_UNIT ( * ) PLANE_ANGLE_UNIT ( ) SI_UNIT ( $, .RADIAN. ) );
#46282 = EDGE_LOOP ( 'NONE', ( #78089, #87469, #10503, #17174 ) ) ;
#46283 = CARTESIAN_POINT ( 'NONE',  ( 0.5774900079438590739, 32.64701867748816966, -5.440088680355550821 ) ) ;
#46284 = VERTEX_POINT ( 'NONE', #51277 ) ;
#46285 = CARTESIAN_POINT ( 'NONE',  ( 15.44008868035555793, 31.39701867748817676, -9.422509992056140149 ) ) ;
#46286 = FACE_OUTER_BOUND ( 'NONE', #76406, .T. ) ;
#46287 = ORIENTED_EDGE ( 'NONE', *, *, #33124, .T. ) ;
#46288 = CARTESIAN_POINT ( 'NONE',  ( 6.565887622018943937, 23.08196800326375708, -12.81628187352647608 ) ) ;
#46289 = CARTESIAN_POINT ( 'NONE',  ( 12.63842701281683034, 7.467264484334118713, 9.846743663894596210 ) ) ;
#46290 = DIRECTION ( 'NONE',  ( -1.000000000000000000, 0.000000000000000000, 0.000000000000000000 ) ) ;
#46291 = EDGE_CURVE ( 'NONE', #88480, #85215, #12883, .T. ) ;
#46292 = DIRECTION ( 'NONE',  ( 0.000000000000000000, 1.000000000000000000, 0.000000000000000000 ) ) ;
#46293 = CARTESIAN_POINT ( 'NONE',  ( 0.1532563361054083140, 11.00893115100078568, 1.131784320476157264E-15 ) ) ;
#46294 = CARTESIAN_POINT ( 'NONE',  ( 4.559911319644449179, 28.89701867748817321, 9.422509992056141925 ) ) ;
#46295 = ORIENTED_EDGE ( 'NONE', *, *, #81489, .T. ) ;
#46296 = ADVANCED_FACE ( 'NONE', ( #48068 ), #57631, .T. ) ;
#46297 = ORIENTED_EDGE ( 'NONE', *, *, #70514, .F. ) ;
#46298 = CARTESIAN_POINT ( 'NONE',  ( 12.26500600480481040, 44.99999999999999289, 0.000000000000000000 ) ) ;
#46299 = CARTESIAN_POINT ( 'NONE',  ( 20.88017736071110164, 55.35535201082149825, 2.915334737309930979 ) ) ;
#46300 = CARTESIAN_POINT ( 'NONE',  ( -46.59701958359876528, 103.7651961684614861, -6.068442458532165240 ) ) ;
#46301 = CARTESIAN_POINT ( 'NONE',  ( 22.81628187352647785, 61.62363466993041783, 6.195893100308588602E-16 ) ) ;
#46302 = CARTESIAN_POINT ( 'NONE',  ( 19.42250999205614548, 65.98035201082151957, -5.440088680355545492 ) ) ;
#46303 = EDGE_CURVE ( 'NONE', #40303, #46764, #17599, .T. ) ;
#46304 = CARTESIAN_POINT ( 'NONE',  ( 0.1532563361054100626, 65.80059781766745175, -2.638427012816831230 ) ) ;
#46305 = CARTESIAN_POINT ( 'NONE',  ( -29.94000000000001549, 92.00000000000000000, -10.09898361729590199 ) ) ;
#46306 = VECTOR ( 'NONE', #81278, 1000.000000000000000 ) ;
#46307 = CARTESIAN_POINT ( 'NONE',  ( 0.1532563361054082862, 31.21726448433412315, 2.638427012816831674 ) ) ;
#46308 = CARTESIAN_POINT ( 'NONE',  ( 6.565887622018943937, 53.08196800326374643, -12.81628187352647608 ) ) ;
#46309 = CARTESIAN_POINT ( 'NONE',  ( 5.076628168052704559, 25.17559781766745175, -8.527530157486179263 ) ) ;
#46310 = CARTESIAN_POINT ( 'NONE',  ( 10.00000000000000178, 20.37363466993042138, 12.81628187352647608 ) ) ;
#46312 = CARTESIAN_POINT ( 'NONE',  ( -3.771484078448132937, -6.414704524388527673, -2.750000000000000444 ) ) ;
#46311 = CARTESIAN_POINT ( 'NONE',  ( 50.81170089112749366, 69.44265788454083577, -8.000000000000000000 ) ) ;
#46313 = CARTESIAN_POINT ( 'NONE',  ( 7.084665262690076126, 34.10535201082151247, 10.88017736071109987 ) ) ;
#46314 = AXIS2_PLACEMENT_3D ( 'NONE', #61889, #1425, #31877 ) ;
#46315 = CARTESIAN_POINT ( 'NONE',  ( 14.92337183194729988, 64.34226448433412315, -8.527530157486177487 ) ) ;
#46316 = VECTOR ( 'NONE', #55731, 1000.000000000000114 ) ;
#46317 = CARTESIAN_POINT ( 'NONE',  ( 14.92337183194729988, 14.34226448433411782, -8.527530157486177487 ) ) ;
#46318 = CARTESIAN_POINT ( 'NONE',  ( 12.91533473730992121, 19.52201867748816611, 10.88017736071110164 ) ) ;
#46319 = CARTESIAN_POINT ( 'NONE',  ( -2.816281873526473856, 14.33196800326375531, 3.434112377981055619 ) ) ;
#46320 =( NAMED_UNIT ( * ) PLANE_ANGLE_UNIT ( ) SI_UNIT ( $, .RADIAN. ) );
#46321 = FILL_AREA_STYLE ('',( #54298 ) ) ;
#46322 = CARTESIAN_POINT ( 'NONE',  ( 2.791683348922240793, 66.63393115100079456, 7.208316651077764092 ) ) ;
#46323 = CARTESIAN_POINT ( 'NONE',  ( 4.919406150865614613, -13.80316667494924054, -2.749999999999999556 ) ) ;
#46324 = CARTESIAN_POINT ( 'NONE',  ( 7.084665262690076126, 24.10535201082150181, 10.88017736071109987 ) ) ;
#46325 = CARTESIAN_POINT ( 'NONE',  ( 2.791683348922240793, 41.63393115100078745, 7.208316651077764092 ) ) ;
#46326 = CARTESIAN_POINT ( 'NONE',  ( 20.88017736071110519, 20.56368534415484106, 2.639326808657452039E-16 ) ) ;
#46327 = DIRECTION ( 'NONE',  ( -0.8320502943378436100, 0.5547001962252291474, -0.000000000000000000 ) ) ;
#46328 = EDGE_CURVE ( 'NONE', #89237, #94114, #25111, .T. ) ;
#46329 = CARTESIAN_POINT ( 'NONE',  ( 0.5774900079438590739, 27.64701867748817676, -5.440088680355550821 ) ) ;
#46331 = DIRECTION ( 'NONE',  ( -0.000000000000000000, 1.000000000000000000, -0.000000000000000000 ) ) ;
#46330 = CARTESIAN_POINT ( 'NONE',  ( 4.559911319644449179, 2.230352010821504916, -9.422509992056141925 ) ) ;
#46332 = CARTESIAN_POINT ( 'NONE',  ( 0.1532563361054083140, 1.008931151000784787, 1.131784320476157264E-15 ) ) ;
#46333 = AXIS2_PLACEMENT_3D ( 'NONE', #15244, #60225, #23731 ) ;
#46334 = CARTESIAN_POINT ( 'NONE',  ( 1.472469842513823179, 20.59226448433411960, -4.923371831947296329 ) ) ;
#46335 = CARTESIAN_POINT ( 'NONE',  ( 19.38216949554541557, 12.24863466993041961, -9.382169495545420901 ) ) ;
#46336 = FACE_OUTER_BOUND ( 'NONE', #60330, .T. ) ;
#46337 = CARTESIAN_POINT ( 'NONE',  ( 0.000000000000000000, 0.5000000000000004441, 0.000000000000000000 ) ) ;
#46338 = CARTESIAN_POINT ( 'NONE',  ( -8.897294703381261272, -15.56348197610850725, -4.000000000000000000 ) ) ;
#46339 = CARTESIAN_POINT ( 'NONE',  ( -4.164238869374099039, 16.80374883491396787, 8.674139862899312516E-16 ) ) ;
#46340 = CARTESIAN_POINT ( 'NONE',  ( 19.84674366389459266, 43.71726448433410894, -2.638427012816827677 ) ) ;
#46341 = CARTESIAN_POINT ( 'NONE',  ( 64.56412365047462742, 13.99999999999999467, 9.500000000000000000 ) ) ;
#46342 = VERTEX_POINT ( 'NONE', #56573 ) ;
#46343 = CARTESIAN_POINT ( 'NONE',  ( -2.266590686148945544, 57.22041550158063217, 7.082119434687048631 ) ) ;
#46344 = CARTESIAN_POINT ( 'NONE',  ( 14.92337183194729633, 22.67559781766745175, 8.527530157486181039 ) ) ;
#46346 = CARTESIAN_POINT ( 'NONE',  ( -4.249999999999994671, 43.00000000000000711, -6.250000000000000000 ) ) ;
#46345 = LINE ( 'NONE', #53344, #21111 ) ;
#46347 = CARTESIAN_POINT ( 'NONE',  ( 20.88017736071110875, 50.77201867748817676, -2.915334737309920765 ) ) ;
#46348 = CARTESIAN_POINT ( 'NONE',  ( 10.00000000000000000, 52.87363466993041783, -12.81628187352647608 ) ) ;
#46349 = CARTESIAN_POINT ( 'NONE',  ( 19.42250999205614548, 20.98035201082150891, -5.440088680355545492 ) ) ;
#46350 = CARTESIAN_POINT ( 'NONE',  ( 19.38216949554541557, 42.24863466993041783, -9.382169495545420901 ) ) ;
#46351 = CARTESIAN_POINT ( 'NONE',  ( 16.40814093676324603, 2.456968003263753531, -11.09922568453594671 ) ) ;
#46352 = CARTESIAN_POINT ( 'NONE',  ( 18.52753015748617571, 3.092264484334118269, 4.923371831947298993 ) ) ;
#46353 = ORIENTED_EDGE ( 'NONE', *, *, #45855, .F. ) ;
#46354 = CARTESIAN_POINT ( 'NONE',  ( -2.863845842056022661, 14.95077488074853456, 14.47219703936410617 ) ) ;
#46355 = DIRECTION ( 'NONE',  ( 0.000000000000000000, 1.000000000000000000, 0.000000000000000000 ) ) ;
#46356 = CARTESIAN_POINT ( 'NONE',  ( 22.26659068614895176, 49.72041550158063927, -7.082119434687042414 ) ) ;
#46357 = CARTESIAN_POINT ( 'NONE',  ( -4.164238869374098151, 16.59541550158063927, -3.795296366450310543 ) ) ;
#46358 = CARTESIAN_POINT ( 'NONE',  ( 17.96484262340118221, 26.18868534415483396, -7.964842623401177768 ) ) ;
#46359 = CARTESIAN_POINT ( 'NONE',  ( 7.084665262690076126, 32.02201867748816966, -10.88017736071110164 ) ) ;
#46360 = PLANE ( 'NONE',  #67006 ) ;
#46361 = CARTESIAN_POINT ( 'NONE',  ( 15.33206046421389601, -0.03417435944610275333, 4.561284726668865197 ) ) ;
#46362 = CARTESIAN_POINT ( 'NONE',  ( 0.5774900079438607392, 68.48035201082150536, 5.440088680355550821 ) ) ;
#46363 = CARTESIAN_POINT ( 'NONE',  ( 2.035157376598824452, 68.68868534415484817, 7.964842623401179544 ) ) ;
#46364 = CARTESIAN_POINT ( 'NONE',  ( -1.099225684535947600, 24.54030133659708923, 6.408140936763237150 ) ) ;
#46365 = CARTESIAN_POINT ( 'NONE',  ( 18.61655166652077753, 19.87718327197428891, 6.499999999999971578 ) ) ;
#46366 = DIRECTION ( 'NONE',  ( 1.000000000000000000, 0.000000000000000000, 0.000000000000000000 ) ) ;
#46367 = CARTESIAN_POINT ( 'NONE',  ( 2.791683348922240793, 11.63393115100078568, 7.208316651077764092 ) ) ;
#46368 = CARTESIAN_POINT ( 'NONE',  ( 5.076628168052704559, 35.17559781766745175, -8.527530157486179263 ) ) ;
#46369 = CARTESIAN_POINT ( 'NONE',  ( 19.42250999205614193, 15.14701867748817143, 5.440088680355555262 ) ) ;
#46370 = AXIS2_PLACEMENT_3D ( 'NONE', #7145, #13650, #14661 ) ;
#46371 = CARTESIAN_POINT ( 'NONE',  ( 6.565887622018943937, 38.08196800326376064, -12.81628187352647608 ) ) ;
#46372 = CARTESIAN_POINT ( 'NONE',  ( 1.472469842513823179, 15.59226448433411960, -4.923371831947296329 ) ) ;
#46373 = CARTESIAN_POINT ( 'NONE',  ( 12.91533473730992121, 9.522018677488171434, 10.88017736071110164 ) ) ;
#46374 = CARTESIAN_POINT ( 'NONE',  ( 12.63842701281683922, 49.55059781766744464, -9.846743663894590881 ) ) ;
#46375 = CARTESIAN_POINT ( 'NONE',  ( 1.472469842513823179, 30.59226448433411960, -4.923371831947296329 ) ) ;
#46376 = CARTESIAN_POINT ( 'NONE',  ( 24.16423886937409904, 24.09541550158063927, 3.795296366450317205 ) ) ;
#46377 = VECTOR ( 'NONE', #37399, 1000.000000000000000 ) ;
#46378 = CARTESIAN_POINT ( 'NONE',  ( 10.00000000000000000, 26.81368534415484106, -10.88017736071110342 ) ) ;
#46379 = CARTESIAN_POINT ( 'NONE',  ( -0.8801773607111009756, 8.063685344154837509, 1.068504757029289695E-15 ) ) ;
#46380 = AXIS2_PLACEMENT_3D ( 'NONE', #53360, #83867, #29372 ) ;
#46381 = CARTESIAN_POINT ( 'NONE',  ( 20.88017736071110875, 25.77201867748816966, -2.915334737309920765 ) ) ;
#46382 = EDGE_CURVE ( 'NONE', #37612, #45159, #286, .T. ) ;
#46383 = CARTESIAN_POINT ( 'NONE',  ( 19.42250999205614193, 25.14701867748817321, 5.440088680355555262 ) ) ;
#46384 = ORIENTED_EDGE ( 'NONE', *, *, #56512, .F. ) ;
#46385 = AXIS2_PLACEMENT_3D ( 'NONE', #60182, #14207, #90678 ) ;
#46386 = CARTESIAN_POINT ( 'NONE',  ( 4.559911319644449179, 42.23035201082151247, -9.422509992056141925 ) ) ;
#46387 = ORIENTED_EDGE ( 'NONE', *, *, #26671, .T. ) ;
#46388 = ADVANCED_FACE ( 'NONE', ( #63565 ), #30521, .T. ) ;
#46389 = CARTESIAN_POINT ( 'NONE',  ( 10.00000000000000000, 57.87363466993042493, -12.81628187352647608 ) ) ;
#46390 = CARTESIAN_POINT ( 'NONE',  ( 7.084665262690076126, 42.02201867748816966, -10.88017736071110164 ) ) ;
#46391 = CARTESIAN_POINT ( 'NONE',  ( 10.00000000000000000, 46.81368534415484106, -10.88017736071110342 ) ) ;
#46392 = ORIENTED_EDGE ( 'NONE', *, *, #91320, .F. ) ;
#46393 = CARTESIAN_POINT ( 'NONE',  ( 10.00000000000000000, 56.81368534415484106, -10.88017736071110342 ) ) ;
#46394 = FACE_OUTER_BOUND ( 'NONE', #16558, .T. ) ;
#46395 = CARTESIAN_POINT ( 'NONE',  ( 3.969999999999999751, 10.00000000000000000, -3.750000000000000000 ) ) ;
#46396 = CARTESIAN_POINT ( 'NONE',  ( 10.00000000000000178, 58.05374883491397497, 14.16423886937410082 ) ) ;
#46397 = CARTESIAN_POINT ( 'NONE',  ( 7.084665262690076126, 62.02201867748816966, -10.88017736071110164 ) ) ;
#46398 = CARTESIAN_POINT ( 'NONE',  ( 20.88017736071110519, 55.56368534415484817, 2.639326808657452039E-16 ) ) ;
#46399 = DIRECTION ( 'NONE',  ( -0.000000000000000000, -1.000000000000000000, -0.000000000000000000 ) ) ;
#46400 = CARTESIAN_POINT ( 'NONE',  ( 7.361572987183170547, 32.05059781766745175, 9.846743663894590881 ) ) ;
#46401 = ORIENTED_EDGE ( 'NONE', *, *, #56714, .T. ) ;
#46402 = CARTESIAN_POINT ( 'NONE',  ( 14.92337183194729988, 34.34226448433411605, -8.527530157486177487 ) ) ;
#46403 = AXIS2_PLACEMENT_3D ( 'NONE', #23622, #84602, #16101 ) ;
#46404 = CARTESIAN_POINT ( 'NONE',  ( 19.42250999205614193, 40.14701867748817676, 5.440088680355555262 ) ) ;
#46405 = CARTESIAN_POINT ( 'NONE',  ( 19.84674366389459266, 38.30059781766745175, 2.638427012816836559 ) ) ;
#46406 = CARTESIAN_POINT ( 'NONE',  ( 16.40814093676324603, 17.45696800326375353, -11.09922568453594671 ) ) ;
#46408 = CARTESIAN_POINT ( 'NONE',  ( -0.8801773607111008646, 53.27201867748816966, 2.915334737309923430 ) ) ;
#46407 = CARTESIAN_POINT ( 'NONE',  ( 20.03447792253740189, 2.655141069906897133, -6.401564815979724266 ) ) ;
#46409 = CARTESIAN_POINT ( 'NONE',  ( 10.00000000000000178, 49.31368534415484106, 10.88017736071110342 ) ) ;
#46410 = CARTESIAN_POINT ( 'NONE',  ( 10.00000000000000000, 55.55374883491396787, -14.16423886937410082 ) ) ;
#46411 = ADVANCED_FACE ( 'NONE', ( #10578 ), #86416, .T. ) ;
#46412 = CIRCLE ( 'NONE', #28833, 0.2500000000000002220 ) ;
#46413 = CARTESIAN_POINT ( 'NONE',  ( 0.6178305044545838731, 24.74863466993042493, 9.382169495545420901 ) ) ;
#46414 = CARTESIAN_POINT ( 'NONE',  ( 1.959929470562282283, 51.50257860105348584, 5.767676674365853629 ) ) ;
#46415 = VERTEX_POINT ( 'NONE', #75750 ) ;
#46416 = CARTESIAN_POINT ( 'NONE',  ( 10.00000000000000178, 10.37363466993041961, 12.81628187352647608 ) ) ;
#46417 = CARTESIAN_POINT ( 'NONE',  ( 10.00000000000000000, 26.81368534415484106, -10.88017736071110342 ) ) ;
#46418 = EDGE_CURVE ( 'NONE', #38545, #6951, #7272, .T. ) ;
#46419 = CARTESIAN_POINT ( 'NONE',  ( 7.084665262690076126, 62.02201867748816966, -10.88017736071110164 ) ) ;
#46420 = ORIENTED_EDGE ( 'NONE', *, *, #19347, .F. ) ;
#46421 = CARTESIAN_POINT ( 'NONE',  ( 18.52753015748618282, 3.925597817667451306, -4.923371831947291888 ) ) ;
#46422 = CARTESIAN_POINT ( 'NONE',  ( 14.92337183194729988, 49.34226448433411605, -8.527530157486177487 ) ) ;
#46423 = CARTESIAN_POINT ( 'NONE',  ( 0.1532563361054082862, 31.21726448433412315, 2.638427012816831674 ) ) ;
#46424 = CARTESIAN_POINT ( 'NONE',  ( 1.472469842513823179, 25.59226448433412315, -4.923371831947296329 ) ) ;
#46425 = CARTESIAN_POINT ( 'NONE',  ( 14.69266224296806200, 14.95037104324574884, -1.335284760094769263 ) ) ;
#46426 = CARTESIAN_POINT ( 'NONE',  ( 20.15039907845753220, 25.60158574516642815, -6.262539305110077947 ) ) ;
#46428 = DIRECTION ( 'NONE',  ( 0.000000000000000000, 1.000000000000000000, 0.000000000000000000 ) ) ;
#46427 = CARTESIAN_POINT ( 'NONE',  ( 5.076628168052704559, 15.17559781766745175, -8.527530157486179263 ) ) ;
#46429 = CARTESIAN_POINT ( 'NONE',  ( -12.80781515976305762, 0.000000000000000000, -6.246788841744501219 ) ) ;
#46431 = ORIENTED_EDGE ( 'NONE', *, *, #21818, .F. ) ;
#46430 = CARTESIAN_POINT ( 'NONE',  ( 19.84674366389459621, 43.50893115100078745, 7.409399052514197653E-17 ) ) ;
#46432 =( BOUNDED_CURVE ( )  B_SPLINE_CURVE ( 2, ( #54658, #62651, #24679, #17184, #70177, #26144, #94137, #1693, #78658 ),
 .UNSPECIFIED., .F., .F. ) 
 B_SPLINE_CURVE_WITH_KNOTS ( ( 3, 2, 2, 2, 3 ),
 ( 0.7248575172211797479, 0.7261904761904761640, 0.7321428571428570953, 0.7380952380952381375, 0.7394281970645346647 ),
 .UNSPECIFIED. ) 
 CURVE ( )  GEOMETRIC_REPRESENTATION_ITEM ( )  RATIONAL_B_SPLINE_CURVE ( ( 0.9881565478350733400, 0.9923695281211490915, 1.000000000000000000, 0.9659258262890683122, 1.000000000000000000, 0.9659258262890683122, 1.000000000000000000, 0.9923695281211484254, 0.9881565478350726739 ) ) 
 REPRESENTATION_ITEM ( '' )  );
#46433 = CARTESIAN_POINT ( 'NONE',  ( 4.219999999999999751, 36.75000000000000000, -2.750000000000000000 ) ) ;
#46434 = CARTESIAN_POINT ( 'NONE',  ( 22.81628187352647785, 16.41530133659708923, 3.434112377981063169 ) ) ;
#46435 = ADVANCED_FACE ( 'NONE', ( #94073 ), #41088, .T. ) ;
#46436 = CARTESIAN_POINT ( 'NONE',  ( 0.5774900079438607392, 53.48035201082151247, 5.440088680355550821 ) ) ;
#46437 = CARTESIAN_POINT ( 'NONE',  ( 22.26659068614894466, 38.88708216824731068, 7.082119434687054849 ) ) ;
#46439 = SURFACE_STYLE_FILL_AREA ( #39444 ) ;
#46438 = AXIS2_PLACEMENT_3D ( 'NONE', #53867, #62330, #84854 ) ;
#46440 = CARTESIAN_POINT ( 'NONE',  ( 20.00000000000000711, 89.81725769049432984, 5.338627755225069826 ) ) ;
#46441 = CARTESIAN_POINT ( 'NONE',  ( 24.16423886937409904, 39.09541550158062506, 3.795296366450317205 ) ) ;
#46442 = EDGE_CURVE ( 'NONE', #1044, #22386, #27042, .T. ) ;
#46443 = CARTESIAN_POINT ( 'NONE',  ( 24.16423886937409904, 64.09541550158064638, 3.795296366450317205 ) ) ;
#46444 = CARTESIAN_POINT ( 'NONE',  ( -4.164238869374099927, 27.01208216824730357, 3.795296366450308767 ) ) ;
#46446 = CARTESIAN_POINT ( 'NONE',  ( 13.99999999999999822, 11.50000000000000000, 6.000000000000000000 ) ) ;
#46445 = CARTESIAN_POINT ( 'NONE',  ( 6.204703633549690345, 30.76208216824730357, -14.16423886937410259 ) ) ;
#46447 = CARTESIAN_POINT ( 'NONE',  ( 6.452519493965914954, -47.68837976023561964, -3.750000000000000888 ) ) ;
#46449 = CARTESIAN_POINT ( 'NONE',  ( 5.076628168052703671, 41.84226448433411605, 8.527530157486179263 ) ) ;
#46448 = CARTESIAN_POINT ( 'NONE',  ( -10.00000000000007105, 92.00000000000000000, 9.500000000000000000 ) ) ;
#46450 = LINE ( 'NONE', #38959, #89770 ) ;
#46451 = CARTESIAN_POINT ( 'NONE',  ( 2.897438467171757030E-16, 23.03999999999999915, 0.000000000000000000 ) ) ;
#46452 = CARTESIAN_POINT ( 'NONE',  ( 20.00000000000001066, 87.37138358833496454, -5.317662825072152266 ) ) ;
#46453 = CARTESIAN_POINT ( 'NONE',  ( 0.1532563361054083140, 46.00893115100079456, 1.131784320476157264E-15 ) ) ;
#46454 = CARTESIAN_POINT ( 'NONE',  ( 0.6178305044545838731, 54.74863466993042493, 9.382169495545420901 ) ) ;
#46455 = CARTESIAN_POINT ( 'NONE',  ( -14.16423886937410437, -8.404584498419364280, -3.795296366450299885 ) ) ;
#46456 = CARTESIAN_POINT ( 'NONE',  ( 2.791683348922240793, 36.63393115100078035, 7.208316651077764092 ) ) ;
#46457 = CARTESIAN_POINT ( 'NONE',  ( 12.63842701281683034, 57.46726448433411605, 9.846743663894596210 ) ) ;
#46458 = CARTESIAN_POINT ( 'NONE',  ( -0.3689425029237881626, 42.42874883491396787, 10.36894250292379027 ) ) ;
#46459 = ORIENTED_EDGE ( 'NONE', *, *, #73699, .F. ) ;
#46460 = CARTESIAN_POINT ( 'NONE',  ( 2.917880565312948704, 7.637082168247301794, 12.26659068614894643 ) ) ;
#46461 = CARTESIAN_POINT ( 'NONE',  ( 19.42250999205614548, 60.98035201082151247, -5.440088680355545492 ) ) ;
#46463 = FACE_OUTER_BOUND ( 'NONE', #61533, .T. ) ;
#46462 =( NAMED_UNIT ( * ) SI_UNIT ( $, .STERADIAN. ) SOLID_ANGLE_UNIT ( ) );
#46464 = CARTESIAN_POINT ( 'NONE',  ( 15.44008868035555793, 11.39701867748817143, -9.422509992056140149 ) ) ;
#46465 = CARTESIAN_POINT ( 'NONE',  ( 16.40814093676324603, 12.45696800326375353, -11.09922568453594671 ) ) ;
#46466 = CARTESIAN_POINT ( 'NONE',  ( 1.472469842513823179, 1.425597817667451528, 4.923371831947296329 ) ) ;
#46467 = CARTESIAN_POINT ( 'NONE',  ( 14.42571047809456175, 0.2306972965111693252, 3.890621016587945569 ) ) ;
#46468 = CARTESIAN_POINT ( 'NONE',  ( 17.08211943468705840, 60.13708216824729647, -12.26659068614894466 ) ) ;
#46469 = FACE_OUTER_BOUND ( 'NONE', #30850, .T. ) ;
#46470 = CARTESIAN_POINT ( 'NONE',  ( 7.084665262690076126, 22.02201867748817321, -10.88017736071110164 ) ) ;
#46471 = CARTESIAN_POINT ( 'NONE',  ( 20.88017736071110164, 25.35535201082150891, 2.915334737309930979 ) ) ;
#46472 = CARTESIAN_POINT ( 'NONE',  ( 10.00000000000000178, 52.25893115100078745, 9.846743663894594434 ) ) ;
#46473 = CARTESIAN_POINT ( 'NONE',  ( 5.076628168052703671, 56.84226448433412315, 8.527530157486179263 ) ) ;
#46474 = CARTESIAN_POINT ( 'NONE',  ( 19.38216949554541202, 50.99863466993042493, 9.382169495545424454 ) ) ;
#46475 = CARTESIAN_POINT ( 'NONE',  ( 5.076628168052703671, 1.842264484334118047, 8.527530157486179263 ) ) ;
#46476 = ORIENTED_EDGE ( 'NONE', *, *, #21654, .F. ) ;
#46477 = VECTOR ( 'NONE', #864, 1000.000000000000000 ) ;
#46478 = COLOUR_RGB ( '', 0.08235294, 0.09019608, 0.10196078) ;
#46479 = CARTESIAN_POINT ( 'NONE',  ( 20.88017736071110875, 10.77201867748817143, -2.915334737309920765 ) ) ;
#46480 = CARTESIAN_POINT ( 'NONE',  ( 6.565887622018943937, 18.08196800326375708, -12.81628187352647608 ) ) ;
#46481 = STYLED_ITEM ( 'NONE', ( #39473 ), #79694 ) ;
#46482 = CARTESIAN_POINT ( 'NONE',  ( 1.472469842513823179, 46.42559781766745175, 4.923371831947296329 ) ) ;
#46483 = CARTESIAN_POINT ( 'NONE',  ( -0.8801773607111008646, 48.27201867748816966, 2.915334737309923430 ) ) ;
#46484 = CARTESIAN_POINT ( 'NONE',  ( 13.43411237798105340, 15.58196800326374998, 12.81628187352647963 ) ) ;
#46486 = CARTESIAN_POINT ( 'NONE',  ( 4.629999999999995453, 43.00000000000000711, -4.250000000000000000 ) ) ;
#46485 = CARTESIAN_POINT ( 'NONE',  ( 0.5774900079438590739, 67.64701867748817676, -5.440088680355550821 ) ) ;
#46487 = VERTEX_POINT ( 'NONE', #28029 ) ;
#46488 = DIRECTION ( 'NONE',  ( 0.000000000000000000, 0.000000000000000000, 1.000000000000000000 ) ) ;
#46489 = CYLINDRICAL_SURFACE ( 'NONE', #22283, 15.00000000000000000 ) ;
#46490 = CARTESIAN_POINT ( 'NONE',  ( 4.559911319644449179, 48.89701867748817676, 9.422509992056141925 ) ) ;
#46492 = CARTESIAN_POINT ( 'NONE',  ( 20.36894250292379382, 13.67874883491396965, 10.36894250292379205 ) ) ;
#46491 = CARTESIAN_POINT ( 'NONE',  ( 16.40814093676324603, 52.45696800326375353, -11.09922568453594671 ) ) ;
#46493 = CARTESIAN_POINT ( 'NONE',  ( 12.63842701281683034, 7.467264484334118713, 9.846743663894596210 ) ) ;
#46494 = FACE_OUTER_BOUND ( 'NONE', #14653, .T. ) ;
#46495 = CARTESIAN_POINT ( 'NONE',  ( 19.84674366389459266, 18.30059781766745175, 2.638427012816836559 ) ) ;
#46496 = DIRECTION ( 'NONE',  ( -0.000000000000000000, -0.000000000000000000, -1.000000000000000000 ) ) ;
#46497 = CARTESIAN_POINT ( 'NONE',  ( -4.164238869374099927, 52.01208216824729647, 3.795296366450308767 ) ) ;
#46498 = EDGE_CURVE ( 'NONE', #42399, #18624, #45819, .T. ) ;
#46499 = CARTESIAN_POINT ( 'NONE',  ( 0.5774900079438590739, 7.647018677488171434, -5.440088680355550821 ) ) ;
#46500 = DIRECTION ( 'NONE',  ( -2.042810365310288034E-14, 0.000000000000000000, 1.000000000000000000 ) ) ;
#46501 = CIRCLE ( 'NONE', #32136, 0.1000000000000001166 ) ;
#46502 = ORIENTED_EDGE ( 'NONE', *, *, #12686, .F. ) ;
#46503 = ORIENTED_EDGE ( 'NONE', *, *, #4231, .F. ) ;
#46504 = CARTESIAN_POINT ( 'NONE',  ( 10.00000000000000178, 9.313685344154839285, 10.88017736071110342 ) ) ;
#46505 = CARTESIAN_POINT ( 'NONE',  ( -0.8801773607111009756, 13.06368534415483929, 1.068504757029289695E-15 ) ) ;
#46506 = CARTESIAN_POINT ( 'NONE',  ( 7.361572987183170547, 42.05059781766745886, 9.846743663894590881 ) ) ;
#46507 = CARTESIAN_POINT ( 'NONE',  ( 3.591859063236763294, 38.29030133659708923, -11.09922568453595026 ) ) ;
#46508 = CARTESIAN_POINT ( 'NONE',  ( 19.72487221294570858, 70.00000000000000000, -6.000000000000000000 ) ) ;
#46510 = CARTESIAN_POINT ( 'NONE',  ( 20.36894250292379382, 13.67874883491396965, 10.36894250292379205 ) ) ;
#46509 = CARTESIAN_POINT ( 'NONE',  ( 1.274849032793998305, 2.555090184799397424, -6.499999999999581668 ) ) ;
#46511 = CARTESIAN_POINT ( 'NONE',  ( -0.8801773607110991993, 32.85535201082151247, -2.915334737309923874 ) ) ;
#46512 = CARTESIAN_POINT ( 'NONE',  ( -0.8801773607111008646, 8.272018677488171434, 2.915334737309923430 ) ) ;
#46513 = CARTESIAN_POINT ( 'NONE',  ( 18.52753015748617571, 38.09226448433412315, 4.923371831947298993 ) ) ;
#46514 = DIRECTION ( 'NONE',  ( -1.000000000000000000, 0.000000000000000000, 0.000000000000000000 ) ) ;
#46515 = CARTESIAN_POINT ( 'NONE',  ( 19.84674366389459266, 18.71726448433411960, -2.638427012816827677 ) ) ;
#46516 = CARTESIAN_POINT ( 'NONE',  ( 8.838651438279482520, 14.95077488074853456, 11.81204219878344475 ) ) ;
#46517 = CARTESIAN_POINT ( 'NONE',  ( 4.923371831947295441, 24.34226448433413026, -8.527530157486179263 ) ) ;
#46518 = EDGE_LOOP ( 'NONE', ( #40471, #51351, #71983, #583 ) ) ;
#46519 = VECTOR ( 'NONE', #97562, 1000.000000000000000 ) ;
#46520 =( NAMED_UNIT ( * ) SI_UNIT ( $, .STERADIAN. ) SOLID_ANGLE_UNIT ( ) );
#46521 = ORIENTED_EDGE ( 'NONE', *, *, #80080, .T. ) ;
#46522 = CARTESIAN_POINT ( 'NONE',  ( 14.92337183194729633, 62.67559781766745886, 8.527530157486181039 ) ) ;
#46524 = CARTESIAN_POINT ( 'NONE',  ( 15.44008868035555260, 34.73035201082151247, 9.422509992056143702 ) ) ;
#46523 = CARTESIAN_POINT ( 'NONE',  ( 20.88017736071110164, 30.35535201082151247, 2.915334737309930979 ) ) ;
#46526 = CARTESIAN_POINT ( 'NONE',  ( -2.816281873526473856, 34.33196800326376064, 3.434112377981055619 ) ) ;
#46525 = CARTESIAN_POINT ( 'NONE',  ( 17.96484262340118221, 9.938685344154837509, 7.964842623401181321 ) ) ;
#46527 = CARTESIAN_POINT ( 'NONE',  ( 17.08211943468705130, 13.47041550158063572, 12.26659068614894998 ) ) ;
#46528 = EDGE_CURVE ( 'NONE', #13075, #77672, #20543, .T. ) ;
#46529 = CARTESIAN_POINT ( 'NONE',  ( 0.6178305044545838731, 44.74863466993042493, 9.382169495545420901 ) ) ;
#46530 = ORIENTED_EDGE ( 'NONE', *, *, #39088, .T. ) ;
#46531 = CARTESIAN_POINT ( 'NONE',  ( 10.00000000000000178, 42.25893115100078745, 9.846743663894594434 ) ) ;
#46532 = ADVANCED_FACE ( 'NONE', ( #43042 ), #57050, .T. ) ;
#46533 = CARTESIAN_POINT ( 'NONE',  ( -0.8801773607111009756, 23.06368534415484106, 1.068504757029289695E-15 ) ) ;
#46534 = ORIENTED_EDGE ( 'NONE', *, *, #2392, .F. ) ;
#46535 = FACE_OUTER_BOUND ( 'NONE', #43678, .T. ) ;
#46536 = CARTESIAN_POINT ( 'NONE',  ( -0.8801773607111008646, 23.27201867748817676, 2.915334737309923430 ) ) ;
#46537 = ORIENTED_EDGE ( 'NONE', *, *, #52742, .T. ) ;
#46538 = CARTESIAN_POINT ( 'NONE',  ( 10.00000000000000178, 59.31368534415484106, 10.88017736071110342 ) ) ;
#46539 = CARTESIAN_POINT ( 'NONE',  ( 15.44008868035555793, 66.39701867748817676, -9.422509992056140149 ) ) ;
#46540 = CARTESIAN_POINT ( 'NONE',  ( 15.44008868035555793, 61.39701867748817676, -9.422509992056140149 ) ) ;
#46541 = CARTESIAN_POINT ( 'NONE',  ( 19.84674366389459266, 3.300597817667451750, 2.638427012816836559 ) ) ;
#46542 = CARTESIAN_POINT ( 'NONE',  ( 17.96484262340118221, 61.18868534415482685, -7.964842623401177768 ) ) ;
#46543 = STYLED_ITEM ( 'NONE', ( #53838 ), #39083 ) ;
#46544 = LINE ( 'NONE', #9039, #20315 ) ;
#46545 = CARTESIAN_POINT ( 'NONE',  ( -46.94000000000001194, 101.9444105523804893, 6.894162316358291243 ) ) ;
#46547 = EDGE_LOOP ( 'NONE', ( #81523, #65078, #76172, #21924 ) ) ;
#46546 = CARTESIAN_POINT ( 'NONE',  ( 5.076628168052704559, 10.17559781766745175, -8.527530157486179263 ) ) ;
#46548 = MECHANICAL_DESIGN_GEOMETRIC_PRESENTATION_REPRESENTATION (  '', ( #88081 ), #62523 ) ;
#46549 = CARTESIAN_POINT ( 'NONE',  ( 0.1532563361054082862, 46.21726448433411605, 2.638427012816831674 ) ) ;
#46550 = ORIENTED_EDGE ( 'NONE', *, *, #42281, .T. ) ;
#46551 = ORIENTED_EDGE ( 'NONE', *, *, #33872, .T. ) ;
#46552 = DIRECTION ( 'NONE',  ( -0.9099612708765399960, 0.000000000000000000, -0.4146932426562462415 ) ) ;
#46553 = CARTESIAN_POINT ( 'NONE',  ( 8.629999999999995453, 41.24999999999999289, -6.250000000000000000 ) ) ;
#46554 = LINE ( 'NONE', #23586, #22539 ) ;
#46555 = CARTESIAN_POINT ( 'NONE',  ( 10.00000000000000000, 25.55374883491396787, -14.16423886937410082 ) ) ;
#46556 = CARTESIAN_POINT ( 'NONE',  ( 0.2751277870542911397, 35.30223176428830811, 6.499999999999992006 ) ) ;
#46557 = DIRECTION ( 'NONE',  ( -0.000000000000000000, 1.000000000000000000, -0.000000000000000000 ) ) ;
#46558 = CARTESIAN_POINT ( 'NONE',  ( 12.91533473730992121, 19.52201867748816611, 10.88017736071110164 ) ) ;
#46559 = DIRECTION ( 'NONE',  ( 1.000000000000000000, 0.000000000000000000, 0.000000000000000000 ) ) ;
#46560 = VERTEX_POINT ( 'NONE', #34042 ) ;
#46561 = CARTESIAN_POINT ( 'NONE',  ( 5.076628168052703671, 6.842264484334118713, 8.527530157486179263 ) ) ;
#46562 = CARTESIAN_POINT ( 'NONE',  ( 3.591859063236761518, 34.95696800326375353, 11.09922568453594849 ) ) ;
#46564 = EDGE_CURVE ( 'NONE', #25275, #26584, #22616, .T. ) ;
#46563 = CARTESIAN_POINT ( 'NONE',  ( 0.1532563361054083140, 21.00893115100078745, 1.131784320476157264E-15 ) ) ;
#46565 = FILL_AREA_STYLE_COLOUR ( '', #34577 ) ;
#46566 = CARTESIAN_POINT ( 'NONE',  ( 22.81628187352648496, 11.83196800326375531, -3.434112377981050290 ) ) ;
#46567 = DIRECTION ( 'NONE',  ( -0.000000000000000000, 0.000000000000000000, 1.000000000000000000 ) ) ;
#46568 = AXIS2_PLACEMENT_3D ( 'NONE', #92095, #76107, #60106 ) ;
#46569 = CARTESIAN_POINT ( 'NONE',  ( 0.1532563361054083140, 1.008931151000784787, 1.131784320476157264E-15 ) ) ;
#46570 = EDGE_LOOP ( 'NONE', ( #84668, #96604, #61866, #48029, #4616, #67376 ) ) ;
#46571 = ORIENTED_EDGE ( 'NONE', *, *, #7616, .F. ) ;
#46572 = CARTESIAN_POINT ( 'NONE',  ( 2.035157376598822676, 27.43868534415483396, -7.964842623401177768 ) ) ;
#46573 = CARTESIAN_POINT ( 'NONE',  ( 6.204703633549690345, 22.84541550158062861, 14.16423886937410082 ) ) ;
#46574 = CARTESIAN_POINT ( 'NONE',  ( 10.00000000000000000, 39.75893115100078745, -9.846743663894594434 ) ) ;
#46575 = CARTESIAN_POINT ( 'NONE',  ( 5.076628168052704559, 0.1755978176674514724, -8.527530157486179263 ) ) ;
#46576 = PRESENTATION_LAYER_ASSIGNMENT (  '', '', ( #11468 ) ) ;
#46578 = DIRECTION ( 'NONE',  ( 1.000000000000000000, 0.000000000000000000, 0.000000000000000000 ) ) ;
#46577 = CARTESIAN_POINT ( 'NONE',  ( 22.81628187352648496, 51.83196800326376064, -3.434112377981050290 ) ) ;
#46579 = CARTESIAN_POINT ( 'NONE',  ( 4.559911319644449179, 27.23035201082150536, -9.422509992056141925 ) ) ;
#46580 = DIRECTION ( 'NONE',  ( 1.000000000000000000, 0.000000000000000000, 0.000000000000000000 ) ) ;
#46581 = CARTESIAN_POINT ( 'NONE',  ( -1.099225684535947600, 13.70696800326375353, -6.408140936763238038 ) ) ;
#46582 = CARTESIAN_POINT ( 'NONE',  ( -2.816281873526473856, 4.123634669930420493, 9.499525473075851096E-16 ) ) ;
#46583 = CARTESIAN_POINT ( 'NONE',  ( 19.84674366389459266, 43.30059781766744464, 2.638427012816836559 ) ) ;
#46584 = CARTESIAN_POINT ( 'NONE',  ( 10.88017736071109987, 0.7720186774881703240, -2.915334737309928315 ) ) ;
#46585 = CARTESIAN_POINT ( 'NONE',  ( 13.43411237798105340, 45.58196800326374643, 12.81628187352647963 ) ) ;
#46586 = CARTESIAN_POINT ( 'NONE',  ( -0.1034006766821533585, 0.000000000000000000, -14.49963131600461175 ) ) ;
#46587 =( GEOMETRIC_REPRESENTATION_CONTEXT ( 3 ) GLOBAL_UNCERTAINTY_ASSIGNED_CONTEXT ( ( #16126 ) ) GLOBAL_UNIT_ASSIGNED_CONTEXT ( ( #21549, #89047, #13045 ) ) REPRESENTATION_CONTEXT ( 'NONE', 'WORKASPACE' ) );
#46589 = LINE ( 'NONE', #94548, #30274 ) ;
#46588 = CARTESIAN_POINT ( 'NONE',  ( 20.88017736071110519, 55.56368534415484817, 2.639326808657452039E-16 ) ) ;
#46590 = CARTESIAN_POINT ( 'NONE',  ( -14.56311970191023164, 0.2301500865527675577, -3.337330457606075829 ) ) ;
#46591 = CARTESIAN_POINT ( 'NONE',  ( -0.8801773607111008646, 53.27201867748816966, 2.915334737309923430 ) ) ;
#46592 = CARTESIAN_POINT ( 'NONE',  ( 2.035157376598824452, 43.68868534415484106, 7.964842623401179544 ) ) ;
#46593 = CARTESIAN_POINT ( 'NONE',  ( 7.771322705631503069, 15.00000000000000000, -12.24159072199917375 ) ) ;
#46594 = CARTESIAN_POINT ( 'NONE',  ( 0.5774900079438607392, 68.48035201082150536, 5.440088680355550821 ) ) ;
#46595 = CARTESIAN_POINT ( 'NONE',  ( 2.791683348922237240, 45.38393115100079456, -7.208316651077763204 ) ) ;
#46597 = CARTESIAN_POINT ( 'NONE',  ( 9.240973841163606650, 4.560084876699663581E-16, -11.17382667070372726 ) ) ;
#46596 = CARTESIAN_POINT ( 'NONE',  ( 0.5774900079438607392, 8.480352010821505360, 5.440088680355550821 ) ) ;
#46598 = CARTESIAN_POINT ( 'NONE',  ( -2.816281873526473856, 29.12363466993041783, 9.499525473075851096E-16 ) ) ;
#46599 = ORIENTED_EDGE ( 'NONE', *, *, #19468, .T. ) ;
#46600 = CARTESIAN_POINT ( 'NONE',  ( 17.96484262340118221, 41.18868534415484106, -7.964842623401177768 ) ) ;
#46602 = DIRECTION ( 'NONE',  ( 1.000000000000000000, 0.000000000000000000, 0.000000000000000000 ) ) ;
#46601 = CARTESIAN_POINT ( 'NONE',  ( 3.591859063236761518, 4.956968003263753531, 11.09922568453594849 ) ) ;
#46603 = CARTESIAN_POINT ( 'NONE',  ( 15.44008868035555793, 16.39701867748817321, -9.422509992056140149 ) ) ;
#46604 = CARTESIAN_POINT ( 'NONE',  ( 2.035157376598824452, 23.68868534415484461, 7.964842623401179544 ) ) ;
#46605 = CARTESIAN_POINT ( 'NONE',  ( 10.00000000000000000, 40.55374883491397497, -14.16423886937410082 ) ) ;
#46606 = CARTESIAN_POINT ( 'NONE',  ( 18.52753015748617571, 28.09226448433411960, 4.923371831947298993 ) ) ;
#46607 = CARTESIAN_POINT ( 'NONE',  ( 12.91533473730992121, 64.52201867748817676, 10.88017736071110164 ) ) ;
#46608 = DIRECTION ( 'NONE',  ( -1.000000000000000000, 0.000000000000000000, 0.000000000000000000 ) ) ;
#46609 =( LENGTH_UNIT ( ) NAMED_UNIT ( * ) SI_UNIT ( .MILLI., .METRE. ) );
#46610 = ADVANCED_FACE ( 'NONE', ( #80550 ), #36026, .F. ) ;
#46611 = CARTESIAN_POINT ( 'NONE',  ( 0.000000000000000000, 14.49999999999999822, 0.000000000000000000 ) ) ;
#46612 = CARTESIAN_POINT ( 'NONE',  ( 19.84674366389459266, 53.71726448433411605, -2.638427012816827677 ) ) ;
#46613 = ORIENTED_EDGE ( 'NONE', *, *, #4287, .T. ) ;
#46614 = ORIENTED_EDGE ( 'NONE', *, *, #73494, .F. ) ;
#46615 = VECTOR ( 'NONE', #88564, 1000.000000000000114 ) ;
#46616 = CARTESIAN_POINT ( 'NONE',  ( 20.36894250292379738, 29.92874883491396432, -10.36894250292379027 ) ) ;
#46617 = CARTESIAN_POINT ( 'NONE',  ( -4.164238869374099039, 41.80374883491397497, 8.674139862899312516E-16 ) ) ;
#46618 = CARTESIAN_POINT ( 'NONE',  ( 0.1532563361054083140, 1.008931151000784787, 1.131784320476157264E-15 ) ) ;
#46619 = CARTESIAN_POINT ( 'NONE',  ( 14.92337183194729633, 62.67559781766745886, 8.527530157486181039 ) ) ;
#46620 = CARTESIAN_POINT ( 'NONE',  ( -10.07339213344192963, -32.14942050451718814, 3.750000000000000000 ) ) ;
#46622 = CARTESIAN_POINT ( 'NONE',  ( 10.00000000000000178, 20.37363466993042138, 12.81628187352647608 ) ) ;
#46621 = CARTESIAN_POINT ( 'NONE',  ( 10.00000000000000000, 61.81368534415484106, -10.88017736071110342 ) ) ;
#46623 = CARTESIAN_POINT ( 'NONE',  ( -4.164238869374098151, 31.59541550158063927, -3.795296366450310543 ) ) ;
#46624 = CARTESIAN_POINT ( 'NONE',  ( 4.559911319644449179, 32.23035201082150536, -9.422509992056141925 ) ) ;
#46625 = CARTESIAN_POINT ( 'NONE',  ( -0.8801773607111008646, 28.27201867748817321, 2.915334737309923430 ) ) ;
#46626 = DIRECTION ( 'NONE',  ( -0.000000000000000000, -0.000000000000000000, 1.000000000000000000 ) ) ;
#46627 = CARTESIAN_POINT ( 'NONE',  ( 12.91533473730992121, 54.52201867748816255, 10.88017736071110164 ) ) ;
#46628 = CARTESIAN_POINT ( 'NONE',  ( -7.208316651077764980, -4.616068848999211660, -7.208316651077759651 ) ) ;
#46629 = ORIENTED_EDGE ( 'NONE', *, *, #62428, .F. ) ;
#46630 = DIRECTION ( 'NONE',  ( -0.000000000000000000, 0.000000000000000000, 1.000000000000000000 ) ) ;
#46631 = CYLINDRICAL_SURFACE ( 'NONE', #76487, 0.5000000000000004441 ) ;
#46632 = ORIENTED_EDGE ( 'NONE', *, *, #74543, .F. ) ;
#46633 = CARTESIAN_POINT ( 'NONE',  ( 24.16423886937409904, 9.095415501580633943, 3.795296366450317205 ) ) ;
#46635 = CARTESIAN_POINT ( 'NONE',  ( 20.36894250292379382, 63.67874883491396787, 10.36894250292379205 ) ) ;
#46634 = CARTESIAN_POINT ( 'NONE',  ( -2.266590686148945544, 57.22041550158063217, 7.082119434687048631 ) ) ;
#46637 = CARTESIAN_POINT ( 'NONE',  ( 7.361572987183169658, 64.96726448433412315, -9.846743663894592657 ) ) ;
#46636 = CARTESIAN_POINT ( 'NONE',  ( 18.52753015748617571, 33.09226448433411605, 4.923371831947298993 ) ) ;
#46638 = DIRECTION ( 'NONE',  ( 0.3502073812594559410, 0.000000000000000000, 0.9366721892484018985 ) ) ;
#46639 = CARTESIAN_POINT ( 'NONE',  ( -2.393480905993275343, 14.63606894034134420, 14.80781041047753810 ) ) ;
#46640 = AXIS2_PLACEMENT_3D ( 'NONE', #86759, #34719, #56742 ) ;
#46641 = EDGE_CURVE ( 'NONE', #37440, #63858, #43357, .T. ) ;
#46642 = CARTESIAN_POINT ( 'NONE',  ( 13.43411237798106583, 7.665301336597086568, -12.81628187352647252 ) ) ;
#46643 = VERTEX_POINT ( 'NONE', #59022 ) ;
#46644 = VECTOR ( 'NONE', #2573, 1000.000000000000227 ) ;
#46645 = CARTESIAN_POINT ( 'NONE',  ( -0.3689425029237881626, 52.42874883491396076, 10.36894250292379027 ) ) ;
#46646 = ADVANCED_FACE ( 'NONE', ( #95046 ), #89528, .F. ) ;
#46647 = TOROIDAL_SURFACE ( 'NONE', #37097, 14.49999999999999822, 0.5000000000000000000 ) ;
#46648 = CARTESIAN_POINT ( 'NONE',  ( -4.164238869374099927, 42.01208216824728936, 3.795296366450308767 ) ) ;
#46649 = EDGE_LOOP ( 'NONE', ( #56720, #13596, #78465, #13706, #25544, #85446 ) ) ;
#46650 = CARTESIAN_POINT ( 'NONE',  ( 19.42250999205614548, 15.98035201082150714, -5.440088680355545492 ) ) ;
#46651 = CARTESIAN_POINT ( 'NONE',  ( 21.09922568453595559, 62.04030133659709634, -6.408140936763230044 ) ) ;
#46652 = CARTESIAN_POINT ( 'NONE',  ( 10.00000000000000178, 29.31368534415483751, 10.88017736071110342 ) ) ;
#46653 = CARTESIAN_POINT ( 'NONE',  ( 5.076628168052703671, 46.84226448433412315, 8.527530157486179263 ) ) ;
#46654 = CARTESIAN_POINT ( 'NONE',  ( 17.96484262340118221, 31.18868534415483751, -7.964842623401177768 ) ) ;
#46655 = AXIS2_PLACEMENT_3D ( 'NONE', #38855, #1851, #77811 ) ;
#46656 = CARTESIAN_POINT ( 'NONE',  ( -0.2418659066527717449, 65.11633188102328518, 6.114288769123044531 ) ) ;
#46657 = CARTESIAN_POINT ( 'NONE',  ( 18.52753015748618282, 58.92559781766745886, -4.923371831947291888 ) ) ;
#46658 = CARTESIAN_POINT ( 'NONE',  ( 17.96484262340118221, 59.93868534415484106, 7.964842623401181321 ) ) ;
#46659 = AXIS2_PLACEMENT_3D ( 'NONE', #33772, #2841, #72765 ) ;
#46661 = ORIENTED_EDGE ( 'NONE', *, *, #50666, .F. ) ;
#46660 = DIRECTION ( 'NONE',  ( 0.000000000000000000, -0.000000000000000000, -1.000000000000000000 ) ) ;
#46662 = DIRECTION ( 'NONE',  ( 0.000000000000000000, 0.000000000000000000, 1.000000000000000000 ) ) ;
#46663 = DIRECTION ( 'NONE',  ( 0.000000000000000000, 0.000000000000000000, 1.000000000000000000 ) ) ;
#46664 = ORIENTED_EDGE ( 'NONE', *, *, #47660, .T. ) ;
#46665 =( NAMED_UNIT ( * ) PLANE_ANGLE_UNIT ( ) SI_UNIT ( $, .RADIAN. ) );
#46666 = CARTESIAN_POINT ( 'NONE',  ( 5.076628168052704559, 30.17559781766745175, -8.527530157486179263 ) ) ;
#46667 = LINE ( 'NONE', #8673, #89963 ) ;
#46668 = CARTESIAN_POINT ( 'NONE',  ( 19.38216949554541202, 45.99863466993041072, 9.382169495545424454 ) ) ;
#46669 = CARTESIAN_POINT ( 'NONE',  ( 15.00000000000000000, 60.50000000000000000, 6.500000000000000888 ) ) ;
#46670 = CARTESIAN_POINT ( 'NONE',  ( 6.880000000000009663, 41.24999999999999289, 6.250000000000000000 ) ) ;
#46671 = ORIENTED_EDGE ( 'NONE', *, *, #3565, .F. ) ;
#46672 = CARTESIAN_POINT ( 'NONE',  ( 7.361572987183169658, 64.96726448433412315, -9.846743663894592657 ) ) ;
#46673 = CARTESIAN_POINT ( 'NONE',  ( 0.000000000000000000, 14.49999999999999822, 0.000000000000000000 ) ) ;
#46674 = CARTESIAN_POINT ( 'NONE',  ( 0.1532563361054100626, 55.80059781766745175, -2.638427012816831230 ) ) ;
#46675 = CARTESIAN_POINT ( 'NONE',  ( 13.79529636645031943, 30.34541550158063927, -14.16423886937409904 ) ) ;
#46676 = CARTESIAN_POINT ( 'NONE',  ( 0.1532563361054082862, 61.21726448433412315, 2.638427012816831674 ) ) ;
#46677 = CARTESIAN_POINT ( 'NONE',  ( 2.603489959281586774, 5.435752660568278216, -6.500000000000001776 ) ) ;
#46678 = CARTESIAN_POINT ( 'NONE',  ( 18.52753015748618282, 18.92559781766745175, -4.923371831947291888 ) ) ;
#46679 = CARTESIAN_POINT ( 'NONE',  ( 10.00000000000000178, 55.37363466993042493, 12.81628187352647608 ) ) ;
#46680 = CARTESIAN_POINT ( 'NONE',  ( 24.16423886937409904, 4.095415501580634832, 3.795296366450317205 ) ) ;
#46681 = CARTESIAN_POINT ( 'NONE',  ( -1.099225684535947600, -1.293031996736246469, -6.408140936763238038 ) ) ;
#46683 = ADVANCED_FACE ( 'NONE', ( #82518 ), #60005, .T. ) ;
#46682 = CARTESIAN_POINT ( 'NONE',  ( -0.8801773607110991993, 52.85535201082151247, -2.915334737309923874 ) ) ;
#46684 = CARTESIAN_POINT ( 'NONE',  ( 18.52753015748618282, 38.92559781766745175, -4.923371831947291888 ) ) ;
#46685 = CARTESIAN_POINT ( 'NONE',  ( -6.599999999999995204, -97.00000000000000000, 4.000000000000000000 ) ) ;
#46686 = ORIENTED_EDGE ( 'NONE', *, *, #46851, .T. ) ;
#46687 = CARTESIAN_POINT ( 'NONE',  ( -38.69000000000001194, 93.50000000000000000, -9.500000000000000000 ) ) ;
#46688 = CARTESIAN_POINT ( 'NONE',  ( 10.00000000000000178, 29.31368534415483751, 10.88017736071110342 ) ) ;
#46690 = CARTESIAN_POINT ( 'NONE',  ( 12.91533473730992121, 59.52201867748816966, 10.88017736071110164 ) ) ;
#46689 = CARTESIAN_POINT ( 'NONE',  ( 21.09922568453595559, 2.040301336597086568, -6.408140936763230044 ) ) ;
#46691 = DIRECTION ( 'NONE',  ( -1.000000000000000000, 0.000000000000000000, -0.000000000000000000 ) ) ;
#46692 = ADVANCED_FACE ( 'NONE', ( #90499 ), #98545, .T. ) ;
#46693 = CARTESIAN_POINT ( 'NONE',  ( 0.5774900079438607392, 68.48035201082150536, 5.440088680355550821 ) ) ;
#46694 = CARTESIAN_POINT ( 'NONE',  ( 10.32896413005680181, 5.578790035174474582, -5.963430220938285231 ) ) ;
#46696 = CARTESIAN_POINT ( 'NONE',  ( 0.2751277870542909731, 62.28217586085237656, -6.499999999999992006 ) ) ;
#46695 = CARTESIAN_POINT ( 'NONE',  ( 12.91533473730993009, 36.60535201082151247, -10.88017736071109987 ) ) ;
#46697 = CARTESIAN_POINT ( 'NONE',  ( 17.20831665107776587, 44.13393115100078745, -7.208316651077762316 ) ) ;
#46698 = CARTESIAN_POINT ( 'NONE',  ( 0.1532563361054083140, 1.008931151000784787, 1.131784320476157264E-15 ) ) ;
#46699 = CARTESIAN_POINT ( 'NONE',  ( -10.88017736071109987, -31.72798132251182679, 2.915334737309934532 ) ) ;
#46700 = CARTESIAN_POINT ( 'NONE',  ( 21.09922568453594849, 11.20696800326375531, 6.408140936763242479 ) ) ;
#46701 = CARTESIAN_POINT ( 'NONE',  ( 7.084665262690076126, 9.105352010821503583, 10.88017736071109987 ) ) ;
#46702 = PLANE ( 'NONE',  #48467 ) ;
#46703 = CARTESIAN_POINT ( 'NONE',  ( -2.266590686148945544, 17.22041550158063572, 7.082119434687048631 ) ) ;
#46704 = CARTESIAN_POINT ( 'NONE',  ( 22.26659068614895176, 59.72041550158063927, -7.082119434687042414 ) ) ;
#46705 = CARTESIAN_POINT ( 'NONE',  ( 19.84674366389459266, 23.30059781766745530, 2.638427012816836559 ) ) ;
#46706 = SURFACE_STYLE_FILL_AREA ( #7249 ) ;
#46707 = ORIENTED_EDGE ( 'NONE', *, *, #97575, .F. ) ;
#46708 = CARTESIAN_POINT ( 'NONE',  ( 12.63842701281683034, 22.46726448433411605, 9.846743663894596210 ) ) ;
#46709 = CARTESIAN_POINT ( 'NONE',  ( 7.084665262690076126, 27.02201867748817676, -10.88017736071110164 ) ) ;
#46710 = CARTESIAN_POINT ( 'NONE',  ( 0.1532563361054083140, 66.00893115100079456, 1.131784320476157264E-15 ) ) ;
#46711 = CARTESIAN_POINT ( 'NONE',  ( 24.16423886937410614, 14.51208216824730179, -3.795296366450302550 ) ) ;
#46712 = DIRECTION ( 'NONE',  ( 0.000000000000000000, -0.000000000000000000, -1.000000000000000000 ) ) ;
#46713 = PRESENTATION_LAYER_ASSIGNMENT (  '', '', ( #80191 ) ) ;
#46714 = PRESENTATION_LAYER_ASSIGNMENT (  '', '', ( #16402 ) ) ;
#46715 = CARTESIAN_POINT ( 'NONE',  ( 17.20831665107776587, 7.883931151000784787, 7.208316651077764980 ) ) ;
#46716 = CARTESIAN_POINT ( 'NONE',  ( 0.6178305044545838731, 34.74863466993042493, 9.382169495545420901 ) ) ;
#46717 = CARTESIAN_POINT ( 'NONE',  ( 5.076628168052703671, 41.84226448433411605, 8.527530157486179263 ) ) ;
#46718 = ORIENTED_EDGE ( 'NONE', *, *, #31371, .F. ) ;
#46719 = CARTESIAN_POINT ( 'NONE',  ( 2.791683348922240793, 16.63393115100078745, 7.208316651077764092 ) ) ;
#46720 = MECHANICAL_DESIGN_GEOMETRIC_PRESENTATION_REPRESENTATION (  '', ( #5267 ), #93036 ) ;
#46721 = CARTESIAN_POINT ( 'NONE',  ( 14.17193700899789022, -0.03417435944610275333, 1.489530601564113654 ) ) ;
#46722 = DIRECTION ( 'NONE',  ( -0.000000000000000000, -1.000000000000000000, -0.000000000000000000 ) ) ;
#46723 = CARTESIAN_POINT ( 'NONE',  ( 10.00000000000000000, 55.55374883491396787, -14.16423886937410082 ) ) ;
#46724 = PRESENTATION_STYLE_ASSIGNMENT (( #24244 ) ) ;
#46725 = CARTESIAN_POINT ( 'NONE',  ( 20.88017736071110164, 55.35535201082149825, 2.915334737309930979 ) ) ;
#46726 = CARTESIAN_POINT ( 'NONE',  ( 18.52753015748618282, 38.92559781766745175, -4.923371831947291888 ) ) ;
#46727 = CARTESIAN_POINT ( 'NONE',  ( 0.5774900079438590739, 22.64701867748817321, -5.440088680355550821 ) ) ;
#46728 = COLOUR_RGB ( '', 0.09019608, 0.27058824, 0.51372549) ;
#46729 = DIRECTION ( 'NONE',  ( 0.000000000000000000, 0.000000000000000000, 1.000000000000000000 ) ) ;
#46730 = CARTESIAN_POINT ( 'NONE',  ( 7.361572987183169658, 54.96726448433413026, -9.846743663894592657 ) ) ;
#46731 = CARTESIAN_POINT ( 'NONE',  ( -0.8801773607111008646, 43.27201867748817676, 2.915334737309923430 ) ) ;
#46732 = EDGE_CURVE ( 'NONE', #13300, #64876, #30491, .T. ) ;
#46733 = SURFACE_SIDE_STYLE ('',( #84266 ) ) ;
#46734 = VERTEX_POINT ( 'NONE', #84002 ) ;
#46735 = ORIENTED_EDGE ( 'NONE', *, *, #6509, .F. ) ;
#46736 = CARTESIAN_POINT ( 'NONE',  ( -11.62719953690071506, 15.00000000000000000, 9.476720473301710967 ) ) ;
#46737 = CARTESIAN_POINT ( 'NONE',  ( 6.204703633549690345, 2.845415501580634388, 14.16423886937410082 ) ) ;
#46738 = CARTESIAN_POINT ( 'NONE',  ( 5.076628168052704559, 45.17559781766745175, -8.527530157486179263 ) ) ;
#46739 = CARTESIAN_POINT ( 'NONE',  ( 17.20831665107776587, 17.88393115100078745, 7.208316651077764980 ) ) ;
#46740 = CARTESIAN_POINT ( 'NONE',  ( 22.81628187352648496, 56.83196800326374643, -3.434112377981050290 ) ) ;
#46742 = CARTESIAN_POINT ( 'NONE',  ( 18.52753015748617571, 43.09226448433412315, 4.923371831947298993 ) ) ;
#46741 = CARTESIAN_POINT ( 'NONE',  ( 10.00000000000000178, 14.31368534415483929, 10.88017736071110342 ) ) ;
#46743 = DIRECTION ( 'NONE',  ( 0.000000000000000000, -1.000000000000000000, 0.000000000000000000 ) ) ;
#46744 = ADVANCED_FACE ( 'NONE', ( #59518 ), #38540, .T. ) ;
#46745 = CARTESIAN_POINT ( 'NONE',  ( 22.26659068614895176, 24.72041550158063572, -7.082119434687042414 ) ) ;
#46746 = CARTESIAN_POINT ( 'NONE',  ( 22.26659068614894466, 63.88708216824730357, 7.082119434687054849 ) ) ;
#46747 = CARTESIAN_POINT ( 'NONE',  ( 17.20831665107776587, 62.88393115100078745, 7.208316651077764980 ) ) ;
#46748 = CARTESIAN_POINT ( 'NONE',  ( -11.29168986245629469, 14.76984976272667360, 9.783658503027758968 ) ) ;
#46749 = CARTESIAN_POINT ( 'NONE',  ( 20.88017736071110164, 50.35535201082151247, 2.915334737309930979 ) ) ;
#46750 = CARTESIAN_POINT ( 'NONE',  ( 0.1532563361054100626, 20.80059781766744464, -2.638427012816831230 ) ) ;
#46751 = AXIS2_PLACEMENT_3D ( 'NONE', #57971, #88477, #4506 ) ;
#46752 = CARTESIAN_POINT ( 'NONE',  ( -7.232415441807423129, -88.12698951299773853, 4.000000000000000000 ) ) ;
#46753 = ORIENTED_EDGE ( 'NONE', *, *, #31843, .F. ) ;
#46754 = LINE ( 'NONE', #32233, #82611 ) ;
#46755 = ORIENTED_EDGE ( 'NONE', *, *, #25222, .F. ) ;
#46756 = EDGE_CURVE ( 'NONE', #50558, #97012, #60920, .T. ) ;
#46757 = CARTESIAN_POINT ( 'NONE',  ( 7.361572987183169658, 9.967264484334119601, -9.846743663894592657 ) ) ;
#46758 = ORIENTED_EDGE ( 'NONE', *, *, #76347, .F. ) ;
#46759 = CARTESIAN_POINT ( 'NONE',  ( 24.16423886937410614, 19.51208216824729647, -3.795296366450302550 ) ) ;
#46760 = CARTESIAN_POINT ( 'NONE',  ( 0.1532563361054082862, 21.21726448433412315, 2.638427012816831674 ) ) ;
#46761 = CARTESIAN_POINT ( 'NONE',  ( 20.88017736071110875, 40.77201867748818387, -2.915334737309920765 ) ) ;
#46762 = ORIENTED_EDGE ( 'NONE', *, *, #9402, .T. ) ;
#46763 = CARTESIAN_POINT ( 'NONE',  ( 4.559911319644449179, 27.23035201082150536, -9.422509992056141925 ) ) ;
#46764 = VERTEX_POINT ( 'NONE', #60989 ) ;
#46765 = CARTESIAN_POINT ( 'NONE',  ( 7.084665262690076126, 44.10535201082151247, 10.88017736071109987 ) ) ;
#46766 = CARTESIAN_POINT ( 'NONE',  ( 22.26659068614894466, 3.887082168247300906, 7.082119434687054849 ) ) ;
#46767 = ORIENTED_EDGE ( 'NONE', *, *, #20474, .T. ) ;
#46768 = EDGE_CURVE ( 'NONE', #88041, #72980, #73686, .T. ) ;
#46769 = ORIENTED_EDGE ( 'NONE', *, *, #92673, .T. ) ;
#46770 = CARTESIAN_POINT ( 'NONE',  ( 10.00000000000000178, 20.37363466993042138, 12.81628187352647608 ) ) ;
#46771 = CARTESIAN_POINT ( 'NONE',  ( 0.1532563361054100626, 15.80059781766745353, -2.638427012816831230 ) ) ;
#46772 = DIRECTION ( 'NONE',  ( 1.000000000000000000, 0.000000000000000000, 0.000000000000000000 ) ) ;
#46773 = CARTESIAN_POINT ( 'NONE',  ( 13.43411237798106583, 47.66530133659709634, -12.81628187352647252 ) ) ;
#46774 = DIRECTION ( 'NONE',  ( 0.8038568606172162845, -0.000000000000000000, 0.5948227867513425915 ) ) ;
#46775 = CARTESIAN_POINT ( 'NONE',  ( 17.20831665107776587, 17.88393115100078745, 7.208316651077764980 ) ) ;
#46776 = CARTESIAN_POINT ( 'NONE',  ( 15.44008868035555793, 26.39701867748817321, -9.422509992056140149 ) ) ;
#46777 = COLOUR_RGB ( '', 0.40784314, 0.44705882, 0.49803922) ;
#46778 = ORIENTED_EDGE ( 'NONE', *, *, #7546, .F. ) ;
#46779 = CARTESIAN_POINT ( 'NONE',  ( 32.56412365047463453, 14.00000000000001066, -9.500000000000000000 ) ) ;
#46780 = CARTESIAN_POINT ( 'NONE',  ( 20.88017736071110875, 55.77201867748816966, -2.915334737309920765 ) ) ;
#46781 = DIRECTION ( 'NONE',  ( 0.000000000000000000, 0.000000000000000000, 1.000000000000000000 ) ) ;
#46782 = SPHERICAL_SURFACE ( 'NONE', #46165, 0.5000000000000000000 ) ;
#46783 = CARTESIAN_POINT ( 'NONE',  ( 20.88017736071110875, 65.77201867748817676, -2.915334737309920765 ) ) ;
#46784 = TOROIDAL_SURFACE ( 'NONE', #59565, 14.49999999999999822, 0.5000000000000000000 ) ;
#46785 =( GEOMETRIC_REPRESENTATION_CONTEXT ( 3 ) GLOBAL_UNCERTAINTY_ASSIGNED_CONTEXT ( ( #47338 ) ) GLOBAL_UNIT_ASSIGNED_CONTEXT ( ( #377, #46814, #8335 ) ) REPRESENTATION_CONTEXT ( 'NONE', 'WORKASPACE' ) );
#46786 = CARTESIAN_POINT ( 'NONE',  ( 13.43411237798105340, 0.5819680032637533085, 12.81628187352647963 ) ) ;
#46787 = CARTESIAN_POINT ( 'NONE',  ( 3.014428414850136129, 11.57636696231598350, 11.25000000000000000 ) ) ;
#46788 = CARTESIAN_POINT ( 'NONE',  ( 2.791683348922237240, 25.38393115100078390, -7.208316651077763204 ) ) ;
#46789 = CARTESIAN_POINT ( 'NONE',  ( 3.591859063236761518, 54.95696800326376064, 11.09922568453594849 ) ) ;
#46790 = CARTESIAN_POINT ( 'NONE',  ( -0.000000000000000000, 76.60832266181904515, 7.291975907158628090 ) ) ;
#46791 = CARTESIAN_POINT ( 'NONE',  ( 14.92337183194729988, 14.34226448433411782, -8.527530157486177487 ) ) ;
#46792 = STYLED_ITEM ( 'NONE', ( #84043 ), #76858 ) ;
#46793 = CARTESIAN_POINT ( 'NONE',  ( 3.591859063236761518, 19.95696800326375353, 11.09922568453594849 ) ) ;
#46795 = CARTESIAN_POINT ( 'NONE',  ( -45.94000000000000483, 92.50000000000000000, -8.999999999999998224 ) ) ;
#46794 = FILL_AREA_STYLE_COLOUR ( '', #80345 ) ;
#46796 = CARTESIAN_POINT ( 'NONE',  ( 12.91533473730993009, 46.60535201082150536, -10.88017736071109987 ) ) ;
#46797 = CARTESIAN_POINT ( 'NONE',  ( 1.472469842513823179, 60.59226448433412315, -4.923371831947296329 ) ) ;
#46798 = CARTESIAN_POINT ( 'NONE',  ( 12.60589901313216110, 0.5000000000000004441, 8.129656208642140669 ) ) ;
#46799 = CARTESIAN_POINT ( 'NONE',  ( 0.1532563361054100626, 15.80059781766745353, -2.638427012816831230 ) ) ;
#46801 = ADVANCED_FACE ( 'NONE', ( #83015 ), #68864, .F. ) ;
#46800 = CARTESIAN_POINT ( 'NONE',  ( 20.88017736071110875, 10.77201867748817143, -2.915334737309920765 ) ) ;
#46802 = CARTESIAN_POINT ( 'NONE',  ( 3.591859063236761518, 19.95696800326375353, 11.09922568453594849 ) ) ;
#46803 = PRESENTATION_STYLE_ASSIGNMENT (( #67846 ) ) ;
#46804 = CARTESIAN_POINT ( 'NONE',  ( -8.331109669465192269, 86.16998870897720053, 4.268594137767635743 ) ) ;
#46805 = CARTESIAN_POINT ( 'NONE',  ( 0.000000000000000000, 0.5000000000000004441, 0.000000000000000000 ) ) ;
#46806 = CARTESIAN_POINT ( 'NONE',  ( 4.559911319644449179, 13.89701867748817321, 9.422509992056141925 ) ) ;
#46807 = CARTESIAN_POINT ( 'NONE',  ( -1.926860441876564023, 49.68830936912750929, 1.004413902775740781E-15 ) ) ;
#46809 = CARTESIAN_POINT ( 'NONE',  ( 2.035157376598822676, 12.43868534415483751, -7.964842623401177768 ) ) ;
#46808 = CARTESIAN_POINT ( 'NONE',  ( 0.1532563361054083140, 36.00893115100078745, 1.131784320476157264E-15 ) ) ;
#46810 = DIRECTION ( 'NONE',  ( 0.8338858220671618859, 0.000000000000000000, 0.5519369853120676961 ) ) ;
#46811 = CARTESIAN_POINT ( 'NONE',  ( 12.91533473730993009, 31.60535201082150891, -10.88017736071109987 ) ) ;
#46813 = CARTESIAN_POINT ( 'NONE',  ( 9.399392868737718842, 15.00000000000000000, 11.04089732309479110 ) ) ;
#46812 = CARTESIAN_POINT ( 'NONE',  ( 20.36894250292379382, 63.67874883491396787, 10.36894250292379205 ) ) ;
#46814 =( NAMED_UNIT ( * ) PLANE_ANGLE_UNIT ( ) SI_UNIT ( $, .RADIAN. ) );
#46815 = CARTESIAN_POINT ( 'NONE',  ( 19.84674366389459621, 28.50893115100078745, 7.409399052514197653E-17 ) ) ;
#46816 = CARTESIAN_POINT ( 'NONE',  ( 0.000000000000000000, 0.5000000000000000000, -10.00000000000000000 ) ) ;
#46817 = FILL_AREA_STYLE ('',( #36869 ) ) ;
#46818 = VECTOR ( 'NONE', #41683, 1000.000000000000000 ) ;
#46819 = DIRECTION ( 'NONE',  ( -0.000000000000000000, -1.000000000000000000, -0.000000000000000000 ) ) ;
#46820 = CARTESIAN_POINT ( 'NONE',  ( -8.000000000000000000, 1.019547802438466100, -3.750000000000000000 ) ) ;
#46821 = CARTESIAN_POINT ( 'NONE',  ( 22.26659068614894466, 23.88708216824730357, 7.082119434687054849 ) ) ;
#46822 = CIRCLE ( 'NONE', #80377, 0.2500000000000002220 ) ;
#46823 = CARTESIAN_POINT ( 'NONE',  ( 0.1532563361054082862, 36.21726448433410894, 2.638427012816831674 ) ) ;
#46824 = FACE_OUTER_BOUND ( 'NONE', #71652, .T. ) ;
#46825 = CARTESIAN_POINT ( 'NONE',  ( 2.917880565312948704, 52.63708216824730357, 12.26659068614894643 ) ) ;
#46826 = CARTESIAN_POINT ( 'NONE',  ( 1.472469842513823179, 20.59226448433411960, -4.923371831947296329 ) ) ;
#46828 = DIRECTION ( 'NONE',  ( 1.000000000000000000, 0.000000000000000000, 0.000000000000000000 ) ) ;
#46827 = DIRECTION ( 'NONE',  ( 0.02617694830786938473, -0.000000000000000000, 0.9996573249755573709 ) ) ;
#46829 = CARTESIAN_POINT ( 'NONE',  ( 10.00000000000000000, 46.81368534415484106, -10.88017736071110342 ) ) ;
#46830 = CARTESIAN_POINT ( 'NONE',  ( 19.38216949554541202, 55.99863466993041072, 9.382169495545424454 ) ) ;
#46831 = CARTESIAN_POINT ( 'NONE',  ( 4.559911319644449179, 17.23035201082150536, -9.422509992056141925 ) ) ;
#46832 = CARTESIAN_POINT ( 'NONE',  ( -2.816281873526473856, 49.33196800326374643, 3.434112377981055619 ) ) ;
#46833 = CARTESIAN_POINT ( 'NONE',  ( 6.565887622018943937, -1.918031996736246692, -12.81628187352647608 ) ) ;
#46834 = PRESENTATION_STYLE_ASSIGNMENT (( #15383 ) ) ;
#46835 = ORIENTED_EDGE ( 'NONE', *, *, #58471, .T. ) ;
#46836 = CARTESIAN_POINT ( 'NONE',  ( -3.750000000000000000, 10.25000000000000000, -4.000000000000000000 ) ) ;
#46837 = CARTESIAN_POINT ( 'NONE',  ( 22.26659068614894466, 53.88708216824731068, 7.082119434687054849 ) ) ;
#46838 = CARTESIAN_POINT ( 'NONE',  ( 22.26659068614894466, 8.887082168247300018, 7.082119434687054849 ) ) ;
#46839 = CARTESIAN_POINT ( 'NONE',  ( 0.5774900079438607392, 13.48035201082150358, 5.440088680355550821 ) ) ;
#46840 = CARTESIAN_POINT ( 'NONE',  ( 4.559911319644449179, 33.89701867748817676, 9.422509992056141925 ) ) ;
#46841 = CARTESIAN_POINT ( 'NONE',  ( 9.820177974736397530, 14.76984956101181368, -11.25994418464053126 ) ) ;
#46842 = CARTESIAN_POINT ( 'NONE',  ( -46.71044717097655763, 100.6858870166936413, -9.426445562487726804 ) ) ;
#46843 = CARTESIAN_POINT ( 'NONE',  ( 4.559911319644449179, 63.89701867748817676, 9.422509992056141925 ) ) ;
#46844 = DIRECTION ( 'NONE',  ( 0.000000000000000000, -1.000000000000000000, 0.000000000000000000 ) ) ;
#46845 = CARTESIAN_POINT ( 'NONE',  ( 19.84674366389459621, 18.50893115100078745, 7.409399052514197653E-17 ) ) ;
#46846 = PLANE ( 'NONE',  #44249 ) ;
#46847 = CARTESIAN_POINT ( 'NONE',  ( 0.000000000000000000, 15.00000000000000000, 0.000000000000000000 ) ) ;
#46848 = CARTESIAN_POINT ( 'NONE',  ( 19.84674366389459621, 8.508931151000785675, 7.409399052514197653E-17 ) ) ;
#46849 = CARTESIAN_POINT ( 'NONE',  ( 17.20831665107776587, 32.88393115100078745, 7.208316651077764980 ) ) ;
#46850 = CARTESIAN_POINT ( 'NONE',  ( 19.42250999205614193, 10.14701867748816966, 5.440088680355555262 ) ) ;
#46851 = EDGE_CURVE ( 'NONE', #33104, #93159, #94392, .T. ) ;
#46852 = CARTESIAN_POINT ( 'NONE',  ( 10.00000000000000000, 32.87363466993042493, -12.81628187352647608 ) ) ;
#46853 = CARTESIAN_POINT ( 'NONE',  ( 14.92337183194729633, 2.675597817667451750, 8.527530157486181039 ) ) ;
#46855 = ADVANCED_FACE ( 'NONE', ( #46007 ), #82019, .T. ) ;
#46854 = CARTESIAN_POINT ( 'NONE',  ( 19.39235739573469530, 54.87576471608601736, 6.499999999999995559 ) ) ;
#46856 = EDGE_CURVE ( 'NONE', #44442, #61653, #27370, .T. ) ;
#46857 = CARTESIAN_POINT ( 'NONE',  ( 14.92337183194729988, 49.34226448433411605, -8.527530157486177487 ) ) ;
#46858 = AXIS2_PLACEMENT_3D ( 'NONE', #70665, #25659, #48139 ) ;
#46860 = CARTESIAN_POINT ( 'NONE',  ( -2.266590686148945544, 1.387082168247301128, -7.082119434687050408 ) ) ;
#46859 = CARTESIAN_POINT ( 'NONE',  ( 0.1532563361054100626, 35.80059781766745175, -2.638427012816831230 ) ) ;
#46861 = CARTESIAN_POINT ( 'NONE',  ( -4.164238869374099039, 21.80374883491396787, 8.674139862899312516E-16 ) ) ;
#46862 = CARTESIAN_POINT ( 'NONE',  ( 7.084665262690076126, 34.10535201082151247, 10.88017736071109987 ) ) ;
#46863 = CARTESIAN_POINT ( 'NONE',  ( 17.96484262340118221, 16.18868534415483396, -7.964842623401177768 ) ) ;
#46864 = AXIS2_PLACEMENT_3D ( 'NONE', #12913, #27910, #50915 ) ;
#46865 = CARTESIAN_POINT ( 'NONE',  ( 17.96484262340118221, 49.93868534415484106, 7.964842623401181321 ) ) ;
#46866 = CARTESIAN_POINT ( 'NONE',  ( 19.42250999205614548, 35.98035201082151247, -5.440088680355545492 ) ) ;
#46867 = VERTEX_POINT ( 'NONE', #76497 ) ;
#46868 = VECTOR ( 'NONE', #95236, 1000.000000000000114 ) ;
#46869 = CARTESIAN_POINT ( 'NONE',  ( 3.591859063236763294, 38.29030133659708923, -11.09922568453595026 ) ) ;
#46870 = CARTESIAN_POINT ( 'NONE',  ( 15.44008868035555793, 41.39701867748817676, -9.422509992056140149 ) ) ;
#46871 = EDGE_CURVE ( 'NONE', #81215, #91132, #33253, .T. ) ;
#46872 = ORIENTED_EDGE ( 'NONE', *, *, #22261, .F. ) ;
#46873 = CARTESIAN_POINT ( 'NONE',  ( -2.816281873526471635, 58.91530133659707502, -3.434112377981056508 ) ) ;
#46874 = CARTESIAN_POINT ( 'NONE',  ( 19.42250999205614548, 50.98035201082151247, -5.440088680355545492 ) ) ;
#46875 = EDGE_LOOP ( 'NONE', ( #7106, #81107, #85543, #39665 ) ) ;
#46876 = CARTESIAN_POINT ( 'NONE',  ( 7.084665262690076126, 44.10535201082151247, 10.88017736071109987 ) ) ;
#46877 = CARTESIAN_POINT ( 'NONE',  ( 1.274849032794317383, 27.55509018479935790, -6.500000000000010658 ) ) ;
#46878 = CARTESIAN_POINT ( 'NONE',  ( 24.16423886937410614, 54.30374883491396787, 8.672049930838204340E-16 ) ) ;
#46879 = CARTESIAN_POINT ( 'NONE',  ( 17.96484262340118221, 59.93868534415484106, 7.964842623401181321 ) ) ;
#46880 = CARTESIAN_POINT ( 'NONE',  ( 19.42250999205614193, 55.14701867748817676, 5.440088680355555262 ) ) ;
#46881 = CYLINDRICAL_SURFACE ( 'NONE', #52500, 15.00000000000000000 ) ;
#46882 = FILL_AREA_STYLE ('',( #15437 ) ) ;
#46883 = CARTESIAN_POINT ( 'NONE',  ( 5.076628168052704559, 30.17559781766745175, -8.527530157486179263 ) ) ;
#46884 = ORIENTED_EDGE ( 'NONE', *, *, #65715, .T. ) ;
#46885 = EDGE_CURVE ( 'NONE', #31483, #48866, #71359, .T. ) ;
#46886 = CARTESIAN_POINT ( 'NONE',  ( 5.076628168052704559, 40.17559781766745175, -8.527530157486179263 ) ) ;
#46887 = CARTESIAN_POINT ( 'NONE',  ( 4.559911319644449179, 38.89701867748817676, 9.422509992056141925 ) ) ;
#46888 = CARTESIAN_POINT ( 'NONE',  ( 0.1532563361054100626, 40.80059781766745886, -2.638427012816831230 ) ) ;
#46889 = CARTESIAN_POINT ( 'NONE',  ( 19.38216949554541557, 22.24863466993041428, -9.382169495545420901 ) ) ;
#46890 = CARTESIAN_POINT ( 'NONE',  ( 12.91533473730992121, 64.52201867748817676, 10.88017736071110164 ) ) ;
#46891 = CARTESIAN_POINT ( 'NONE',  ( 15.44008868035555260, 49.73035201082150536, 9.422509992056143702 ) ) ;
#46892 = CARTESIAN_POINT ( 'NONE',  ( -2.266590686148945544, 56.38708216824731068, -7.082119434687050408 ) ) ;
#46893 = EDGE_CURVE ( 'NONE', #68696, #50677, #64049, .T. ) ;
#46894 = CARTESIAN_POINT ( 'NONE',  ( 13.43411237798105340, 25.58196800326374998, 12.81628187352647963 ) ) ;
#46895 = CARTESIAN_POINT ( 'NONE',  ( -13.21236992757677164, 15.00000000000000000, 5.338143956176621074 ) ) ;
#46896 = ORIENTED_EDGE ( 'NONE', *, *, #71907, .T. ) ;
#46897 = CARTESIAN_POINT ( 'NONE',  ( -2.816281873526471635, 23.91530133659708568, -3.434112377981056508 ) ) ;
#46898 = CARTESIAN_POINT ( 'NONE',  ( 10.00000000000000000, 16.81368534415483751, -10.88017736071110342 ) ) ;
#46899 = ORIENTED_EDGE ( 'NONE', *, *, #35578, .T. ) ;
#46900 = DIRECTION ( 'NONE',  ( 0.5075383629606904368, 0.000000000000000000, 0.8616291604415338146 ) ) ;
#46901 = CARTESIAN_POINT ( 'NONE',  ( 7.361572987183170547, 7.050597817667451750, 9.846743663894590881 ) ) ;
#46902 = CARTESIAN_POINT ( 'NONE',  ( 0.1532563361054082862, 46.21726448433411605, 2.638427012816831674 ) ) ;
#46903 = CARTESIAN_POINT ( 'NONE',  ( 0.1532563361054083140, 41.00893115100078745, 1.131784320476157264E-15 ) ) ;
#46904 = CARTESIAN_POINT ( 'NONE',  ( 0.000000000000000000, 15.00000000000000000, 0.000000000000000000 ) ) ;
#46905 = DIRECTION ( 'NONE',  ( -2.930988785010413267E-14, 0.000000000000000000, 1.000000000000000000 ) ) ;
#46906 = CARTESIAN_POINT ( 'NONE',  ( 18.52753015748618282, 23.92559781766745530, -4.923371831947291888 ) ) ;
#46907 = CARTESIAN_POINT ( 'NONE',  ( 14.94699059465108171, 14.49999999999999112, -1.259949270174796965 ) ) ;
#46908 = DIRECTION ( 'NONE',  ( -0.3007057995042767273, 0.000000000000000000, 0.9537169507482258224 ) ) ;
#46910 = CARTESIAN_POINT ( 'NONE',  ( 12.80781515976314822, -0.03417435944610275333, -6.246788841744324472 ) ) ;
#46909 = CARTESIAN_POINT ( 'NONE',  ( 1.472469842513823179, 11.42559781766745175, 4.923371831947296329 ) ) ;
#46911 = LINE ( 'NONE', #44943, #44140 ) ;
#46913 = ORIENTED_EDGE ( 'NONE', *, *, #8602, .F. ) ;
#46912 = CARTESIAN_POINT ( 'NONE',  ( 10.00000000000000000, 44.75893115100078745, -9.846743663894594434 ) ) ;
#46914 = CARTESIAN_POINT ( 'NONE',  ( 11.12471383767373467, 2.500000000000004885, 1.674288514525068328 ) ) ;
#46915 = CARTESIAN_POINT ( 'NONE',  ( 0.6178305044545818747, 13.49863466993041783, -9.382169495545419124 ) ) ;
#46916 = CIRCLE ( 'NONE', #8604, 4.000000000000001776 ) ;
#46917 = CARTESIAN_POINT ( 'NONE',  ( -0.8801773607111008646, 58.27201867748816966, 2.915334737309923430 ) ) ;
#46918 = CARTESIAN_POINT ( 'NONE',  ( -4.164238869374099927, 52.01208216824729647, 3.795296366450308767 ) ) ;
#46919 = CARTESIAN_POINT ( 'NONE',  ( 2.791683348922240793, 1.633931151000784565, 7.208316651077764092 ) ) ;
#46920 = CARTESIAN_POINT ( 'NONE',  ( 14.35840480524197282, 0.5000000000000004441, 4.340070442838948495 ) ) ;
#46921 = AXIS2_PLACEMENT_3D ( 'NONE', #80140, #3672, #74108 ) ;
#46922 = CARTESIAN_POINT ( 'NONE',  ( 22.26659068614895176, 44.72041550158063927, -7.082119434687042414 ) ) ;
#46923 = CARTESIAN_POINT ( 'NONE',  ( -0.3689425029237898834, 61.17874883491396076, -10.36894250292378850 ) ) ;
#46924 = CARTESIAN_POINT ( 'NONE',  ( 2.917880565312948704, 17.63708216824730357, 12.26659068614894643 ) ) ;
#46926 = CARTESIAN_POINT ( 'NONE',  ( 3.969999999999999751, 9.750000000000000000, -3.750000000000000000 ) ) ;
#46925 = CARTESIAN_POINT ( 'NONE',  ( 20.36894250292379738, 29.92874883491396432, -10.36894250292379027 ) ) ;
#46927 = CARTESIAN_POINT ( 'NONE',  ( 4.903136312256997087, -13.39483660680936339, -3.750000000000000888 ) ) ;
#46929 = CARTESIAN_POINT ( 'NONE',  ( 0.1532563361054100626, 40.80059781766745886, -2.638427012816831230 ) ) ;
#46928 = CARTESIAN_POINT ( 'NONE',  ( -3.420591144908650350, 0.3640475087720806968, 14.60477854057954339 ) ) ;
#46930 = VERTEX_POINT ( 'NONE', #24497 ) ;
#46931 = CARTESIAN_POINT ( 'NONE',  ( 0.5774900079438590739, 42.64701867748816966, -5.440088680355550821 ) ) ;
#46932 = DIRECTION ( 'NONE',  ( -0.000000000000000000, -1.000000000000000000, 0.000000000000000000 ) ) ;
#46933 = FACE_OUTER_BOUND ( 'NONE', #15957, .T. ) ;
#46934 = ADVANCED_FACE ( 'NONE', ( #53990 ), #16990, .T. ) ;
#46935 = CARTESIAN_POINT ( 'NONE',  ( 20.00000000000000711, 90.58866250143879029, -4.971011742375100795 ) ) ;
#46936 = CARTESIAN_POINT ( 'NONE',  ( 10.00000000000000000, 44.75893115100078745, -9.846743663894594434 ) ) ;
#46937 = CARTESIAN_POINT ( 'NONE',  ( 21.09922568453595559, 57.04030133659708923, -6.408140936763230044 ) ) ;
#46938 = CARTESIAN_POINT ( 'NONE',  ( -7.082119434687058401, -9.029584498419360727, -12.26659068614894110 ) ) ;
#46939 = CARTESIAN_POINT ( 'NONE',  ( 5.076628168052703671, 46.84226448433412315, 8.527530157486179263 ) ) ;
#46940 = CARTESIAN_POINT ( 'NONE',  ( 14.92337183194729633, 52.67559781766745175, 8.527530157486181039 ) ) ;
#46941 = CARTESIAN_POINT ( 'NONE',  ( 13.79529636645030344, 38.26208216824729647, 14.16423886937410614 ) ) ;
#46942 = ORIENTED_EDGE ( 'NONE', *, *, #33284, .F. ) ;
#46943 = CARTESIAN_POINT ( 'NONE',  ( 2.917880565312948704, 17.63708216824730357, 12.26659068614894643 ) ) ;
#46944 = LINE ( 'NONE', #984, #56632 ) ;
#46946 = PLANE ( 'NONE',  #88693 ) ;
#46945 = CARTESIAN_POINT ( 'NONE',  ( -0.03932841506541930043, 68.12161441960500952, 6.397827110479001433 ) ) ;
#46947 = CARTESIAN_POINT ( 'NONE',  ( -0.8801773607111009756, 8.063685344154837509, 1.068504757029289695E-15 ) ) ;
#46948 = CARTESIAN_POINT ( 'NONE',  ( -2.816281873526473856, 14.33196800326375531, 3.434112377981055619 ) ) ;
#46949 = DIRECTION ( 'NONE',  ( 0.000000000000000000, -0.000000000000000000, -1.000000000000000000 ) ) ;
#46950 = CARTESIAN_POINT ( 'NONE',  ( 4.559911319644449179, 62.23035201082150536, -9.422509992056141925 ) ) ;
#46951 = CARTESIAN_POINT ( 'NONE',  ( 4.380000000000000782, 0.08775168532224617013, -3.750000000000000000 ) ) ;
#46952 = CARTESIAN_POINT ( 'NONE',  ( -46.94000000000000483, 102.2681967859571870, -7.165875991463089179 ) ) ;
#46953 = FACE_OUTER_BOUND ( 'NONE', #9628, .T. ) ;
#46954 = CARTESIAN_POINT ( 'NONE',  ( 20.36894250292379382, 58.67874883491396076, 10.36894250292379205 ) ) ;
#46955 = DIRECTION ( 'NONE',  ( 0.000000000000000000, 0.000000000000000000, 1.000000000000000000 ) ) ;
#46956 = CARTESIAN_POINT ( 'NONE',  ( -0.8801773607110991993, 22.85535201082150181, -2.915334737309923874 ) ) ;
#46957 = CARTESIAN_POINT ( 'NONE',  ( -0.8801773607110991993, 17.85535201082150536, -2.915334737309923874 ) ) ;
#46958 = CARTESIAN_POINT ( 'NONE',  ( 18.52753015748617571, 53.09226448433412315, 4.923371831947298993 ) ) ;
#46959 = CARTESIAN_POINT ( 'NONE',  ( 7.361572987183169658, 54.96726448433413026, -9.846743663894592657 ) ) ;
#46960 = CARTESIAN_POINT ( 'NONE',  ( -1.099225684535947600, 59.54030133659708923, 6.408140936763237150 ) ) ;
#46961 = DIRECTION ( 'NONE',  ( 0.06975647374410356982, 0.9975640502598257520, -0.000000000000000000 ) ) ;
#46962 = EDGE_CURVE ( 'NONE', #51568, #156, #62961, .T. ) ;
#46963 = VERTEX_POINT ( 'NONE', #25487 ) ;
#46964 = CARTESIAN_POINT ( 'NONE',  ( 0.5774900079438607392, 28.48035201082150891, 5.440088680355550821 ) ) ;
#46965 = CARTESIAN_POINT ( 'NONE',  ( 22.81628187352647785, 31.62363466993042138, 6.195893100308588602E-16 ) ) ;
#46966 = LINE ( 'NONE', #54467, #215 ) ;
#46967 = EDGE_CURVE ( 'NONE', #63997, #32629, #38072, .T. ) ;
#46968 = CARTESIAN_POINT ( 'NONE',  ( 17.20831665107776587, 59.13393115100078745, -7.208316651077762316 ) ) ;
#46969 = CARTESIAN_POINT ( 'NONE',  ( 12.91533473730992121, 44.52201867748816966, 10.88017736071110164 ) ) ;
#46970 = EDGE_CURVE ( 'NONE', #25526, #42104, #51296, .T. ) ;
#46971 = CARTESIAN_POINT ( 'NONE',  ( 10.00000000000000178, 17.25893115100078745, 9.846743663894594434 ) ) ;
#46972 = CARTESIAN_POINT ( 'NONE',  ( 22.81628187352647785, 16.62363466993042138, 6.195893100308588602E-16 ) ) ;
#46974 = CARTESIAN_POINT ( 'NONE',  ( 14.99999999999997868, 80.07179676972448590, 4.250000000000000000 ) ) ;
#46973 = CARTESIAN_POINT ( 'NONE',  ( 19.42250999205614193, 60.14701867748817676, 5.440088680355555262 ) ) ;
#46975 = DIRECTION ( 'NONE',  ( -0.000000000000000000, -1.000000000000000000, -0.000000000000000000 ) ) ;
#46976 = VERTEX_POINT ( 'NONE', #54474 ) ;
#46977 = CARTESIAN_POINT ( 'NONE',  ( -0.8801773607111009756, 48.27201867748816966, 2.915334737309923874 ) ) ;
#46978 = DIRECTION ( 'NONE',  ( -0.000000000000000000, -1.000000000000000000, -0.000000000000000000 ) ) ;
#46979 = CARTESIAN_POINT ( 'NONE',  ( 4.559911319644449179, 47.23035201082150536, -9.422509992056141925 ) ) ;
#46981 = CARTESIAN_POINT ( 'NONE',  ( 2.917880565312950480, 10.97041550158063572, -12.26659068614894821 ) ) ;
#46980 = CARTESIAN_POINT ( 'NONE',  ( 6.565887622018943937, 48.08196800326375353, -12.81628187352647608 ) ) ;
#46982 = CARTESIAN_POINT ( 'NONE',  ( 10.00000000000000000, 19.75893115100078390, -9.846743663894594434 ) ) ;
#46983 = CARTESIAN_POINT ( 'NONE',  ( 0.5774900079438607392, 3.480352010821504027, 5.440088680355550821 ) ) ;
#46984 = CARTESIAN_POINT ( 'NONE',  ( 17.20831665107776587, 14.13393115100078568, -7.208316651077762316 ) ) ;
#46985 = CARTESIAN_POINT ( 'NONE',  ( 19.72487221294571214, 15.71833443783937589, -6.500000000000001776 ) ) ;
#46986 = CARTESIAN_POINT ( 'NONE',  ( -2.266590686148945544, 51.38708216824730357, -7.082119434687050408 ) ) ;
#46987 = VERTEX_POINT ( 'NONE', #9976 ) ;
#46988 = DIRECTION ( 'NONE',  ( -1.000000000000000000, 0.000000000000000000, 0.000000000000000000 ) ) ;
#46989 = CARTESIAN_POINT ( 'NONE',  ( 2.035157376598824452, 8.688685344154839285, 7.964842623401179544 ) ) ;
#46990 = CARTESIAN_POINT ( 'NONE',  ( 1.711636803080549329, 31.84492782695769719, -6.499999999999986677 ) ) ;
#46991 = ORIENTED_EDGE ( 'NONE', *, *, #67143, .F. ) ;
#46992 = CARTESIAN_POINT ( 'NONE',  ( 20.88017736071110519, 10.56368534415483929, 2.639326808657452039E-16 ) ) ;
#46993 = CARTESIAN_POINT ( 'NONE',  ( 20.88017736071110164, 10.35535201082150714, 2.915334737309930979 ) ) ;
#46994 = CARTESIAN_POINT ( 'NONE',  ( 18.52753015748618282, 38.92559781766745175, -4.923371831947291888 ) ) ;
#46995 = CARTESIAN_POINT ( 'NONE',  ( 0.6178305044545818747, 38.49863466993042493, -9.382169495545419124 ) ) ;
#46996 = DIRECTION ( 'NONE',  ( -0.000000000000000000, 0.000000000000000000, 1.000000000000000000 ) ) ;
#46999 = CARTESIAN_POINT ( 'NONE',  ( -0.3689425029237881626, 22.42874883491397142, 10.36894250292379027 ) ) ;
#46998 = CARTESIAN_POINT ( 'NONE',  ( -9.323033696084856103, 14.95037104545394868, -11.43408728005525710 ) ) ;
#46997 = CIRCLE ( 'NONE', #3899, 0.2999999999999999334 ) ;
#47000 = CARTESIAN_POINT ( 'NONE',  ( 0.5774900079438607392, 28.48035201082150891, 5.440088680355550821 ) ) ;
#47001 = CARTESIAN_POINT ( 'NONE',  ( 7.084665262690076126, 2.022018677488171434, -10.88017736071110164 ) ) ;
#47002 = EDGE_CURVE ( 'NONE', #19346, #48651, #40482, .T. ) ;
#47003 = CARTESIAN_POINT ( 'NONE',  ( 19.84674366389459266, 48.30059781766745175, 2.638427012816836559 ) ) ;
#47004 = DIRECTION ( 'NONE',  ( -0.02617694830786282401, 0.000000000000000000, -0.9996573249755575929 ) ) ;
#47005 = CARTESIAN_POINT ( 'NONE',  ( 2.791683348922240793, 31.63393115100078745, 7.208316651077764092 ) ) ;
#47006 = CIRCLE ( 'NONE', #714, 15.00000000000000000 ) ;
#47007 = ADVANCED_FACE ( 'NONE', ( #77469 ), #85212, .T. ) ;
#47008 = CARTESIAN_POINT ( 'NONE',  ( 3.469446951953614189E-15, 27.25893115100078035, 9.846743663894594434 ) ) ;
#47009 = ORIENTED_EDGE ( 'NONE', *, *, #1307, .F. ) ;
#47010 = CARTESIAN_POINT ( 'NONE',  ( 7.084665262690076126, 4.105352010821503583, 10.88017736071109987 ) ) ;
#47011 = CARTESIAN_POINT ( 'NONE',  ( 0.5774900079438590739, 62.64701867748817676, -5.440088680355550821 ) ) ;
#47012 = CARTESIAN_POINT ( 'NONE',  ( 18.52753015748618282, 53.92559781766745175, -4.923371831947291888 ) ) ;
#47013 = CARTESIAN_POINT ( 'NONE',  ( -0.8801773607111008646, 38.27201867748816255, 2.915334737309923430 ) ) ;
#47015 = CARTESIAN_POINT ( 'NONE',  ( 3.591859063236761518, 29.95696800326375708, 11.09922568453594849 ) ) ;
#47014 = CARTESIAN_POINT ( 'NONE',  ( 20.88017736071110519, 10.56368534415483751, 2.639326808657452039E-16 ) ) ;
#47016 = CARTESIAN_POINT ( 'NONE',  ( 6.204703633549690345, 12.84541550158063572, 14.16423886937410082 ) ) ;
#47017 = CARTESIAN_POINT ( 'NONE',  ( 3.591859063236763294, 43.29030133659708923, -11.09922568453595026 ) ) ;
#47018 = EDGE_LOOP ( 'NONE', ( #13418, #56119, #40742, #96954 ) ) ;
#47019 =( BOUNDED_SURFACE ( )  B_SPLINE_SURFACE ( 1, 2, ( 
 ( #68757, #773, #69253, #61722, #44261, #14785, #29262, #288, #45255, #75752, #52753, #46250, #37282, #83261, #21785, #15278, #92237, #8252, #74767, #45759, #7274, #6275, #68272, #31225, #23764, #14283, #75258, #7770, #37775, #76735, #60743, #44756, #38264, #30734, #61241, #36781, #98792, #52265, #23267, #30239, #6771, #91747, #38751, #82761, #53743, #67272, #67772, #98293, #84262, #15764, #97800, #29748, #60257, #90751, #91244, #22768, #53249, #24247, #63687, #93208, #39249, #8731, #16738, #64172, #25720, #10707, #17237, #18213, #85235, #69739, #56212, #78712, #24731, #26198, #70730, #25239, #2738, #47215, #55209, #47715, #39738, #86707, #41222, #54713, #1265, #78210, #77226, #16245, #40221, #85724, #17726, #2245, #77716, #10223, #94693, #32703, #9722, #9229, #63199, #84741, #46727, #70233, #1752, #32207, #62216, #48692, #86215, #92722, #93704, #33675, #33194, #31720, #94190, #55720, #48199, #62708, #40712, #71217, #71699, #79195, #3213, #96177, #88657, #88162, #19676, #65161, #89154, #80174, #95679, #3707, #27660, #5671, #51160, #18704, #58148, #27165, #49188, #12169, #74136, #43651, #57173, #19183, #20165, #57665, #20664, #4693, #87670, #50669, #81157, #12662, #66657, #42674, #95171, #66146, #73153, #49664, #35661, #81644, #34168, #43161, #79690, #11685, #26678, #73647, #5176, #96679, #28158, #72178, #42195, #11188, #34664, #41708, #72659, #58654, #50165, #64658, #4194, #80674, #36153, #13152, #97181, #35155, #56690, #65654, #87183, #68634, #22648, #67654, #69128, #14660, #68145, #45630, #90130, #37158, #60126, #82640, #164, #53617, #97669, #44133, #90624, #21159, #59139, #83135, #98164, #60624, #45126, #29135, #53128, #8134, #75632, #22149, #59639, #52632, #38627, #89647, #21660, #52144, #14158, #6154, #61119, #30119, #36659, #7144, #76617, #76129, #28649, #7655, #37648, #29620, #51660, #82139, #13648, #84135, #67145, #98671, #91125, #83636, #15151, #38149, #74644, #44641, #30613, #91628, #15647, #46129, #75135, #6641, #23144, #16123, #86100, #48080, #62585, #93090, #79075, #56097, #63086, #69615, #55605, #93586, #84619, #24621, #2131, #61601, #86590, #8619, #92115, #660, #63576, #31108, #77106, #70605, #9601, #17610, #39128, #62094, #92602, #55087, #2625, #18099, #85108, #70111, #85607, #17122, #48576, #23646, #40602, #10588, #41100, #9108, #47604, #71099, #24126, #94086, #78593, #10105, #33080, #54106, #32591, #39622, #1137, #46607, #31599, #25605, #1636, #54595, #16619, #78099, #47095, #77593, #32087, #40104, #25123, #5060, #64547, #64058, #73533, #50550, #34542, #50058, #58535, #41599, #13038, #80061, #94570 ),
 ( #89043, #20554, #72067, #34051, #73041, #42083, #35545, #19562, #3592, #4576, #65539, #27545, #81532, #27052, #11079, #81045, #57550, #95054, #12552, #66036, #49076, #35037, #26089, #26563, #57060, #96062, #42557, #58039, #43055, #87074, #87561, #56584, #49549, #18583, #19071, #96565, #11565, #79578, #72546, #4079, #51039, #28040, #71596, #65037, #95563, #88049, #80562, #12056, #3108, #33562, #88547, #20048, #67535, #60014, #53, #43535, #83521, #30500, #84012, #52034, #98050, #15039, #36546, #7539, #60512, #22535, #45511, #5560, #14542, #82527, #44023, #97067, #61002, #91004, #14043, #51538, #59033, #37037, #74029, #67035, #97557, #53006, #22044, #76011, #29018, #36036, #38031, #68522, #6528, #52519, #91513, #13539, #66539, #44524, #28539, #89538, #75023, #74526, #23030, #21048, #82029, #37538, #7032, #53502, #6047, #59528, #90021, #21543, #29506, #90509, #83026, #68027, #45012, #75517, #98555, #30006, #10844, #48339, #78842, #71356, #86842, #33803, #57310, #94821, #46017, #25850, #72309, #2875, #41843, #10353, #2382, #94330, #64310, #85860, #33324, #86350, #32836, #40852, #8020, #18346, #63338, #24873, #34299, #79335, #47842, #41365, #17853, #17372, #56347, #26325, #63819, #48824, #95315, #3840, #71832, #78345, #3341, #56822, #546, #87321, #18838, #76506, #64797, #55355, #38517, #15535, #79822, #69015, #93348, #49318, #11324, #26817, #32347, #62850, #9867, #40365, #70866, #93843, #25370, #55855, #12308, #65294, #21299, #89297, #95821, #73789, #36796, #36295, #67290, #66792, #35799, #88801, #19323, #49807, #11815, #13795, #27301, #66286, #28297, #20808, #58790, #81781, #34805, #72796, #96821, #43782, #74785, #44281, #97818, #87802, #20311, #4335, #74275, #50809, #81300, #96325, #51791, #42816, #27798, #57802, #51295, #29279, #82278, #80315, #13296, #58283, #42322, #43295, #6294, #88309, #19807, #50297, #5803, #12795, #80810, #97312, #73300, #28785, #59283, #89782, #4824, #5320, #35298, #65791, #45778, #90772, #38768, #54246, #37302, #23286, #52283, #52770, #29765, #84279, #30751, #61258, #69270, #75277, #14803, #14301, #37792, #82781, #98311, #790, #68289, #44772, #6788, #22296, #39269, #31243, #84758, #91262, #92257, #60273, #67789, #61739, #53764, #98810, #1286, #76270, #307, #76752, #83278, #30259, #22788, #45275, #23780, #16264, #75770, #7291, #53266, #60762, #90268, #15296, #83772, #91764, #7787, #38282, #15779, #69758, #68777, #46268, #8271, #46747, #77243, #8750, #59775, #21802, #62727, #11209, #71719, #56711, #63220, #64193, #32226, #54730, #3230, #25741, #70752, #72198, #17744, #71235, #48712, #93227, #40242 ) ),
 .UNSPECIFIED., .F., .F., .F. ) 
 B_SPLINE_SURFACE_WITH_KNOTS ( ( 2, 2 ),
 ( 3, 2, 2, 2, 2, 2, 2, 2, 2, 2, 2, 2, 2, 2, 2, 2, 2, 2, 2, 2, 2, 2, 2, 2, 2, 2, 2, 2, 2, 2, 2, 2, 2, 2, 2, 2, 2, 2, 2, 2, 2, 2, 2, 2, 2, 2, 2, 2, 2, 2, 2, 2, 2, 2, 2, 2, 2, 2, 2, 2, 2, 2, 2, 2, 2, 2, 2, 2, 2, 2, 2, 2, 2, 2, 2, 2, 2, 2, 2, 2, 2, 2, 2, 2, 2, 2, 2, 2, 2, 2, 2, 2, 2, 2, 2, 2, 2, 2, 2, 2, 2, 2, 2, 2, 2, 2, 2, 2, 2, 2, 2, 2, 2, 2, 2, 2, 2, 2, 2, 2, 2, 2, 2, 2, 2, 2, 2, 2, 2, 2, 2, 2, 2, 2, 2, 2, 2, 2, 2, 2, 2, 2, 2, 2, 2, 2, 2, 2, 2, 2, 2, 2, 2, 2, 2, 2, 2, 2, 2, 2, 2, 2, 3 ),
 ( 0.000000000000000000, 1.000000000000000000 ),
 ( 0.000000000000000000, 0.005952380952380952051, 0.01190476190476190410, 0.01785714285714285615, 0.02380952380952380820, 0.02976190476190476025, 0.03571428571428571230, 0.04166666666666666435, 0.04761904761904761640, 0.05357142857142856845, 0.05952380952380952051, 0.06547619047619047949, 0.07142857142857142461, 0.07738095238095238360, 0.08333333333333332871, 0.08928571428571428770, 0.09523809523809523281, 0.1011904761904761918, 0.1071428571428571369, 0.1130952380952380959, 0.1190476190476190410, 0.1250000000000000000, 0.1309523809523809590, 0.1369047619047619180, 0.1428571428571428492, 0.1488095238095238082, 0.1547619047619047672, 0.1607142857142857262, 0.1666666666666666574, 0.1726190476190476164, 0.1785714285714285754, 0.1845238095238095344, 0.1904761904761904656, 0.1964285714285714246, 0.2023809523809523836, 0.2083333333333333426, 0.2142857142857142738, 0.2202380952380952328, 0.2261904761904761918, 0.2321428571428571508, 0.2380952380952380820, 0.2440476190476190410, 0.2500000000000000000, 0.2559523809523809312, 0.2619047619047619180, 0.2678571428571428492, 0.2738095238095238360, 0.2797619047619047672, 0.2857142857142856984, 0.2916666666666666852, 0.2976190476190476164, 0.3035714285714285476, 0.3095238095238095344, 0.3154761904761904656, 0.3214285714285714524, 0.3273809523809523836, 0.3333333333333333148, 0.3392857142857143016, 0.3452380952380952328, 0.3511904761904761640, 0.3571428571428571508, 0.3630952380952380820, 0.3690476190476190688, 0.3750000000000000000, 0.3809523809523809312, 0.3869047619047619180, 0.3928571428571428492, 0.3988095238095238360, 0.4047619047619047672, 0.4107142857142856984, 0.4166666666666666852, 0.4226190476190476164, 0.4285714285714285476, 0.4345238095238095344, 0.4404761904761904656, 0.4464285714285714524, 0.4523809523809523836, 0.4583333333333333148, 0.4642857142857143016, 0.4702380952380952328, 0.4761904761904761640, 0.4821428571428571508, 0.4880952380952380820, 0.4940476190476190688, 0.5000000000000000000, 0.5059523809523809312, 0.5119047619047618625, 0.5178571428571429047, 0.5238095238095238360, 0.5297619047619047672, 0.5357142857142856984, 0.5416666666666666297, 0.5476190476190476719, 0.5535714285714286031, 0.5595238095238095344, 0.5654761904761904656, 0.5714285714285713969, 0.5773809523809523281, 0.5833333333333333703, 0.5892857142857143016, 0.5952380952380952328, 0.6011904761904761640, 0.6071428571428570953, 0.6130952380952381375, 0.6190476190476190688, 0.6250000000000000000, 0.6309523809523809312, 0.6369047619047618625, 0.6428571428571429047, 0.6488095238095238360, 0.6547619047619047672, 0.6607142857142856984, 0.6666666666666666297, 0.6726190476190476719, 0.6785714285714286031, 0.6845238095238095344, 0.6904761904761904656, 0.6964285714285713969, 0.7023809523809523281, 0.7083333333333333703, 0.7142857142857143016, 0.7202380952380952328, 0.7261904761904761640, 0.7321428571428570953, 0.7380952380952381375, 0.7440476190476190688, 0.7500000000000000000, 0.7559523809523809312, 0.7619047619047618625, 0.7678571428571429047, 0.7738095238095238360, 0.7797619047619047672, 0.7857142857142856984, 0.7916666666666666297, 0.7976190476190476719, 0.8035714285714286031, 0.8095238095238095344, 0.8154761904761904656, 0.8214285714285713969, 0.8273809523809523281, 0.8333333333333333703, 0.8392857142857143016, 0.8452380952380952328, 0.8511904761904761640, 0.8571428571428570953, 0.8630952380952381375, 0.8690476190476190688, 0.8750000000000000000, 0.8809523809523809312, 0.8869047619047618625, 0.8928571428571429047, 0.8988095238095238360, 0.9047619047619047672, 0.9107142857142856984, 0.9166666666666666297, 0.9226190476190476719, 0.9285714285714286031, 0.9345238095238095344, 0.9404761904761904656, 0.9464285714285713969, 0.9523809523809523281, 0.9583333333333333703, 0.9642857142857143016 ),
 .UNSPECIFIED. ) 
 GEOMETRIC_REPRESENTATION_ITEM ( )  RATIONAL_B_SPLINE_SURFACE ( (
 ( 1.000000000000000000, 0.9659258262890683122, 1.000000000000000000, 0.9659258262890683122, 1.000000000000000000, 0.9659258262890683122, 1.000000000000000000, 0.9659258262890683122, 1.000000000000000000, 0.9659258262890683122, 1.000000000000000000, 0.9659258262890683122, 1.000000000000000000, 0.9659258262890683122, 1.000000000000000000, 0.9659258262890683122, 1.000000000000000000, 0.9659258262890683122, 1.000000000000000000, 0.9659258262890683122, 1.000000000000000000, 0.9659258262890683122, 1.000000000000000000, 0.9659258262890683122, 1.000000000000000000, 0.9659258262890683122, 1.000000000000000000, 0.9659258262890683122, 1.000000000000000000, 0.9659258262890683122, 1.000000000000000000, 0.9659258262890683122, 1.000000000000000000, 0.9659258262890683122, 1.000000000000000000, 0.9659258262890683122, 1.000000000000000000, 0.9659258262890683122, 1.000000000000000000, 0.9659258262890683122, 1.000000000000000000, 0.9659258262890683122, 1.000000000000000000, 0.9659258262890683122, 1.000000000000000000, 0.9659258262890683122, 1.000000000000000000, 0.9659258262890683122, 1.000000000000000000, 0.9659258262890683122, 1.000000000000000000, 0.9659258262890683122, 1.000000000000000000, 0.9659258262890683122, 1.000000000000000000, 0.9659258262890683122, 1.000000000000000000, 0.9659258262890683122, 1.000000000000000000, 0.9659258262890683122, 1.000000000000000000, 0.9659258262890683122, 1.000000000000000000, 0.9659258262890683122, 1.000000000000000000, 0.9659258262890683122, 1.000000000000000000, 0.9659258262890683122, 1.000000000000000000, 0.9659258262890683122, 1.000000000000000000, 0.9659258262890683122, 1.000000000000000000, 0.9659258262890683122, 1.000000000000000000, 0.9659258262890683122, 1.000000000000000000, 0.9659258262890683122, 1.000000000000000000, 0.9659258262890683122, 1.000000000000000000, 0.9659258262890683122, 1.000000000000000000, 0.9659258262890683122, 1.000000000000000000, 0.9659258262890683122, 1.000000000000000000, 0.9659258262890683122, 1.000000000000000000, 0.9659258262890683122, 1.000000000000000000, 0.9659258262890683122, 1.000000000000000000, 0.9659258262890683122, 1.000000000000000000, 0.9659258262890683122, 1.000000000000000000, 0.9659258262890683122, 1.000000000000000000, 0.9659258262890683122, 1.000000000000000000, 0.9659258262890683122, 1.000000000000000000, 0.9659258262890683122, 1.000000000000000000, 0.9659258262890683122, 1.000000000000000000, 0.9659258262890683122, 1.000000000000000000, 0.9659258262890683122, 1.000000000000000000, 0.9659258262890683122, 1.000000000000000000, 0.9659258262890683122, 1.000000000000000000, 0.9659258262890683122, 1.000000000000000000, 0.9659258262890683122, 1.000000000000000000, 0.9659258262890683122, 1.000000000000000000, 0.9659258262890683122, 1.000000000000000000, 0.9659258262890683122, 1.000000000000000000, 0.9659258262890683122, 1.000000000000000000, 0.9659258262890683122, 1.000000000000000000, 0.9659258262890683122, 1.000000000000000000, 0.9659258262890683122, 1.000000000000000000, 0.9659258262890683122, 1.000000000000000000, 0.9659258262890683122, 1.000000000000000000, 0.9659258262890683122, 1.000000000000000000, 0.9659258262890683122, 1.000000000000000000, 0.9659258262890683122, 1.000000000000000000, 0.9659258262890683122, 1.000000000000000000, 0.9659258262890683122, 1.000000000000000000, 0.9659258262890683122, 1.000000000000000000, 0.9659258262890683122, 1.000000000000000000, 0.9659258262890683122, 1.000000000000000000, 0.9659258262890683122, 1.000000000000000000, 0.9659258262890683122, 1.000000000000000000, 0.9659258262890683122, 1.000000000000000000, 0.9659258262890683122, 1.000000000000000000, 0.9659258262890683122, 1.000000000000000000, 0.9659258262890683122, 1.000000000000000000, 0.9659258262890683122, 1.000000000000000000, 0.9659258262890683122, 1.000000000000000000, 0.9659258262890683122, 1.000000000000000000, 0.9659258262890683122, 1.000000000000000000, 0.9659258262890683122, 1.000000000000000000, 0.9659258262890683122, 1.000000000000000000, 0.9659258262890683122, 1.000000000000000000, 0.9659258262890683122, 1.000000000000000000, 0.9659258262890683122, 1.000000000000000000, 0.9659258262890683122, 1.000000000000000000, 0.9659258262890683122, 1.000000000000000000, 0.9659258262890683122, 1.000000000000000000, 0.9659258262890683122, 1.000000000000000000, 0.9659258262890683122, 1.000000000000000000, 0.9659258262890683122, 1.000000000000000000, 0.9659258262890683122, 1.000000000000000000, 0.9659258262890683122, 1.000000000000000000, 0.9659258262890683122, 1.000000000000000000, 0.9659258262890683122, 1.000000000000000000, 0.9659258262890683122, 1.000000000000000000, 0.9659258262890683122, 1.000000000000000000, 0.9659258262890683122, 1.000000000000000000, 0.9659258262890683122, 1.000000000000000000, 0.9659258262890683122, 1.000000000000000000, 0.9659258262890683122, 1.000000000000000000, 0.9659258262890683122, 1.000000000000000000, 0.9659258262890683122, 1.000000000000000000, 0.9659258262890683122, 1.000000000000000000, 0.9659258262890683122, 1.000000000000000000, 0.9659258262890683122, 1.000000000000000000, 0.9659258262890683122, 1.000000000000000000, 0.9659258262890683122, 1.000000000000000000, 0.9659258262890683122, 1.000000000000000000, 0.9659258262890683122, 1.000000000000000000, 0.9659258262890683122, 1.000000000000000000, 0.9659258262890683122, 1.000000000000000000, 0.9659258262890683122, 1.000000000000000000, 0.9659258262890683122, 1.000000000000000000, 0.9659258262890683122, 1.000000000000000000, 0.9659258262890683122, 1.000000000000000000, 0.9659258262890683122, 1.000000000000000000, 0.9659258262890683122, 1.000000000000000000, 0.9659258262890683122, 1.000000000000000000, 0.9659258262890683122, 1.000000000000000000, 0.9659258262890683122, 1.000000000000000000, 0.9659258262890683122, 1.000000000000000000, 0.9659258262890683122, 1.000000000000000000, 0.9659258262890683122, 1.000000000000000000, 0.9659258262890683122, 1.000000000000000000, 0.9659258262890683122, 1.000000000000000000, 0.9659258262890683122, 1.000000000000000000, 0.9659258262890683122, 1.000000000000000000, 0.9659258262890683122, 1.000000000000000000, 0.9659258262890683122, 1.000000000000000000, 0.9659258262890683122, 1.000000000000000000, 0.9659258262890683122, 1.000000000000000000, 0.9659258262890683122, 1.000000000000000000, 0.9659258262890683122, 1.000000000000000000, 0.9659258262890683122, 1.000000000000000000, 0.9659258262890683122, 1.000000000000000000, 0.9659258262890683122, 1.000000000000000000, 0.9659258262890683122, 1.000000000000000000, 0.9659258262890683122, 1.000000000000000000, 0.9659258262890683122, 1.000000000000000000, 0.9659258262890683122, 1.000000000000000000, 0.9659258262890683122, 1.000000000000000000, 0.9659258262890683122, 1.000000000000000000, 0.9659258262890683122, 1.000000000000000000, 0.9659258262890683122, 1.000000000000000000, 0.9659258262890683122, 1.000000000000000000, 0.9659258262890683122, 1.000000000000000000, 0.9659258262890683122, 1.000000000000000000, 0.9659258262890683122, 1.000000000000000000, 0.9659258262890683122, 1.000000000000000000, 0.9659258262890683122, 1.000000000000000000, 0.9659258262890683122, 1.000000000000000000, 0.9659258262890683122, 1.000000000000000000, 0.9659258262890683122, 1.000000000000000000, 0.9659258262890683122, 1.000000000000000000, 0.9659258262890683122, 1.000000000000000000),
 ( 1.000000000000000000, 0.9659258262890683122, 1.000000000000000000, 0.9659258262890683122, 1.000000000000000000, 0.9659258262890683122, 1.000000000000000000, 0.9659258262890683122, 1.000000000000000000, 0.9659258262890683122, 1.000000000000000000, 0.9659258262890683122, 1.000000000000000000, 0.9659258262890683122, 1.000000000000000000, 0.9659258262890683122, 1.000000000000000000, 0.9659258262890683122, 1.000000000000000000, 0.9659258262890683122, 1.000000000000000000, 0.9659258262890683122, 1.000000000000000000, 0.9659258262890683122, 1.000000000000000000, 0.9659258262890683122, 1.000000000000000000, 0.9659258262890683122, 1.000000000000000000, 0.9659258262890683122, 1.000000000000000000, 0.9659258262890683122, 1.000000000000000000, 0.9659258262890683122, 1.000000000000000000, 0.9659258262890683122, 1.000000000000000000, 0.9659258262890683122, 1.000000000000000000, 0.9659258262890683122, 1.000000000000000000, 0.9659258262890683122, 1.000000000000000000, 0.9659258262890683122, 1.000000000000000000, 0.9659258262890683122, 1.000000000000000000, 0.9659258262890683122, 1.000000000000000000, 0.9659258262890683122, 1.000000000000000000, 0.9659258262890683122, 1.000000000000000000, 0.9659258262890683122, 1.000000000000000000, 0.9659258262890683122, 1.000000000000000000, 0.9659258262890683122, 1.000000000000000000, 0.9659258262890683122, 1.000000000000000000, 0.9659258262890683122, 1.000000000000000000, 0.9659258262890683122, 1.000000000000000000, 0.9659258262890683122, 1.000000000000000000, 0.9659258262890683122, 1.000000000000000000, 0.9659258262890683122, 1.000000000000000000, 0.9659258262890683122, 1.000000000000000000, 0.9659258262890683122, 1.000000000000000000, 0.9659258262890683122, 1.000000000000000000, 0.9659258262890683122, 1.000000000000000000, 0.9659258262890683122, 1.000000000000000000, 0.9659258262890683122, 1.000000000000000000, 0.9659258262890683122, 1.000000000000000000, 0.9659258262890683122, 1.000000000000000000, 0.9659258262890683122, 1.000000000000000000, 0.9659258262890683122, 1.000000000000000000, 0.9659258262890683122, 1.000000000000000000, 0.9659258262890683122, 1.000000000000000000, 0.9659258262890683122, 1.000000000000000000, 0.9659258262890683122, 1.000000000000000000, 0.9659258262890683122, 1.000000000000000000, 0.9659258262890683122, 1.000000000000000000, 0.9659258262890683122, 1.000000000000000000, 0.9659258262890683122, 1.000000000000000000, 0.9659258262890683122, 1.000000000000000000, 0.9659258262890683122, 1.000000000000000000, 0.9659258262890683122, 1.000000000000000000, 0.9659258262890683122, 1.000000000000000000, 0.9659258262890683122, 1.000000000000000000, 0.9659258262890683122, 1.000000000000000000, 0.9659258262890683122, 1.000000000000000000, 0.9659258262890683122, 1.000000000000000000, 0.9659258262890683122, 1.000000000000000000, 0.9659258262890683122, 1.000000000000000000, 0.9659258262890683122, 1.000000000000000000, 0.9659258262890683122, 1.000000000000000000, 0.9659258262890683122, 1.000000000000000000, 0.9659258262890683122, 1.000000000000000000, 0.9659258262890683122, 1.000000000000000000, 0.9659258262890683122, 1.000000000000000000, 0.9659258262890683122, 1.000000000000000000, 0.9659258262890683122, 1.000000000000000000, 0.9659258262890683122, 1.000000000000000000, 0.9659258262890683122, 1.000000000000000000, 0.9659258262890683122, 1.000000000000000000, 0.9659258262890683122, 1.000000000000000000, 0.9659258262890683122, 1.000000000000000000, 0.9659258262890683122, 1.000000000000000000, 0.9659258262890683122, 1.000000000000000000, 0.9659258262890683122, 1.000000000000000000, 0.9659258262890683122, 1.000000000000000000, 0.9659258262890683122, 1.000000000000000000, 0.9659258262890683122, 1.000000000000000000, 0.9659258262890683122, 1.000000000000000000, 0.9659258262890683122, 1.000000000000000000, 0.9659258262890683122, 1.000000000000000000, 0.9659258262890683122, 1.000000000000000000, 0.9659258262890683122, 1.000000000000000000, 0.9659258262890683122, 1.000000000000000000, 0.9659258262890683122, 1.000000000000000000, 0.9659258262890683122, 1.000000000000000000, 0.9659258262890683122, 1.000000000000000000, 0.9659258262890683122, 1.000000000000000000, 0.9659258262890683122, 1.000000000000000000, 0.9659258262890683122, 1.000000000000000000, 0.9659258262890683122, 1.000000000000000000, 0.9659258262890683122, 1.000000000000000000, 0.9659258262890683122, 1.000000000000000000, 0.9659258262890683122, 1.000000000000000000, 0.9659258262890683122, 1.000000000000000000, 0.9659258262890683122, 1.000000000000000000, 0.9659258262890683122, 1.000000000000000000, 0.9659258262890683122, 1.000000000000000000, 0.9659258262890683122, 1.000000000000000000, 0.9659258262890683122, 1.000000000000000000, 0.9659258262890683122, 1.000000000000000000, 0.9659258262890683122, 1.000000000000000000, 0.9659258262890683122, 1.000000000000000000, 0.9659258262890683122, 1.000000000000000000, 0.9659258262890683122, 1.000000000000000000, 0.9659258262890683122, 1.000000000000000000, 0.9659258262890683122, 1.000000000000000000, 0.9659258262890683122, 1.000000000000000000, 0.9659258262890683122, 1.000000000000000000, 0.9659258262890683122, 1.000000000000000000, 0.9659258262890683122, 1.000000000000000000, 0.9659258262890683122, 1.000000000000000000, 0.9659258262890683122, 1.000000000000000000, 0.9659258262890683122, 1.000000000000000000, 0.9659258262890683122, 1.000000000000000000, 0.9659258262890683122, 1.000000000000000000, 0.9659258262890683122, 1.000000000000000000, 0.9659258262890683122, 1.000000000000000000, 0.9659258262890683122, 1.000000000000000000, 0.9659258262890683122, 1.000000000000000000, 0.9659258262890683122, 1.000000000000000000, 0.9659258262890683122, 1.000000000000000000, 0.9659258262890683122, 1.000000000000000000, 0.9659258262890683122, 1.000000000000000000, 0.9659258262890683122, 1.000000000000000000, 0.9659258262890683122, 1.000000000000000000, 0.9659258262890683122, 1.000000000000000000, 0.9659258262890683122, 1.000000000000000000, 0.9659258262890683122, 1.000000000000000000, 0.9659258262890683122, 1.000000000000000000, 0.9659258262890683122, 1.000000000000000000, 0.9659258262890683122, 1.000000000000000000, 0.9659258262890683122, 1.000000000000000000, 0.9659258262890683122, 1.000000000000000000, 0.9659258262890683122, 1.000000000000000000, 0.9659258262890683122, 1.000000000000000000, 0.9659258262890683122, 1.000000000000000000, 0.9659258262890683122, 1.000000000000000000, 0.9659258262890683122, 1.000000000000000000, 0.9659258262890683122, 1.000000000000000000, 0.9659258262890683122, 1.000000000000000000, 0.9659258262890683122, 1.000000000000000000, 0.9659258262890683122, 1.000000000000000000, 0.9659258262890683122, 1.000000000000000000, 0.9659258262890683122, 1.000000000000000000, 0.9659258262890683122, 1.000000000000000000, 0.9659258262890683122, 1.000000000000000000, 0.9659258262890683122, 1.000000000000000000, 0.9659258262890683122, 1.000000000000000000, 0.9659258262890683122, 1.000000000000000000, 0.9659258262890683122, 1.000000000000000000, 0.9659258262890683122, 1.000000000000000000, 0.9659258262890683122, 1.000000000000000000, 0.9659258262890683122, 1.000000000000000000, 0.9659258262890683122, 1.000000000000000000, 0.9659258262890683122, 1.000000000000000000, 0.9659258262890683122, 1.000000000000000000, 0.9659258262890683122, 1.000000000000000000) ) ) 
 REPRESENTATION_ITEM ( '' )  SURFACE ( )  );
#47020 = CARTESIAN_POINT ( 'NONE',  ( 18.52753015748618282, 53.92559781766745175, -4.923371831947291888 ) ) ;
#47021 = CARTESIAN_POINT ( 'NONE',  ( 19.42250999205614193, 15.14701867748817143, 5.440088680355555262 ) ) ;
#47022 = ORIENTED_EDGE ( 'NONE', *, *, #15600, .F. ) ;
#47023 = CARTESIAN_POINT ( 'NONE',  ( 20.88017736071110164, 10.35535201082150714, 2.915334737309930979 ) ) ;
#47024 = VERTEX_POINT ( 'NONE', #65433 ) ;
#47025 = CARTESIAN_POINT ( 'NONE',  ( 10.00000000000000178, 64.31368534415483396, 10.88017736071110342 ) ) ;
#47026 = CARTESIAN_POINT ( 'NONE',  ( -0.8801773607111009756, 68.06368534415484817, 1.068504757029289695E-15 ) ) ;
#47027 = CARTESIAN_POINT ( 'NONE',  ( 10.00000000000000000, 4.758931151000784787, -9.846743663894594434 ) ) ;
#47028 = CARTESIAN_POINT ( 'NONE',  ( -0.8801773607111009756, 68.06368534415484817, 1.068504757029289695E-15 ) ) ;
#47029 = FILL_AREA_STYLE ('',( #31533 ) ) ;
#47030 = AXIS2_PLACEMENT_3D ( 'NONE', #17254, #54727, #78727 ) ;
#47032 = ORIENTED_EDGE ( 'NONE', *, *, #14001, .F. ) ;
#47031 = CARTESIAN_POINT ( 'NONE',  ( 18.52753015748618282, 3.925597817667451306, -4.923371831947291888 ) ) ;
#47033 = CARTESIAN_POINT ( 'NONE',  ( 19.84674366389459266, 38.71726448433412315, -2.638427012816827677 ) ) ;
#47034 = VERTEX_POINT ( 'NONE', #65928 ) ;
#47035 = ORIENTED_EDGE ( 'NONE', *, *, #25575, .T. ) ;
#47036 = DIRECTION ( 'NONE',  ( -1.000000000000000000, 0.000000000000000000, 0.000000000000000000 ) ) ;
#47037 = CARTESIAN_POINT ( 'NONE',  ( 17.08211943468705130, 3.470415501580634388, 12.26659068614894998 ) ) ;
#47038 = CARTESIAN_POINT ( 'NONE',  ( 0.6178305044545838731, 59.74863466993041783, 9.382169495545420901 ) ) ;
#47039 = CARTESIAN_POINT ( 'NONE',  ( 22.26659068614895176, 9.720415501580633943, -7.082119434687042414 ) ) ;
#47040 = CARTESIAN_POINT ( 'NONE',  ( 22.26659068614894466, 13.88708216824730179, 7.082119434687054849 ) ) ;
#47041 = CARTESIAN_POINT ( 'NONE',  ( -0.1503990784575328643, 70.00000000000000000, -6.262539305110068177 ) ) ;
#47042 = LINE ( 'NONE', #62043, #91332 ) ;
#47043 = CARTESIAN_POINT ( 'NONE',  ( 15.44008868035555793, 21.39701867748817321, -9.422509992056140149 ) ) ;
#47044 = FILL_AREA_STYLE_COLOUR ( '', #37096 ) ;
#47045 = EDGE_LOOP ( 'NONE', ( #16045, #46187, #14664, #23508 ) ) ;
#47046 = SURFACE_SIDE_STYLE ('',( #6594 ) ) ;
#47047 = AXIS2_PLACEMENT_3D ( 'NONE', #23982, #63434, #69473 ) ;
#47048 = CARTESIAN_POINT ( 'NONE',  ( 2.791683348922237240, 0.3839311510007847872, -7.208316651077763204 ) ) ;
#47049 = CARTESIAN_POINT ( 'NONE',  ( 10.00000000000000178, 30.37363466993042138, 12.81628187352647608 ) ) ;
#47050 = CARTESIAN_POINT ( 'NONE',  ( 1.472469842513823179, 30.59226448433411960, -4.923371831947296329 ) ) ;
#47051 = ADVANCED_FACE ( 'NONE', ( #13937 ), #35927, .F. ) ;
#47052 = CARTESIAN_POINT ( 'NONE',  ( 6.565887622018943937, 13.08196800326374998, -12.81628187352647608 ) ) ;
#47053 = CARTESIAN_POINT ( 'NONE',  ( 15.00000000000000000, 77.07179676972447169, -4.000000000000000000 ) ) ;
#47054 = CARTESIAN_POINT ( 'NONE',  ( 0.1532563361054083140, 6.008931151000784787, 1.131784320476157264E-15 ) ) ;
#47055 = COLOUR_RGB ( '', 0.09019608, 0.27058824, 0.51372549) ;
#47056 = ORIENTED_EDGE ( 'NONE', *, *, #64090, .F. ) ;
#47057 = EDGE_LOOP ( 'NONE', ( #29847, #56308, #72217, #74701 ) ) ;
#47058 = CARTESIAN_POINT ( 'NONE',  ( 10.00000000000000000, 41.81368534415484106, -10.88017736071110342 ) ) ;
#47059 = CARTESIAN_POINT ( 'NONE',  ( -4.164238869374099927, 27.01208216824730357, 3.795296366450308767 ) ) ;
#47060 = CARTESIAN_POINT ( 'NONE',  ( 5.076628168052703671, 36.84226448433412315, 8.527530157486179263 ) ) ;
#47061 = CARTESIAN_POINT ( 'NONE',  ( 12.63842701281683034, 2.467264484334118269, 9.846743663894596210 ) ) ;
#47063 = CARTESIAN_POINT ( 'NONE',  ( -6.757332319902496387, -55.97232334539076959, -3.750000000000000000 ) ) ;
#47062 = CARTESIAN_POINT ( 'NONE',  ( -2.816281873526473856, 59.33196800326374643, 3.434112377981055619 ) ) ;
#47064 = CARTESIAN_POINT ( 'NONE',  ( 4.559911319644449179, 32.23035201082150536, -9.422509992056141925 ) ) ;
#47065 =( LENGTH_UNIT ( ) NAMED_UNIT ( * ) SI_UNIT ( .MILLI., .METRE. ) );
#47066 = CARTESIAN_POINT ( 'NONE',  ( 21.09922568453595559, 17.04030133659708923, -6.408140936763230044 ) ) ;
#47067 = CARTESIAN_POINT ( 'NONE',  ( -2.816281873526471635, 3.915301336597087456, -3.434112377981056508 ) ) ;
#47068 = CARTESIAN_POINT ( 'NONE',  ( 0.1532563361054083140, 41.00893115100078745, 1.131784320476157264E-15 ) ) ;
#47069 = CARTESIAN_POINT ( 'NONE',  ( -5.440088680355547268, 3.897018677488178540, 9.422509992056143702 ) ) ;
#47070 = CARTESIAN_POINT ( 'NONE',  ( 22.81628187352647785, 51.41530133659708923, 3.434112377981063169 ) ) ;
#47071 = PRESENTATION_LAYER_ASSIGNMENT (  '', '', ( #45431 ) ) ;
#47072 =( LENGTH_UNIT ( ) NAMED_UNIT ( * ) SI_UNIT ( .MILLI., .METRE. ) );
#47074 = DIRECTION ( 'NONE',  ( 0.000000000000000000, -0.000000000000000000, 1.000000000000000000 ) ) ;
#47073 = CARTESIAN_POINT ( 'NONE',  ( 19.42250999205614548, 55.98035201082150536, -5.440088680355545492 ) ) ;
#47075 = CARTESIAN_POINT ( 'NONE',  ( -7.909656208964993773, -4.175824794491008518, 4.000000000000000000 ) ) ;
#47076 = DIRECTION ( 'NONE',  ( 0.7716245833877107829, 0.000000000000000000, 0.6360782202777751637 ) ) ;
#47077 = CARTESIAN_POINT ( 'NONE',  ( 0.5774900079438607392, 48.48035201082150536, 5.440088680355550821 ) ) ;
#47078 = CARTESIAN_POINT ( 'NONE',  ( 4.559911319644449179, 63.89701867748817676, 9.422509992056141925 ) ) ;
#47079 = CARTESIAN_POINT ( 'NONE',  ( 20.03743638938529870, 56.75197528031016958, 6.399506433553887597 ) ) ;
#47080 = EDGE_CURVE ( 'NONE', #35357, #35809, #60990, .T. ) ;
#47081 = AXIS2_PLACEMENT_3D ( 'NONE', #46346, #54324, #869 ) ;
#47082 = CARTESIAN_POINT ( 'NONE',  ( -7.264509831664514472, 0.2301509507469247651, -13.05561747642799375 ) ) ;
#47083 = CARTESIAN_POINT ( 'NONE',  ( 12.91533473730993009, 6.605352010821504471, -10.88017736071109987 ) ) ;
#47084 = ADVANCED_FACE ( 'NONE', ( #29404 ), #92215, .T. ) ;
#47085 = CARTESIAN_POINT ( 'NONE',  ( 19.84674366389459621, 48.50893115100078745, 7.409399052514197653E-17 ) ) ;
#47086 = CARTESIAN_POINT ( 'NONE',  ( 4.559911319644449179, 22.23035201082150536, -9.422509992056141925 ) ) ;
#47087 = CARTESIAN_POINT ( 'NONE',  ( -2.816281873526473856, 24.12363466993042138, 9.499525473075851096E-16 ) ) ;
#47088 = ORIENTED_EDGE ( 'NONE', *, *, #68466, .F. ) ;
#47089 = CARTESIAN_POINT ( 'NONE',  ( 4.559911319644449179, 33.89701867748817676, 9.422509992056141925 ) ) ;
#47090 = CARTESIAN_POINT ( 'NONE',  ( 22.81628187352647785, 11.41530133659708390, 3.434112377981063169 ) ) ;
#47091 = CARTESIAN_POINT ( 'NONE',  ( -0.8801773607111008646, 8.272018677488171434, 2.915334737309923430 ) ) ;
#47092 = CARTESIAN_POINT ( 'NONE',  ( 10.00000000000000000, 36.81368534415484106, -10.88017736071110342 ) ) ;
#47093 = CARTESIAN_POINT ( 'NONE',  ( -4.164238869374098151, 56.59541550158063927, -3.795296366450310543 ) ) ;
#47094 = CARTESIAN_POINT ( 'NONE',  ( 1.472469842513823179, 26.42559781766745175, 4.923371831947296329 ) ) ;
#47095 = CARTESIAN_POINT ( 'NONE',  ( 19.42250999205614548, 65.98035201082151957, -5.440088680355545492 ) ) ;
#47096 = CARTESIAN_POINT ( 'NONE',  ( 0.2751277870542908621, 32.28217586085237656, -6.499999999999992006 ) ) ;
#47097 = CARTESIAN_POINT ( 'NONE',  ( -0.3689425029237881626, 12.42874883491396609, 10.36894250292379027 ) ) ;
#47098 = AXIS2_PLACEMENT_3D ( 'NONE', #85741, #53759, #47730 ) ;
#47099 =( LENGTH_UNIT ( ) NAMED_UNIT ( * ) SI_UNIT ( .MILLI., .METRE. ) );
#47100 = CARTESIAN_POINT ( 'NONE',  ( 1.821708436314933843, 21.66792564121896092, -6.500000000000008882 ) ) ;
#47101 = ORIENTED_EDGE ( 'NONE', *, *, #80278, .T. ) ;
#47102 = ORIENTED_EDGE ( 'NONE', *, *, #32000, .F. ) ;
#47103 = CARTESIAN_POINT ( 'NONE',  ( 24.16423886937409904, 39.09541550158062506, 3.795296366450317205 ) ) ;
#47104 = CARTESIAN_POINT ( 'NONE',  ( 10.00000000000000000, 30.55374883491397142, -14.16423886937410082 ) ) ;
#47105 = CARTESIAN_POINT ( 'NONE',  ( 10.00000000000000178, 69.31368534415484817, 10.88017736071110342 ) ) ;
#47106 = CARTESIAN_POINT ( 'NONE',  ( 19.84674366389459266, 58.71726448433411605, -2.638427012816827677 ) ) ;
#47107 = FACE_OUTER_BOUND ( 'NONE', #10996, .T. ) ;
#47109 = CARTESIAN_POINT ( 'NONE',  ( 13.43411237798106583, 22.66530133659708923, -12.81628187352647252 ) ) ;
#47108 = CARTESIAN_POINT ( 'NONE',  ( 15.44008868035555793, 56.39701867748817676, -9.422509992056140149 ) ) ;
#47110 = CARTESIAN_POINT ( 'NONE',  ( 20.36894250292379738, 34.92874883491396076, -10.36894250292379027 ) ) ;
#47111 = CARTESIAN_POINT ( 'NONE',  ( 20.88017736071110875, 30.77201867748816966, -2.915334737309920765 ) ) ;
#47112 = CARTESIAN_POINT ( 'NONE',  ( -0.8801773607110991993, 27.85535201082150181, -2.915334737309923874 ) ) ;
#47113 = CARTESIAN_POINT ( 'NONE',  ( -3.999999999999994671, 43.00000000000000711, -6.250000000000000000 ) ) ;
#47114 = CARTESIAN_POINT ( 'NONE',  ( 17.96484262340118221, 54.93868534415484106, 7.964842623401181321 ) ) ;
#47115 = CARTESIAN_POINT ( 'NONE',  ( 9.846743663894594434, -16.49106884899920900, -2.168404344971008868E-15 ) ) ;
#47116 = ORIENTED_EDGE ( 'NONE', *, *, #32860, .T. ) ;
#47117 = DIRECTION ( 'NONE',  ( 0.8870108331782213806, 0.000000000000000000, -0.4617486132350345773 ) ) ;
#47118 = CARTESIAN_POINT ( 'NONE',  ( -3.750000000000000000, 37.00000000000000000, 3.750000000000000000 ) ) ;
#47119 = ORIENTED_EDGE ( 'NONE', *, *, #68527, .T. ) ;
#47121 = CARTESIAN_POINT ( 'NONE',  ( 20.36894250292379738, 64.92874883491397497, -10.36894250292379027 ) ) ;
#47120 = CARTESIAN_POINT ( 'NONE',  ( 10.00000000000000178, 63.05374883491396076, 14.16423886937410082 ) ) ;
#47123 = CARTESIAN_POINT ( 'NONE',  ( 10.00000000000000000, 54.75893115100078745, -9.846743663894594434 ) ) ;
#47122 = CARTESIAN_POINT ( 'NONE',  ( 1.472469842513823179, 41.42559781766745886, 4.923371831947296329 ) ) ;
#47124 = CARTESIAN_POINT ( 'NONE',  ( 20.32896413005680358, 59.74545670184114243, 5.963430220938287007 ) ) ;
#47125 = DIRECTION ( 'NONE',  ( -0.000000000000000000, 0.000000000000000000, 1.000000000000000000 ) ) ;
#47126 = B_SPLINE_CURVE_WITH_KNOTS ( 'NONE', 3,
 ( #32522, #33978, #11010, #2555, #56028, #55535 ),
 .UNSPECIFIED., .F., .F.,
 ( 4, 2, 4 ),
 ( 0.0002800808511812512844, 0.0006862868719359046989, 0.001092492892690558005 ),
 .UNSPECIFIED. ) ;
#47128 = CARTESIAN_POINT ( 'NONE',  ( 3.591859063236763294, 8.290301336597087456, -11.09922568453595026 ) ) ;
#47127 = AXIS2_PLACEMENT_3D ( 'NONE', #62784, #74208, #96750 ) ;
#47129 = CARTESIAN_POINT ( 'NONE',  ( -6.408140936763232709, 29.95696800326377840, 11.09922568453595026 ) ) ;
#47130 = ORIENTED_EDGE ( 'NONE', *, *, #10761, .T. ) ;
#47131 = CARTESIAN_POINT ( 'NONE',  ( 2.917880565312950480, 50.97041550158064638, -12.26659068614894821 ) ) ;
#47132 = ORIENTED_EDGE ( 'NONE', *, *, #44628, .T. ) ;
#47133 = CARTESIAN_POINT ( 'NONE',  ( 10.00000000000000000, 40.55374883491397497, -14.16423886937410082 ) ) ;
#47134 = ORIENTED_EDGE ( 'NONE', *, *, #43799, .F. ) ;
#47135 = CARTESIAN_POINT ( 'NONE',  ( 15.44008868035555260, 19.73035201082150536, 9.422509992056143702 ) ) ;
#47136 = CARTESIAN_POINT ( 'NONE',  ( -0.4278561937608865717, 0.000000000000000000, 5.436428395565740423 ) ) ;
#47137 = CARTESIAN_POINT ( 'NONE',  ( -0.8801773607111009756, 43.06368534415484106, 1.068504757029289695E-15 ) ) ;
#47138 = CARTESIAN_POINT ( 'NONE',  ( 17.20831665107776587, 44.13393115100078745, -7.208316651077762316 ) ) ;
#47139 = CARTESIAN_POINT ( 'NONE',  ( 20.88017736071110164, 40.35535201082150536, 2.915334737309930979 ) ) ;
#47140 = CARTESIAN_POINT ( 'NONE',  ( 14.97687855664614531, 14.49999999999999112, -0.8325315005900779664 ) ) ;
#47141 = CARTESIAN_POINT ( 'NONE',  ( 19.42250999205614548, 65.98035201082151957, -5.440088680355545492 ) ) ;
#47142 = CARTESIAN_POINT ( 'NONE',  ( 20.88017736071110164, 25.35535201082150891, 2.915334737309930979 ) ) ;
#47143 = CARTESIAN_POINT ( 'NONE',  ( 0.3093388210927641713, 0.3627605259888580513, -14.99680997725065978 ) ) ;
#47144 = AXIS2_PLACEMENT_3D ( 'NONE', #13470, #43951, #58460 ) ;
#47145 = CARTESIAN_POINT ( 'NONE',  ( 1.472469842513823179, 1.425597817667451528, 4.923371831947296329 ) ) ;
#47146 = CARTESIAN_POINT ( 'NONE',  ( -3.770608837274703973, -6.399801140530443355, 2.500000000000806910 ) ) ;
#47147 = ORIENTED_EDGE ( 'NONE', *, *, #21041, .T. ) ;
#47148 = CARTESIAN_POINT ( 'NONE',  ( 0.2751277870542967463, 70.00000000000000000, -6.500000000000000888 ) ) ;
#47149 = CARTESIAN_POINT ( 'NONE',  ( 18.52753015748617571, 28.09226448433411960, 4.923371831947298993 ) ) ;
#47150 = FACE_OUTER_BOUND ( 'NONE', #82185, .T. ) ;
#47151 = LINE ( 'NONE', #69677, #37963 ) ;
#47152 = ORIENTED_EDGE ( 'NONE', *, *, #70361, .T. ) ;
#47153 = CARTESIAN_POINT ( 'NONE',  ( 14.15281240980447031, -3.205596188883898450E-15, -3.688687068602698016 ) ) ;
#47154 = CARTESIAN_POINT ( 'NONE',  ( -42.16485527613926365, 107.5383484153110061, 5.000000000000000888 ) ) ;
#47155 = CARTESIAN_POINT ( 'NONE',  ( 2.791683348922237240, 50.38393115100078035, -7.208316651077763204 ) ) ;
#47156 = CARTESIAN_POINT ( 'NONE',  ( 13.79529636645030344, 48.26208216824728936, 14.16423886937410614 ) ) ;
#47157 = CARTESIAN_POINT ( 'NONE',  ( 12.63842701281683922, 59.55059781766744464, -9.846743663894590881 ) ) ;
#47158 = LINE ( 'NONE', #77662, #12852 ) ;
#47159 = CARTESIAN_POINT ( 'NONE',  ( 18.52753015748618282, 13.92559781766745175, -4.923371831947291888 ) ) ;
#47160 = CARTESIAN_POINT ( 'NONE',  ( -1.099225684535947600, 54.54030133659708923, 6.408140936763237150 ) ) ;
#47161 = CARTESIAN_POINT ( 'NONE',  ( 19.84674366389459621, 58.50893115100078745, 7.409399052514197653E-17 ) ) ;
#47162 = CARTESIAN_POINT ( 'NONE',  ( 15.44008868035555793, 56.39701867748817676, -9.422509992056140149 ) ) ;
#47163 = EDGE_CURVE ( 'NONE', #69512, #23460, #27450, .T. ) ;
#47164 = CARTESIAN_POINT ( 'NONE',  ( 18.52753015748618282, 48.92559781766745886, -4.923371831947291888 ) ) ;
#47165 = CARTESIAN_POINT ( 'NONE',  ( 18.72515096720568195, 31.07228050351032422, -6.500000000000018652 ) ) ;
#47166 =( GEOMETRIC_REPRESENTATION_CONTEXT ( 3 ) GLOBAL_UNCERTAINTY_ASSIGNED_CONTEXT ( ( #33313 ) ) GLOBAL_UNIT_ASSIGNED_CONTEXT ( ( #81747, #28262, #21265 ) ) REPRESENTATION_CONTEXT ( 'NONE', 'WORKASPACE' ) );
#47167 = B_SPLINE_CURVE_WITH_KNOTS ( 'NONE', 3,
 ( #55682, #17692, #64137, #2706, #94159, #48657 ),
 .UNSPECIFIED., .F., .F.,
 ( 4, 2, 4 ),
 ( 0.0002800245631444417513, 0.0006862300328522872098, 0.001092435502560132722 ),
 .UNSPECIFIED. ) ;
#47168 = ORIENTED_EDGE ( 'NONE', *, *, #2304, .F. ) ;
#47169 = CARTESIAN_POINT ( 'NONE',  ( 20.36894250292379738, 54.92874883491396076, -10.36894250292379027 ) ) ;
#47170 = CARTESIAN_POINT ( 'NONE',  ( 0.000000000000000000, 14.49999999999999822, 0.000000000000000000 ) ) ;
#47171 = CARTESIAN_POINT ( 'NONE',  ( 0.5774900079438590739, 27.64701867748817676, -5.440088680355550821 ) ) ;
#47173 = CARTESIAN_POINT ( 'NONE',  ( 0.5774900079438590739, 62.64701867748817676, -5.440088680355550821 ) ) ;
#47172 = CARTESIAN_POINT ( 'NONE',  ( 21.09922568453594849, 11.20696800326375531, 6.408140936763242479 ) ) ;
#47174 = CARTESIAN_POINT ( 'NONE',  ( -12.60589901313210071, 15.00000000000000000, -8.129656208642224158 ) ) ;
#47175 = FILL_AREA_STYLE_COLOUR ( '', #57129 ) ;
#47176 = DIRECTION ( 'NONE',  ( -0.9848077530122086864, -0.1736481776669272781, 0.000000000000000000 ) ) ;
#47178 = CARTESIAN_POINT ( 'NONE',  ( 2.603489959281582777, 31.58210964143329136, 6.499999999999995559 ) ) ;
#47177 = CARTESIAN_POINT ( 'NONE',  ( 4.559911319644449179, 53.89701867748817676, 9.422509992056141925 ) ) ;
#47179 = CARTESIAN_POINT ( 'NONE',  ( 5.076628168052704559, 40.17559781766745175, -8.527530157486179263 ) ) ;
#47180 = CARTESIAN_POINT ( 'NONE',  ( 2.791683348922237240, 0.3839311510007847872, -7.208316651077763204 ) ) ;
#47181 = CARTESIAN_POINT ( 'NONE',  ( -14.16423886937409726, 32.01208216824730357, 3.795296366450320757 ) ) ;
#47182 = CARTESIAN_POINT ( 'NONE',  ( 10.00000000000000000, 12.87363466993042138, -12.81628187352647608 ) ) ;
#47184 =( LENGTH_UNIT ( ) NAMED_UNIT ( * ) SI_UNIT ( .MILLI., .METRE. ) );
#47183 = CARTESIAN_POINT ( 'NONE',  ( 19.42250999205614548, 15.98035201082150714, -5.440088680355545492 ) ) ;
#47185 = CARTESIAN_POINT ( 'NONE',  ( -14.40939250469964783, 15.00000000000000000, 1.618458416365647023 ) ) ;
#47186 = CARTESIAN_POINT ( 'NONE',  ( 22.26659068614894466, 38.88708216824731068, 7.082119434687054849 ) ) ;
#47187 = CARTESIAN_POINT ( 'NONE',  ( 17.08211943468705130, 58.47041550158063927, 12.26659068614894998 ) ) ;
#47188 = AXIS2_PLACEMENT_3D ( 'NONE', #47484, #10964, #94456 ) ;
#47189 = CARTESIAN_POINT ( 'NONE',  ( 19.84674366389459266, 28.71726448433411960, -2.638427012816827677 ) ) ;
#47190 = CARTESIAN_POINT ( 'NONE',  ( 7.361572987183169658, 19.96726448433411960, -9.846743663894592657 ) ) ;
#47191 = CARTESIAN_POINT ( 'NONE',  ( 15.44008868035555260, 14.73035201082150536, 9.422509992056143702 ) ) ;
#47192 = AXIS2_PLACEMENT_3D ( 'NONE', #48403, #1948, #16934 ) ;
#47193 = ORIENTED_EDGE ( 'NONE', *, *, #38922, .T. ) ;
#47194 = CARTESIAN_POINT ( 'NONE',  ( 10.00000000000000000, 34.75893115100078745, -9.846743663894594434 ) ) ;
#47195 = EDGE_CURVE ( 'NONE', #93468, #2418, #369, .T. ) ;
#47196 = CARTESIAN_POINT ( 'NONE',  ( -0.8801773607111009756, 23.06368534415484106, 1.068504757029289695E-15 ) ) ;
#47197 = CARTESIAN_POINT ( 'NONE',  ( 1.472469842513823179, 55.59226448433412315, -4.923371831947296329 ) ) ;
#47199 = DIRECTION ( 'NONE',  ( -0.6626200482157305061, 0.000000000000000000, -0.7489557207890082946 ) ) ;
#47198 = CARTESIAN_POINT ( 'NONE',  ( 22.26659068614895176, 4.720415501580633943, -7.082119434687042414 ) ) ;
#47200 = CARTESIAN_POINT ( 'NONE',  ( 14.88232117145535760, 14.49999999999999112, 1.875237731503272887 ) ) ;
#47201 = AXIS2_PLACEMENT_3D ( 'NONE', #98029, #20530, #52985 ) ;
#47202 = UNCERTAINTY_MEASURE_WITH_UNIT (LENGTH_MEASURE( 1.000000000000000082E-05 ), #78487, 'distance_accuracy_value', 'NONE');
#47203 = CARTESIAN_POINT ( 'NONE',  ( 0.1532563361054100626, 5.800597817667452638, -2.638427012816831230 ) ) ;
#47204 = CARTESIAN_POINT ( 'NONE',  ( 21.09922568453594849, 56.20696800326375353, 6.408140936763242479 ) ) ;
#47205 = CARTESIAN_POINT ( 'NONE',  ( 5.076628168052703671, 56.84226448433412315, 8.527530157486179263 ) ) ;
#47206 = VERTEX_POINT ( 'NONE', #68414 ) ;
#47207 = CARTESIAN_POINT ( 'NONE',  ( 19.84674366389459266, 18.30059781766745175, 2.638427012816836559 ) ) ;
#47208 = CARTESIAN_POINT ( 'NONE',  ( 1.707155281725204476, 12.90189080397283483, 6.499999999999992006 ) ) ;
#47209 = DIRECTION ( 'NONE',  ( 0.000000000000000000, 0.000000000000000000, 1.000000000000000000 ) ) ;
#47210 = CARTESIAN_POINT ( 'NONE',  ( 6.204703633549690345, 67.84541550158060375, 14.16423886937410082 ) ) ;
#47211 = CARTESIAN_POINT ( 'NONE',  ( 10.00000000000000000, 51.81368534415484106, -10.88017736071110342 ) ) ;
#47212 = CARTESIAN_POINT ( 'NONE',  ( 0.04758788293968784638, 0.000000000000000000, 5.453031268574421553 ) ) ;
#47213 = CARTESIAN_POINT ( 'NONE',  ( 0.5774900079438590739, 52.64701867748817676, -5.440088680355550821 ) ) ;
#47214 = CARTESIAN_POINT ( 'NONE',  ( 5.076628168052703671, 36.84226448433412315, 8.527530157486179263 ) ) ;
#47215 = CARTESIAN_POINT ( 'NONE',  ( -0.8801773607110991993, 17.85535201082150536, -2.915334737309923874 ) ) ;
#47216 = CARTESIAN_POINT ( 'NONE',  ( -10.58981376305275468, 0.000000000000000000, -9.535111140613857117 ) ) ;
#47217 = CARTESIAN_POINT ( 'NONE',  ( 10.00000000000000178, 62.25893115100078745, 9.846743663894594434 ) ) ;
#47218 = ORIENTED_EDGE ( 'NONE', *, *, #95142, .T. ) ;
#47219 = ORIENTED_EDGE ( 'NONE', *, *, #72949, .T. ) ;
#47220 = LINE ( 'NONE', #46736, #2283 ) ;
#47221 = AXIS2_PLACEMENT_3D ( 'NONE', #36749, #91209, #8223 ) ;
#47222 = CARTESIAN_POINT ( 'NONE',  ( -10.77730536144846596, -98.63085534186639336, 3.750000000000000000 ) ) ;
#47223 = CARTESIAN_POINT ( 'NONE',  ( 19.84674366389459266, 38.30059781766745175, 2.638427012816836559 ) ) ;
#47224 = CARTESIAN_POINT ( 'NONE',  ( 14.92337183194729633, 22.67559781766745175, 8.527530157486181039 ) ) ;
#47225 = CARTESIAN_POINT ( 'NONE',  ( 10.00000000000000178, 60.37363466993041783, 12.81628187352647608 ) ) ;
#47227 = CARTESIAN_POINT ( 'NONE',  ( 0.1532563361054100626, 45.80059781766745886, -2.638427012816831230 ) ) ;
#47226 = CARTESIAN_POINT ( 'NONE',  ( 10.00000000000000178, 19.31368534415484106, 10.88017736071110342 ) ) ;
#47228 = CARTESIAN_POINT ( 'NONE',  ( -1.926860441876564023, 34.68830936912750929, 1.004413902775740781E-15 ) ) ;
#47229 = CARTESIAN_POINT ( 'NONE',  ( -0.3689425029237898834, 46.17874883491397497, -10.36894250292378850 ) ) ;
#47230 = CARTESIAN_POINT ( 'NONE',  ( 24.16423886937410614, 59.51208216824728936, -3.795296366450302550 ) ) ;
#47231 = CARTESIAN_POINT ( 'NONE',  ( -45.94000000000001194, 103.9981609152045650, -5.961202730336927047 ) ) ;
#47232 = CARTESIAN_POINT ( 'NONE',  ( 2.148416515056654763, 67.23726573380442062, 6.500000000000004441 ) ) ;
#47233 = CARTESIAN_POINT ( 'NONE',  ( 7.084665262690076126, 47.02201867748818387, -10.88017736071110164 ) ) ;
#47234 = B_SPLINE_CURVE_WITH_KNOTS ( 'NONE', 3,
 ( #7841, #68832, #364, #10782, #3284, #32778 ),
 .UNSPECIFIED., .F., .F.,
 ( 4, 2, 4 ),
 ( 3.409110551496121881E-05, 0.0004400426677367866800, 0.0008459942299586121345 ),
 .UNSPECIFIED. ) ;
#47235 = CARTESIAN_POINT ( 'NONE',  ( 7.361572987183170547, 17.05059781766745530, 9.846743663894590881 ) ) ;
#47236 = CARTESIAN_POINT ( 'NONE',  ( -6.982525766850296023, -88.11956318484570261, 4.000000000000000000 ) ) ;
#47237 = ADVANCED_FACE ( 'NONE', ( #31376 ), #98441, .F. ) ;
#47238 = ORIENTED_EDGE ( 'NONE', *, *, #95076, .F. ) ;
#47239 = CARTESIAN_POINT ( 'NONE',  ( 20.32896413005680714, 30.57879003517447103, -5.963430220938276349 ) ) ;
#47240 = VERTEX_POINT ( 'NONE', #31862 ) ;
#47241 = CARTESIAN_POINT ( 'NONE',  ( 0.1532563361054082862, 6.217264484334118713, 2.638427012816831674 ) ) ;
#47242 = ORIENTED_EDGE ( 'NONE', *, *, #90792, .T. ) ;
#47243 = PRESENTATION_LAYER_ASSIGNMENT (  '', '', ( #24859 ) ) ;
#47244 = CARTESIAN_POINT ( 'NONE',  ( 20.36894250292379382, 13.67874883491396965, 10.36894250292379205 ) ) ;
#47245 = CARTESIAN_POINT ( 'NONE',  ( 17.20831665107776587, 14.13393115100078568, -7.208316651077762316 ) ) ;
#47246 = CARTESIAN_POINT ( 'NONE',  ( 4.559911319644449179, 43.89701867748816966, 9.422509992056141925 ) ) ;
#47247 = ADVANCED_FACE ( 'NONE', ( #46394 ), #84885, .F. ) ;
#47248 = SURFACE_STYLE_FILL_AREA ( #3742 ) ;
#47249 = ORIENTED_EDGE ( 'NONE', *, *, #45293, .T. ) ;
#47250 = CARTESIAN_POINT ( 'NONE',  ( 12.91533473730993009, 46.60535201082150536, -10.88017736071109987 ) ) ;
#47251 = EDGE_LOOP ( 'NONE', ( #12770, #51867, #31607, #78217 ) ) ;
#47252 = CARTESIAN_POINT ( 'NONE',  ( 17.08211943468705130, 8.470415501580635720, 12.26659068614894998 ) ) ;
#47253 = VERTEX_POINT ( 'NONE', #25863 ) ;
#47254 = EDGE_CURVE ( 'NONE', #29544, #11914, #56360, .T. ) ;
#47255 = ORIENTED_EDGE ( 'NONE', *, *, #42921, .T. ) ;
#47256 = CARTESIAN_POINT ( 'NONE',  ( 22.81628187352647785, 21.41530133659708923, 3.434112377981063169 ) ) ;
#47257 = CARTESIAN_POINT ( 'NONE',  ( 10.00000000000000178, 7.258931151000785675, 9.846743663894594434 ) ) ;
#47258 = CARTESIAN_POINT ( 'NONE',  ( 20.88017736071110875, 5.772018677488170546, -2.915334737309920765 ) ) ;
#47259 = CARTESIAN_POINT ( 'NONE',  ( 1.915564264621337776, 15.00000000000000000, 14.37291249357991774 ) ) ;
#47260 = CARTESIAN_POINT ( 'NONE',  ( 17.20831665107776587, 12.88393115100078390, 7.208316651077764980 ) ) ;
#47261 = CARTESIAN_POINT ( 'NONE',  ( 19.42250999205614193, 35.14701867748816966, 5.440088680355555262 ) ) ;
#47262 = AXIS2_PLACEMENT_3D ( 'NONE', #51423, #65428, #95952 ) ;
#47263 = ORIENTED_EDGE ( 'NONE', *, *, #47583, .F. ) ;
#47264 = ORIENTED_EDGE ( 'NONE', *, *, #27686, .T. ) ;
#47265 = CARTESIAN_POINT ( 'NONE',  ( 22.81628187352647785, 61.41530133659709634, 3.434112377981063169 ) ) ;
#47266 = CARTESIAN_POINT ( 'NONE',  ( 7.084665262690076126, 62.02201867748816966, -10.88017736071110164 ) ) ;
#47267 = CARTESIAN_POINT ( 'NONE',  ( -42.50369195530268485, 107.9060299417078426, 4.500000000000000888 ) ) ;
#47268 = CIRCLE ( 'NONE', #32927, 1.500000000000001332 ) ;
#47269 = CARTESIAN_POINT ( 'NONE',  ( 8.629999999999995453, 40.99999999999999289, -6.250000000000000000 ) ) ;
#47270 = CARTESIAN_POINT ( 'NONE',  ( 0.5774900079438590739, 67.64701867748817676, -5.440088680355550821 ) ) ;
#47271 = CARTESIAN_POINT ( 'NONE',  ( 13.43411237798106583, 12.66530133659708746, -12.81628187352647252 ) ) ;
#47272 = DIRECTION ( 'NONE',  ( 0.000000000000000000, 0.000000000000000000, -1.000000000000000000 ) ) ;
#47273 = CARTESIAN_POINT ( 'NONE',  ( 17.20831665107776587, 27.88393115100078390, 7.208316651077764980 ) ) ;
#47274 = CARTESIAN_POINT ( 'NONE',  ( 16.40814093676324603, 52.45696800326375353, -11.09922568453594671 ) ) ;
#47275 = CARTESIAN_POINT ( 'NONE',  ( 20.36894250292379382, 3.678748834913967869, 10.36894250292379205 ) ) ;
#47276 = CARTESIAN_POINT ( 'NONE',  ( 18.52753015748617571, 13.09226448433411960, 4.923371831947298993 ) ) ;
#47277 = CARTESIAN_POINT ( 'NONE',  ( -1.099225684535947600, 24.54030133659708923, 6.408140936763237150 ) ) ;
#47279 = DIRECTION ( 'NONE',  ( -0.000000000000000000, -0.000000000000000000, -1.000000000000000000 ) ) ;
#47278 = FILL_AREA_STYLE ('',( #86280 ) ) ;
#47280 = CARTESIAN_POINT ( 'NONE',  ( 10.00000000000000000, 51.81368534415484106, -10.88017736071110342 ) ) ;
#47281 = CARTESIAN_POINT ( 'NONE',  ( 19.84674366389459266, 63.30059781766745886, 2.638427012816836559 ) ) ;
#47282 = CARTESIAN_POINT ( 'NONE',  ( 1.472469842513823179, 31.42559781766745530, 4.923371831947296329 ) ) ;
#47283 = CARTESIAN_POINT ( 'NONE',  ( 7.361572987183170547, 27.05059781766745175, 9.846743663894590881 ) ) ;
#47284 = CARTESIAN_POINT ( 'NONE',  ( -0.8801773607111008646, 8.272018677488171434, 2.915334737309923430 ) ) ;
#47285 = ADVANCED_FACE ( 'NONE', ( #41378 ), #23131, .T. ) ;
#47286 = CARTESIAN_POINT ( 'NONE',  ( 19.38216949554541557, 22.24863466993041428, -9.382169495545420901 ) ) ;
#47287 = CARTESIAN_POINT ( 'NONE',  ( 17.20831665107776587, 24.13393115100078035, -7.208316651077762316 ) ) ;
#47288 =( NAMED_UNIT ( * ) SI_UNIT ( $, .STERADIAN. ) SOLID_ANGLE_UNIT ( ) );
#47289 = CARTESIAN_POINT ( 'NONE',  ( -8.004790597918161055, 84.51838969325523010, 3.750000002001242283 ) ) ;
#47291 = ADVANCED_FACE ( 'NONE', ( #13824 ), #43808, .F. ) ;
#47290 = CARTESIAN_POINT ( 'NONE',  ( -0.8801773607111009756, 13.06368534415483929, 1.068504757029289695E-15 ) ) ;
#47292 = CARTESIAN_POINT ( 'NONE',  ( 5.817157072110800797, 0.5000000000000004441, -13.82608706751086558 ) ) ;
#47294 = CARTESIAN_POINT ( 'NONE',  ( 7.084665262690076126, 14.10535201082150358, 10.88017736071109987 ) ) ;
#47293 = CARTESIAN_POINT ( 'NONE',  ( 19.84674366389459266, 48.71726448433413026, -2.638427012816827677 ) ) ;
#47295 = CARTESIAN_POINT ( 'NONE',  ( 15.44008868035555260, 29.73035201082150891, 9.422509992056143702 ) ) ;
#47296 = CARTESIAN_POINT ( 'NONE',  ( 20.88017736071110164, 15.35535201082150358, 2.915334737309930979 ) ) ;
#47297 = CARTESIAN_POINT ( 'NONE',  ( 5.076628168052704559, 20.17559781766745175, -8.527530157486179263 ) ) ;
#47298 = CARTESIAN_POINT ( 'NONE',  ( 10.00000000000000000, 44.75893115100078745, -9.846743663894594434 ) ) ;
#47299 = EDGE_CURVE ( 'NONE', #18731, #58682, #14150, .T. ) ;
#47300 = DIRECTION ( 'NONE',  ( -0.9366721892483995671, 0.000000000000000000, 0.3502073812594621027 ) ) ;
#47301 = CIRCLE ( 'NONE', #26542, 14.49999999999999822 ) ;
#47302 = DIRECTION ( 'NONE',  ( 0.000000000000000000, 0.000000000000000000, 1.000000000000000000 ) ) ;
#47303 = FILL_AREA_STYLE_COLOUR ( '', #66565 ) ;
#47304 = CARTESIAN_POINT ( 'NONE',  ( -7.750000000000000000, 1.019547802438466100, -4.000000000000000000 ) ) ;
#47305 = CARTESIAN_POINT ( 'NONE',  ( -2.266590686148945544, 21.38708216824730357, -7.082119434687050408 ) ) ;
#47306 = CARTESIAN_POINT ( 'NONE',  ( 12.63842701281683034, 37.46726448433411605, 9.846743663894596210 ) ) ;
#47307 = CARTESIAN_POINT ( 'NONE',  ( 1.274849032794199255, 23.57228050351030646, 6.499999999999850786 ) ) ;
#47308 = B_SPLINE_CURVE_WITH_KNOTS ( 'NONE', 3,
 ( #70915, #32893, #2925, #69927, #18892, #78397 ),
 .UNSPECIFIED., .F., .F.,
 ( 4, 2, 4 ),
 ( 3.409110551496121881E-05, 0.0004400426677367872763, 0.0008459942299586133271 ),
 .UNSPECIFIED. ) ;
#47309 = EDGE_CURVE ( 'NONE', #76280, #43600, #57829, .T. ) ;
#47310 = CARTESIAN_POINT ( 'NONE',  ( -4.164238869374098151, 51.59541550158063217, -3.795296366450310543 ) ) ;
#47311 = CARTESIAN_POINT ( 'NONE',  ( 5.076628168052703671, 16.84226448433411960, 8.527530157486179263 ) ) ;
#47312 = CARTESIAN_POINT ( 'NONE',  ( 6.879999999999995453, 43.00000000000000000, -6.250000000000000000 ) ) ;
#47313 = CARTESIAN_POINT ( 'NONE',  ( 17.96484262340118221, 41.18868534415484106, -7.964842623401177768 ) ) ;
#47314 = CARTESIAN_POINT ( 'NONE',  ( 3.420591144908486481, 14.49999999999999112, 14.60477854057964109 ) ) ;
#47315 =( GEOMETRIC_REPRESENTATION_CONTEXT ( 3 ) GLOBAL_UNCERTAINTY_ASSIGNED_CONTEXT ( ( #56454 ) ) GLOBAL_UNIT_ASSIGNED_CONTEXT ( ( #43913, #44903, #59411 ) ) REPRESENTATION_CONTEXT ( 'NONE', 'WORKASPACE' ) );
#47316 = CARTESIAN_POINT ( 'NONE',  ( 12.91533473730992121, 19.52201867748816611, 10.88017736071110164 ) ) ;
#47317 = CARTESIAN_POINT ( 'NONE',  ( 19.38216949554541202, 45.99863466993041072, 9.382169495545424454 ) ) ;
#47318 = CARTESIAN_POINT ( 'NONE',  ( 0.6178305044545818747, -1.501365330069579951, -9.382169495545419124 ) ) ;
#47319 = CARTESIAN_POINT ( 'NONE',  ( 7.361572987183170547, 12.05059781766744997, 9.846743663894590881 ) ) ;
#47321 = VERTEX_POINT ( 'NONE', #42352 ) ;
#47320 = EDGE_CURVE ( 'NONE', #30635, #48953, #56234, .T. ) ;
#47322 = LINE ( 'NONE', #31826, #8543 ) ;
#47323 = CARTESIAN_POINT ( 'NONE',  ( -14.94699059465102664, 15.00000000000000000, 1.259949270174715696 ) ) ;
#47324 = CARTESIAN_POINT ( 'NONE',  ( -4.164238869374099927, 52.01208216824729647, 3.795296366450308767 ) ) ;
#47325 = CARTESIAN_POINT ( 'NONE',  ( 2.917880565312950480, 15.97041550158063217, -12.26659068614894821 ) ) ;
#47326 = CARTESIAN_POINT ( 'NONE',  ( -0.8801773607110991993, 17.85535201082150536, -2.915334737309923874 ) ) ;
#47327 = CARTESIAN_POINT ( 'NONE',  ( 10.00000000000000178, 34.31368534415484106, 10.88017736071110342 ) ) ;
#47328 = CARTESIAN_POINT ( 'NONE',  ( 14.35840480524197282, 0.5000000000000004441, 4.340070442838948495 ) ) ;
#47329 = LINE ( 'NONE', #62830, #27302 ) ;
#47330 = CARTESIAN_POINT ( 'NONE',  ( 7.084665262690076126, 62.02201867748816966, -10.88017736071110164 ) ) ;
#47331 = CARTESIAN_POINT ( 'NONE',  ( 17.20831665107776587, 24.13393115100078035, -7.208316651077762316 ) ) ;
#47332 = CARTESIAN_POINT ( 'NONE',  ( 1.274849032794294290, 63.57228050351031357, 6.499999999999979572 ) ) ;
#47333 = SURFACE_SIDE_STYLE ('',( #86334 ) ) ;
#47334 = CARTESIAN_POINT ( 'NONE',  ( 10.00000000000000178, 12.25893115100078568, 9.846743663894594434 ) ) ;
#47335 = CARTESIAN_POINT ( 'NONE',  ( 10.00000000000000000, 39.75893115100078745, -9.846743663894594434 ) ) ;
#47336 = CARTESIAN_POINT ( 'NONE',  ( -0.8801773607111008646, 13.27201867748817143, 2.915334737309923430 ) ) ;
#47337 = AXIS2_PLACEMENT_3D ( 'NONE', #50761, #82233, #26768 ) ;
#47338 = UNCERTAINTY_MEASURE_WITH_UNIT (LENGTH_MEASURE( 1.000000000000000082E-05 ), #377, 'distance_accuracy_value', 'NONE');
#47339 = CARTESIAN_POINT ( 'NONE',  ( 16.40814093676323893, 30.79030133659708923, 11.09922568453595026 ) ) ;
#47340 = CARTESIAN_POINT ( 'NONE',  ( 7.084665262690076126, 52.02201867748816255, -10.88017736071110164 ) ) ;
#47342 = CARTESIAN_POINT ( 'NONE',  ( 12.63842701281683034, 7.467264484334118713, 9.846743663894596210 ) ) ;
#47341 = CARTESIAN_POINT ( 'NONE',  ( 24.16423886937410614, 49.51208216824730357, -3.795296366450302550 ) ) ;
#47343 = CARTESIAN_POINT ( 'NONE',  ( 2.603489959281613420, 35.43575266056827644, -6.500000000000031086 ) ) ;
#47344 = CARTESIAN_POINT ( 'NONE',  ( 2.791683348922237240, 50.38393115100078035, -7.208316651077763204 ) ) ;
#47346 = CARTESIAN_POINT ( 'NONE',  ( -0.3689425029237898834, 6.178748834913968757, -10.36894250292378850 ) ) ;
#47345 = CARTESIAN_POINT ( 'NONE',  ( 10.00000000000000000, 29.75893115100078745, -9.846743663894594434 ) ) ;
#47347 =( BOUNDED_CURVE ( )  B_SPLINE_CURVE ( 2, ( #54939, #15505, #23981, #76962, #60970, #61462, #70458, #32444, #519 ),
 .UNSPECIFIED., .F., .F. ) 
 B_SPLINE_CURVE_WITH_KNOTS ( ( 3, 2, 2, 2, 3 ),
 ( 0.4382284501891250961, 0.4404761904761904656, 0.4464285714285714524, 0.4523809523809523836, 0.4546286926680177531 ),
 .UNSPECIFIED. ) 
 CURVE ( )  GEOMETRIC_REPRESENTATION_ITEM ( )  RATIONAL_B_SPLINE_CURVE ( ( 0.9839835555609424134, 0.9871328979762477029, 1.000000000000000000, 0.9659258262890683122, 1.000000000000000000, 0.9659258262890683122, 1.000000000000000000, 0.9871328979762477029, 0.9839835555609424134 ) ) 
 REPRESENTATION_ITEM ( '' )  );
#47348 = CARTESIAN_POINT ( 'NONE',  ( 10.00000000000000178, 23.05374883491397142, 14.16423886937410082 ) ) ;
#47349 = CARTESIAN_POINT ( 'NONE',  ( 2.035157376598824452, 43.68868534415484106, 7.964842623401179544 ) ) ;
#47350 = VECTOR ( 'NONE', #33037, 1000.000000000000000 ) ;
#47351 = CARTESIAN_POINT ( 'NONE',  ( 15.44008868035555793, 11.39701867748817143, -9.422509992056140149 ) ) ;
#47352 = CARTESIAN_POINT ( 'NONE',  ( 7.084665262690076126, 44.10535201082151247, 10.88017736071109987 ) ) ;
#47353 = CARTESIAN_POINT ( 'NONE',  ( 2.035157376598824452, 28.68868534415484106, 7.964842623401179544 ) ) ;
#47354 = ORIENTED_EDGE ( 'NONE', *, *, #51256, .F. ) ;
#47355 = CIRCLE ( 'NONE', #20240, 0.2500000000000002220 ) ;
#47356 = CARTESIAN_POINT ( 'NONE',  ( 4.559911319644449179, 43.89701867748816966, 9.422509992056141925 ) ) ;
#47357 = ORIENTED_EDGE ( 'NONE', *, *, #10646, .T. ) ;
#47358 = CARTESIAN_POINT ( 'NONE',  ( 10.00000000000000000, 62.87363466993042493, -12.81628187352647608 ) ) ;
#47359 = EDGE_CURVE ( 'NONE', #39036, #36269, #3493, .T. ) ;
#47360 = VECTOR ( 'NONE', #11982, 1000.000000000000000 ) ;
#47361 = CARTESIAN_POINT ( 'NONE',  ( 7.084665262690076126, 57.02201867748817676, -10.88017736071110164 ) ) ;
#47362 = EDGE_LOOP ( 'NONE', ( #37923, #52097, #58587, #44648, #69898, #87523 ) ) ;
#47363 = VECTOR ( 'NONE', #89833, 1000.000000000000000 ) ;
#47364 = CARTESIAN_POINT ( 'NONE',  ( 10.00000000000000178, 54.31368534415484106, 10.88017736071110342 ) ) ;
#47365 = CARTESIAN_POINT ( 'NONE',  ( -0.8801773607111009756, 3.063685344154837509, 1.068504757029289695E-15 ) ) ;
#47366 = CIRCLE ( 'NONE', #36167, 14.49999999999999822 ) ;
#47367 = CARTESIAN_POINT ( 'NONE',  ( 18.72515096720571393, 41.07228050351032778, -6.499999999999974243 ) ) ;
#47368 = FACE_OUTER_BOUND ( 'NONE', #31770, .T. ) ;
#47369 = CARTESIAN_POINT ( 'NONE',  ( -0.3689425029237898834, 61.17874883491396076, -10.36894250292378850 ) ) ;
#47370 = CARTESIAN_POINT ( 'NONE',  ( 17.96484262340118221, 64.93868534415483396, 7.964842623401181321 ) ) ;
#47371 = CARTESIAN_POINT ( 'NONE',  ( -4.164238869374099039, 6.803748834913967869, 8.674139862899312516E-16 ) ) ;
#47372 = CARTESIAN_POINT ( 'NONE',  ( -14.22792531055123888, 15.00000000000000711, 3.387425595041007043 ) ) ;
#47373 = CARTESIAN_POINT ( 'NONE',  ( 20.88017736071110875, 15.77201867748817143, -2.915334737309920765 ) ) ;
#47374 = CARTESIAN_POINT ( 'NONE',  ( 0.1532563361054083140, 51.00893115100078745, 1.131784320476157264E-15 ) ) ;
#47375 = ORIENTED_EDGE ( 'NONE', *, *, #33872, .F. ) ;
#47376 = CARTESIAN_POINT ( 'NONE',  ( 12.63842701281683922, 49.55059781766744464, -9.846743663894590881 ) ) ;
#47377 = CARTESIAN_POINT ( 'NONE',  ( -0.8801773607111008646, 43.27201867748817676, 2.915334737309923430 ) ) ;
#47378 = CARTESIAN_POINT ( 'NONE',  ( 0.1532563361054082862, 36.21726448433410894, 2.638427012816831674 ) ) ;
#47380 = CARTESIAN_POINT ( 'NONE',  ( 20.88017736071110519, 65.56368534415483396, 2.639326808657452039E-16 ) ) ;
#47379 = SURFACE_STYLE_FILL_AREA ( #94359 ) ;
#47381 = CARTESIAN_POINT ( 'NONE',  ( 12.91533473730992121, 44.52201867748816966, 10.88017736071110164 ) ) ;
#47382 = CARTESIAN_POINT ( 'NONE',  ( -4.164238869374099927, 62.01208216824728936, 3.795296366450308767 ) ) ;
#47383 = CARTESIAN_POINT ( 'NONE',  ( 19.38216949554541202, 25.99863466993042138, 9.382169495545424454 ) ) ;
#47384 = CARTESIAN_POINT ( 'NONE',  ( 6.000000000000000000, 61.00000000000000711, 5.000000000000000000 ) ) ;
#47385 = ORIENTED_EDGE ( 'NONE', *, *, #83431, .F. ) ;
#47386 = CARTESIAN_POINT ( 'NONE',  ( -2.816281873526473856, 29.12363466993041783, 9.499525473075851096E-16 ) ) ;
#47387 = CARTESIAN_POINT ( 'NONE',  ( 7.084665262690076126, 24.10535201082150181, 10.88017736071109987 ) ) ;
#47388 = CIRCLE ( 'NONE', #72947, 18.53834841531100608 ) ;
#47389 = EDGE_CURVE ( 'NONE', #25008, #9131, #9905, .T. ) ;
#47390 = VERTEX_POINT ( 'NONE', #38794 ) ;
#47391 = CARTESIAN_POINT ( 'NONE',  ( 7.084665262690076126, 69.10535201082151957, 10.88017736071109987 ) ) ;
#47392 = CARTESIAN_POINT ( 'NONE',  ( 5.076628168052704559, 50.17559781766745886, -8.527530157486179263 ) ) ;
#47394 = CARTESIAN_POINT ( 'NONE',  ( 12.63842701281683922, 39.55059781766744464, -9.846743663894590881 ) ) ;
#47393 = CARTESIAN_POINT ( 'NONE',  ( 0.1532563361054100626, 10.80059781766745175, -2.638427012816831230 ) ) ;
#47395 = CARTESIAN_POINT ( 'NONE',  ( 0.000000000000000000, 0.000000000000000000, 0.000000000000000000 ) ) ;
#47396 = DIRECTION ( 'NONE',  ( 0.000000000000000000, 0.000000000000000000, 1.000000000000000000 ) ) ;
#47397 = CARTESIAN_POINT ( 'NONE',  ( 19.84674366389459621, 23.50893115100078390, 7.409399052514197653E-17 ) ) ;
#47398 = CARTESIAN_POINT ( 'NONE',  ( 20.04068437667226732, 54.71974360917722890, 6.396802510829642685 ) ) ;
#47399 = CARTESIAN_POINT ( 'NONE',  ( 5.500000000000000000, 11.00000000000000000, 6.000000000000000000 ) ) ;
#47401 = CARTESIAN_POINT ( 'NONE',  ( 9.779999999999990479, 20.99999999999999645, -3.000000000000000000 ) ) ;
#47400 = CARTESIAN_POINT ( 'NONE',  ( 1.472469842513823179, 31.42559781766745530, 4.923371831947296329 ) ) ;
#47402 = DIRECTION ( 'NONE',  ( 0.000000000000000000, 1.000000000000000000, 0.000000000000000000 ) ) ;
#47403 = ADVANCED_FACE ( 'NONE', ( #53291 ), #15806, .F. ) ;
#47405 = VERTEX_POINT ( 'NONE', #16292 ) ;
#47404 = CARTESIAN_POINT ( 'NONE',  ( 5.076628168052704559, 50.17559781766745886, -8.527530157486179263 ) ) ;
#47406 = CARTESIAN_POINT ( 'NONE',  ( 11.59936910322016423, 56.97882069866371069, 0.000000000000000000 ) ) ;
#47407 = CARTESIAN_POINT ( 'NONE',  ( 21.09922568453594849, 21.20696800326375353, 6.408140936763242479 ) ) ;
#47408 = EDGE_CURVE ( 'NONE', #46208, #70611, #62259, .T. ) ;
#47409 = CARTESIAN_POINT ( 'NONE',  ( -13.80105244023572197, 90.89655890636302615, 7.750000000000543565 ) ) ;
#47410 = CIRCLE ( 'NONE', #95311, 0.2500000000000002220 ) ;
#47412 = ADVANCED_FACE ( 'NONE', ( #37818 ), #59341, .T. ) ;
#47411 = CARTESIAN_POINT ( 'NONE',  ( -0.3689425029237898834, 41.17874883491397497, -10.36894250292378850 ) ) ;
#47413 = CARTESIAN_POINT ( 'NONE',  ( 12.63842701281683922, 14.55059781766744997, -9.846743663894590881 ) ) ;
#47414 =( LENGTH_UNIT ( ) NAMED_UNIT ( * ) SI_UNIT ( .MILLI., .METRE. ) );
#47415 = CARTESIAN_POINT ( 'NONE',  ( 20.00000000000000711, 98.59912998021083297, 4.500000000000000888 ) ) ;
#47416 = CARTESIAN_POINT ( 'NONE',  ( 24.16423886937409904, 44.09541550158063927, 3.795296366450317205 ) ) ;
#47418 = B_SPLINE_CURVE_WITH_KNOTS ( 'NONE', 3,
 ( #87506, #57496, #19018, #87990, #49496, #41537 ),
 .UNSPECIFIED., .F., .F.,
 ( 4, 2, 4 ),
 ( 0.0002800364959418014067, 0.0006862420824208874913, 0.001092447668899973467 ),
 .UNSPECIFIED. ) ;
#47417 = CARTESIAN_POINT ( 'NONE',  ( 14.92337183194729988, 59.34226448433412315, -8.527530157486177487 ) ) ;
#47419 = CARTESIAN_POINT ( 'NONE',  ( 13.79529636645031943, 60.34541550158063927, -14.16423886937409904 ) ) ;
#47420 = CARTESIAN_POINT ( 'NONE',  ( -0.3689425029237881626, 22.42874883491397142, 10.36894250292379027 ) ) ;
#47422 = CARTESIAN_POINT ( 'NONE',  ( -44.79809994011756658, 105.6827849507685926, -4.824119973700185859 ) ) ;
#47421 = CARTESIAN_POINT ( 'NONE',  ( 10.00000000000000178, 28.05374883491396787, 14.16423886937410082 ) ) ;
#47423 = CARTESIAN_POINT ( 'NONE',  ( 13.95749458852077218, 14.76930270348881002, 5.331641351773115822 ) ) ;
#47424 = APPLICATION_CONTEXT ( 'automotive_design' ) ;
#47426 = CARTESIAN_POINT ( 'NONE',  ( 12.63842701281683922, 49.55059781766744464, -9.846743663894590881 ) ) ;
#47425 = CARTESIAN_POINT ( 'NONE',  ( 5.056330833731752072, 3.901243639414221473E-16, -13.58983143750699973 ) ) ;
#47427 = ORIENTED_EDGE ( 'NONE', *, *, #66413, .T. ) ;
#47428 = CARTESIAN_POINT ( 'NONE',  ( 2.035157376598824452, 33.68868534415484106, 7.964842623401179544 ) ) ;
#47429 = DIRECTION ( 'NONE',  ( 0.000000000000000000, 0.000000000000000000, 1.000000000000000000 ) ) ;
#47430 = DIRECTION ( 'NONE',  ( 0.000000000000000000, 0.000000000000000000, 1.000000000000000000 ) ) ;
#47431 = CARTESIAN_POINT ( 'NONE',  ( 5.076628168052704559, 35.17559781766745175, -8.527530157486179263 ) ) ;
#47433 = CARTESIAN_POINT ( 'NONE',  ( 16.40814093676324603, 52.45696800326375353, -11.09922568453594671 ) ) ;
#47432 = VECTOR ( 'NONE', #79516, 1000.000000000000227 ) ;
#47434 = CARTESIAN_POINT ( 'NONE',  ( 7.082119434687054849, -11.52958449841935717, 12.26659068614894288 ) ) ;
#47435 = CIRCLE ( 'NONE', #64974, 0.4999999999999995559 ) ;
#47436 = CARTESIAN_POINT ( 'NONE',  ( 7.361572987183169658, 44.96726448433412315, -9.846743663894592657 ) ) ;
#47437 = CARTESIAN_POINT ( 'NONE',  ( 0.1532563361054100626, 60.80059781766744464, -2.638427012816831230 ) ) ;
#47439 = EDGE_CURVE ( 'NONE', #74806, #81557, #54560, .T. ) ;
#47438 = ORIENTED_EDGE ( 'NONE', *, *, #61114, .F. ) ;
#47440 = CARTESIAN_POINT ( 'NONE',  ( 6.204703633549690345, 10.76208216824729824, -14.16423886937410259 ) ) ;
#47441 = DIRECTION ( 'NONE',  ( 0.000000000000000000, 1.000000000000000000, -0.000000000000000000 ) ) ;
#47443 = CARTESIAN_POINT ( 'NONE',  ( -10.58981376305275468, -0.03417435944610275333, -9.535111140613857117 ) ) ;
#47442 = FILL_AREA_STYLE ('',( #32435 ) ) ;
#47444 = CARTESIAN_POINT ( 'NONE',  ( -2.266590686148945544, 67.22041550158063217, 7.082119434687048631 ) ) ;
#47445 = CARTESIAN_POINT ( 'NONE',  ( -2.816281873526473856, 14.12363466993041961, 9.499525473075851096E-16 ) ) ;
#47446 = CARTESIAN_POINT ( 'NONE',  ( 0.5774900079438590739, 62.64701867748817676, -5.440088680355550821 ) ) ;
#47447 = ADVANCED_FACE ( 'NONE', ( #24291 ), #54757, .F. ) ;
#47448 = FILL_AREA_STYLE_COLOUR ( '', #59624 ) ;
#47449 = CARTESIAN_POINT ( 'NONE',  ( -46.94000000000001194, 102.4380508258080198, -6.413016458746108484 ) ) ;
#47450 = CARTESIAN_POINT ( 'NONE',  ( -14.03351048042393856, 15.00000000000000000, -2.474486531753901541 ) ) ;
#47451 = CARTESIAN_POINT ( 'NONE',  ( -2.266590686148945544, 56.38708216824731068, -7.082119434687050408 ) ) ;
#47452 = CARTESIAN_POINT ( 'NONE',  ( 6.000000000000000000, 10.49999999999999822, 6.000000000000000000 ) ) ;
#47453 = CARTESIAN_POINT ( 'NONE',  ( 2.035157376598822676, 27.43868534415483396, -7.964842623401177768 ) ) ;
#47454 = CARTESIAN_POINT ( 'NONE',  ( 20.88017736071110875, 35.77201867748816966, -2.915334737309920765 ) ) ;
#47455 = CARTESIAN_POINT ( 'NONE',  ( 6.565887622018943937, 3.081968003263753531, -12.81628187352647608 ) ) ;
#47456 = CARTESIAN_POINT ( 'NONE',  ( 17.20831665107776587, 57.88393115100078745, 7.208316651077764980 ) ) ;
#47457 = FACE_OUTER_BOUND ( 'NONE', #55563, .T. ) ;
#47458 = EDGE_LOOP ( 'NONE', ( #23250, #87138, #82552, #30766 ) ) ;
#47459 = CARTESIAN_POINT ( 'NONE',  ( 20.88017736071110519, 35.56368534415484106, 2.639326808657452039E-16 ) ) ;
#47460 = CARTESIAN_POINT ( 'NONE',  ( 21.09922568453594849, 26.20696800326375353, 6.408140936763242479 ) ) ;
#47461 = ADVANCED_FACE ( 'NONE', ( #91288 ), #45804, .T. ) ;
#47462 = CARTESIAN_POINT ( 'NONE',  ( 17.20831665107776587, 64.13393115100079456, -7.208316651077762316 ) ) ;
#47463 = CARTESIAN_POINT ( 'NONE',  ( 20.88017736071110519, 45.56368534415484106, 2.639326808657452039E-16 ) ) ;
#47464 = CARTESIAN_POINT ( 'NONE',  ( 18.52753015748617571, 18.09226448433411960, 4.923371831947298993 ) ) ;
#47465 = AXIS2_PLACEMENT_3D ( 'NONE', #12901, #66894, #13400 ) ;
#47466 = CARTESIAN_POINT ( 'NONE',  ( -2.816281873526473856, 29.33196800326376064, 3.434112377981055619 ) ) ;
#47468 = FACE_OUTER_BOUND ( 'NONE', #26601, .T. ) ;
#47467 = CARTESIAN_POINT ( 'NONE',  ( 19.42250999205614548, 60.98035201082151247, -5.440088680355545492 ) ) ;
#47469 = DIRECTION ( 'NONE',  ( 6.608470384673550777E-17, 1.000000000000000000, -0.000000000000000000 ) ) ;
#47470 = CARTESIAN_POINT ( 'NONE',  ( 21.09922568453595559, 62.04030133659709634, -6.408140936763230044 ) ) ;
#47471 = ORIENTED_EDGE ( 'NONE', *, *, #39878, .T. ) ;
#47472 = CARTESIAN_POINT ( 'NONE',  ( -6.982525766850298687, -88.11956318484570261, 2.750000000000000444 ) ) ;
#47473 = CARTESIAN_POINT ( 'NONE',  ( 7.551349515323100725, 15.00000000000000000, 12.08468537022911349 ) ) ;
#47474 = CARTESIAN_POINT ( 'NONE',  ( 4.559911319644449179, 3.897018677488170990, 9.422509992056141925 ) ) ;
#47476 = CARTESIAN_POINT ( 'NONE',  ( 13.79529636645031943, 10.34541550158063394, -14.16423886937409904 ) ) ;
#47475 = CARTESIAN_POINT ( 'NONE',  ( 10.00000000000000000, 47.87363466993042493, -12.81628187352647608 ) ) ;
#47477 = CARTESIAN_POINT ( 'NONE',  ( 17.20831665107776587, 19.13393115100078035, -7.208316651077762316 ) ) ;
#47478 = CARTESIAN_POINT ( 'NONE',  ( 2.035157376598822676, 2.438685344154837953, -7.964842623401177768 ) ) ;
#47479 = CARTESIAN_POINT ( 'NONE',  ( 18.52753015748618282, 13.92559781766745175, -4.923371831947291888 ) ) ;
#47480 = CARTESIAN_POINT ( 'NONE',  ( 20.36894250292379738, 54.92874883491396076, -10.36894250292379027 ) ) ;
#47481 = ORIENTED_EDGE ( 'NONE', *, *, #38881, .F. ) ;
#47482 = CARTESIAN_POINT ( 'NONE',  ( 4.559911319644449179, 2.230352010821504471, -9.422509992056141925 ) ) ;
#47483 = CARTESIAN_POINT ( 'NONE',  ( 4.559911319644449179, 12.23035201082150536, -9.422509992056141925 ) ) ;
#47484 = CARTESIAN_POINT ( 'NONE',  ( 8.629999999999995453, 41.24999999999999289, 4.250000000000000000 ) ) ;
#47485 = ORIENTED_EDGE ( 'NONE', *, *, #10178, .T. ) ;
#47486 = CARTESIAN_POINT ( 'NONE',  ( 12.91533473730992121, 9.522018677488171434, 10.88017736071110164 ) ) ;
#47487 = CARTESIAN_POINT ( 'NONE',  ( 17.96484262340118221, 6.188685344154837509, -7.964842623401177768 ) ) ;
#47488 = CARTESIAN_POINT ( 'NONE',  ( 1.472469842513823179, 46.42559781766745175, 4.923371831947296329 ) ) ;
#47489 = CARTESIAN_POINT ( 'NONE',  ( 3.591859063236761518, 54.95696800326376064, 11.09922568453594849 ) ) ;
#47490 = SURFACE_STYLE_FILL_AREA ( #54983 ) ;
#47492 = CARTESIAN_POINT ( 'NONE',  ( 13.79529636645031943, 20.34541550158063572, -14.16423886937409904 ) ) ;
#47491 = DIRECTION ( 'NONE',  ( 0.000000000000000000, 0.000000000000000000, 1.000000000000000000 ) ) ;
#47493 = CARTESIAN_POINT ( 'NONE',  ( 7.084665262690076126, 29.10535201082150181, 10.88017736071109987 ) ) ;
#47494 = CARTESIAN_POINT ( 'NONE',  ( 2.035157376598822676, 2.438685344154838397, -7.964842623401177768 ) ) ;
#47495 = CARTESIAN_POINT ( 'NONE',  ( 5.076628168052703671, 61.84226448433412315, 8.527530157486179263 ) ) ;
#47496 = FACE_OUTER_BOUND ( 'NONE', #86713, .T. ) ;
#47497 = CARTESIAN_POINT ( 'NONE',  ( 1.472469842513823179, 41.42559781766745886, 4.923371831947296329 ) ) ;
#47498 = DIRECTION ( 'NONE',  ( 0.000000000000000000, -1.000000000000000000, 0.000000000000000000 ) ) ;
#47499 = CARTESIAN_POINT ( 'NONE',  ( 7.361572987183169658, 4.967264484334119601, -9.846743663894592657 ) ) ;
#47500 = CARTESIAN_POINT ( 'NONE',  ( -9.846743663894590881, 26.21726448433411960, 2.638427012816840111 ) ) ;
#47501 = PRESENTATION_LAYER_ASSIGNMENT (  '', '', ( #85770 ) ) ;
#47502 = ORIENTED_EDGE ( 'NONE', *, *, #15946, .T. ) ;
#47503 = SURFACE_SIDE_STYLE ('',( #54996 ) ) ;
#47504 = CARTESIAN_POINT ( 'NONE',  ( 2.791683348922237240, 0.3839311510007847872, -7.208316651077763204 ) ) ;
#47506 = CARTESIAN_POINT ( 'NONE',  ( 13.43411237798105340, 0.5819680032637533085, 12.81628187352647963 ) ) ;
#47505 = AXIS2_PLACEMENT_3D ( 'NONE', #24341, #46819, #37868 ) ;
#47507 = CARTESIAN_POINT ( 'NONE',  ( 12.91533473730993009, 41.60535201082149825, -10.88017736071109987 ) ) ;
#47509 = CARTESIAN_POINT ( 'NONE',  ( 21.09922568453595559, 42.04030133659708213, -6.408140936763230044 ) ) ;
#47508 = CARTESIAN_POINT ( 'NONE',  ( 10.00000000000000178, 9.313685344154839285, 10.88017736071110342 ) ) ;
#47510 = CARTESIAN_POINT ( 'NONE',  ( -4.164238869374099039, 21.80374883491396787, 8.674139862899312516E-16 ) ) ;
#47511 = EDGE_CURVE ( 'NONE', #84080, #10597, #69785, .T. ) ;
#47512 = AXIS2_PLACEMENT_3D ( 'NONE', #17904, #95366, #87857 ) ;
#47513 = VECTOR ( 'NONE', #29020, 1000.000000000000000 ) ;
#47514 = ORIENTED_EDGE ( 'NONE', *, *, #78155, .F. ) ;
#47515 = CARTESIAN_POINT ( 'NONE',  ( 22.81628187352648496, 46.83196800326376064, -3.434112377981050290 ) ) ;
#47516 = VERTEX_POINT ( 'NONE', #14324 ) ;
#47517 = CARTESIAN_POINT ( 'NONE',  ( 5.076628168052703671, 51.84226448433412315, 8.527530157486179263 ) ) ;
#47518 = CARTESIAN_POINT ( 'NONE',  ( 12.91533473730993009, 21.60535201082150536, -10.88017736071109987 ) ) ;
#47519 = CARTESIAN_POINT ( 'NONE',  ( 10.00000000000000178, 34.31368534415484106, 10.88017736071110342 ) ) ;
#47520 = ORIENTED_EDGE ( 'NONE', *, *, #24059, .F. ) ;
#47521 = CARTESIAN_POINT ( 'NONE',  ( 5.076628168052704559, 10.17559781766745175, -8.527530157486179263 ) ) ;
#47522 = CARTESIAN_POINT ( 'NONE',  ( 10.00000000000000178, 69.31368534415484817, 10.88017736071110342 ) ) ;
#47523 = CARTESIAN_POINT ( 'NONE',  ( -0.1503990784575359729, 18.10158574516642460, 6.262539305110062848 ) ) ;
#47524 = B_SPLINE_CURVE_WITH_KNOTS ( 'NONE', 3,
 ( #50334, #36330, #74313, #65334, #73824, #81816 ),
 .UNSPECIFIED., .F., .F.,
 ( 4, 2, 4 ),
 ( 3.409110551496077836E-05, 0.0004400426677367842406, 0.0008459942299586076893 ),
 .UNSPECIFIED. ) ;
#47525 = CARTESIAN_POINT ( 'NONE',  ( 12.63842701281683922, 9.550597817667449974, -9.846743663894590881 ) ) ;
#47526 = EDGE_CURVE ( 'NONE', #1162, #43600, #89217, .T. ) ;
#47527 = CARTESIAN_POINT ( 'NONE',  ( 19.42250999205614193, 65.14701867748817676, 5.440088680355555262 ) ) ;
#47528 = CARTESIAN_POINT ( 'NONE',  ( 18.72515096720583827, 65.05509018479936856, 6.499999999999810818 ) ) ;
#47529 = CARTESIAN_POINT ( 'NONE',  ( 0.5774900079438607392, 38.48035201082150536, 5.440088680355550821 ) ) ;
#47530 = CARTESIAN_POINT ( 'NONE',  ( 19.42250999205614193, 65.14701867748817676, 5.440088680355555262 ) ) ;
#47532 = ORIENTED_EDGE ( 'NONE', *, *, #25263, .F. ) ;
#47531 = CARTESIAN_POINT ( 'NONE',  ( 17.20831665107776587, 4.133931151000785675, -7.208316651077762316 ) ) ;
#47533 =( BOUNDED_CURVE ( )  B_SPLINE_CURVE ( 2, ( #53695, #84218, #38706, #97256, #13732, #86663, #39700, #10663, #69206, #8689, #55161, #77669, #10175 ),
 .UNSPECIFIED., .F., .F. ) 
 B_SPLINE_CURVE_WITH_KNOTS ( ( 3, 2, 2, 2, 2, 2, 3 ),
 ( 0.5999999999999999778, 0.6055555555555555136, 0.6111111111111111605, 0.6166666666666666963, 0.6222222222222223431, 0.6277777777777778789, 0.6333333333333334147 ),
 .UNSPECIFIED. ) 
 CURVE ( )  GEOMETRIC_REPRESENTATION_ITEM ( )  RATIONAL_B_SPLINE_CURVE ( ( 1.000000000000000000, 0.9659258262890682012, 1.000000000000000000, 0.9659258262890682012, 1.000000000000000000, 0.9659258262890682012, 1.000000000000000000, 0.9659258262890682012, 1.000000000000000000, 0.9659258262890682012, 1.000000000000000000, 0.9659258262890675351, 1.000000000000000666 ) ) 
 REPRESENTATION_ITEM ( '' )  );
#47534 = EDGE_CURVE ( 'NONE', #15285, #51412, #91402, .T. ) ;
#47535 = B_SPLINE_CURVE_WITH_KNOTS ( 'NONE', 3,
 ( #59334, #43835, #50861, #12850, #42381, #43349 ),
 .UNSPECIFIED., .F., .F.,
 ( 4, 2, 4 ),
 ( 0.0002800111042658766803, 0.0006862164422996869110, 0.001092421780333497142 ),
 .UNSPECIFIED. ) ;
#47536 = CARTESIAN_POINT ( 'NONE',  ( 17.20831665107776587, 59.13393115100078745, -7.208316651077762316 ) ) ;
#47537 = ORIENTED_EDGE ( 'NONE', *, *, #27402, .F. ) ;
#47538 = VERTEX_POINT ( 'NONE', #22322 ) ;
#47539 = DIRECTION ( 'NONE',  ( 1.000000000000000000, 0.000000000000000000, 0.000000000000000000 ) ) ;
#47541 = EDGE_CURVE ( 'NONE', #36269, #73854, #76122, .T. ) ;
#47540 = CARTESIAN_POINT ( 'NONE',  ( -4.164238869374098151, 6.595415501580634832, -3.795296366450310543 ) ) ;
#47542 = CARTESIAN_POINT ( 'NONE',  ( -2.816281873526473856, 54.12363466993041783, 9.499525473075851096E-16 ) ) ;
#47543 = CARTESIAN_POINT ( 'NONE',  ( -4.164238869374099039, 1.803748834913967647, 8.674139862899312516E-16 ) ) ;
#47544 = CARTESIAN_POINT ( 'NONE',  ( 24.16423886937409904, 19.09541550158063927, 3.795296366450317205 ) ) ;
#47545 = CARTESIAN_POINT ( 'NONE',  ( 0.1143410931637208749, 45.21691075486302935, 6.480892540919845679 ) ) ;
#47547 = CARTESIAN_POINT ( 'NONE',  ( 10.00000000000000178, 59.31368534415484106, 10.88017736071110342 ) ) ;
#47546 = DIRECTION ( 'NONE',  ( -0.000000000000000000, -0.000000000000000000, -1.000000000000000000 ) ) ;
#47548 = CARTESIAN_POINT ( 'NONE',  ( 4.559911319644449179, 17.23035201082150536, -9.422509992056141925 ) ) ;
#47549 = SURFACE_SIDE_STYLE ('',( #24075 ) ) ;
#47550 = VERTEX_POINT ( 'NONE', #77759 ) ;
#47551 = CARTESIAN_POINT ( 'NONE',  ( 18.52753015748618282, 8.925597817667451750, -4.923371831947291888 ) ) ;
#47552 = CARTESIAN_POINT ( 'NONE',  ( 7.361572987183170547, 7.050597817667451750, 9.846743663894590881 ) ) ;
#47553 = CARTESIAN_POINT ( 'NONE',  ( 22.81628187352648496, 31.83196800326375353, -3.434112377981050290 ) ) ;
#47554 = CARTESIAN_POINT ( 'NONE',  ( 17.20831665107776587, 42.88393115100077324, 7.208316651077764980 ) ) ;
#47555 = DIRECTION ( 'NONE',  ( 1.000000000000000000, 0.000000000000000000, 0.000000000000000000 ) ) ;
#47556 = CARTESIAN_POINT ( 'NONE',  ( -2.816281873526473856, 9.331968003263753531, 3.434112377981055619 ) ) ;
#47557 = DIRECTION ( 'NONE',  ( -6.938893903907222067E-15, 1.000000000000000000, 0.000000000000000000 ) ) ;
#47558 = COLOUR_RGB ( '', 0.40784314, 0.44705882, 0.49803922) ;
#47559 = CARTESIAN_POINT ( 'NONE',  ( 14.92337183194729988, 29.34226448433411960, -8.527530157486177487 ) ) ;
#47560 = CARTESIAN_POINT ( 'NONE',  ( 0.1532563361054082862, 1.217264484334117824, 2.638427012816831674 ) ) ;
#47561 = EDGE_LOOP ( 'NONE', ( #16274, #86734, #66071, #27098 ) ) ;
#47562 = ORIENTED_EDGE ( 'NONE', *, *, #58886, .F. ) ;
#47563 = CARTESIAN_POINT ( 'NONE',  ( 2.035157376598822676, 32.43868534415483396, -7.964842623401177768 ) ) ;
#47564 = CARTESIAN_POINT ( 'NONE',  ( -2.266590686148945544, 36.38708216824730357, -7.082119434687050408 ) ) ;
#47565 = CARTESIAN_POINT ( 'NONE',  ( 5.076628168052704559, 35.17559781766745175, -8.527530157486179263 ) ) ;
#47566 = CARTESIAN_POINT ( 'NONE',  ( 12.63842701281683034, 17.46726448433411250, 9.846743663894596210 ) ) ;
#47568 = LINE ( 'NONE', #39094, #32036 ) ;
#47567 = CARTESIAN_POINT ( 'NONE',  ( 3.591859063236763294, 53.29030133659708923, -11.09922568453595026 ) ) ;
#47569 = CARTESIAN_POINT ( 'NONE',  ( 20.88017736071110164, 30.35535201082151247, 2.915334737309930979 ) ) ;
#47570 = EDGE_CURVE ( 'NONE', #36257, #22305, #55767, .T. ) ;
#47571 = CARTESIAN_POINT ( 'NONE',  ( -14.62617646268089899, 15.00000000000000000, 3.327906561566782440 ) ) ;
#47572 = AXIS2_PLACEMENT_3D ( 'NONE', #29162, #90156, #69640 ) ;
#47573 = CARTESIAN_POINT ( 'NONE',  ( 6.565887622018943937, 28.08196800326375353, -12.81628187352647608 ) ) ;
#47574 = CARTESIAN_POINT ( 'NONE',  ( 18.52753015748618282, 43.92559781766745175, -4.923371831947291888 ) ) ;
#47575 = CARTESIAN_POINT ( 'NONE',  ( -2.915334737309934532, 7.022018677488174099, -10.88017736071109987 ) ) ;
#47576 = CARTESIAN_POINT ( 'NONE',  ( 19.38216949554541202, 45.99863466993041072, 9.382169495545424454 ) ) ;
#47577 = CARTESIAN_POINT ( 'NONE',  ( 32.06412365047463453, 26.99999999999998224, 10.00000000000000000 ) ) ;
#47579 = DIRECTION ( 'NONE',  ( 1.000000000000000000, 0.000000000000000000, 0.000000000000000000 ) ) ;
#47578 = CARTESIAN_POINT ( 'NONE',  ( 15.44008868035555260, 59.73035201082151247, 9.422509992056143702 ) ) ;
#47580 = STYLED_ITEM ( 'NONE', ( #56155 ), #57825 ) ;
#47581 = CARTESIAN_POINT ( 'NONE',  ( -11.01435017114802406, -93.41041245699096862, 4.000000000000000000 ) ) ;
#47583 = EDGE_CURVE ( 'NONE', #93734, #63206, #86259, .T. ) ;
#47582 = PLANE ( 'NONE',  #56013 ) ;
#47584 = AXIS2_PLACEMENT_3D ( 'NONE', #2761, #78230, #16758 ) ;
#47585 = CARTESIAN_POINT ( 'NONE',  ( -0.8801773607110991993, 52.85535201082151247, -2.915334737309923874 ) ) ;
#47586 = CARTESIAN_POINT ( 'NONE',  ( 12.91533473730992121, 54.52201867748816255, 10.88017736071110164 ) ) ;
#47587 = FACE_OUTER_BOUND ( 'NONE', #95341, .T. ) ;
#47588 = DIRECTION ( 'NONE',  ( 0.000000000000000000, 1.000000000000000000, 0.000000000000000000 ) ) ;
#47589 = CARTESIAN_POINT ( 'NONE',  ( 20.88017736071110519, 10.56368534415483929, 2.639326808657452039E-16 ) ) ;
#47590 = CARTESIAN_POINT ( 'NONE',  ( 1.472469842513823179, 65.59226448433412315, -4.923371831947296329 ) ) ;
#47592 = CARTESIAN_POINT ( 'NONE',  ( 17.39651004071842522, 24.08210964143329491, -6.499999999999992895 ) ) ;
#47591 = CARTESIAN_POINT ( 'NONE',  ( 17.96484262340118221, 19.93868534415484106, 7.964842623401181321 ) ) ;
#47593 = CARTESIAN_POINT ( 'NONE',  ( -0.1503990784575328643, 70.00000000000000000, 6.262539305110068177 ) ) ;
#47594 = CARTESIAN_POINT ( 'NONE',  ( -1.099225684535947600, 24.54030133659708923, 6.408140936763237150 ) ) ;
#47595 = ORIENTED_EDGE ( 'NONE', *, *, #50795, .T. ) ;
#47596 = CARTESIAN_POINT ( 'NONE',  ( 19.42250999205614193, 35.14701867748816966, 5.440088680355555262 ) ) ;
#47597 = CARTESIAN_POINT ( 'NONE',  ( 14.92337183194729633, 42.67559781766745886, 8.527530157486181039 ) ) ;
#47599 = CARTESIAN_POINT ( 'NONE',  ( -7.750000000000000000, 80.07179676972448590, -6.250000000000000000 ) ) ;
#47598 = CARTESIAN_POINT ( 'NONE',  ( 6.565887622018943937, 13.08196800326374998, -12.81628187352647608 ) ) ;
#47600 = CARTESIAN_POINT ( 'NONE',  ( 19.42250999205614193, 15.14701867748817143, 5.440088680355555262 ) ) ;
#47601 = CARTESIAN_POINT ( 'NONE',  ( 20.88017736071110164, 45.35535201082149115, 2.915334737309930979 ) ) ;
#47602 = CARTESIAN_POINT ( 'NONE',  ( 20.36894250292379738, 44.92874883491396787, -10.36894250292379027 ) ) ;
#47603 = CARTESIAN_POINT ( 'NONE',  ( 1.472469842513823179, 35.59226448433412315, -4.923371831947296329 ) ) ;
#47604 = CARTESIAN_POINT ( 'NONE',  ( 4.559911319644449179, 62.23035201082150536, -9.422509992056141925 ) ) ;
#47605 = FILL_AREA_STYLE ('',( #92603 ) ) ;
#47606 = CARTESIAN_POINT ( 'NONE',  ( -4.164238869374099927, 12.01208216824730357, 3.795296366450308767 ) ) ;
#47607 = B_SPLINE_CURVE_WITH_KNOTS ( 'NONE', 3,
 ( #88517, #81016, #12517, #5027, #35513, #43502 ),
 .UNSPECIFIED., .F., .F.,
 ( 4, 2, 4 ),
 ( 0.000000000000000000, 0.0002565770811490877411, 0.0005131541622981754822 ),
 .UNSPECIFIED. ) ;
#47608 = CARTESIAN_POINT ( 'NONE',  ( 18.18329248733322245, 12.60290668512019963, 6.499999999999997335 ) ) ;
#47609 = VERTEX_POINT ( 'NONE', #17772 ) ;
#47610 = CARTESIAN_POINT ( 'NONE',  ( 2.917880565312950480, 30.97041550158063572, -12.26659068614894821 ) ) ;
#47611 = CARTESIAN_POINT ( 'NONE',  ( 24.16423886937410614, 34.51208216824731068, -3.795296366450302550 ) ) ;
#47612 = CARTESIAN_POINT ( 'NONE',  ( 14.92337183194729988, 9.342264484334119601, -8.527530157486177487 ) ) ;
#47613 = CARTESIAN_POINT ( 'NONE',  ( 6.565887622018943937, 20.16530133659708213, 12.81628187352647430 ) ) ;
#47614 = CARTESIAN_POINT ( 'NONE',  ( 2.791683348922240793, 66.63393115100079456, 7.208316651077764092 ) ) ;
#47615 = CARTESIAN_POINT ( 'NONE',  ( 19.72487221294571569, 52.80223176428831522, -6.499999999999990230 ) ) ;
#47617 = CARTESIAN_POINT ( 'NONE',  ( 0.6178305044545818747, 38.49863466993042493, -9.382169495545419124 ) ) ;
#47616 = CARTESIAN_POINT ( 'NONE',  ( 2.035157376598822676, 57.43868534415484106, -7.964842623401177768 ) ) ;
#47618 = CARTESIAN_POINT ( 'NONE',  ( 10.00000000000000000, 30.55374883491397142, -14.16423886937410082 ) ) ;
#47619 = CARTESIAN_POINT ( 'NONE',  ( 20.88017736071110875, 25.77201867748816966, -2.915334737309920765 ) ) ;
#47620 = FACE_OUTER_BOUND ( 'NONE', #22727, .T. ) ;
#47621 = CARTESIAN_POINT ( 'NONE',  ( 5.076628168052703671, 1.842264484334118047, 8.527530157486179263 ) ) ;
#47622 = CARTESIAN_POINT ( 'NONE',  ( -8.527530157486173934, -13.57440218233254470, 4.923371831947302546 ) ) ;
#47623 = EDGE_CURVE ( 'NONE', #94129, #74647, #39783, .T. ) ;
#47624 = ORIENTED_EDGE ( 'NONE', *, *, #58886, .T. ) ;
#47625 = CARTESIAN_POINT ( 'NONE',  ( 0.000000000000000000, 15.00000000000000000, 0.000000000000000000 ) ) ;
#47626 = SURFACE_SIDE_STYLE ('',( #26113 ) ) ;
#47627 = VERTEX_POINT ( 'NONE', #10754 ) ;
#47628 = CARTESIAN_POINT ( 'NONE',  ( -2.266590686148945544, 1.387082168247301128, -7.082119434687050408 ) ) ;
#47630 = CARTESIAN_POINT ( 'NONE',  ( 12.91533473730993009, 11.60535201082150714, -10.88017736071109987 ) ) ;
#47629 = CARTESIAN_POINT ( 'NONE',  ( 0.5774900079438607392, 8.480352010821505360, 5.440088680355550821 ) ) ;
#47632 = CARTESIAN_POINT ( 'NONE',  ( -1.099225684535947600, -1.293031996736246469, -6.408140936763238038 ) ) ;
#47631 = CARTESIAN_POINT ( 'NONE',  ( 1.472469842513823179, 30.59226448433411960, -4.923371831947296329 ) ) ;
#47633 = DIRECTION ( 'NONE',  ( 0.9366721892484018985, 0.000000000000000000, -0.3502073812594559410 ) ) ;
#47634 = EDGE_CURVE ( 'NONE', #42131, #44141, #85772, .T. ) ;
#47635 = FACE_OUTER_BOUND ( 'NONE', #63668, .T. ) ;
#47636 = VECTOR ( 'NONE', #63953, 1000.000000000000000 ) ;
#47637 = CARTESIAN_POINT ( 'NONE',  ( 3.591859063236763294, 3.290301336597087012, -11.09922568453595026 ) ) ;
#47638 = ORIENTED_EDGE ( 'NONE', *, *, #55589, .T. ) ;
#47639 = CARTESIAN_POINT ( 'NONE',  ( 2.917880565312950480, 45.97041550158063927, -12.26659068614894821 ) ) ;
#47640 = ORIENTED_EDGE ( 'NONE', *, *, #13652, .T. ) ;
#47641 = CARTESIAN_POINT ( 'NONE',  ( 2.917880565312948704, 62.63708216824730357, 12.26659068614894643 ) ) ;
#47642 = ORIENTED_EDGE ( 'NONE', *, *, #56902, .F. ) ;
#47643 = CARTESIAN_POINT ( 'NONE',  ( -0.8801773607111009756, 18.06368534415484106, 1.068504757029289695E-15 ) ) ;
#47644 = STYLED_ITEM ( 'NONE', ( #22931 ), #13115 ) ;
#47645 = CARTESIAN_POINT ( 'NONE',  ( 2.035157376598822676, 42.43868534415483396, -7.964842623401177768 ) ) ;
#47646 = CARTESIAN_POINT ( 'NONE',  ( 19.84674366389459266, 58.71726448433411605, -2.638427012816827677 ) ) ;
#47647 = CARTESIAN_POINT ( 'NONE',  ( 17.96484262340118221, 39.93868534415484106, 7.964842623401181321 ) ) ;
#47648 = CARTESIAN_POINT ( 'NONE',  ( 20.88017736071110875, 65.77201867748817676, -2.915334737309920765 ) ) ;
#47649 = CARTESIAN_POINT ( 'NONE',  ( 7.084665262690076126, 34.10535201082151247, 10.88017736071109987 ) ) ;
#47650 = COLOUR_RGB ( '', 0.08235294, 0.09019608, 0.10196078) ;
#47651 = CIRCLE ( 'NONE', #46087, 0.5000000000000004441 ) ;
#47652 = LINE ( 'NONE', #71637, #26579 ) ;
#47653 = ADVANCED_FACE ( 'NONE', ( #18751 ), #95431, .T. ) ;
#47654 = CARTESIAN_POINT ( 'NONE',  ( 1.472469842513823179, 5.592264484334118713, -4.923371831947296329 ) ) ;
#47655 = CARTESIAN_POINT ( 'NONE',  ( 0.000000000000000000, 0.5000000000000004441, 0.000000000000000000 ) ) ;
#47656 = ORIENTED_EDGE ( 'NONE', *, *, #63110, .T. ) ;
#47657 = DIRECTION ( 'NONE',  ( 1.000000000000000000, 0.000000000000000000, 0.000000000000000000 ) ) ;
#47658 = CARTESIAN_POINT ( 'NONE',  ( 1.472469842513823179, 40.59226448433411605, -4.923371831947296329 ) ) ;
#47660 = EDGE_CURVE ( 'NONE', #1911, #14086, #72608, .T. ) ;
#47659 = CARTESIAN_POINT ( 'NONE',  ( -14.71525861348286313, 0.3640475087720981273, -2.908807992686782029 ) ) ;
#47661 = FILL_AREA_STYLE ('',( #39685 ) ) ;
#47662 = DIRECTION ( 'NONE',  ( 0.9099612708765483227, 0.000000000000000000, -0.4146932426562279783 ) ) ;
#47663 = FACE_OUTER_BOUND ( 'NONE', #82092, .T. ) ;
#47664 = LINE ( 'NONE', #10649, #15552 ) ;
#47665 = CARTESIAN_POINT ( 'NONE',  ( 17.20831665107776587, 54.13393115100079456, -7.208316651077762316 ) ) ;
#47666 = CARTESIAN_POINT ( 'NONE',  ( 24.16423886937409904, 54.09541550158063217, 3.795296366450317205 ) ) ;
#47667 = CARTESIAN_POINT ( 'NONE',  ( 1.472469842513823179, 65.59226448433412315, -4.923371831947296329 ) ) ;
#47668 = ORIENTED_EDGE ( 'NONE', *, *, #78572, .F. ) ;
#47669 = DIRECTION ( 'NONE',  ( 1.000000000000000000, 0.000000000000000000, 0.000000000000000000 ) ) ;
#47670 = CARTESIAN_POINT ( 'NONE',  ( 1.472469842513823179, 21.42559781766745175, 4.923371831947296329 ) ) ;
#47671 = CARTESIAN_POINT ( 'NONE',  ( -2.816281873526471635, 48.91530133659708213, -3.434112377981056508 ) ) ;
#47672 = CARTESIAN_POINT ( 'NONE',  ( 12.63842701281683922, 64.55059781766745175, -9.846743663894590881 ) ) ;
#47673 = CARTESIAN_POINT ( 'NONE',  ( -0.8801773607111009756, 63.06368534415484106, 1.068504757029289695E-15 ) ) ;
#47674 = CARTESIAN_POINT ( 'NONE',  ( 5.500000000000000000, 11.00000000000000000, 6.500000000000000888 ) ) ;
#47675 = EDGE_CURVE ( 'NONE', #4350, #82368, #3561, .T. ) ;
#47676 = ORIENTED_EDGE ( 'NONE', *, *, #3989, .T. ) ;
#47677 = CARTESIAN_POINT ( 'NONE',  ( 6.204703633549690345, 57.84541550158063927, 14.16423886937410082 ) ) ;
#47678 = CARTESIAN_POINT ( 'NONE',  ( 2.603489959281613420, 65.43575266056828355, -6.500000000000031086 ) ) ;
#47679 = CARTESIAN_POINT ( 'NONE',  ( 10.00000000000000178, 34.31368534415484106, 10.88017736071110342 ) ) ;
#47681 = CARTESIAN_POINT ( 'NONE',  ( 7.084665262690076126, 52.02201867748816255, -10.88017736071110164 ) ) ;
#47680 = CARTESIAN_POINT ( 'NONE',  ( -2.816281873526473856, 14.12363466993041961, 9.499525473075851096E-16 ) ) ;
#47682 = DIRECTION ( 'NONE',  ( 0.000000000000000000, 0.000000000000000000, -1.000000000000000000 ) ) ;
#47684 = EDGE_CURVE ( 'NONE', #41376, #98547, #10610, .T. ) ;
#47683 = DIRECTION ( 'NONE',  ( -0.000000000000000000, -1.000000000000000000, -0.000000000000000000 ) ) ;
#47685 = DIRECTION ( 'NONE',  ( -0.000000000000000000, -0.000000000000000000, -1.000000000000000000 ) ) ;
#47686 = CARTESIAN_POINT ( 'NONE',  ( 7.361572987183170547, 52.05059781766745175, 9.846743663894590881 ) ) ;
#47687 = CARTESIAN_POINT ( 'NONE',  ( 17.20831665107776587, 2.883931151000785231, 7.208316651077764980 ) ) ;
#47688 = CARTESIAN_POINT ( 'NONE',  ( -9.422509992056136596, -36.51964798917849464, 5.440088680355559703 ) ) ;
#47689 = CARTESIAN_POINT ( 'NONE',  ( -1.099225684535947600, 3.706968003263753531, -6.408140936763238038 ) ) ;
#47691 = FILL_AREA_STYLE ('',( #85207 ) ) ;
#47690 = CARTESIAN_POINT ( 'NONE',  ( 7.084665262690076126, 7.022018677488170546, -10.88017736071110164 ) ) ;
#47692 = SURFACE_STYLE_USAGE ( .BOTH. , #32678 ) ;
#47693 = CARTESIAN_POINT ( 'NONE',  ( 20.36894250292379382, 33.67874883491396076, 10.36894250292379205 ) ) ;
#47694 = CARTESIAN_POINT ( 'NONE',  ( -4.164238869374098151, 26.59541550158063217, -3.795296366450310543 ) ) ;
#47695 = CARTESIAN_POINT ( 'NONE',  ( 2.917880565312948704, 62.63708216824730357, 12.26659068614894643 ) ) ;
#47696 = CARTESIAN_POINT ( 'NONE',  ( 0.1532563361054100626, 30.80059781766744820, -2.638427012816831230 ) ) ;
#47697 = CARTESIAN_POINT ( 'NONE',  ( 17.20831665107776587, 17.88393115100078745, 7.208316651077764980 ) ) ;
#47698 = CARTESIAN_POINT ( 'NONE',  ( -0.8801773607111008646, 18.27201867748817321, 2.915334737309923430 ) ) ;
#47699 = VERTEX_POINT ( 'NONE', #79638 ) ;
#47700 = CARTESIAN_POINT ( 'NONE',  ( 5.076628168052704559, 35.17559781766745175, -8.527530157486179263 ) ) ;
#47701 = CARTESIAN_POINT ( 'NONE',  ( 17.96484262340118221, 41.18868534415484106, -7.964842623401177768 ) ) ;
#47702 = CARTESIAN_POINT ( 'NONE',  ( 0.1532563361054083140, 56.00893115100078745, 1.131784320476157264E-15 ) ) ;
#47703 = CARTESIAN_POINT ( 'NONE',  ( 2.917880565312948704, 17.63708216824730357, 12.26659068614894643 ) ) ;
#47704 = CARTESIAN_POINT ( 'NONE',  ( -2.189666204609083788, 15.00000000000000888, -14.46180170876169413 ) ) ;
#47705 = CARTESIAN_POINT ( 'NONE',  ( 5.076628168052703671, 11.84226448433411960, 8.527530157486179263 ) ) ;
#47706 = CARTESIAN_POINT ( 'NONE',  ( 19.38216949554541202, 45.99863466993041072, 9.382169495545424454 ) ) ;
#47707 = CARTESIAN_POINT ( 'NONE',  ( 19.84674366389459266, 53.71726448433411605, -2.638427012816827677 ) ) ;
#47708 = VERTEX_POINT ( 'NONE', #48637 ) ;
#47709 = CARTESIAN_POINT ( 'NONE',  ( 8.880000000000000782, 1.019547802438459216, -4.000000000000000000 ) ) ;
#47710 = CARTESIAN_POINT ( 'NONE',  ( 10.00000000000000000, 6.813685344154838397, -10.88017736071110342 ) ) ;
#47711 = CARTESIAN_POINT ( 'NONE',  ( -0.8801773607111008646, 48.27201867748816966, 2.915334737309923430 ) ) ;
#47712 = CARTESIAN_POINT ( 'NONE',  ( -2.266590686148945544, 7.220415501580634832, 7.082119434687048631 ) ) ;
#47713 = CARTESIAN_POINT ( 'NONE',  ( 2.035157376598824452, 68.68868534415484817, 7.964842623401179544 ) ) ;
#47714 = CARTESIAN_POINT ( 'NONE',  ( 10.00000000000000178, 37.25893115100078745, 9.846743663894594434 ) ) ;
#47715 = CARTESIAN_POINT ( 'NONE',  ( -0.8801773607111008646, 18.27201867748817321, 2.915334737309923430 ) ) ;
#47716 = CARTESIAN_POINT ( 'NONE',  ( 18.50749283717775384, 39.69955587570481725, 6.500000000000040856 ) ) ;
#47717 = CARTESIAN_POINT ( 'NONE',  ( 14.92337183194729988, 59.34226448433412315, -8.527530157486177487 ) ) ;
#47718 = AXIS2_PLACEMENT_3D ( 'NONE', #13433, #74923, #73434 ) ;
#47719 = CARTESIAN_POINT ( 'NONE',  ( 0.6178305044545838731, 64.74863466993043914, 9.382169495545420901 ) ) ;
#47720 = ORIENTED_EDGE ( 'NONE', *, *, #11878, .T. ) ;
#47721 = VERTEX_POINT ( 'NONE', #80625 ) ;
#47722 = FACE_OUTER_BOUND ( 'NONE', #2406, .T. ) ;
#47723 = DIRECTION ( 'NONE',  ( -0.000000000000000000, 1.000000000000000000, 0.000000000000000000 ) ) ;
#47724 = CARTESIAN_POINT ( 'NONE',  ( 24.16423886937410614, 39.30374883491396787, 8.672049930838204340E-16 ) ) ;
#47725 = CARTESIAN_POINT ( 'NONE',  ( 2.791683348922237240, 45.38393115100079456, -7.208316651077763204 ) ) ;
#47726 = CARTESIAN_POINT ( 'NONE',  ( 5.076628168052704559, 25.17559781766745175, -8.527530157486179263 ) ) ;
#47727 = LINE ( 'NONE', #95184, #88533 ) ;
#47729 = CARTESIAN_POINT ( 'NONE',  ( 12.63842701281683034, 57.46726448433411605, 9.846743663894596210 ) ) ;
#47728 = CARTESIAN_POINT ( 'NONE',  ( 20.88017736071110875, 15.77201867748817143, -2.915334737309920765 ) ) ;
#47730 = DIRECTION ( 'NONE',  ( -1.000000000000000000, 0.000000000000000000, 0.000000000000000000 ) ) ;
#47731 = CARTESIAN_POINT ( 'NONE',  ( 17.08211943468705840, 60.13708216824729647, -12.26659068614894466 ) ) ;
#47732 = CARTESIAN_POINT ( 'NONE',  ( 0.000000000000000000, 0.000000000000000000, 0.000000000000000000 ) ) ;
#47733 = CARTESIAN_POINT ( 'NONE',  ( -12.00809552683946357, 14.49999999999999822, -8.989195838243713155 ) ) ;
#47734 = CARTESIAN_POINT ( 'NONE',  ( -0.8801773607110991993, 67.85535201082151957, -2.915334737309923874 ) ) ;
#47735 = CARTESIAN_POINT ( 'NONE',  ( 17.20831665107776587, 12.88393115100078390, 7.208316651077764980 ) ) ;
#47736 = CARTESIAN_POINT ( 'NONE',  ( -6.281594481404161989, -39.81112291747235332, 3.999999999999999112 ) ) ;
#47737 = ORIENTED_EDGE ( 'NONE', *, *, #23888, .F. ) ;
#47738 = CARTESIAN_POINT ( 'NONE',  ( 0.000000000000000000, 14.49999999999999822, 0.000000000000000000 ) ) ;
#47739 = ORIENTED_EDGE ( 'NONE', *, *, #60765, .F. ) ;
#47740 = CARTESIAN_POINT ( 'NONE',  ( 18.52753015748618282, 28.92559781766745175, -4.923371831947291888 ) ) ;
#47741 = EDGE_LOOP ( 'NONE', ( #17288, #21930, #17987, #44180, #3496, #35103 ) ) ;
#47742 = CARTESIAN_POINT ( 'NONE',  ( 24.16423886937409904, 19.09541550158063927, 3.795296366450317205 ) ) ;
#47743 = CARTESIAN_POINT ( 'NONE',  ( 2.791683348922237240, 20.38393115100078745, -7.208316651077763204 ) ) ;
#47744 = CARTESIAN_POINT ( 'NONE',  ( 0.5774900079438590739, 42.64701867748816966, -5.440088680355550821 ) ) ;
#47745 = EDGE_CURVE ( 'NONE', #93854, #35809, #6757, .T. ) ;
#47746 = DIRECTION ( 'NONE',  ( 0.000000000000000000, 1.000000000000000000, -0.000000000000000000 ) ) ;
#47747 = ORIENTED_EDGE ( 'NONE', *, *, #69317, .T. ) ;
#47748 = CARTESIAN_POINT ( 'NONE',  ( 2.035157376598822676, 37.43868534415484106, -7.964842623401177768 ) ) ;
#47749 = CARTESIAN_POINT ( 'NONE',  ( 12.60589901313222505, 14.49999999999999112, 8.129656208642151327 ) ) ;
#47750 = CARTESIAN_POINT ( 'NONE',  ( -9.382169495545422677, -6.501365330069580395, -9.382169495545417348 ) ) ;
#47751 = VERTEX_POINT ( 'NONE', #65104 ) ;
#47752 = CARTESIAN_POINT ( 'NONE',  ( -4.164238869374098151, 6.595415501580634832, -3.795296366450310543 ) ) ;
#47753 = ORIENTED_EDGE ( 'NONE', *, *, #24985, .T. ) ;
#47754 = ORIENTED_EDGE ( 'NONE', *, *, #32410, .F. ) ;
#47755 = CARTESIAN_POINT ( 'NONE',  ( 19.38216949554541202, 30.99863466993042138, 9.382169495545424454 ) ) ;
#47756 = AXIS2_PLACEMENT_3D ( 'NONE', #46926, #84454, #92430 ) ;
#47757 = PRESENTATION_STYLE_ASSIGNMENT (( #57217 ) ) ;
#47758 = CARTESIAN_POINT ( 'NONE',  ( 5.076628168052703671, 6.842264484334118713, 8.527530157486179263 ) ) ;
#47759 = DIRECTION ( 'NONE',  ( 0.000000000000000000, 1.000000000000000000, 0.000000000000000000 ) ) ;
#47760 = CARTESIAN_POINT ( 'NONE',  ( 21.09922568453594849, 46.20696800326376064, 6.408140936763242479 ) ) ;
#47761 = PLANE ( 'NONE',  #81485 ) ;
#47762 = CARTESIAN_POINT ( 'NONE',  ( 1.472469842513823179, 31.42559781766745530, 4.923371831947296329 ) ) ;
#47763 = ORIENTED_EDGE ( 'NONE', *, *, #29122, .T. ) ;
#47764 = EDGE_CURVE ( 'NONE', #75142, #84080, #73829, .T. ) ;
#47765 = CARTESIAN_POINT ( 'NONE',  ( 0.000000000000000000, 0.5000000000000004441, 0.000000000000000000 ) ) ;
#47766 = CARTESIAN_POINT ( 'NONE',  ( 19.42250999205614548, 60.98035201082151247, -5.440088680355545492 ) ) ;
#47767 = DIRECTION ( 'NONE',  ( -0.000000000000000000, 1.000000000000000000, -0.000000000000000000 ) ) ;
#47768 = FACE_OUTER_BOUND ( 'NONE', #11498, .T. ) ;
#47769 = CARTESIAN_POINT ( 'NONE',  ( 19.84674366389459266, 8.717264484334116048, -2.638427012816827677 ) ) ;
#47770 = EDGE_CURVE ( 'NONE', #16203, #20878, #13177, .T. ) ;
#47771 = CARTESIAN_POINT ( 'NONE',  ( -4.838527690343430443, 15.00000000000000000, -14.19819177887733375 ) ) ;
#47772 = CARTESIAN_POINT ( 'NONE',  ( 10.00000000000000000, 34.75893115100078745, -9.846743663894594434 ) ) ;
#47773 = CARTESIAN_POINT ( 'NONE',  ( 18.72515096720573879, 35.05509018479936145, 6.499999999999937828 ) ) ;
#47774 = CARTESIAN_POINT ( 'NONE',  ( 13.79529636645030344, 13.26208216824729824, 14.16423886937410614 ) ) ;
#47775 = CARTESIAN_POINT ( 'NONE',  ( 5.076628168052703671, 16.84226448433411960, 8.527530157486179263 ) ) ;
#47776 = CARTESIAN_POINT ( 'NONE',  ( 16.40814093676324603, 22.45696800326375353, -11.09922568453594671 ) ) ;
#47778 = CARTESIAN_POINT ( 'NONE',  ( -7.124967621222336511, -78.82395726652279677, -2.750000000000000888 ) ) ;
#47777 = CARTESIAN_POINT ( 'NONE',  ( 2.148416515056672083, 17.23726573380437443, 6.499999999999988454 ) ) ;
#47779 = CARTESIAN_POINT ( 'NONE',  ( 20.88017736071110875, 45.77201867748816966, -2.915334737309920765 ) ) ;
#47780 = CARTESIAN_POINT ( 'NONE',  ( 19.84674366389459621, 58.50893115100078745, 7.409399052514197653E-17 ) ) ;
#47781 = DIRECTION ( 'NONE',  ( -0.000000000000000000, -1.000000000000000000, -0.000000000000000000 ) ) ;
#47783 = CARTESIAN_POINT ( 'NONE',  ( 17.20831665107776587, 27.88393115100078390, 7.208316651077764980 ) ) ;
#47782 = PRESENTATION_LAYER_ASSIGNMENT (  '', '', ( #46164 ) ) ;
#47784 = CARTESIAN_POINT ( 'NONE',  ( 12.63842701281683034, 27.46726448433411250, 9.846743663894596210 ) ) ;
#47785 = CARTESIAN_POINT ( 'NONE',  ( -0.8801773607110991993, 17.85535201082150536, -2.915334737309923874 ) ) ;
#47786 = CARTESIAN_POINT ( 'NONE',  ( 10.00000000000000178, 20.37363466993042138, 12.81628187352647608 ) ) ;
#47787 = CARTESIAN_POINT ( 'NONE',  ( 17.20831665107776587, 19.13393115100078035, -7.208316651077762316 ) ) ;
#47788 = CARTESIAN_POINT ( 'NONE',  ( -8.000343251535923628, 84.06932101904432386, 4.000000000000000000 ) ) ;
#47789 = CARTESIAN_POINT ( 'NONE',  ( 15.44008868035555793, 21.39701867748817321, -9.422509992056140149 ) ) ;
#47790 = CARTESIAN_POINT ( 'NONE',  ( -0.8801773607111008646, 58.27201867748816966, 2.915334737309923430 ) ) ;
#47791 = DIRECTION ( 'NONE',  ( 0.000000000000000000, 0.000000000000000000, 1.000000000000000000 ) ) ;
#47793 = CARTESIAN_POINT ( 'NONE',  ( -0.8801773607110991993, 12.85535201082150358, -2.915334737309923874 ) ) ;
#47792 = CARTESIAN_POINT ( 'NONE',  ( 12.63842701281683922, 39.55059781766744464, -9.846743663894590881 ) ) ;
#47794 = CARTESIAN_POINT ( 'NONE',  ( 4.559911319644449179, 52.23035201082151247, -9.422509992056141925 ) ) ;
#47796 = PRESENTATION_STYLE_ASSIGNMENT (( #48778 ) ) ;
#47795 = CARTESIAN_POINT ( 'NONE',  ( 17.96484262340118221, 11.18868534415484106, -7.964842623401177768 ) ) ;
#47797 = CARTESIAN_POINT ( 'NONE',  ( 0.1532563361054083140, 21.00893115100078745, 1.131784320476157264E-15 ) ) ;
#47798 = CARTESIAN_POINT ( 'NONE',  ( 10.00000000000000000, 39.75893115100078745, -9.846743663894594434 ) ) ;
#47799 = FACE_OUTER_BOUND ( 'NONE', #72098, .T. ) ;
#47800 = EDGE_CURVE ( 'NONE', #59298, #86107, #57613, .T. ) ;
#47801 = DIRECTION ( 'NONE',  ( 1.000000000000000000, -5.818595309480553908E-17, 0.000000000000000000 ) ) ;
#47802 = CARTESIAN_POINT ( 'NONE',  ( 2.917880565312948704, 27.63708216824730357, 12.26659068614894643 ) ) ;
#47803 = CARTESIAN_POINT ( 'NONE',  ( 5.076628168052704559, 35.17559781766745175, -8.527530157486179263 ) ) ;
#47804 = DIRECTION ( 'NONE',  ( 1.000000000000000000, 0.000000000000000000, 0.000000000000000000 ) ) ;
#47805 = CARTESIAN_POINT ( 'NONE',  ( 19.42250999205614193, 5.147018677488171434, 5.440088680355555262 ) ) ;
#47806 = CARTESIAN_POINT ( 'NONE',  ( 19.84674366389459266, 23.30059781766745530, 2.638427012816836559 ) ) ;
#47808 =( LENGTH_UNIT ( ) NAMED_UNIT ( * ) SI_UNIT ( .MILLI., .METRE. ) );
#47807 = CARTESIAN_POINT ( 'NONE',  ( -6.767445849361338084, 14.63595249122788999, 13.38662304974494077 ) ) ;
#47809 = CARTESIAN_POINT ( 'NONE',  ( 15.44008868035555260, 49.73035201082150536, 9.422509992056143702 ) ) ;
#47811 = CARTESIAN_POINT ( 'NONE',  ( -8.564643372776451713, 0.3640475087720985714, -12.31449893000753093 ) ) ;
#47810 = B_SPLINE_CURVE_WITH_KNOTS ( 'NONE', 3,
 ( #57724, #58204, #88227, #58717, #20731, #36726 ),
 .UNSPECIFIED., .F., .F.,
 ( 4, 2, 4 ),
 ( 3.409110551496127980E-05, 0.0004400426677367858127, 0.0008459942299586103998 ),
 .UNSPECIFIED. ) ;
#47812 = CARTESIAN_POINT ( 'NONE',  ( 10.00000000000000000, 21.81368534415484106, -10.88017736071110342 ) ) ;
#47813 = CARTESIAN_POINT ( 'NONE',  ( 10.00000000000000000, 42.87363466993042493, -12.81628187352647608 ) ) ;
#47814 = CARTESIAN_POINT ( 'NONE',  ( 19.38216949554541202, 5.998634669930420493, 9.382169495545424454 ) ) ;
#47815 = CARTESIAN_POINT ( 'NONE',  ( 0.1532563361054083140, 16.00893115100078390, 1.131784320476157264E-15 ) ) ;
#47816 = VERTEX_POINT ( 'NONE', #78661 ) ;
#47817 = CARTESIAN_POINT ( 'NONE',  ( -2.826948239414023067, 14.76930270348881180, 14.67127868811023639 ) ) ;
#47818 = CARTESIAN_POINT ( 'NONE',  ( 1.983216688680843109, 15.00000000000000000, 14.11131997956739070 ) ) ;
#47819 = CARTESIAN_POINT ( 'NONE',  ( 20.36894250292379738, 54.92874883491396076, -10.36894250292379027 ) ) ;
#47820 = CARTESIAN_POINT ( 'NONE',  ( 2.917880565312948704, 22.63708216824730002, 12.26659068614894643 ) ) ;
#47821 = CARTESIAN_POINT ( 'NONE',  ( -0.8801773607111009756, 23.06368534415484106, 1.068504757029289695E-15 ) ) ;
#47822 = CARTESIAN_POINT ( 'NONE',  ( 15.44008868035555793, 51.39701867748816966, -9.422509992056140149 ) ) ;
#47823 = VECTOR ( 'NONE', #7360, 1000.000000000000000 ) ;
#47824 = CARTESIAN_POINT ( 'NONE',  ( 19.72487221294571569, 47.80223176428831522, -6.499999999999982236 ) ) ;
#47825 = CARTESIAN_POINT ( 'NONE',  ( 2.035157376598822676, 62.43868534415483396, -7.964842623401177768 ) ) ;
#47826 = CARTESIAN_POINT ( 'NONE',  ( 17.20831665107776587, 19.13393115100078035, -7.208316651077762316 ) ) ;
#47827 = CYLINDRICAL_SURFACE ( 'NONE', #92156, 0.2500000000000002220 ) ;
#47828 = CARTESIAN_POINT ( 'NONE',  ( -4.000000000000000000, 37.25000000000000000, 3.750000000000000000 ) ) ;
#47829 = CARTESIAN_POINT ( 'NONE',  ( 12.63842701281683922, 29.55059781766745175, -9.846743663894590881 ) ) ;
#47830 = CARTESIAN_POINT ( 'NONE',  ( 5.076628168052704559, 55.17559781766745175, -8.527530157486179263 ) ) ;
#47831 = CARTESIAN_POINT ( 'NONE',  ( 0.5774900079438607392, 18.48035201082150536, 5.440088680355550821 ) ) ;
#47832 = CARTESIAN_POINT ( 'NONE',  ( 13.43411237798105340, 30.58196800326374998, 12.81628187352647963 ) ) ;
#47833 = CARTESIAN_POINT ( 'NONE',  ( 12.91533473730992121, 49.52201867748817676, 10.88017736071110164 ) ) ;
#47834 = CARTESIAN_POINT ( 'NONE',  ( 0.1532563361054082862, 26.21726448433411605, 2.638427012816831674 ) ) ;
#47836 = CARTESIAN_POINT ( 'NONE',  ( 17.20831665107776587, 2.883931151000785231, 7.208316651077764980 ) ) ;
#47835 = CARTESIAN_POINT ( 'NONE',  ( 10.00000000000000178, 43.05374883491397497, 14.16423886937410082 ) ) ;
#47837 = DIRECTION ( 'NONE',  ( 0.9636304532086191754, 0.000000000000000000, 0.2672383760782702788 ) ) ;
#47838 = CARTESIAN_POINT ( 'NONE',  ( 12.63842701281683922, 54.55059781766745175, -9.846743663894590881 ) ) ;
#47840 = CARTESIAN_POINT ( 'NONE',  ( 20.36894250292379738, 9.928748834913966093, -10.36894250292379027 ) ) ;
#47839 = CARTESIAN_POINT ( 'NONE',  ( 19.84674366389459266, 38.30059781766745175, 2.638427012816836559 ) ) ;
#47841 = CARTESIAN_POINT ( 'NONE',  ( 2.917880565312948704, 22.63708216824730002, 12.26659068614894643 ) ) ;
#47842 = CARTESIAN_POINT ( 'NONE',  ( 10.00000000000000000, 29.75893115100078745, -9.846743663894594434 ) ) ;
#47843 = CARTESIAN_POINT ( 'NONE',  ( 20.88017736071110875, 50.77201867748817676, -2.915334737309920765 ) ) ;
#47844 = CARTESIAN_POINT ( 'NONE',  ( 17.96484262340118221, 9.938685344154837509, 7.964842623401181321 ) ) ;
#47845 = CARTESIAN_POINT ( 'NONE',  ( -0.8801773607111008646, 48.27201867748816966, 2.915334737309923430 ) ) ;
#47846 = CARTESIAN_POINT ( 'NONE',  ( 4.559911319644449179, 28.89701867748817321, 9.422509992056141925 ) ) ;
#47847 = EDGE_LOOP ( 'NONE', ( #60555, #40652, #54533, #77526 ) ) ;
#47848 = CARTESIAN_POINT ( 'NONE',  ( 12.91533473730992121, 39.52201867748817676, 10.88017736071110164 ) ) ;
#47849 = EDGE_LOOP ( 'NONE', ( #27108, #28689, #46173, #84983 ) ) ;
#47850 = CARTESIAN_POINT ( 'NONE',  ( 13.43411237798105340, 55.58196800326374643, 12.81628187352647963 ) ) ;
#47851 = EDGE_CURVE ( 'NONE', #23913, #45067, #10166, .T. ) ;
#47852 = CARTESIAN_POINT ( 'NONE',  ( 12.91533473730992121, 64.52201867748817676, 10.88017736071110164 ) ) ;
#47853 = EDGE_LOOP ( 'NONE', ( #72962, #6569, #55141, #57572, #52659, #48732 ) ) ;
#47854 = CARTESIAN_POINT ( 'NONE',  ( 19.42250999205614548, 45.98035201082150536, -5.440088680355545492 ) ) ;
#47855 = CARTESIAN_POINT ( 'NONE',  ( -0.8801773607111008646, 3.272018677488171434, 2.915334737309923430 ) ) ;
#47856 = CARTESIAN_POINT ( 'NONE',  ( 1.711636803080536451, 26.84492782695771140, -6.499999999999968914 ) ) ;
#47857 = DIRECTION ( 'NONE',  ( 0.000000000000000000, 1.000000000000000000, 0.000000000000000000 ) ) ;
#47858 = CARTESIAN_POINT ( 'NONE',  ( 2.917880565312950480, 55.97041550158063217, -12.26659068614894821 ) ) ;
#47859 = CARTESIAN_POINT ( 'NONE',  ( 18.52753015748617571, 8.092264484334117824, 4.923371831947298993 ) ) ;
#47860 = CARTESIAN_POINT ( 'NONE',  ( 10.00000000000000178, 8.053748834913967869, 14.16423886937410082 ) ) ;
#47861 = CARTESIAN_POINT ( 'NONE',  ( 1.472469842513823179, 11.42559781766745175, 4.923371831947296329 ) ) ;
#47862 = CARTESIAN_POINT ( 'NONE',  ( 20.88017736071110519, 10.56368534415483751, 2.639326808657452039E-16 ) ) ;
#47863 = CARTESIAN_POINT ( 'NONE',  ( 19.84674366389459266, 43.71726448433410894, -2.638427012816827677 ) ) ;
#47864 = EDGE_LOOP ( 'NONE', ( #91223, #85403 ) ) ;
#47865 = CIRCLE ( 'NONE', #17557, 0.5000000000000004441 ) ;
#47866 = CARTESIAN_POINT ( 'NONE',  ( 5.076628168052704559, 45.17559781766745175, -8.527530157486179263 ) ) ;
#47867 = CARTESIAN_POINT ( 'NONE',  ( -14.47650479471824880, 15.00000000000000000, 3.928206833721914482 ) ) ;
#47868 = CARTESIAN_POINT ( 'NONE',  ( 12.91533473730993009, 36.60535201082151247, -10.88017736071109987 ) ) ;
#47869 = CARTESIAN_POINT ( 'NONE',  ( 2.791683348922240793, 56.63393115100078035, 7.208316651077764092 ) ) ;
#47870 = CARTESIAN_POINT ( 'NONE',  ( 19.42250999205614193, 65.14701867748817676, 5.440088680355555262 ) ) ;
#47871 = CARTESIAN_POINT ( 'NONE',  ( 4.559911319644449179, 43.89701867748816966, 9.422509992056141925 ) ) ;
#47872 = AXIS2_PLACEMENT_3D ( 'NONE', #2788, #24293, #32749 ) ;
#47873 = CARTESIAN_POINT ( 'NONE',  ( 12.91533473730993009, 6.605352010821504471, -10.88017736071109987 ) ) ;
#47874 = VECTOR ( 'NONE', #49241, 1000.000000000000000 ) ;
#47875 = EDGE_CURVE ( 'NONE', #39231, #51116, #34116, .T. ) ;
#47876 = CARTESIAN_POINT ( 'NONE',  ( 0.6178305044545818747, 23.49863466993041783, -9.382169495545419124 ) ) ;
#47877 = FACE_OUTER_BOUND ( 'NONE', #90096, .T. ) ;
#47878 = VERTEX_POINT ( 'NONE', #56161 ) ;
#47879 = CARTESIAN_POINT ( 'NONE',  ( 19.38216949554541202, 25.99863466993042138, 9.382169495545424454 ) ) ;
#47880 = CARTESIAN_POINT ( 'NONE',  ( 15.44008868035555260, 19.73035201082150536, 9.422509992056143702 ) ) ;
#47881 = EDGE_CURVE ( 'NONE', #42118, #16779, #18159, .T. ) ;
#47882 = ORIENTED_EDGE ( 'NONE', *, *, #66971, .T. ) ;
#47883 = EDGE_LOOP ( 'NONE', ( #47152, #96208, #13144, #15031, #41882, #58828 ) ) ;
#47884 = VECTOR ( 'NONE', #376, 1000.000000000000000 ) ;
#47885 = CARTESIAN_POINT ( 'NONE',  ( -0.8801773607111009756, 68.06368534415484817, 1.068504757029289695E-15 ) ) ;
#47886 = CARTESIAN_POINT ( 'NONE',  ( 12.63842701281683922, 54.55059781766745175, -9.846743663894590881 ) ) ;
#47888 = CARTESIAN_POINT ( 'NONE',  ( 10.00000000000000178, 37.25893115100078745, 9.846743663894594434 ) ) ;
#47887 = CARTESIAN_POINT ( 'NONE',  ( 14.92337183194729633, 17.67559781766745175, 8.527530157486181039 ) ) ;
#47889 = CARTESIAN_POINT ( 'NONE',  ( -11.02747836460322084, -96.55788089094548354, 3.750000000000000444 ) ) ;
#47890 = CARTESIAN_POINT ( 'NONE',  ( 5.076628168052703671, 26.84226448433411960, 8.527530157486179263 ) ) ;
#47891 = DIRECTION ( 'NONE',  ( -0.1073935270325955676, -0.9942165912674659767, 0.000000000000000000 ) ) ;
#47892 = DIRECTION ( 'NONE',  ( -0.07845909572783862918, 0.000000000000000000, -0.9969173337331285190 ) ) ;
#47894 = CARTESIAN_POINT ( 'NONE',  ( 0.1532563361054083140, 1.008931151000784787, 1.131784320476157264E-15 ) ) ;
#47893 = CARTESIAN_POINT ( 'NONE',  ( 0.1532563361054083140, 31.00893115100078390, 1.131784320476157264E-15 ) ) ;
#47895 = FACE_OUTER_BOUND ( 'NONE', #42128, .T. ) ;
#47897 = ORIENTED_EDGE ( 'NONE', *, *, #1883, .T. ) ;
#47896 = CARTESIAN_POINT ( 'NONE',  ( 0.1532563361054100626, 40.80059781766745886, -2.638427012816831230 ) ) ;
#47898 = CARTESIAN_POINT ( 'NONE',  ( 0.5774900079438607392, 8.480352010821505360, 5.440088680355550821 ) ) ;
#47899 = CARTESIAN_POINT ( 'NONE',  ( 10.00000000000000178, 30.37363466993042138, 12.81628187352647608 ) ) ;
#47900 = CARTESIAN_POINT ( 'NONE',  ( -1.780824192092282265, 14.63606913465075365, -14.89391369643520058 ) ) ;
#47901 = CARTESIAN_POINT ( 'NONE',  ( 20.36894250292379382, 48.67874883491396076, 10.36894250292379205 ) ) ;
#47902 = CARTESIAN_POINT ( 'NONE',  ( 14.92337183194729633, 17.67559781766745175, 8.527530157486181039 ) ) ;
#47903 = CARTESIAN_POINT ( 'NONE',  ( 12.63842701281683922, 4.550597817667451750, -9.846743663894590881 ) ) ;
#47904 = FACE_OUTER_BOUND ( 'NONE', #96224, .T. ) ;
#47905 = CARTESIAN_POINT ( 'NONE',  ( 17.08211943468705130, 38.47041550158063217, 12.26659068614894998 ) ) ;
#47906 = CARTESIAN_POINT ( 'NONE',  ( 0.1532563361054100626, 65.80059781766745175, -2.638427012816831230 ) ) ;
#47907 = CARTESIAN_POINT ( 'NONE',  ( 15.44008868035555793, 11.39701867748817143, -9.422509992056140149 ) ) ;
#47908 = CARTESIAN_POINT ( 'NONE',  ( 13.79529636645031943, 20.34541550158063572, -14.16423886937409904 ) ) ;
#47909 = CARTESIAN_POINT ( 'NONE',  ( 6.204703633549690345, 40.76208216824731778, -14.16423886937410259 ) ) ;
#47910 = CARTESIAN_POINT ( 'NONE',  ( 12.34597252984337956, 14.95037103437615755, -8.076773567935822129 ) ) ;
#47912 = CARTESIAN_POINT ( 'NONE',  ( 7.361572987183169658, 54.96726448433413026, -9.846743663894592657 ) ) ;
#47911 = CARTESIAN_POINT ( 'NONE',  ( -3.384800920124265033, 0.2306972965111788454, 14.55270344038004815 ) ) ;
#47913 = ORIENTED_EDGE ( 'NONE', *, *, #12173, .T. ) ;
#47914 = CARTESIAN_POINT ( 'NONE',  ( 0.5774900079438590739, 37.64701867748817676, -5.440088680355550821 ) ) ;
#47915 = CARTESIAN_POINT ( 'NONE',  ( 10.82344394350231198, 14.95077488074853456, -10.02492699998876979 ) ) ;
#47916 = CARTESIAN_POINT ( 'NONE',  ( 19.50000000000000711, 98.59912998021081876, -4.999999999999999112 ) ) ;
#47917 = ADVANCED_FACE ( 'NONE', ( #35102 ), #71162, .T. ) ;
#47918 = CARTESIAN_POINT ( 'NONE',  ( 18.52753015748617571, 43.09226448433412315, 4.923371831947298993 ) ) ;
#47919 = CARTESIAN_POINT ( 'NONE',  ( 17.85999999999999588, 33.98752635800203592, -10.00000000000000000 ) ) ;
#47920 = CARTESIAN_POINT ( 'NONE',  ( -14.16423886937409726, -2.987917831752693765, 3.795296366450320757 ) ) ;
#47921 = CARTESIAN_POINT ( 'NONE',  ( 18.52753015748617571, 43.09226448433412315, 4.923371831947298993 ) ) ;
#47922 = CARTESIAN_POINT ( 'NONE',  ( 2.791683348922237240, 65.38393115100078035, -7.208316651077763204 ) ) ;
#47923 = VERTEX_POINT ( 'NONE', #72123 ) ;
#47924 = CARTESIAN_POINT ( 'NONE',  ( 24.16423886937410614, 9.303748834913967869, 8.672049930838204340E-16 ) ) ;
#47925 = DIRECTION ( 'NONE',  ( -1.000000000000000000, 0.000000000000000000, 0.000000000000000000 ) ) ;
#47927 = CARTESIAN_POINT ( 'NONE',  ( 8.880000000000020322, 79.82179676972448590, 6.250000000000000000 ) ) ;
#47926 = CARTESIAN_POINT ( 'NONE',  ( -5.559677335903118411, -36.09286816789838781, -2.500000000000000888 ) ) ;
#47928 = CARTESIAN_POINT ( 'NONE',  ( -4.164238869374099039, 66.80374883491396076, 8.674139862899312516E-16 ) ) ;
#47929 = CARTESIAN_POINT ( 'NONE',  ( 19.38216949554541557, 27.24863466993041783, -9.382169495545420901 ) ) ;
#47930 = CARTESIAN_POINT ( 'NONE',  ( -8.124115902427741176, 75.04369783535875627, 3.000000000000000000 ) ) ;
#47931 = CARTESIAN_POINT ( 'NONE',  ( 7.361572987183170547, 2.050597817667451750, 9.846743663894590881 ) ) ;
#47932 = ADVANCED_FACE ( 'NONE', ( #56641 ), #54631, .T. ) ;
#47933 = CIRCLE ( 'NONE', #46380, 6.999999999999999112 ) ;
#47934 = SURFACE_SIDE_STYLE ('',( #34899 ) ) ;
#47935 = CARTESIAN_POINT ( 'NONE',  ( -4.164238869374098151, 66.59541550158060375, -3.795296366450310543 ) ) ;
#47936 = FACE_OUTER_BOUND ( 'NONE', #3555, .T. ) ;
#47937 = CARTESIAN_POINT ( 'NONE',  ( 7.084665262690076126, 27.02201867748817676, -10.88017736071110164 ) ) ;
#47938 = CARTESIAN_POINT ( 'NONE',  ( 15.44008868035555260, 34.73035201082151247, 9.422509992056143702 ) ) ;
#47939 = CARTESIAN_POINT ( 'NONE',  ( 19.84674366389459266, 63.30059781766745886, 2.638427012816836559 ) ) ;
#47940 = CARTESIAN_POINT ( 'NONE',  ( 1.472469842513823179, 50.59226448433411605, -4.923371831947296329 ) ) ;
#47941 = CARTESIAN_POINT ( 'NONE',  ( -42.84233569985355672, 106.9556388676848258, -5.000000000000000888 ) ) ;
#47942 = CARTESIAN_POINT ( 'NONE',  ( 5.076628168052704559, 5.175597817667451750, -8.527530157486179263 ) ) ;
#47944 = VERTEX_POINT ( 'NONE', #3651 ) ;
#47943 = VECTOR ( 'NONE', #52809, 1000.000000000000000 ) ;
#47945 = CARTESIAN_POINT ( 'NONE',  ( 15.44008868035555793, 31.39701867748817676, -9.422509992056140149 ) ) ;
#47946 = CARTESIAN_POINT ( 'NONE',  ( 19.38216949554541557, 27.24863466993041783, -9.382169495545420901 ) ) ;
#47947 = CARTESIAN_POINT ( 'NONE',  ( -11.36220558719268325, 15.00000000000000000, -9.008345252852777207 ) ) ;
#47948 = CARTESIAN_POINT ( 'NONE',  ( 7.361572987183169658, 59.96726448433410894, -9.846743663894592657 ) ) ;
#47949 = CARTESIAN_POINT ( 'NONE',  ( 15.44008868035555260, 49.73035201082150536, 9.422509992056143702 ) ) ;
#47950 = CARTESIAN_POINT ( 'NONE',  ( 2.791683348922237240, 10.38393115100078390, -7.208316651077763204 ) ) ;
#47951 = CARTESIAN_POINT ( 'NONE',  ( 10.00000000000000178, 40.37363466993042493, 12.81628187352647608 ) ) ;
#47953 = FILL_AREA_STYLE ('',( #17487 ) ) ;
#47952 = CARTESIAN_POINT ( 'NONE',  ( -0.8801773607111009756, 68.06368534415484817, 1.068504757029289695E-15 ) ) ;
#47954 = CARTESIAN_POINT ( 'NONE',  ( 18.50749283717779647, 54.69955587570481725, 6.499999999999920952 ) ) ;
#47955 = ORIENTED_EDGE ( 'NONE', *, *, #61757, .F. ) ;
#47956 = B_SPLINE_CURVE_WITH_KNOTS ( 'NONE', 3,
 ( #23723, #53212, #67733, #84220 ),
 .UNSPECIFIED., .F., .F.,
 ( 4, 4 ),
 ( 3.227937720230791035E-17, 0.002392975128318423038 ),
 .UNSPECIFIED. ) ;
#47957 = CARTESIAN_POINT ( 'NONE',  ( 1.711636803080541558, 16.84492782695771496, -6.499999999999984901 ) ) ;
#47958 = CARTESIAN_POINT ( 'NONE',  ( 2.035157376598822676, 7.438685344154837509, -7.964842623401177768 ) ) ;
#47960 = CARTESIAN_POINT ( 'NONE',  ( -2.266590686148945544, 17.22041550158063572, 7.082119434687048631 ) ) ;
#47959 = CARTESIAN_POINT ( 'NONE',  ( 21.09922568453595559, 52.04030133659708923, -6.408140936763230044 ) ) ;
#47961 = CARTESIAN_POINT ( 'NONE',  ( 19.84674366389459621, 13.50893115100078568, 7.409399052514197653E-17 ) ) ;
#47962 = CARTESIAN_POINT ( 'NONE',  ( 12.91533473730992121, 9.522018677488171434, 10.88017736071110164 ) ) ;
#47963 = AXIS2_PLACEMENT_3D ( 'NONE', #83226, #53707, #67239 ) ;
#47964 = CARTESIAN_POINT ( 'NONE',  ( 18.52753015748617571, 18.09226448433411960, 4.923371831947298993 ) ) ;
#47965 = CARTESIAN_POINT ( 'NONE',  ( 13.79529636645030344, 53.26208216824730357, 14.16423886937410614 ) ) ;
#47966 = ORIENTED_EDGE ( 'NONE', *, *, #51780, .T. ) ;
#47967 = CARTESIAN_POINT ( 'NONE',  ( 2.035157376598824452, 3.688685344154837953, 7.964842623401179544 ) ) ;
#47968 = EDGE_CURVE ( 'NONE', #61498, #49656, #43501, .T. ) ;
#47969 = CARTESIAN_POINT ( 'NONE',  ( -0.8801773607111009756, 18.06368534415484106, 1.068504757029289695E-15 ) ) ;
#47970 = CARTESIAN_POINT ( 'NONE',  ( 1.274849032794324932, 32.55509018479936145, -6.500000000000021316 ) ) ;
#47971 = EDGE_LOOP ( 'NONE', ( #15113, #59763, #43085, #29754, #70137, #42678 ) ) ;
#47972 = ORIENTED_EDGE ( 'NONE', *, *, #12449, .F. ) ;
#47973 = CARTESIAN_POINT ( 'NONE',  ( 12.91533473730993009, 16.60535201082150891, -10.88017736071109987 ) ) ;
#47974 = CARTESIAN_POINT ( 'NONE',  ( 20.88017736071110164, 15.35535201082150358, 2.915334737309930979 ) ) ;
#47975 = CARTESIAN_POINT ( 'NONE',  ( 1.472469842513823179, 56.42559781766745886, 4.923371831947296329 ) ) ;
#47976 = CIRCLE ( 'NONE', #8093, 14.49999999999999822 ) ;
#47977 = CARTESIAN_POINT ( 'NONE',  ( 0.3093388210927642268, 0.5000000000000004441, -14.99680997725065978 ) ) ;
#47979 = CARTESIAN_POINT ( 'NONE',  ( 17.08211943468705130, 18.47041550158063572, 12.26659068614894998 ) ) ;
#47978 = DIRECTION ( 'NONE',  ( -0.000000000000000000, 0.000000000000000000, -1.000000000000000000 ) ) ;
#47980 = CARTESIAN_POINT ( 'NONE',  ( -0.8801773607111008646, 23.27201867748817676, 2.915334737309923430 ) ) ;
#47981 = CARTESIAN_POINT ( 'NONE',  ( 19.42250999205614193, 20.14701867748817321, 5.440088680355555262 ) ) ;
#47982 = EDGE_CURVE ( 'NONE', #93214, #25445, #1062, .T. ) ;
#47983 = CARTESIAN_POINT ( 'NONE',  ( 1.472469842513823179, 50.59226448433411605, -4.923371831947296329 ) ) ;
#47984 = DIRECTION ( 'NONE',  ( 0.000000000000000000, 0.000000000000000000, 1.000000000000000000 ) ) ;
#47985 = CARTESIAN_POINT ( 'NONE',  ( 7.361572987183169658, 29.96726448433411960, -9.846743663894592657 ) ) ;
#47986 = CARTESIAN_POINT ( 'NONE',  ( -8.000000000000000000, 80.32179676972448590, 4.250000000000000000 ) ) ;
#47987 = CARTESIAN_POINT ( 'NONE',  ( 19.84674366389459266, 3.300597817667451750, 2.638427012816836559 ) ) ;
#47988 = CARTESIAN_POINT ( 'NONE',  ( 9.846743663894590881, 28.30059781766746951, 2.638427012816828565 ) ) ;
#47989 = EDGE_LOOP ( 'NONE', ( #46459, #71738, #66292, #85037 ) ) ;
#47990 =( LENGTH_UNIT ( ) NAMED_UNIT ( * ) SI_UNIT ( .MILLI., .METRE. ) );
#47991 = CARTESIAN_POINT ( 'NONE',  ( 14.92337183194729633, 12.67559781766745353, 8.527530157486181039 ) ) ;
#47992 = CARTESIAN_POINT ( 'NONE',  ( 0.6178305044545818747, -1.501365330069579951, -9.382169495545419124 ) ) ;
#47994 = CARTESIAN_POINT ( 'NONE',  ( -0.8801773607110991993, 47.85535201082150536, -2.915334737309923874 ) ) ;
#47993 = CARTESIAN_POINT ( 'NONE',  ( -0.8801773607111008646, 43.27201867748817676, 2.915334737309923430 ) ) ;
#47996 = CARTESIAN_POINT ( 'NONE',  ( 13.43411237798106583, 47.66530133659709634, -12.81628187352647252 ) ) ;
#47995 = CARTESIAN_POINT ( 'NONE',  ( 19.42250999205614193, 5.147018677488171434, 5.440088680355555262 ) ) ;
#47997 = CARTESIAN_POINT ( 'NONE',  ( 10.00000000000000000, 20.55374883491396787, -14.16423886937410082 ) ) ;
#47998 = COLOUR_RGB ( '', 0.31764706, 0.68627451, 0.89019608) ;
#47999 = CARTESIAN_POINT ( 'NONE',  ( 22.81628187352647785, 56.62363466993042493, 6.195893100308588602E-16 ) ) ;
#48000 = VERTEX_POINT ( 'NONE', #97623 ) ;
#48001 = B_SPLINE_CURVE_WITH_KNOTS ( 'NONE', 3,
 ( #44300, #84301, #44791, #38303, #90285, #61763 ),
 .UNSPECIFIED., .F., .F.,
 ( 4, 2, 4 ),
 ( 6.992893892674702526E-18, 0.0002605067024381006627, 0.0005210134048761942780 ),
 .UNSPECIFIED. ) ;
#48002 = CARTESIAN_POINT ( 'NONE',  ( 7.361572987183169658, 59.96726448433410894, -9.846743663894592657 ) ) ;
#48003 = CARTESIAN_POINT ( 'NONE',  ( -0.8801773607111008646, 23.27201867748817676, 2.915334737309923430 ) ) ;
#48004 = EDGE_CURVE ( 'NONE', #53609, #22386, #82590, .T. ) ;
#48005 = ORIENTED_EDGE ( 'NONE', *, *, #81318, .T. ) ;
#48006 = CARTESIAN_POINT ( 'NONE',  ( 18.52753015748618282, 8.925597817667451750, -4.923371831947291888 ) ) ;
#48007 = DIRECTION ( 'NONE',  ( 0.000000000000000000, 0.000000000000000000, 1.000000000000000000 ) ) ;
#48008 = CARTESIAN_POINT ( 'NONE',  ( 17.20831665107776587, 7.883931151000784787, 7.208316651077764980 ) ) ;
#48009 = CARTESIAN_POINT ( 'NONE',  ( 0.1532563361054083140, 1.008931151000784787, 1.131784320476157264E-15 ) ) ;
#48010 =( LENGTH_UNIT ( ) NAMED_UNIT ( * ) SI_UNIT ( .MILLI., .METRE. ) );
#48012 = DIRECTION ( 'NONE',  ( 1.000000000000000000, 0.000000000000000000, 0.000000000000000000 ) ) ;
#48011 = CARTESIAN_POINT ( 'NONE',  ( 10.00000000000000000, 61.81368534415484106, -10.88017736071110342 ) ) ;
#48013 = CARTESIAN_POINT ( 'NONE',  ( 7.084665262690076126, 67.02201867748817676, -10.88017736071110164 ) ) ;
#48015 = ORIENTED_EDGE ( 'NONE', *, *, #84933, .F. ) ;
#48014 = CARTESIAN_POINT ( 'NONE',  ( 12.63842701281683034, 7.467264484334118713, 9.846743663894596210 ) ) ;
#48016 = DIRECTION ( 'NONE',  ( -1.257402221000611116E-16, 1.000000000000000000, -0.000000000000000000 ) ) ;
#48017 = CARTESIAN_POINT ( 'NONE',  ( 10.00000000000000000, 54.75893115100078745, -9.846743663894594434 ) ) ;
#48018 = ORIENTED_EDGE ( 'NONE', *, *, #67474, .T. ) ;
#48019 = VERTEX_POINT ( 'NONE', #66603 ) ;
#48020 = DIRECTION ( 'NONE',  ( -0.000000000000000000, -1.000000000000000000, -0.000000000000000000 ) ) ;
#48021 = CARTESIAN_POINT ( 'NONE',  ( 22.81628187352648496, 56.83196800326374643, -3.434112377981050290 ) ) ;
#48022 =( NAMED_UNIT ( * ) SI_UNIT ( $, .STERADIAN. ) SOLID_ANGLE_UNIT ( ) );
#48023 = CARTESIAN_POINT ( 'NONE',  ( 20.36894250292379738, 19.92874883491396787, -10.36894250292379027 ) ) ;
#48024 = CARTESIAN_POINT ( 'NONE',  ( -0.1503990784575328643, 45.12777174578613426, 6.262539305110068177 ) ) ;
#48026 = CARTESIAN_POINT ( 'NONE',  ( 15.44008868035555260, 64.73035201082151957, 9.422509992056143702 ) ) ;
#48025 =( NAMED_UNIT ( * ) SI_UNIT ( $, .STERADIAN. ) SOLID_ANGLE_UNIT ( ) );
#48027 = CARTESIAN_POINT ( 'NONE',  ( 15.44008868035555260, 24.73035201082150891, 9.422509992056143702 ) ) ;
#48028 = FACE_OUTER_BOUND ( 'NONE', #9648, .T. ) ;
#48029 = ORIENTED_EDGE ( 'NONE', *, *, #50484, .T. ) ;
#48030 = CARTESIAN_POINT ( 'NONE',  ( 10.00000000000000178, 22.25893115100078745, 9.846743663894594434 ) ) ;
#48031 = CARTESIAN_POINT ( 'NONE',  ( 16.40814093676324603, 37.45696800326376064, -11.09922568453594671 ) ) ;
#48032 = CARTESIAN_POINT ( 'NONE',  ( 2.791683348922240793, 41.63393115100078745, 7.208316651077764092 ) ) ;
#48033 = PLANE ( 'NONE',  #1149 ) ;
#48034 = EDGE_CURVE ( 'NONE', #46342, #46043, #20616, .T. ) ;
#48035 = CARTESIAN_POINT ( 'NONE',  ( 3.591859063236763294, 33.29030133659708213, -11.09922568453595026 ) ) ;
#48036 = CARTESIAN_POINT ( 'NONE',  ( 0.1034006766821432000, 15.00000000000000000, 14.49963131600458688 ) ) ;
#48037 = B_SPLINE_CURVE_WITH_KNOTS ( 'NONE', 3,
 ( #89856, #65375, #42889, #80886, #88387, #44354 ),
 .UNSPECIFIED., .F., .F.,
 ( 4, 2, 4 ),
 ( 7.909150811748204484E-18, 0.0002626113303185971786, 0.0005252226606371864425 ),
 .UNSPECIFIED. ) ;
#48038 = CARTESIAN_POINT ( 'NONE',  ( 7.361572987183170547, 32.05059781766745175, 9.846743663894590881 ) ) ;
#48039 = CARTESIAN_POINT ( 'NONE',  ( 10.00000000000000000, 15.55374883491396787, -14.16423886937410082 ) ) ;
#48040 = ORIENTED_EDGE ( 'NONE', *, *, #19256, .F. ) ;
#48041 = CARTESIAN_POINT ( 'NONE',  ( -0.8801773607111009756, 33.06368534415484106, 1.068504757029289695E-15 ) ) ;
#48042 = CARTESIAN_POINT ( 'NONE',  ( -0.3689425029237898834, 31.17874883491396787, -10.36894250292378850 ) ) ;
#48043 = CARTESIAN_POINT ( 'NONE',  ( 0.1532563361054100626, 50.80059781766745175, -2.638427012816831230 ) ) ;
#48044 = CARTESIAN_POINT ( 'NONE',  ( 5.076628168052704559, 15.17559781766745175, -8.527530157486179263 ) ) ;
#48046 = LINE ( 'NONE', #78560, #65583 ) ;
#48045 = CARTESIAN_POINT ( 'NONE',  ( -2.816281873526473856, 54.33196800326376064, 3.434112377981055619 ) ) ;
#48047 = CARTESIAN_POINT ( 'NONE',  ( 4.559911319644449179, 23.89701867748817321, 9.422509992056141925 ) ) ;
#48048 = CARTESIAN_POINT ( 'NONE',  ( 10.00000000000000000, 17.87363466993041783, -12.81628187352647608 ) ) ;
#48049 = CARTESIAN_POINT ( 'NONE',  ( 16.40814093676323893, 20.79030133659708923, 11.09922568453595026 ) ) ;
#48050 = CARTESIAN_POINT ( 'NONE',  ( 0.1532563361054083140, 46.00893115100079456, 1.131784320476157264E-15 ) ) ;
#48051 = CARTESIAN_POINT ( 'NONE',  ( 5.440088680355549045, -3.602981322511821016, -9.422509992056141925 ) ) ;
#48052 = CARTESIAN_POINT ( 'NONE',  ( -2.816281873526473856, 44.12363466993042493, 9.499525473075851096E-16 ) ) ;
#48053 = PLANE ( 'NONE',  #517 ) ;
#48055 = DIRECTION ( 'NONE',  ( 0.000000000000000000, 0.000000000000000000, 1.000000000000000000 ) ) ;
#48054 = CARTESIAN_POINT ( 'NONE',  ( 4.559911319644449179, 52.23035201082151247, -9.422509992056141925 ) ) ;
#48056 = AXIS2_PLACEMENT_3D ( 'NONE', #58722, #58209, #88726 ) ;
#48057 = CARTESIAN_POINT ( 'NONE',  ( -11.38910255664659310, -77.84149852289132809, 4.000000000000000000 ) ) ;
#48058 = CARTESIAN_POINT ( 'NONE',  ( -3.999999999999999112, 78.07179676972445748, 6.500000000000000888 ) ) ;
#48059 = CARTESIAN_POINT ( 'NONE',  ( 2.035157376598822676, 57.43868534415484106, -7.964842623401177768 ) ) ;
#48060 = TOROIDAL_SURFACE ( 'NONE', #65691, 14.49999999999999822, 0.5000000000000000000 ) ;
#48061 = CARTESIAN_POINT ( 'NONE',  ( 0.5774900079438607392, 58.48035201082151247, 5.440088680355550821 ) ) ;
#48062 = DIRECTION ( 'NONE',  ( -1.000000000000000000, 0.000000000000000000, 0.000000000000000000 ) ) ;
#48063 = LINE ( 'NONE', #71084, #50797 ) ;
#48064 = CARTESIAN_POINT ( 'NONE',  ( -0.8801773607111008646, 8.272018677488171434, 2.915334737309923430 ) ) ;
#48065 = CARTESIAN_POINT ( 'NONE',  ( 7.361572987183170547, 67.05059781766746596, 9.846743663894590881 ) ) ;
#48067 = CARTESIAN_POINT ( 'NONE',  ( -8.606322355891181886, 15.00000000000000000, -11.66967075398817322 ) ) ;
#48066 = CARTESIAN_POINT ( 'NONE',  ( 0.5774900079438607392, 18.48035201082150536, 5.440088680355550821 ) ) ;
#48068 = FACE_OUTER_BOUND ( 'NONE', #90, .T. ) ;
#48069 = AXIS2_PLACEMENT_3D ( 'NONE', #84260, #94561, #26079 ) ;
#48070 = CARTESIAN_POINT ( 'NONE',  ( 10.00000000000000000, 22.87363466993042138, -12.81628187352647608 ) ) ;
#48071 = ORIENTED_EDGE ( 'NONE', *, *, #38181, .T. ) ;
#48072 = CARTESIAN_POINT ( 'NONE',  ( 20.88017736071110875, 45.77201867748816966, -2.915334737309920765 ) ) ;
#48073 = CARTESIAN_POINT ( 'NONE',  ( 1.472469842513823179, 40.59226448433411605, -4.923371831947296329 ) ) ;
#48075 = LINE ( 'NONE', #92597, #68546 ) ;
#48074 = CARTESIAN_POINT ( 'NONE',  ( 16.40814093676324603, 7.456968003263754419, -11.09922568453594671 ) ) ;
#48076 = CARTESIAN_POINT ( 'NONE',  ( 10.00000000000000000, 26.81368534415484106, -10.88017736071110342 ) ) ;
#48077 = CARTESIAN_POINT ( 'NONE',  ( 2.035157376598822676, 37.43868534415484106, -7.964842623401177768 ) ) ;
#48078 = CARTESIAN_POINT ( 'NONE',  ( 2.917880565312950480, 50.97041550158064638, -12.26659068614894821 ) ) ;
#48079 = CARTESIAN_POINT ( 'NONE',  ( 19.84674366389459266, 43.30059781766744464, 2.638427012816836559 ) ) ;
#48080 = CARTESIAN_POINT ( 'NONE',  ( 7.084665262690076126, 54.10535201082151247, 10.88017736071109987 ) ) ;
#48081 = SURFACE_STYLE_FILL_AREA ( #35040 ) ;
#48082 = CARTESIAN_POINT ( 'NONE',  ( -4.164238869374099039, 16.80374883491396787, 8.674139862899312516E-16 ) ) ;
#48083 = EDGE_CURVE ( 'NONE', #47721, #59353, #29570, .T. ) ;
#48084 = CARTESIAN_POINT ( 'NONE',  ( -9.402796353261216211, 0.3639308891339976815, 11.68706210897754083 ) ) ;
#48085 = CARTESIAN_POINT ( 'NONE',  ( 0.1532563361054083140, 66.00893115100079456, 1.131784320476157264E-15 ) ) ;
#48087 = ORIENTED_EDGE ( 'NONE', *, *, #25464, .F. ) ;
#48086 = ADVANCED_FACE ( 'NONE', ( #21108 ), #52096, .F. ) ;
#48088 = ORIENTED_EDGE ( 'NONE', *, *, #55233, .T. ) ;
#48089 = CARTESIAN_POINT ( 'NONE',  ( 2.917880565312948704, 47.63708216824730357, 12.26659068614894643 ) ) ;
#48090 = CARTESIAN_POINT ( 'NONE',  ( 13.79529636645031943, 40.34541550158063217, -14.16423886937409904 ) ) ;
#48091 = CARTESIAN_POINT ( 'NONE',  ( 12.63842701281683034, 17.46726448433411250, 9.846743663894596210 ) ) ;
#48092 = CARTESIAN_POINT ( 'NONE',  ( -2.816281873526471635, 18.91530133659708213, -3.434112377981056508 ) ) ;
#48093 = CARTESIAN_POINT ( 'NONE',  ( 2.791683348922237240, 65.38393115100078035, -7.208316651077763204 ) ) ;
#48094 = CARTESIAN_POINT ( 'NONE',  ( -8.000000000000000000, 1.019547802438466100, 3.750000000000000000 ) ) ;
#48096 = CARTESIAN_POINT ( 'NONE',  ( -1.099225684535947600, 28.70696800326375353, -6.408140936763238038 ) ) ;
#48095 = CARTESIAN_POINT ( 'NONE',  ( 12.91533473730992121, 64.52201867748817676, 10.88017736071110164 ) ) ;
#48097 = CARTESIAN_POINT ( 'NONE',  ( 10.00000000000000178, 33.05374883491396787, 14.16423886937410082 ) ) ;
#48098 = ADVANCED_FACE ( 'NONE', ( #36096 ), #53065, .T. ) ;
#48099 = CARTESIAN_POINT ( 'NONE',  ( 17.96484262340118221, 29.93868534415484106, 7.964842623401181321 ) ) ;
#48100 = EDGE_CURVE ( 'NONE', #47321, #66421, #28100, .T. ) ;
#48101 = DIRECTION ( 'NONE',  ( -1.000000000000000000, 0.000000000000000000, 0.000000000000000000 ) ) ;
#48102 = CARTESIAN_POINT ( 'NONE',  ( 2.035157376598824452, 68.68868534415484817, 7.964842623401179544 ) ) ;
#48103 = CARTESIAN_POINT ( 'NONE',  ( 8.527530157486179263, -11.90773551566587329, 4.923371831947292776 ) ) ;
#48104 = CARTESIAN_POINT ( 'NONE',  ( 0.1532563361054082862, 6.217264484334118713, 2.638427012816831674 ) ) ;
#48105 = ORIENTED_EDGE ( 'NONE', *, *, #12449, .T. ) ;
#48106 = FACE_OUTER_BOUND ( 'NONE', #26825, .T. ) ;
#48107 = CARTESIAN_POINT ( 'NONE',  ( 20.15039907845753220, 57.62777174578613426, -6.262539305110077947 ) ) ;
#48108 = ORIENTED_EDGE ( 'NONE', *, *, #19903, .F. ) ;
#48110 = CARTESIAN_POINT ( 'NONE',  ( 20.88017736071110164, 5.355352010821503583, 2.915334737309930979 ) ) ;
#48109 = CARTESIAN_POINT ( 'NONE',  ( 2.035157376598822676, 7.438685344154837509, -7.964842623401177768 ) ) ;
#48112 = CARTESIAN_POINT ( 'NONE',  ( -1.099225684535947600, -0.4596986634029132657, 6.408140936763237150 ) ) ;
#48111 = CARTESIAN_POINT ( 'NONE',  ( 7.361572987183169658, 29.96726448433411960, -9.846743663894592657 ) ) ;
#48113 = EDGE_CURVE ( 'NONE', #18352, #97076, #67601, .T. ) ;
#48114 = FACE_OUTER_BOUND ( 'NONE', #27822, .T. ) ;
#48115 = CIRCLE ( 'NONE', #14592, 14.49999999999999822 ) ;
#48116 = DIRECTION ( 'NONE',  ( -0.000000000000000000, -1.000000000000000000, -0.000000000000000000 ) ) ;
#48117 = AXIS2_PLACEMENT_3D ( 'NONE', #77935, #18922, #56429 ) ;
#48118 = CARTESIAN_POINT ( 'NONE',  ( 10.00000000000000000, 7.873634669930421381, -12.81628187352647608 ) ) ;
#48119 = VERTEX_POINT ( 'NONE', #81106 ) ;
#48120 = CARTESIAN_POINT ( 'NONE',  ( -2.266590686148945544, 46.38708216824730357, -7.082119434687050408 ) ) ;
#48121 = ORIENTED_EDGE ( 'NONE', *, *, #21004, .T. ) ;
#48122 = ADVANCED_FACE ( 'NONE', ( #58601 ), #28601, .F. ) ;
#48123 = CARTESIAN_POINT ( 'NONE',  ( -2.266590686148945544, 51.38708216824730357, -7.082119434687050408 ) ) ;
#48124 = VERTEX_POINT ( 'NONE', #45078 ) ;
#48125 = CARTESIAN_POINT ( 'NONE',  ( 20.88017736071110519, 40.56368534415484106, 2.639326808657452039E-16 ) ) ;
#48126 = CARTESIAN_POINT ( 'NONE',  ( 2.035157376598822676, 37.43868534415484106, -7.964842623401177768 ) ) ;
#48127 = CARTESIAN_POINT ( 'NONE',  ( -0.8801773607110991993, 37.85535201082151247, -2.915334737309923874 ) ) ;
#48128 = CARTESIAN_POINT ( 'NONE',  ( 4.559911319644449179, 62.23035201082150536, -9.422509992056141925 ) ) ;
#48129 = CONICAL_SURFACE ( 'NONE', #5036, 1.249999999999987121, 1.029744258676652979 ) ;
#48130 = CARTESIAN_POINT ( 'NONE',  ( 7.084665262690076126, 24.10535201082150181, 10.88017736071109987 ) ) ;
#48131 = EDGE_CURVE ( 'NONE', #11431, #86051, #49906, .T. ) ;
#48133 = CONICAL_SURFACE ( 'NONE', #294, 13.74999999999999467, 0.7853981633974458365 ) ;
#48132 = FACE_OUTER_BOUND ( 'NONE', #98246, .T. ) ;
#48134 = CARTESIAN_POINT ( 'NONE',  ( 10.00000000000000000, 19.75893115100078390, -9.846743663894594434 ) ) ;
#48135 = CARTESIAN_POINT ( 'NONE',  ( 19.72487221294571214, 2.802231764288312998, -6.500000000000001776 ) ) ;
#48136 = ORIENTED_EDGE ( 'NONE', *, *, #24195, .F. ) ;
#48137 = DIRECTION ( 'NONE',  ( -0.000000000000000000, -0.000000000000000000, 1.000000000000000000 ) ) ;
#48138 = CARTESIAN_POINT ( 'NONE',  ( 14.92337183194729988, 49.34226448433411605, -8.527530157486177487 ) ) ;
#48139 = DIRECTION ( 'NONE',  ( 1.000000000000000000, 0.000000000000000000, 0.000000000000000000 ) ) ;
#48140 = PRESENTATION_LAYER_ASSIGNMENT (  '', '', ( #35366 ) ) ;
#48141 = B_SPLINE_CURVE_WITH_KNOTS ( 'NONE', 3,
 ( #85686, #70691, #16702, #20012, #17693, #73006 ),
 .UNSPECIFIED., .F., .F.,
 ( 4, 2, 4 ),
 ( 0.0002800015744458473265, 0.0006862068192651732488, 0.001092412064084499279 ),
 .UNSPECIFIED. ) ;
#48142 = CARTESIAN_POINT ( 'NONE',  ( -3.500000000000000444, -0.04521315095527938394, 3.750000000000000444 ) ) ;
#48143 = DIRECTION ( 'NONE',  ( 0.000000000000000000, 0.000000000000000000, -1.000000000000000000 ) ) ;
#48144 = DIRECTION ( 'NONE',  ( 0.000000000000000000, 0.000000000000000000, 1.000000000000000000 ) ) ;
#48145 = CARTESIAN_POINT ( 'NONE',  ( 0.1532563361054082862, 56.21726448433411605, 2.638427012816831674 ) ) ;
#48146 = CARTESIAN_POINT ( 'NONE',  ( 17.08211943468705130, 53.47041550158063217, 12.26659068614894998 ) ) ;
#48147 = CARTESIAN_POINT ( 'NONE',  ( 18.72515096720570327, 6.072280503510315341, -6.499999999999985789 ) ) ;
#48148 = EDGE_LOOP ( 'NONE', ( #89563, #97092, #57813, #97777 ) ) ;
#48150 = AXIS2_PLACEMENT_3D ( 'NONE', #13101, #29567, #6590 ) ;
#48149 = CARTESIAN_POINT ( 'NONE',  ( -7.750000000000000000, 79.82179676972448590, -6.500000000000000888 ) ) ;
#48151 = CARTESIAN_POINT ( 'NONE',  ( 14.92337183194729633, 17.67559781766745175, 8.527530157486181039 ) ) ;
#48152 = CARTESIAN_POINT ( 'NONE',  ( 16.40814093676323893, 60.79030133659709634, 11.09922568453595026 ) ) ;
#48153 = CARTESIAN_POINT ( 'NONE',  ( 10.00000000000000000, -2.126365330069579951, -12.81628187352647608 ) ) ;
#48154 = CARTESIAN_POINT ( 'NONE',  ( 0.5774900079438590739, 62.64701867748817676, -5.440088680355550821 ) ) ;
#48155 = CARTESIAN_POINT ( 'NONE',  ( 0.1532563361054083140, 51.00893115100078745, 1.131784320476157264E-15 ) ) ;
#48156 = CARTESIAN_POINT ( 'NONE',  ( 0.000000000000000000, 14.49999999999999822, 0.000000000000000000 ) ) ;
#48157 = ORIENTED_EDGE ( 'NONE', *, *, #68322, .F. ) ;
#48158 = CARTESIAN_POINT ( 'NONE',  ( 24.16423886937409904, 59.09541550158063217, 3.795296366450317205 ) ) ;
#48159 = CARTESIAN_POINT ( 'NONE',  ( 3.927832320392154575, 0.000000000000000000, 13.69797916712106733 ) ) ;
#48160 = CARTESIAN_POINT ( 'NONE',  ( 2.035157376598824452, 48.68868534415483396, 7.964842623401179544 ) ) ;
#48162 = CARTESIAN_POINT ( 'NONE',  ( -0.8801773607111008646, 68.27201867748817676, 2.915334737309923430 ) ) ;
#48161 = CARTESIAN_POINT ( 'NONE',  ( 0.6178305044545818747, 18.49863466993041428, -9.382169495545419124 ) ) ;
#48163 = CARTESIAN_POINT ( 'NONE',  ( 13.86186289918443215, 15.00000000000000888, -4.667665767314964853 ) ) ;
#48164 = LINE ( 'NONE', #64999, #17270 ) ;
#48165 = CARTESIAN_POINT ( 'NONE',  ( -14.48718990079891888, 15.00000000000000000, -0.6093675230842395818 ) ) ;
#48166 = DIRECTION ( 'NONE',  ( 0.9961946980917462113, -0.08715574274765140739, 0.000000000000000000 ) ) ;
#48167 = CARTESIAN_POINT ( 'NONE',  ( 14.92337183194729633, 52.67559781766745175, 8.527530157486181039 ) ) ;
#48168 = CARTESIAN_POINT ( 'NONE',  ( 1.472469842513823179, 6.425597817667451750, 4.923371831947296329 ) ) ;
#48169 = CARTESIAN_POINT ( 'NONE',  ( -5.440088680355558814, -37.76964798917849464, -9.422509992056136596 ) ) ;
#48170 = CARTESIAN_POINT ( 'NONE',  ( 3.591859063236761518, 9.956968003263753531, 11.09922568453594849 ) ) ;
#48171 = CARTESIAN_POINT ( 'NONE',  ( 17.96484262340118221, 16.18868534415483396, -7.964842623401177768 ) ) ;
#48172 = PLANE ( 'NONE',  #72358 ) ;
#48173 = EDGE_CURVE ( 'NONE', #82904, #44178, #6106, .T. ) ;
#48174 = CARTESIAN_POINT ( 'NONE',  ( 13.79529636645031943, 35.34541550158063927, -14.16423886937409904 ) ) ;
#48175 = CARTESIAN_POINT ( 'NONE',  ( 6.204703633549690345, 35.76208216824729647, -14.16423886937410259 ) ) ;
#48176 = CARTESIAN_POINT ( 'NONE',  ( -2.266590686148945544, 62.22041550158063927, 7.082119434687048631 ) ) ;
#48177 = CARTESIAN_POINT ( 'NONE',  ( 17.20831665107776587, 32.88393115100078745, 7.208316651077764980 ) ) ;
#48178 = CARTESIAN_POINT ( 'NONE',  ( 22.81628187352647785, 41.41530133659708923, 3.434112377981063169 ) ) ;
#48179 = CARTESIAN_POINT ( 'NONE',  ( -0.8801773607110991993, 7.855352010821504471, -2.915334737309923874 ) ) ;
#48180 = CIRCLE ( 'NONE', #91370, 14.49999999999999822 ) ;
#48181 = VERTEX_POINT ( 'NONE', #81592 ) ;
#48182 = CARTESIAN_POINT ( 'NONE',  ( 10.00000000000000178, 37.25893115100078745, 9.846743663894594434 ) ) ;
#48183 = CARTESIAN_POINT ( 'NONE',  ( 19.42250999205614193, 45.14701867748817676, 5.440088680355555262 ) ) ;
#48184 = CARTESIAN_POINT ( 'NONE',  ( 5.076628168052704559, 65.17559781766745175, -8.527530157486179263 ) ) ;
#48185 = CARTESIAN_POINT ( 'NONE',  ( -4.164238869374099927, 17.01208216824730357, 3.795296366450308767 ) ) ;
#48186 = DIRECTION ( 'NONE',  ( 0.7808688094430307203, -0.6246950475544238435, 0.000000000000000000 ) ) ;
#48187 = UNCERTAINTY_MEASURE_WITH_UNIT (LENGTH_MEASURE( 1.000000000000000082E-05 ), #24067, 'distance_accuracy_value', 'NONE');
#48188 =( BOUNDED_CURVE ( )  B_SPLINE_CURVE ( 2, ( #38165, #97203, #28672, #31620, #91646, #30629, #54611, #39145, #32103 ),
 .UNSPECIFIED., .F., .F. ) 
 B_SPLINE_CURVE_WITH_KNOTS ( ( 3, 2, 2, 2, 3 ),
 ( 0.9044266512259456769, 0.9047619047619047672, 0.9107142857142856984, 0.9166666666666667407, 0.9170019202026259419 ),
 .UNSPECIFIED. ) 
 CURVE ( )  GEOMETRIC_REPRESENTATION_ITEM ( )  RATIONAL_B_SPLINE_CURVE ( ( 0.9963778908391764944, 0.9980808541467923733, 1.000000000000000000, 0.9659258262890682012, 1.000000000000000000, 0.9659258262890682012, 1.000000000000000000, 0.9980808541467917072, 0.9963778908391753841 ) ) 
 REPRESENTATION_ITEM ( '' )  );
#48189 = CARTESIAN_POINT ( 'NONE',  ( 18.52753015748618282, 28.92559781766745175, -4.923371831947291888 ) ) ;
#48190 = CARTESIAN_POINT ( 'NONE',  ( 6.565887622018943937, 48.08196800326375353, -12.81628187352647608 ) ) ;
#48191 = CARTESIAN_POINT ( 'NONE',  ( 14.92337183194729633, 52.67559781766745175, 8.527530157486181039 ) ) ;
#48192 = VERTEX_POINT ( 'NONE', #51607 ) ;
#48193 = DIRECTION ( 'NONE',  ( 0.000000000000000000, 0.000000000000000000, -1.000000000000000000 ) ) ;
#48194 = CARTESIAN_POINT ( 'NONE',  ( -46.49699363514445594, 103.0259809974584044, -6.596269562656988938 ) ) ;
#48195 = CARTESIAN_POINT ( 'NONE',  ( -4.164238869374099927, 62.01208216824728936, 3.795296366450308767 ) ) ;
#48196 = CARTESIAN_POINT ( 'NONE',  ( 2.917880565312948704, 12.63708216824730179, 12.26659068614894643 ) ) ;
#48197 = CARTESIAN_POINT ( 'NONE',  ( 19.84674366389459266, 3.300597817667451750, 2.638427012816836559 ) ) ;
#48198 = CARTESIAN_POINT ( 'NONE',  ( 17.20831665107776587, 44.13393115100078745, -7.208316651077762316 ) ) ;
#48199 = CARTESIAN_POINT ( 'NONE',  ( 20.88017736071110519, 25.56368534415483751, 2.639326808657452039E-16 ) ) ;
#48200 = CARTESIAN_POINT ( 'NONE',  ( 17.85999999999999943, 37.99999999999997868, -10.00000000000000000 ) ) ;
#48201 = CARTESIAN_POINT ( 'NONE',  ( 19.84674366389459621, 58.50893115100078745, 7.409399052514197653E-17 ) ) ;
#48202 = VERTEX_POINT ( 'NONE', #13103 ) ;
#48203 = AXIS2_PLACEMENT_3D ( 'NONE', #43918, #73433, #65935 ) ;
#48204 = FACE_OUTER_BOUND ( 'NONE', #4537, .T. ) ;
#48206 = ORIENTED_EDGE ( 'NONE', *, *, #23390, .F. ) ;
#48205 = ADVANCED_FACE ( 'NONE', ( #37597 ), #60074, .F. ) ;
#48207 = AXIS2_PLACEMENT_3D ( 'NONE', #41852, #10853, #19334 ) ;
#48208 = ORIENTED_EDGE ( 'NONE', *, *, #33440, .F. ) ;
#48209 = DIRECTION ( 'NONE',  ( 0.000000000000000000, 0.000000000000000000, 1.000000000000000000 ) ) ;
#48210 = CARTESIAN_POINT ( 'NONE',  ( -5.378451019861586246, 0.000000000000000000, -0.9000440264803170054 ) ) ;
#48211 = CARTESIAN_POINT ( 'NONE',  ( 10.00000000000000000, 0.5537488349139675359, -14.16423886937410082 ) ) ;
#48212 = CARTESIAN_POINT ( 'NONE',  ( 19.84674366389459266, 58.71726448433411605, -2.638427012816827677 ) ) ;
#48213 = CARTESIAN_POINT ( 'NONE',  ( 18.52753015748617571, 18.09226448433411960, 4.923371831947298993 ) ) ;
#48214 = CARTESIAN_POINT ( 'NONE',  ( 0.000000000000000000, 15.00000000000000000, -11.25000000000000178 ) ) ;
#48216 = CARTESIAN_POINT ( 'NONE',  ( 18.52753015748618282, 63.92559781766745886, -4.923371831947291888 ) ) ;
#48215 = CARTESIAN_POINT ( 'NONE',  ( 4.559911319644449179, 23.89701867748817321, 9.422509992056141925 ) ) ;
#48217 = CARTESIAN_POINT ( 'NONE',  ( 11.35178980618974087, 0.5000000000000004441, -9.804941009311923139 ) ) ;
#48218 = ADVANCED_FACE ( 'NONE', ( #82091 ), #9977, .T. ) ;
#48219 = CARTESIAN_POINT ( 'NONE',  ( 2.035157376598822676, 2.438685344154838397, -7.964842623401177768 ) ) ;
#48220 = FACE_OUTER_BOUND ( 'NONE', #3346, .T. ) ;
#48221 = AXIS2_PLACEMENT_3D ( 'NONE', #15903, #29898, #7913 ) ;
#48222 = CARTESIAN_POINT ( 'NONE',  ( 17.78441314508140891, 78.67289652296261693, 4.000000000000000000 ) ) ;
#48223 = CARTESIAN_POINT ( 'NONE',  ( 7.084665262690076126, 69.10535201082151957, 10.88017736071109987 ) ) ;
#48224 = AXIS2_PLACEMENT_3D ( 'NONE', #2143, #79593, #3605 ) ;
#48225 = CARTESIAN_POINT ( 'NONE',  ( 2.791683348922237240, 15.38393115100078212, -7.208316651077763204 ) ) ;
#48226 = FACE_OUTER_BOUND ( 'NONE', #78382, .T. ) ;
#48227 = ORIENTED_EDGE ( 'NONE', *, *, #32000, .T. ) ;
#48228 = LINE ( 'NONE', #40250, #74614 ) ;
#48229 = VECTOR ( 'NONE', #63035, 1000.000000000000000 ) ;
#48230 = VERTEX_POINT ( 'NONE', #83084 ) ;
#48231 = CARTESIAN_POINT ( 'NONE',  ( 5.076628168052704559, 25.17559781766745175, -8.527530157486179263 ) ) ;
#48232 = ORIENTED_EDGE ( 'NONE', *, *, #58957, .T. ) ;
#48233 = CARTESIAN_POINT ( 'NONE',  ( 13.79529636645030344, 28.26208216824729647, 14.16423886937410614 ) ) ;
#48234 = CARTESIAN_POINT ( 'NONE',  ( 19.84674366389459621, 33.50893115100078745, 7.409399052514197653E-17 ) ) ;
#48235 = CARTESIAN_POINT ( 'NONE',  ( 17.96484262340118221, 41.18868534415484106, -7.964842623401177768 ) ) ;
#48236 = DIRECTION ( 'NONE',  ( 0.4924235601034648302, -0.000000000000000000, 0.8703556959399010307 ) ) ;
#48237 = VERTEX_POINT ( 'NONE', #5620 ) ;
#48238 = CARTESIAN_POINT ( 'NONE',  ( 19.42250999205614193, 45.14701867748817676, 5.440088680355555262 ) ) ;
#48239 = B_SPLINE_CURVE_WITH_KNOTS ( 'NONE', 3,
 ( #83292, #53279, #38296, #61270, #23795, #83785 ),
 .UNSPECIFIED., .F., .F.,
 ( 4, 2, 4 ),
 ( 3.409110551485654587E-05, 0.0004400426677367037386, 0.0008459942299585509855 ),
 .UNSPECIFIED. ) ;
#48240 = CARTESIAN_POINT ( 'NONE',  ( -9.382169495545422677, -1.501365330069578619, -9.382169495545417348 ) ) ;
#48241 = ORIENTED_EDGE ( 'NONE', *, *, #33355, .T. ) ;
#48242 = CARTESIAN_POINT ( 'NONE',  ( 2.917880565312948704, 12.63708216824730179, 12.26659068614894643 ) ) ;
#48243 = VERTEX_POINT ( 'NONE', #90575 ) ;
#48244 = EDGE_CURVE ( 'NONE', #75354, #14763, #65484, .T. ) ;
#48245 = ORIENTED_EDGE ( 'NONE', *, *, #81318, .F. ) ;
#48246 = CARTESIAN_POINT ( 'NONE',  ( 22.81628187352647785, 36.62363466993041783, 6.195893100308588602E-16 ) ) ;
#48247 = CARTESIAN_POINT ( 'NONE',  ( 10.00000000000000000, 29.75893115100078745, -9.846743663894594434 ) ) ;
#48248 = CARTESIAN_POINT ( 'NONE',  ( 14.88232117145534339, 0.3639310251205937208, -1.875237731503157645 ) ) ;
#48249 = CARTESIAN_POINT ( 'NONE',  ( 3.591859063236761518, 44.95696800326376064, 11.09922568453594849 ) ) ;
#48250 = CARTESIAN_POINT ( 'NONE',  ( 0.1532563361054082862, 26.21726448433411605, 2.638427012816831674 ) ) ;
#48251 = CARTESIAN_POINT ( 'NONE',  ( 17.96484262340118221, 54.93868534415484106, 7.964842623401181321 ) ) ;
#48252 = AXIS2_PLACEMENT_3D ( 'NONE', #11362, #64835, #93878 ) ;
#48253 = CARTESIAN_POINT ( 'NONE',  ( 0.5774900079438590739, 67.64701867748817676, -5.440088680355550821 ) ) ;
#48254 = DIRECTION ( 'NONE',  ( -0.000000000000000000, -1.000000000000000000, -0.000000000000000000 ) ) ;
#48255 = CARTESIAN_POINT ( 'NONE',  ( 10.00000000000000178, 65.37363466993042493, 12.81628187352647608 ) ) ;
#48256 = CARTESIAN_POINT ( 'NONE',  ( 7.361572987183169658, 9.967264484334119601, -9.846743663894592657 ) ) ;
#48257 = CARTESIAN_POINT ( 'NONE',  ( -1.099225684535947600, 9.540301336597087456, 6.408140936763237150 ) ) ;
#48258 = CARTESIAN_POINT ( 'NONE',  ( -0.1503990784575328643, 0.1277717457861260453, 6.262539305110068177 ) ) ;
#48259 = CARTESIAN_POINT ( 'NONE',  ( 19.84674366389459266, 38.30059781766745175, 2.638427012816836559 ) ) ;
#48260 = CARTESIAN_POINT ( 'NONE',  ( -2.816281873526473856, 64.33196800326376774, 3.434112377981055619 ) ) ;
#48261 = CARTESIAN_POINT ( 'NONE',  ( 20.36894250292379738, 9.928748834913966093, -10.36894250292379027 ) ) ;
#48262 = CARTESIAN_POINT ( 'NONE',  ( 19.84674366389459266, 18.71726448433411960, -2.638427012816827677 ) ) ;
#48263 = CARTESIAN_POINT ( 'NONE',  ( 0.6178305044545818747, 38.49863466993042493, -9.382169495545419124 ) ) ;
#48265 = CARTESIAN_POINT ( 'NONE',  ( 0.8952175423694934686, 22.60160829253886305, -5.990408912944337416 ) ) ;
#48264 = SURFACE_STYLE_USAGE ( .BOTH. , #86774 ) ;
#48266 = CARTESIAN_POINT ( 'NONE',  ( 4.559911319644449179, 47.23035201082150536, -9.422509992056141925 ) ) ;
#48267 = CARTESIAN_POINT ( 'NONE',  ( 22.81628187352647785, 11.62363466993042138, 6.195893100308588602E-16 ) ) ;
#48268 = CARTESIAN_POINT ( 'NONE',  ( -0.2418659066527499291, 32.23410085661203084, -6.114288769123083611 ) ) ;
#48269 = CARTESIAN_POINT ( 'NONE',  ( 7.361572987183169658, 24.96726448433412315, -9.846743663894592657 ) ) ;
#48270 = CARTESIAN_POINT ( 'NONE',  ( 20.88017736071110519, 30.56368534415484106, 2.639326808657452039E-16 ) ) ;
#48271 = CARTESIAN_POINT ( 'NONE',  ( 10.00000000000000000, 32.87363466993042493, -12.81628187352647608 ) ) ;
#48272 = CIRCLE ( 'NONE', #5180, 15.00000000000000000 ) ;
#48273 = CARTESIAN_POINT ( 'NONE',  ( 7.361572987183170547, 22.05059781766745530, 9.846743663894590881 ) ) ;
#48274 = SURFACE_SIDE_STYLE ('',( #70312 ) ) ;
#48275 = CARTESIAN_POINT ( 'NONE',  ( -8.352412229647901754, 86.23350694210130030, 4.048761466749791538 ) ) ;
#48276 = CARTESIAN_POINT ( 'NONE',  ( 0.5774900079438590739, 22.64701867748817321, -5.440088680355550821 ) ) ;
#48277 = ORIENTED_EDGE ( 'NONE', *, *, #97473, .F. ) ;
#48278 = VECTOR ( 'NONE', #9273, 1000.000000000000000 ) ;
#48279 = CARTESIAN_POINT ( 'NONE',  ( 7.084665262690076126, 67.02201867748817676, -10.88017736071110164 ) ) ;
#48280 = CARTESIAN_POINT ( 'NONE',  ( -0.8801773607111009756, 8.063685344154837509, 1.068504757029289695E-15 ) ) ;
#48282 = CARTESIAN_POINT ( 'NONE',  ( 7.084665262690076126, 12.02201867748817321, -10.88017736071110164 ) ) ;
#48281 = CARTESIAN_POINT ( 'NONE',  ( 1.472469842513823179, 45.59226448433412315, -4.923371831947296329 ) ) ;
#48284 = B_SPLINE_CURVE_WITH_KNOTS ( 'NONE', 3,
 ( #77549, #63047, #93543, #62543, #25564, #48036 ),
 .UNSPECIFIED., .F., .F.,
 ( 4, 2, 4 ),
 ( 3.409110551496215394E-05, 0.0004400426677368006120, 0.0008459942299586391311 ),
 .UNSPECIFIED. ) ;
#48283 = CARTESIAN_POINT ( 'NONE',  ( -5.817157072110894944, 14.49999999999999112, 13.82608706751089755 ) ) ;
#48285 = CARTESIAN_POINT ( 'NONE',  ( 4.559911319644449179, 43.89701867748816966, 9.422509992056141925 ) ) ;
#48287 = CARTESIAN_POINT ( 'NONE',  ( -0.2418659066527782397, 20.11633188102327452, 6.114288769123032985 ) ) ;
#48286 = CARTESIAN_POINT ( 'NONE',  ( 12.91533473730992121, 19.52201867748816611, 10.88017736071110164 ) ) ;
#48288 = TOROIDAL_SURFACE ( 'NONE', #6773, 14.49999999999999822, 0.5000000000000000000 ) ;
#48289 = CARTESIAN_POINT ( 'NONE',  ( 7.361572987183170547, 32.05059781766745175, 9.846743663894590881 ) ) ;
#48290 = CARTESIAN_POINT ( 'NONE',  ( -5.810202895580280469, 0.04922511925147063372, -13.56051778013773479 ) ) ;
#48291 = CYLINDRICAL_SURFACE ( 'NONE', #6578, 15.00000000000000000 ) ;
#48292 = ADVANCED_FACE ( 'NONE', ( #8082 ), #81748, .T. ) ;
#48293 = FILL_AREA_STYLE ('',( #47303 ) ) ;
#48295 = AXIS2_PLACEMENT_3D ( 'NONE', #92435, #16453, #10307 ) ;
#48294 = CARTESIAN_POINT ( 'NONE',  ( 6.204703633549690345, 25.76208216824730712, -14.16423886937410259 ) ) ;
#48296 = CARTESIAN_POINT ( 'NONE',  ( 34.56412365047464874, 11.49999999999999645, -10.00000000000000000 ) ) ;
#48297 = ORIENTED_EDGE ( 'NONE', *, *, #38242, .T. ) ;
#48298 = CARTESIAN_POINT ( 'NONE',  ( 6.204703633549690345, 65.76208216824731778, -14.16423886937410259 ) ) ;
#48299 = CARTESIAN_POINT ( 'NONE',  ( 17.20831665107776587, 27.88393115100078390, 7.208316651077764980 ) ) ;
#48301 = CARTESIAN_POINT ( 'NONE',  ( -8.819573739049973327, 87.31373983715974418, -4.675023147224794506 ) ) ;
#48300 = CARTESIAN_POINT ( 'NONE',  ( -18.00000000000000355, 80.99999999999994316, -3.000000000000000000 ) ) ;
#48302 = CARTESIAN_POINT ( 'NONE',  ( 17.96484262340118221, 49.93868534415484106, 7.964842623401181321 ) ) ;
#48303 = CARTESIAN_POINT ( 'NONE',  ( 13.43411237798105340, 60.58196800326376064, 12.81628187352647963 ) ) ;
#48304 = CARTESIAN_POINT ( 'NONE',  ( 15.44008868035555260, 29.73035201082150891, 9.422509992056143702 ) ) ;
#48305 = PLANE ( 'NONE',  #46659 ) ;
#48306 = CARTESIAN_POINT ( 'NONE',  ( 6.565887622018943937, 15.16530133659708568, 12.81628187352647430 ) ) ;
#48307 = CARTESIAN_POINT ( 'NONE',  ( 12.63842701281683922, 14.55059781766744997, -9.846743663894590881 ) ) ;
#48308 = EDGE_LOOP ( 'NONE', ( #1089, #25066, #36079, #77436 ) ) ;
#48309 = CARTESIAN_POINT ( 'NONE',  ( 0.2751277870542909731, 44.36607318730131055, -6.499999999999992006 ) ) ;
#48310 = CARTESIAN_POINT ( 'NONE',  ( 2.917880565312948704, 57.63708216824731068, 12.26659068614894643 ) ) ;
#48311 = AXIS2_PLACEMENT_3D ( 'NONE', #91930, #23457, #79387 ) ;
#48312 = CARTESIAN_POINT ( 'NONE',  ( 24.16423886937409904, 24.09541550158063927, 3.795296366450317205 ) ) ;
#48313 = CARTESIAN_POINT ( 'NONE',  ( 0.5774900079438607392, 18.48035201082150536, 5.440088680355550821 ) ) ;
#48314 = CARTESIAN_POINT ( 'NONE',  ( 17.96484262340118221, 56.18868534415484817, -7.964842623401177768 ) ) ;
#48315 =( LENGTH_UNIT ( ) NAMED_UNIT ( * ) SI_UNIT ( .MILLI., .METRE. ) );
#48316 = CARTESIAN_POINT ( 'NONE',  ( 8.742108547223832460, -4.148811688994628710, -4.000000000000000000 ) ) ;
#48317 = CARTESIAN_POINT ( 'NONE',  ( 18.52753015748618282, 8.925597817667451750, -4.923371831947291888 ) ) ;
#48318 = SURFACE_SIDE_STYLE ('',( #71335 ) ) ;
#48319 = CARTESIAN_POINT ( 'NONE',  ( 18.52753015748617571, 23.09226448433411960, 4.923371831947298993 ) ) ;
#48320 = CARTESIAN_POINT ( 'NONE',  ( -16.94999999999999574, 99.99999999999998579, 8.000000000000000000 ) ) ;
#48321 =( NAMED_UNIT ( * ) PLANE_ANGLE_UNIT ( ) SI_UNIT ( $, .RADIAN. ) );
#48322 = CARTESIAN_POINT ( 'NONE',  ( 0.1532563361054100626, 30.80059781766744820, -2.638427012816831230 ) ) ;
#48323 = CARTESIAN_POINT ( 'NONE',  ( 17.20831665107776587, 49.13393115100078745, -7.208316651077762316 ) ) ;
#48324 = CARTESIAN_POINT ( 'NONE',  ( 4.559911319644449179, 27.23035201082150536, -9.422509992056141925 ) ) ;
#48325 = UNCERTAINTY_MEASURE_WITH_UNIT (LENGTH_MEASURE( 1.000000000000000082E-05 ), #60221, 'distance_accuracy_value', 'NONE');
#48326 = AXIS2_PLACEMENT_3D ( 'NONE', #68439, #91420, #22947 ) ;
#48327 = EDGE_CURVE ( 'NONE', #74552, #46284, #2307, .T. ) ;
#48328 = CARTESIAN_POINT ( 'NONE',  ( 21.09922568453595559, 37.04030133659708923, -6.408140936763230044 ) ) ;
#48329 = CARTESIAN_POINT ( 'NONE',  ( 2.035157376598822676, 57.43868534415484106, -7.964842623401177768 ) ) ;
#48330 = CARTESIAN_POINT ( 'NONE',  ( 19.84674366389459621, 23.50893115100078390, 7.409399052514197653E-17 ) ) ;
#48332 = CARTESIAN_POINT ( 'NONE',  ( 0.1532563361054100626, 15.80059781766745353, -2.638427012816831230 ) ) ;
#48331 = CARTESIAN_POINT ( 'NONE',  ( 17.08211943468705840, 40.13708216824731068, -12.26659068614894466 ) ) ;
#48333 = DIRECTION ( 'NONE',  ( 0.06975647374412534407, 0.9975640502598241977, 0.000000000000000000 ) ) ;
#48334 = CARTESIAN_POINT ( 'NONE',  ( 1.472469842513823179, 56.42559781766745886, 4.923371831947296329 ) ) ;
#48336 = CARTESIAN_POINT ( 'NONE',  ( -2.266590686148945544, 7.220415501580634832, 7.082119434687048631 ) ) ;
#48335 = CARTESIAN_POINT ( 'NONE',  ( 7.361572987183170547, 32.05059781766745175, 9.846743663894590881 ) ) ;
#48337 = EDGE_CURVE ( 'NONE', #18880, #70662, #38666, .T. ) ;
#48338 = CARTESIAN_POINT ( 'NONE',  ( 6.204703633549690345, 15.76208216824730179, -14.16423886937410259 ) ) ;
#48339 = CARTESIAN_POINT ( 'NONE',  ( 17.20831665107776587, 24.13393115100078035, -7.208316651077762316 ) ) ;
#48340 = CARTESIAN_POINT ( 'NONE',  ( 2.035157376598822676, 47.43868534415484817, -7.964842623401177768 ) ) ;
#48341 = CARTESIAN_POINT ( 'NONE',  ( 2.035157376598824452, 28.68868534415484106, 7.964842623401179544 ) ) ;
#48342 = CARTESIAN_POINT ( 'NONE',  ( 2.035157376598824452, 43.68868534415484106, 7.964842623401179544 ) ) ;
#48343 = CARTESIAN_POINT ( 'NONE',  ( 4.559911319644449179, 33.89701867748817676, 9.422509992056141925 ) ) ;
#48344 = EDGE_LOOP ( 'NONE', ( #76052, #86991 ) ) ;
#48345 = CARTESIAN_POINT ( 'NONE',  ( 4.559911319644449179, 58.89701867748817676, 9.422509992056141925 ) ) ;
#48346 = EDGE_LOOP ( 'NONE', ( #85071, #37453, #89208, #31374, #55478, #6995 ) ) ;
#48347 = CARTESIAN_POINT ( 'NONE',  ( 4.559911319644449179, 62.23035201082150536, -9.422509992056141925 ) ) ;
#48348 = TOROIDAL_SURFACE ( 'NONE', #30710, 14.49999999999999822, 0.5000000000000000000 ) ;
#48349 = VERTEX_POINT ( 'NONE', #91577 ) ;
#48350 = CARTESIAN_POINT ( 'NONE',  ( 12.91533473730993009, 66.60535201082150536, -10.88017736071109987 ) ) ;
#48351 = CARTESIAN_POINT ( 'NONE',  ( 2.603489959281601873, 25.43575266056827289, -6.500000000000015987 ) ) ;
#48352 = CARTESIAN_POINT ( 'NONE',  ( 19.72487221294570858, 70.00000000000000000, 6.500000000000000888 ) ) ;
#48353 = CARTESIAN_POINT ( 'NONE',  ( 24.16423886937410614, 64.30374883491396076, 8.672049930838204340E-16 ) ) ;
#48354 = CARTESIAN_POINT ( 'NONE',  ( 19.84674366389459621, 13.50893115100078568, 7.409399052514197653E-17 ) ) ;
#48355 = CARTESIAN_POINT ( 'NONE',  ( -4.164238869374099039, 1.803748834913967647, 8.674139862899312516E-16 ) ) ;
#48356 = CARTESIAN_POINT ( 'NONE',  ( 7.361572987183169658, 4.967264484334119601, -9.846743663894592657 ) ) ;
#48357 =( GEOMETRIC_REPRESENTATION_CONTEXT ( 3 ) GLOBAL_UNCERTAINTY_ASSIGNED_CONTEXT ( ( #70359 ) ) GLOBAL_UNIT_ASSIGNED_CONTEXT ( ( #48522, #41046, #33508 ) ) REPRESENTATION_CONTEXT ( 'NONE', 'WORKASPACE' ) );
#48358 = CARTESIAN_POINT ( 'NONE',  ( 12.63842701281683034, 42.46726448433412315, 9.846743663894596210 ) ) ;
#48359 = ORIENTED_EDGE ( 'NONE', *, *, #311, .T. ) ;
#48360 = VECTOR ( 'NONE', #35874, 1000.000000000000000 ) ;
#48361 = CARTESIAN_POINT ( 'NONE',  ( 10.00000000000000178, 47.25893115100078745, 9.846743663894594434 ) ) ;
#48362 = ORIENTED_EDGE ( 'NONE', *, *, #96197, .T. ) ;
#48363 = CYLINDRICAL_SURFACE ( 'NONE', #44595, 0.2500000000000002220 ) ;
#48364 = CIRCLE ( 'NONE', #54714, 14.49999999999999822 ) ;
#48365 = CARTESIAN_POINT ( 'NONE',  ( 20.88017736071110875, 55.77201867748816966, -2.915334737309920765 ) ) ;
#48366 = CARTESIAN_POINT ( 'NONE',  ( 14.92337183194729988, 49.34226448433411605, -8.527530157486177487 ) ) ;
#48368 = CARTESIAN_POINT ( 'NONE',  ( 6.382347221874338672, 14.63595249122789177, 13.57444820018232434 ) ) ;
#48367 = CARTESIAN_POINT ( 'NONE',  ( -8.000000000000000000, 80.99999999999994316, 0.000000000000000000 ) ) ;
#48369 = CARTESIAN_POINT ( 'NONE',  ( 20.88017736071110519, 60.56368534415484106, 2.639326808657452039E-16 ) ) ;
#48370 = CARTESIAN_POINT ( 'NONE',  ( 2.917880565312950480, 65.97041550158063217, -12.26659068614894821 ) ) ;
#48371 = EDGE_CURVE ( 'NONE', #61558, #76088, #94649, .T. ) ;
#48372 = CARTESIAN_POINT ( 'NONE',  ( 21.09922568453595559, 37.04030133659708923, -6.408140936763230044 ) ) ;
#48373 = DIRECTION ( 'NONE',  ( -0.000000000000000000, -1.000000000000000000, -0.000000000000000000 ) ) ;
#48374 = VERTEX_POINT ( 'NONE', #54542 ) ;
#48375 = CARTESIAN_POINT ( 'NONE',  ( 13.43411237798105340, 30.58196800326374998, 12.81628187352647963 ) ) ;
#48376 = CARTESIAN_POINT ( 'NONE',  ( 12.91533473730992121, 29.52201867748817321, 10.88017736071110164 ) ) ;
#48377 = ORIENTED_EDGE ( 'NONE', *, *, #78386, .F. ) ;
#48378 = VECTOR ( 'NONE', #51312, 1000.000000000000000 ) ;
#48379 = CARTESIAN_POINT ( 'NONE',  ( 5.076628168052704559, 10.17559781766745175, -8.527530157486179263 ) ) ;
#48380 =( BOUNDED_CURVE ( )  B_SPLINE_CURVE ( 3, ( #86094, #17605, #39122, #10100 ),
 .UNSPECIFIED., .F., .T. ) 
 B_SPLINE_CURVE_WITH_KNOTS ( ( 4, 4 ),
 ( 4.712388980384695891, 6.283185307179586232 ),
 .UNSPECIFIED. ) 
 CURVE ( )  GEOMETRIC_REPRESENTATION_ITEM ( )  RATIONAL_B_SPLINE_CURVE ( ( 1.000000000000000000, 0.8047378541243663808, 0.8047378541243663808, 1.000000000000000000 ) ) 
 REPRESENTATION_ITEM ( '' )  );
#48381 = CARTESIAN_POINT ( 'NONE',  ( 12.63842701281683922, 64.55059781766745175, -9.846743663894590881 ) ) ;
#48383 = CARTESIAN_POINT ( 'NONE',  ( 17.20831665107776587, 44.13393115100078745, -7.208316651077762316 ) ) ;
#48382 = CARTESIAN_POINT ( 'NONE',  ( 7.361572987183170547, 7.050597817667451750, 9.846743663894590881 ) ) ;
#48384 = CARTESIAN_POINT ( 'NONE',  ( -9.208448955093622601, -19.73347625016914719, 3.750000000000001332 ) ) ;
#48385 = CARTESIAN_POINT ( 'NONE',  ( 3.591859063236761518, 64.95696800326376774, 11.09922568453594849 ) ) ;
#48386 = CARTESIAN_POINT ( 'NONE',  ( 0.1532563361054100626, 40.80059781766745886, -2.638427012816831230 ) ) ;
#48387 = CARTESIAN_POINT ( 'NONE',  ( 6.579634127946647482, -87.99828267815715321, 2.750000000000000000 ) ) ;
#48388 = CARTESIAN_POINT ( 'NONE',  ( -7.750000000000000000, 79.82179676972448590, -6.500000000000000888 ) ) ;
#48389 = CIRCLE ( 'NONE', #96309, 2.899999999999999911 ) ;
#48391 = LINE ( 'NONE', #17426, #70667 ) ;
#48390 = CARTESIAN_POINT ( 'NONE',  ( 7.361572987183169658, 29.96726448433411960, -9.846743663894592657 ) ) ;
#48392 = FILL_AREA_STYLE ('',( #33374 ) ) ;
#48394 = ORIENTED_EDGE ( 'NONE', *, *, #26632, .F. ) ;
#48393 = CARTESIAN_POINT ( 'NONE',  ( 19.84674366389459266, 53.71726448433411605, -2.638427012816827677 ) ) ;
#48395 = AXIS2_PLACEMENT_3D ( 'NONE', #16300, #92774, #60311 ) ;
#48396 = CARTESIAN_POINT ( 'NONE',  ( 6.565887622018943937, 25.16530133659708213, 12.81628187352647430 ) ) ;
#48397 = CARTESIAN_POINT ( 'NONE',  ( 7.361572987183169658, 49.96726448433410894, -9.846743663894592657 ) ) ;
#48398 = LINE ( 'NONE', #94389, #91956 ) ;
#48399 = CARTESIAN_POINT ( 'NONE',  ( 24.16423886937409904, 49.09541550158063217, 3.795296366450317205 ) ) ;
#48400 = CARTESIAN_POINT ( 'NONE',  ( 19.84674366389459266, 13.30059781766745353, 2.638427012816836559 ) ) ;
#48401 = ORIENTED_EDGE ( 'NONE', *, *, #59426, .T. ) ;
#48402 = SURFACE_SIDE_STYLE ('',( #46439 ) ) ;
#48403 = CARTESIAN_POINT ( 'NONE',  ( 0.000000000000000000, 0.5000000000000004441, 0.000000000000000000 ) ) ;
#48404 = CARTESIAN_POINT ( 'NONE',  ( -4.164238869374099927, 47.01208216824729647, 3.795296366450308767 ) ) ;
#48405 = CARTESIAN_POINT ( 'NONE',  ( 0.1532563361054100626, 60.80059781766744464, -2.638427012816831230 ) ) ;
#48406 = CARTESIAN_POINT ( 'NONE',  ( -0.8801773607111008646, 3.272018677488171434, 2.915334737309923430 ) ) ;
#48407 = CARTESIAN_POINT ( 'NONE',  ( 6.204703633549690345, 25.76208216824730712, -14.16423886937410259 ) ) ;
#48408 = CARTESIAN_POINT ( 'NONE',  ( 10.00000000000000178, 43.05374883491397497, 14.16423886937410082 ) ) ;
#48409 = CARTESIAN_POINT ( 'NONE',  ( 14.49999999999999822, 11.50000000000000000, -6.000000000000000000 ) ) ;
#48411 = CARTESIAN_POINT ( 'NONE',  ( 1.472469842513823179, 56.42559781766745886, 4.923371831947296329 ) ) ;
#48410 = FACE_OUTER_BOUND ( 'NONE', #41090, .T. ) ;
#48412 = CARTESIAN_POINT ( 'NONE',  ( 4.559911319644449179, 38.89701867748817676, 9.422509992056141925 ) ) ;
#48413 = CARTESIAN_POINT ( 'NONE',  ( -7.750000000000000000, 79.82179676972448590, 4.000000000000000000 ) ) ;
#48414 = CARTESIAN_POINT ( 'NONE',  ( 9.512310014786894641, -15.51178930340558360, 3.750000000000001332 ) ) ;
#48415 = EDGE_CURVE ( 'NONE', #28166, #56195, #21100, .T. ) ;
#48416 = CARTESIAN_POINT ( 'NONE',  ( 1.472469842513823179, 35.59226448433412315, -4.923371831947296329 ) ) ;
#48417 = CARTESIAN_POINT ( 'NONE',  ( 6.579634127946608402, -87.99828267815712479, -2.500000000000000000 ) ) ;
#48418 = CARTESIAN_POINT ( 'NONE',  ( 3.469446951953614189E-15, 13.05374883491396787, 14.16423886937410259 ) ) ;
#48419 = CARTESIAN_POINT ( 'NONE',  ( 2.791683348922240793, 61.63393115100079456, 7.208316651077764092 ) ) ;
#48420 = CARTESIAN_POINT ( 'NONE',  ( 0.1532563361054082862, 61.21726448433412315, 2.638427012816831674 ) ) ;
#48421 = EDGE_LOOP ( 'NONE', ( #29164, #65073, #57489, #72684 ) ) ;
#48422 = CARTESIAN_POINT ( 'NONE',  ( -4.164238869374099927, 32.01208216824730357, 3.795296366450308767 ) ) ;
#48423 = CARTESIAN_POINT ( 'NONE',  ( 13.99999999999999822, 60.50000000000000000, 6.000000000000000000 ) ) ;
#48425 = DIRECTION ( 'NONE',  ( -1.776356839400250465E-15, 0.000000000000000000, 1.000000000000000000 ) ) ;
#48424 = CARTESIAN_POINT ( 'NONE',  ( -5.809210876173503735, -36.07757871006351991, -2.499999999998389288 ) ) ;
#48427 = CIRCLE ( 'NONE', #26106, 15.00000000000000000 ) ;
#48426 = CARTESIAN_POINT ( 'NONE',  ( 19.42250999205614548, 10.98035201082150536, -5.440088680355545492 ) ) ;
#48428 = CARTESIAN_POINT ( 'NONE',  ( 19.38216949554541202, 30.99863466993042138, 9.382169495545424454 ) ) ;
#48429 = DIRECTION ( 'NONE',  ( 1.697280217195517047E-15, 1.285704996138754495E-15, -1.000000000000000000 ) ) ;
#48430 = CARTESIAN_POINT ( 'NONE',  ( 17.20831665107776587, 9.133931151000787452, -7.208316651077762316 ) ) ;
#48431 = PRESENTATION_LAYER_ASSIGNMENT (  '', '', ( #64335 ) ) ;
#48432 = CARTESIAN_POINT ( 'NONE',  ( 20.15039907845753220, 41.74884699246887720, 6.262539305110078836 ) ) ;
#48433 = DIRECTION ( 'NONE',  ( -1.000000000000000000, 0.000000000000000000, 0.000000000000000000 ) ) ;
#48434 = CARTESIAN_POINT ( 'NONE',  ( -13.77612262535527954, 90.93158326518027934, -7.883772450803742338 ) ) ;
#48435 = CARTESIAN_POINT ( 'NONE',  ( 20.88017736071110164, 15.35535201082150358, 2.915334737309930979 ) ) ;
#48436 = CYLINDRICAL_SURFACE ( 'NONE', #63910, 0.2500000000000002220 ) ;
#48437 = CARTESIAN_POINT ( 'NONE',  ( 4.559911319644449179, 42.23035201082151247, -9.422509992056141925 ) ) ;
#48439 = AXIS2_PLACEMENT_3D ( 'NONE', #30003, #67033, #91002 ) ;
#48438 = CARTESIAN_POINT ( 'NONE',  ( -0.8801773607110991993, 42.85535201082150536, -2.915334737309923874 ) ) ;
#48440 = CARTESIAN_POINT ( 'NONE',  ( 6.565887622018943937, -1.918031996736246692, -12.81628187352647608 ) ) ;
#48441 = LINE ( 'NONE', #56922, #13860 ) ;
#48442 = CARTESIAN_POINT ( 'NONE',  ( -45.11020673897264999, 105.3618001163576849, -4.929053739391441979 ) ) ;
#48443 = CARTESIAN_POINT ( 'NONE',  ( 12.63842701281683034, 7.467264484334118713, 9.846743663894596210 ) ) ;
#48444 = ORIENTED_EDGE ( 'NONE', *, *, #13039, .T. ) ;
#48445 = CARTESIAN_POINT ( 'NONE',  ( 19.42250999205614548, 35.98035201082151247, -5.440088680355545492 ) ) ;
#48446 = CARTESIAN_POINT ( 'NONE',  ( -1.099225684535947600, 34.54030133659708923, 6.408140936763237150 ) ) ;
#48447 = LINE ( 'NONE', #77460, #16175 ) ;
#48448 = UNCERTAINTY_MEASURE_WITH_UNIT (LENGTH_MEASURE( 1.000000000000000082E-05 ), #23599, 'distance_accuracy_value', 'NONE');
#48449 = EDGE_CURVE ( 'NONE', #6068, #58843, #29549, .T. ) ;
#48450 = CARTESIAN_POINT ( 'NONE',  ( 0.1532563361054082862, 61.21726448433412315, 2.638427012816831674 ) ) ;
#48451 = CARTESIAN_POINT ( 'NONE',  ( -0.8801773607111008646, 58.27201867748816966, 2.915334737309923430 ) ) ;
#48452 = CARTESIAN_POINT ( 'NONE',  ( 19.84674366389459621, 8.508931151000785675, 7.409399052514197653E-17 ) ) ;
#48453 = CARTESIAN_POINT ( 'NONE',  ( -1.099225684535947600, 29.54030133659708923, 6.408140936763237150 ) ) ;
#48455 = DIRECTION ( 'NONE',  ( -0.000000000000000000, -1.000000000000000000, -0.000000000000000000 ) ) ;
#48454 = CARTESIAN_POINT ( 'NONE',  ( 7.084665262690076126, 67.02201867748817676, -10.88017736071110164 ) ) ;
#48456 = ORIENTED_EDGE ( 'NONE', *, *, #27032, .F. ) ;
#48457 = DIRECTION ( 'NONE',  ( -0.9975640502598257520, 0.06975647374410356982, 0.000000000000000000 ) ) ;
#48458 = CARTESIAN_POINT ( 'NONE',  ( 20.88017736071110519, 5.563685344154837509, 2.639326808657452039E-16 ) ) ;
#48460 = CARTESIAN_POINT ( 'NONE',  ( -0.3689425029237898834, 26.17874883491396432, -10.36894250292378850 ) ) ;
#48459 = CARTESIAN_POINT ( 'NONE',  ( 0.6178305044545818747, 63.49863466993043204, -9.382169495545419124 ) ) ;
#48461 = CARTESIAN_POINT ( 'NONE',  ( 2.791683348922237240, 15.38393115100078212, -7.208316651077763204 ) ) ;
#48462 = CARTESIAN_POINT ( 'NONE',  ( 20.88017736071110875, 5.772018677488170546, -2.915334737309920765 ) ) ;
#48463 = CARTESIAN_POINT ( 'NONE',  ( 10.00000000000000178, 22.25893115100078745, 9.846743663894594434 ) ) ;
#48464 = CARTESIAN_POINT ( 'NONE',  ( -4.164238869374099927, 57.01208216824731068, 3.795296366450308767 ) ) ;
#48465 = ORIENTED_EDGE ( 'NONE', *, *, #57686, .T. ) ;
#48466 = CARTESIAN_POINT ( 'NONE',  ( -0.8801773607111009756, 13.06368534415483929, 1.068504757029289695E-15 ) ) ;
#48467 = AXIS2_PLACEMENT_3D ( 'NONE', #8230, #46226, #83730 ) ;
#48468 = CARTESIAN_POINT ( 'NONE',  ( 0.5774900079438590739, 27.64701867748817676, -5.440088680355550821 ) ) ;
#48469 = CARTESIAN_POINT ( 'NONE',  ( 2.153642693323440938, 31.13791097397318097, -6.500000000000005329 ) ) ;
#48470 = VERTEX_POINT ( 'NONE', #92546 ) ;
#48471 = VERTEX_POINT ( 'NONE', #70061 ) ;
#48472 = CARTESIAN_POINT ( 'NONE',  ( 10.00000000000000178, 19.31368534415484106, 10.88017736071110342 ) ) ;
#48473 = CARTESIAN_POINT ( 'NONE',  ( 5.076628168052704559, 60.17559781766745175, -8.527530157486179263 ) ) ;
#48474 = CARTESIAN_POINT ( 'NONE',  ( 0.6178305044545818747, 48.49863466993042493, -9.382169495545419124 ) ) ;
#48475 = LINE ( 'NONE', #10484, #47636 ) ;
#48476 = CARTESIAN_POINT ( 'NONE',  ( 13.79529636645031943, 15.34541550158063750, -14.16423886937409904 ) ) ;
#48477 = CARTESIAN_POINT ( 'NONE',  ( 4.559911319644449179, 43.89701867748816966, 9.422509992056141925 ) ) ;
#48478 = CARTESIAN_POINT ( 'NONE',  ( 17.96484262340118221, 16.18868534415483396, -7.964842623401177768 ) ) ;
#48479 = CARTESIAN_POINT ( 'NONE',  ( 2.791683348922240793, 51.63393115100078745, 7.208316651077764092 ) ) ;
#48480 = CARTESIAN_POINT ( 'NONE',  ( -8.332123631136926889, -7.291398214258985711, -3.750000000000000888 ) ) ;
#48481 = CARTESIAN_POINT ( 'NONE',  ( 19.84674366389459266, 38.30059781766745175, 2.638427012816836559 ) ) ;
#48482 = CARTESIAN_POINT ( 'NONE',  ( 19.84674366389459266, 8.717264484334116048, -2.638427012816827677 ) ) ;
#48483 = CARTESIAN_POINT ( 'NONE',  ( -5.204170427930421283E-15, -27.12636533006957507, -12.81628187352647608 ) ) ;
#48484 = VERTEX_POINT ( 'NONE', #84078 ) ;
#48485 = ADVANCED_FACE ( 'NONE', ( #62536 ), #33845, .T. ) ;
#48486 = CARTESIAN_POINT ( 'NONE',  ( 5.076628168052704559, 15.17559781766745175, -8.527530157486179263 ) ) ;
#48487 = CARTESIAN_POINT ( 'NONE',  ( 7.361572987183169658, 64.96726448433412315, -9.846743663894592657 ) ) ;
#48488 = CARTESIAN_POINT ( 'NONE',  ( 19.42250999205614548, 40.98035201082150536, -5.440088680355545492 ) ) ;
#48490 = CARTESIAN_POINT ( 'NONE',  ( -2.816281873526471635, 48.91530133659708213, -3.434112377981056508 ) ) ;
#48489 = CARTESIAN_POINT ( 'NONE',  ( 0.5774900079438607392, 18.48035201082150536, 5.440088680355550821 ) ) ;
#48491 = CARTESIAN_POINT ( 'NONE',  ( 17.08211943468705840, 25.13708216824730357, -12.26659068614894466 ) ) ;
#48492 = EDGE_CURVE ( 'NONE', #37577, #63243, #24576, .T. ) ;
#48493 = DIRECTION ( 'NONE',  ( -0.000000000000000000, -0.000000000000000000, 1.000000000000000000 ) ) ;
#48494 = AXIS2_PLACEMENT_3D ( 'NONE', #4203, #2747, #41230 ) ;
#48495 = CARTESIAN_POINT ( 'NONE',  ( 22.81628187352647785, 56.41530133659708213, 3.434112377981063169 ) ) ;
#48496 = ORIENTED_EDGE ( 'NONE', *, *, #3302, .T. ) ;
#48497 = CARTESIAN_POINT ( 'NONE',  ( 0.1532563361054082862, 56.21726448433411605, 2.638427012816831674 ) ) ;
#48498 = CARTESIAN_POINT ( 'NONE',  ( -0.8801773607111008646, 38.27201867748816255, 2.915334737309923430 ) ) ;
#48499 = EDGE_CURVE ( 'NONE', #20656, #38087, #19024, .T. ) ;
#48500 = ORIENTED_EDGE ( 'NONE', *, *, #27363, .F. ) ;
#48501 = CARTESIAN_POINT ( 'NONE',  ( 1.472469842513823179, 0.5922644843341181575, -4.923371831947296329 ) ) ;
#48502 = CARTESIAN_POINT ( 'NONE',  ( 7.361572987183169658, 9.967264484334119601, -9.846743663894592657 ) ) ;
#48503 = CARTESIAN_POINT ( 'NONE',  ( -0.8801773607110991993, 62.85535201082150536, -2.915334737309923874 ) ) ;
#48504 = CARTESIAN_POINT ( 'NONE',  ( -10.64017930668191170, 0.5000000000000004441, -10.57291749337230158 ) ) ;
#48506 = CARTESIAN_POINT ( 'NONE',  ( -4.856092091438414471, -2.729140156053354904E-15, 13.79590085420550061 ) ) ;
#48505 = CARTESIAN_POINT ( 'NONE',  ( 0.5774900079438590739, 52.64701867748817676, -5.440088680355550821 ) ) ;
#48507 = CARTESIAN_POINT ( 'NONE',  ( -0.8801773607111008646, 58.27201867748816966, 2.915334737309923430 ) ) ;
#48509 = VERTEX_POINT ( 'NONE', #49501 ) ;
#48508 = CARTESIAN_POINT ( 'NONE',  ( 2.791683348922240793, 1.633931151000784565, 7.208316651077764092 ) ) ;
#48510 = CARTESIAN_POINT ( 'NONE',  ( -0.8801773607111009756, 63.27201867748817676, 2.915334737309923874 ) ) ;
#48511 = CARTESIAN_POINT ( 'NONE',  ( 19.84674366389459266, 58.30059781766745886, 2.638427012816836559 ) ) ;
#48512 = VERTEX_POINT ( 'NONE', #12008 ) ;
#48513 = ORIENTED_EDGE ( 'NONE', *, *, #32933, .T. ) ;
#48514 = CARTESIAN_POINT ( 'NONE',  ( 6.579634127946657252, -87.99828267815705374, -2.750000000000000000 ) ) ;
#48515 = CARTESIAN_POINT ( 'NONE',  ( 22.26659068614894466, 8.887082168247300018, 7.082119434687054849 ) ) ;
#48516 = CARTESIAN_POINT ( 'NONE',  ( 0.6178305044545838731, 64.74863466993043914, 9.382169495545420901 ) ) ;
#48517 = CARTESIAN_POINT ( 'NONE',  ( 6.204703633549690345, 0.7620821682473009062, -14.16423886937410259 ) ) ;
#48518 = CARTESIAN_POINT ( 'NONE',  ( 13.79529636645030344, 33.26208216824730357, 14.16423886937410614 ) ) ;
#48519 = CARTESIAN_POINT ( 'NONE',  ( 0.2751277870542876425, 45.30223176428830811, 6.499999999999984901 ) ) ;
#48520 = CARTESIAN_POINT ( 'NONE',  ( 22.26659068614894466, 3.887082168247300906, 7.082119434687054849 ) ) ;
#48521 = CARTESIAN_POINT ( 'NONE',  ( 19.42250999205614548, 15.98035201082150714, -5.440088680355545492 ) ) ;
#48522 =( LENGTH_UNIT ( ) NAMED_UNIT ( * ) SI_UNIT ( .MILLI., .METRE. ) );
#48523 = EDGE_LOOP ( 'NONE', ( #39762, #5081, #5346, #82052 ) ) ;
#48524 = CARTESIAN_POINT ( 'NONE',  ( 18.52753015748617571, 3.092264484334118269, 4.923371831947298993 ) ) ;
#48525 = CARTESIAN_POINT ( 'NONE',  ( 12.63842701281683922, 14.55059781766744997, -9.846743663894590881 ) ) ;
#48526 = CARTESIAN_POINT ( 'NONE',  ( -2.816281873526473856, 49.33196800326374643, 3.434112377981055619 ) ) ;
